#139934=CARTESIAN_POINT('Ctrl Pts',(20.2935357313021,17.1808649545431,8.74981199697633));
#139935=CARTESIAN_POINT('Ctrl Pts',(20.2268660954868,17.1296498004185,8.75399550841146));
#139936=CARTESIAN_POINT('Ctrl Pts',(20.1577482403935,17.0817815617839,8.75817901984659));
#139937=CARTESIAN_POINT('Ctrl Pts',(20.086560133894,17.0374818647638,8.76236253128172));
#139938=CARTESIAN_POINT('Ctrl Pts',(20.0221613278628,16.9974070863223,8.76614705589809));
#139939=CARTESIAN_POINT('Ctrl Pts',(19.9560688916324,16.9602521636411,8.76993158051446));
#139940=CARTESIAN_POINT('Ctrl Pts',(19.8885775886028,16.9261475776549,8.77371610513083));
#139941=CARTESIAN_POINT('Ctrl Pts',(19.8139509296381,16.8884373662162,8.77790073952388));
#139942=CARTESIAN_POINT('Ctrl Pts',(19.7373359438749,16.8543169479217,8.78208537391693));
#139943=CARTESIAN_POINT('Ctrl Pts',(19.6591123506695,16.8240003898955,8.78627000830997));
#139944=CARTESIAN_POINT('Ctrl Pts',(19.5810000990668,16.7937269837373,8.79044868639392));
#139945=CARTESIAN_POINT('Ctrl Pts',(19.5012842132702,16.7672468481168,8.79462736447787));
#139946=CARTESIAN_POINT('Ctrl Pts',(19.420368077509,16.7447277396491,8.79880604256181));
#139947=CARTESIAN_POINT('Ctrl Pts',(19.3380015781677,16.7218049923462,8.80305962044725));
#139948=CARTESIAN_POINT('Ctrl Pts',(19.2543918069889,16.7029868892007,8.80731319833268));
#139949=CARTESIAN_POINT('Ctrl Pts',(19.1699845756622,16.6883986740302,8.81156677621811));
#139950=CARTESIAN_POINT('Ctrl Pts',(19.0872137432219,16.6740932798773,8.81573789019606));
#139951=CARTESIAN_POINT('Ctrl Pts',(19.0036765695344,16.6638553099793,8.81990900417402));
#139952=CARTESIAN_POINT('Ctrl Pts',(18.9198060037776,16.6577518473599,8.82408011815197));
#139953=CARTESIAN_POINT('Ctrl Pts',(18.8359635815991,16.6516504328162,8.82824983247234));
#139954=CARTESIAN_POINT('Ctrl Pts',(18.7517884479705,16.6496808035662,8.83241954679272));
#139955=CARTESIAN_POINT('Ctrl Pts',(18.6677187513895,16.6518581914863,8.83658926111309));
#139956=CARTESIAN_POINT('Ctrl Pts',(18.5836520463691,16.6540355019256,8.84075882705714));
#139957=CARTESIAN_POINT('Ctrl Pts',(18.4996912307931,16.660359523368,8.84492839300118));
#139958=CARTESIAN_POINT('Ctrl Pts',(18.4162731576902,16.6707933836643,8.84909795894523));
#139959=CARTESIAN_POINT('Ctrl Pts',(18.3299222080443,16.681594085617,8.85341412168415));
#139960=CARTESIAN_POINT('Ctrl Pts',(18.2441533999762,16.6967989420232,8.85773028442307));
#139961=CARTESIAN_POINT('Ctrl Pts',(18.1594420717103,16.7163089996876,8.86204644716199));
#139962=CARTESIAN_POINT('Ctrl Pts',(18.0774902060527,16.7351835192758,8.86622201135367));
#139963=CARTESIAN_POINT('Ctrl Pts',(17.996528423794,16.758086889941,8.87039757554535));
#139964=CARTESIAN_POINT('Ctrl Pts',(17.9169718130409,16.7848786218092,8.87457313973703));
#139965=CARTESIAN_POINT('Ctrl Pts',(17.8333969870066,16.8130235403628,8.87895960174957));
#139966=CARTESIAN_POINT('Ctrl Pts',(17.7513735563979,16.8454597306831,8.88334606376211));
#139967=CARTESIAN_POINT('Ctrl Pts',(17.6713570660694,16.8819680133224,8.88773252577465));
#139968=CARTESIAN_POINT('Ctrl Pts',(17.5913405757408,16.9184762959617,8.89211898778719));
#139969=CARTESIAN_POINT('Ctrl Pts',(17.513331505326,16.959056335675,8.89650544979973));
#139970=CARTESIAN_POINT('Ctrl Pts',(17.4377516489576,17.003435683288,8.90089191181227));
#139971=CARTESIAN_POINT('Ctrl Pts',(17.365649333817,17.0457730713314,8.90507654620532));
#139972=CARTESIAN_POINT('Ctrl Pts',(17.2954892230291,17.091725414496,8.90926118059837));
#139973=CARTESIAN_POINT('Ctrl Pts',(17.2276568480541,17.1410892993693,8.91344581499142));
#139974=CARTESIAN_POINT('Ctrl Pts',(17.159921024069,17.1903829208624,8.91762449307535));
#139975=CARTESIAN_POINT('Ctrl Pts',(17.0945067235342,17.2430781703289,8.92180317115929));
#139976=CARTESIAN_POINT('Ctrl Pts',(17.0317733474474,17.2989266689429,8.92598184924323));
#139977=CARTESIAN_POINT('Ctrl Pts',(16.9679155206799,17.3557762117571,8.93023542712867));
#139978=CARTESIAN_POINT('Ctrl Pts',(16.9068360906096,17.4158929154663,8.9344890050141));
#139979=CARTESIAN_POINT('Ctrl Pts',(16.8488816768788,17.4789697150936,8.93874258289954));
#139980=CARTESIAN_POINT('Ctrl Pts',(16.792050822547,17.540823647876,8.94291369687749));
#139981=CARTESIAN_POINT('Ctrl Pts',(16.7382252223475,17.6055235719755,8.94708481085544));
#139982=CARTESIAN_POINT('Ctrl Pts',(16.6876956296653,17.6727417564176,8.9512559248334));
#139983=CARTESIAN_POINT('Ctrl Pts',(16.637182992676,17.7399373851488,8.95542563915377));
#139984=CARTESIAN_POINT('Ctrl Pts',(16.5899644428518,17.8096492285707,8.95959535347414));
#139985=CARTESIAN_POINT('Ctrl Pts',(16.5462899492621,17.8815171178611,8.96376506779451));
#139986=CARTESIAN_POINT('Ctrl Pts',(16.5026170097983,17.9533824497836,8.96793463373855));
#139987=CARTESIAN_POINT('Ctrl Pts',(16.4624881140049,18.0274032814579,8.9721041996826));
#139988=CARTESIAN_POINT('Ctrl Pts',(16.4261087184981,18.1031923304257,8.97627376562664));
#139989=CARTESIAN_POINT('Ctrl Pts',(16.3884502683242,18.1816460288594,8.98058992836556));
#139990=CARTESIAN_POINT('Ctrl Pts',(16.3548101172679,18.2619941236263,8.98490609110448));
#139991=CARTESIAN_POINT('Ctrl Pts',(16.3253623529172,18.3437833690158,8.9892222538434));
#139992=CARTESIAN_POINT('Ctrl Pts',(16.296873846393,18.4229083383394,8.99339781803508));
#139993=CARTESIAN_POINT('Ctrl Pts',(16.2723088794104,18.5033815448835,8.99757338222676));
#139994=CARTESIAN_POINT('Ctrl Pts',(16.2517740015379,18.5847779207351,9.00174894641844));
#139995=CARTESIAN_POINT('Ctrl Pts',(16.2302019558011,18.6702854340295,9.00613540843099));
#139996=CARTESIAN_POINT('Ctrl Pts',(16.213077931431,18.7568112533014,9.01052187044352));
#139997=CARTESIAN_POINT('Ctrl Pts',(16.2004642109876,18.8438536997419,9.01490833245606));
#139998=CARTESIAN_POINT('Ctrl Pts',(16.1878504905441,18.9308961461825,9.01929479446861));
#139999=CARTESIAN_POINT('Ctrl Pts',(16.179747051756,19.0184546350337,9.02368125648115));
#140000=CARTESIAN_POINT('Ctrl Pts',(16.1761531171477,19.10602703261,9.02806771849369));
#140001=CARTESIAN_POINT('Ctrl Pts',(16.1747268399112,19.1407807303868,9.0298085155863));
#140002=CARTESIAN_POINT('Ctrl Pts',(16.1740088273484,19.1755636940745,9.0315493126789));
#140003=CARTESIAN_POINT('Ctrl Pts',(16.1740000808904,19.2103564484228,9.0332901097715));
#140004=CARTESIAN_POINT('',(16.174000001606,19.2110906788005,8.96670989026365));
#140005=CARTESIAN_POINT('Ctrl Pts',(20.2935357313021,17.1808649545431,8.68337763228924));
#140006=CARTESIAN_POINT('Ctrl Pts',(20.2269370011896,17.1297042696901,8.68754916275219));
#140007=CARTESIAN_POINT('Ctrl Pts',(20.157763917459,17.0817825471759,8.69172069321514));
#140008=CARTESIAN_POINT('Ctrl Pts',(20.0863673947936,17.0373619368673,8.69589222367809));
#140009=CARTESIAN_POINT('Ctrl Pts',(20.0149989840445,16.9929588168851,8.70006211162806));
#140010=CARTESIAN_POINT('Ctrl Pts',(19.9414092630416,16.9520543143202,8.70423199957803));
#140011=CARTESIAN_POINT('Ctrl Pts',(19.8659780913813,16.9148672510865,8.70840188752799));
#140012=CARTESIAN_POINT('Ctrl Pts',(19.7905539926854,16.8776836747771,8.71257138447953));
#140013=CARTESIAN_POINT('Ctrl Pts',(19.7132891992873,16.8442170480217,8.71674088143107));
#140014=CARTESIAN_POINT('Ctrl Pts',(19.6345869032211,16.8146395868429,8.72091037838262));
#140015=CARTESIAN_POINT('Ctrl Pts',(19.5558683784269,16.7850560266733,8.7250807351011));
#140016=CARTESIAN_POINT('Ctrl Pts',(19.4757121933861,16.7593633850936,8.72925109181958));
#140017=CARTESIAN_POINT('Ctrl Pts',(19.3945388869154,16.7376847392876,8.73342144853806));
#140018=CARTESIAN_POINT('Ctrl Pts',(19.3132745110844,16.7159817719345,8.73759648403255));
#140019=CARTESIAN_POINT('Ctrl Pts',(19.2309911818684,16.6983019051782,8.74177151952703));
#140020=CARTESIAN_POINT('Ctrl Pts',(19.1481213253207,16.6847174489154,8.74594655502151));
#140021=CARTESIAN_POINT('Ctrl Pts',(19.0651969677462,16.6711240585619,8.75012433631201));
#140022=CARTESIAN_POINT('Ctrl Pts',(18.9816857717183,16.6616314907568,8.75430211760251));
#140023=CARTESIAN_POINT('Ctrl Pts',(18.8980246357382,16.6562601073943,8.75847989889301));
#140024=CARTESIAN_POINT('Ctrl Pts',(18.8142288636417,16.6508800798485,8.76266440349943));
#140025=CARTESIAN_POINT('Ctrl Pts',(18.7302831289701,16.6496344772916,8.76684890810586));
#140026=CARTESIAN_POINT('Ctrl Pts',(18.6466231447615,16.6524915897796,8.77103341271229));
#140027=CARTESIAN_POINT('Ctrl Pts',(18.6193179827511,16.6534241015426,8.77239916214785));
#140028=CARTESIAN_POINT('Ctrl Pts',(18.5920432050038,16.6547932470753,8.77376491158341));
#140029=CARTESIAN_POINT('Ctrl Pts',(18.5648137584889,16.6565967398072,8.77513066101897));
#140030=CARTESIAN_POINT('Ctrl Pts',(18.4813831705471,16.6621226126484,8.77931529541201));
#140031=CARTESIAN_POINT('Ctrl Pts',(18.3980683312295,16.6717505167586,8.78349992980505));
#140032=CARTESIAN_POINT('Ctrl Pts',(18.3153050503469,16.6854714337124,8.7876845641981));
#140033=CARTESIAN_POINT('Ctrl Pts',(18.2326595727503,16.6991728206391,8.79186324228205));
#140034=CARTESIAN_POINT('Ctrl Pts',(18.150564544139,16.7169555737483,8.796041920366));
#140035=CARTESIAN_POINT('Ctrl Pts',(18.0694525718374,16.738758766681,8.80022059844995));
#140036=CARTESIAN_POINT('Ctrl Pts',(17.9868867257265,16.7609527661774,8.80447417633538));
#140037=CARTESIAN_POINT('Ctrl Pts',(17.9053400062234,16.7873127240842,8.80872775422082));
#140038=CARTESIAN_POINT('Ctrl Pts',(17.8252599013638,16.8177195247672,8.81298133210625));
#140039=CARTESIAN_POINT('Ctrl Pts',(17.7467323056004,16.8475368302849,8.8171524460842));
#140040=CARTESIAN_POINT('Ctrl Pts',(17.6696154154523,16.8812452961237,8.82132356006215));
#140041=CARTESIAN_POINT('Ctrl Pts',(17.5943160431835,16.9186822910916,8.8254946740401));
#140042=CARTESIAN_POINT('Ctrl Pts',(17.5190419383462,16.9561067237143,8.82966438836047));
#140043=CARTESIAN_POINT('Ctrl Pts',(17.4455845517329,16.9972569960431,8.83383410268084));
#140044=CARTESIAN_POINT('Ctrl Pts',(17.3743287784396,17.0419231988562,8.83800381700122));
#140045=CARTESIAN_POINT('Ctrl Pts',(17.3030755407325,17.086587812254,8.84217338294526));
#140046=CARTESIAN_POINT('Ctrl Pts',(17.2340241499107,17.1347678623261,8.8463429488893));
#140047=CARTESIAN_POINT('Ctrl Pts',(17.1675318647116,17.1862092500394,8.85051251483334));
#140048=CARTESIAN_POINT('Ctrl Pts',(17.0987017927918,17.239459253485,8.85482867757226));
#140049=CARTESIAN_POINT('Ctrl Pts',(17.0326145482172,17.2962038761403,8.85914484031118));
#140050=CARTESIAN_POINT('Ctrl Pts',(16.9696289167233,17.3561159927108,8.86346100305011));
#140051=CARTESIAN_POINT('Ctrl Pts',(16.9086950355505,17.4140764783858,8.86763656724179));
#140052=CARTESIAN_POINT('Ctrl Pts',(16.8506640912072,17.4750008911688,8.87181213143347));
#140053=CARTESIAN_POINT('Ctrl Pts',(16.7958218659393,17.5385570202099,8.87598769562515));
#140054=CARTESIAN_POINT('Ctrl Pts',(16.7382096902482,17.6053232182385,8.88037415763769));
#140055=CARTESIAN_POINT('Ctrl Pts',(16.6841171816931,17.6749935141295,8.88476061965023));
#140056=CARTESIAN_POINT('Ctrl Pts',(16.6338248927155,17.7471473712348,8.88914708166278));
#140057=CARTESIAN_POINT('Ctrl Pts',(16.5835326037379,17.8193012283401,8.89353354367532));
#140058=CARTESIAN_POINT('Ctrl Pts',(16.5370407765469,17.8939381139568,8.89792000568786));
#140059=CARTESIAN_POINT('Ctrl Pts',(16.4945737975988,17.9706088181549,8.9023064677004));
#140060=CARTESIAN_POINT('Ctrl Pts',(16.4520961746313,18.0472987392713,8.90669402914567));
#140061=CARTESIAN_POINT('Ctrl Pts',(16.4134992022808,18.1262856298358,8.91108159059094));
#140062=CARTESIAN_POINT('Ctrl Pts',(16.3790251742671,18.2071605854698,8.91546915203621));
#140063=CARTESIAN_POINT('Ctrl Pts',(16.3446454932945,18.2878142059945,8.91984470579152));
#140064=CARTESIAN_POINT('Ctrl Pts',(16.3143664333072,18.3703452363826,8.92422025954683));
#140065=CARTESIAN_POINT('Ctrl Pts',(16.2883841141658,18.4543211123896,8.92859581330214));
#140066=CARTESIAN_POINT('Ctrl Pts',(16.2624439986578,18.5381605845957,8.93296425975245));
#140067=CARTESIAN_POINT('Ctrl Pts',(16.2407868563187,18.6234398583863,8.93733270620276));
#140068=CARTESIAN_POINT('Ctrl Pts',(16.2235607960525,18.7097066694205,8.94170115265307));
#140069=CARTESIAN_POINT('Ctrl Pts',(16.2063704951607,18.7957944002037,8.94606053069715));
#140070=CARTESIAN_POINT('Ctrl Pts',(16.193593030381,18.8828651985171,8.95041990874122));
#140071=CARTESIAN_POINT('Ctrl Pts',(16.1853263642748,18.9704533339262,8.9547792867853));
#140072=CARTESIAN_POINT('Ctrl Pts',(16.1777850503447,19.0503561166421,8.9587561545997));
#140073=CARTESIAN_POINT('Ctrl Pts',(16.1739971536887,19.1306890276032,8.96273302241411));
#140074=CARTESIAN_POINT('Ctrl Pts',(16.174000001606,19.21109067809,8.96670989022851));
#140075=CARTESIAN_POINT('Ctrl Pts',(16.174000001606,19.2110906788005,8.96670989026365));
#140076=CARTESIAN_POINT('Ctrl Pts',(16.1740031377284,19.2996281672636,8.97108917708311));
#140077=CARTESIAN_POINT('Ctrl Pts',(16.1786036643305,19.388071802769,8.97546846390256));
#140078=CARTESIAN_POINT('Ctrl Pts',(16.1877467776184,19.4759424985001,8.97984775072202));
#140079=CARTESIAN_POINT('Ctrl Pts',(16.1969159526896,19.5640636632955,8.98423952038188));
#140080=CARTESIAN_POINT('Ctrl Pts',(16.2106535575187,19.6516082364872,8.98863129004175));
#140081=CARTESIAN_POINT('Ctrl Pts',(16.2288531973791,19.7381048257399,8.99302305970162));
#140082=CARTESIAN_POINT('Ctrl Pts',(16.2470794228643,19.8247277672657,8.99742124475987));
#140083=CARTESIAN_POINT('Ctrl Pts',(16.2697805833341,19.9102992971043,9.00181942981813));
#140084=CARTESIAN_POINT('Ctrl Pts',(16.2968004138021,19.9943633748375,9.00621761487638));
#140085=CARTESIAN_POINT('Ctrl Pts',(16.3238953969119,20.0786612674176,9.01062803299533));
#140086=CARTESIAN_POINT('Ctrl Pts',(16.3553329301083,20.1614429605719,9.01503845111429));
#140087=CARTESIAN_POINT('Ctrl Pts',(16.3909082116845,20.2422714829415,9.01944886923325));
#140088=CARTESIAN_POINT('Ctrl Pts',(16.4178853374884,20.3035646370615,9.02279333761611));
#140089=CARTESIAN_POINT('Ctrl Pts',(16.4472408225494,20.363735085321,9.02613780599897));
#140090=CARTESIAN_POINT('Ctrl Pts',(16.478868382946,20.422602818486,9.02948227438183));
#140091=CARTESIAN_POINT('Ctrl Pts',(16.5184411227219,20.4962587519986,9.03366690877488));
#140092=CARTESIAN_POINT('Ctrl Pts',(16.5616998679758,20.5681109610611,9.03785154316793));
#140093=CARTESIAN_POINT('Ctrl Pts',(16.6084559713663,20.6377664778581,9.04203617756098));
#140094=CARTESIAN_POINT('Ctrl Pts',(16.6551455232309,20.7073228486487,9.04621485564492));
#140095=CARTESIAN_POINT('Ctrl Pts',(16.7053222910481,20.7746883591286,9.05039353372887));
#140096=CARTESIAN_POINT('Ctrl Pts',(16.7587517035101,20.8394944480144,9.05457221181282));
#140097=CARTESIAN_POINT('Ctrl Pts',(16.8131387997914,20.9054621394682,9.05882578969825));
#140098=CARTESIAN_POINT('Ctrl Pts',(16.8708960667842,20.9687773268414,9.06307936758369));
#140099=CARTESIAN_POINT('Ctrl Pts',(16.9317298045576,21.0290819955712,9.06733294546912));
#140100=CARTESIAN_POINT('Ctrl Pts',(16.9913841616171,21.0882175406228,9.07150405944708));
#140101=CARTESIAN_POINT('Ctrl Pts',(17.0539964254171,21.1444579161298,9.07567517342503));
#140102=CARTESIAN_POINT('Ctrl Pts',(17.1192501263854,21.1975001499274,9.07984628740298));
#140103=CARTESIAN_POINT('Ctrl Pts',(17.1844819308442,21.2505245848913,9.08401600172335));
#140104=CARTESIAN_POINT('Ctrl Pts',(17.2523530554692,21.3003527195435,9.08818571604373));
#140105=CARTESIAN_POINT('Ctrl Pts',(17.3225130695873,21.3467211066228,9.0923554303641));
#140106=CARTESIAN_POINT('Ctrl Pts',(17.3926705871109,21.3930878437158,9.09652499630815));
#140107=CARTESIAN_POINT('Ctrl Pts',(17.4651164479275,21.4359948250818,9.10069456225219));
#140108=CARTESIAN_POINT('Ctrl Pts',(17.5394714392698,21.475222055718,9.10486412819623));
#140109=CARTESIAN_POINT('Ctrl Pts',(17.6164406603808,21.5158284673913,9.10918029093515));
#140110=CARTESIAN_POINT('Ctrl Pts',(17.6954552934394,21.5524913076844,9.11349645367408));
#140111=CARTESIAN_POINT('Ctrl Pts',(17.7760690203244,21.5850194266639,9.117812616413));
#140112=CARTESIAN_POINT('Ctrl Pts',(17.8540567635352,21.6164879455891,9.12198818060468));
#140113=CARTESIAN_POINT('Ctrl Pts',(17.9335405590284,21.6440868736176,9.12616374479636));
#140114=CARTESIAN_POINT('Ctrl Pts',(18.0140996850996,21.6676936187906,9.13033930898804));
#140115=CARTESIAN_POINT('Ctrl Pts',(18.0987276611175,21.6924926845425,9.13472577100058));
#140116=CARTESIAN_POINT('Ctrl Pts',(18.1845418843915,21.7128855434687,9.13911223301312));
#140117=CARTESIAN_POINT('Ctrl Pts',(18.2710433987722,21.7287909336122,9.14349869502566));
#140118=CARTESIAN_POINT('Ctrl Pts',(18.3575449131529,21.7446963237556,9.14788515703819));
#140119=CARTESIAN_POINT('Ctrl Pts',(18.4447331334585,21.756114245197,9.15227161905073));
#140120=CARTESIAN_POINT('Ctrl Pts',(18.5321062576865,21.7630264334083,9.15665808106327));
#140121=CARTESIAN_POINT('Ctrl Pts',(18.6154592149507,21.7696205815937,9.16084271545632));
#140122=CARTESIAN_POINT('Ctrl Pts',(18.6992906902526,21.7721390606606,9.16502734984937));
#140123=CARTESIAN_POINT('Ctrl Pts',(18.78316814862,21.7705277871438,9.16921198424242));
#140124=CARTESIAN_POINT('Ctrl Pts',(18.8669262178074,21.7689188070754,9.17339066232636));
#140125=CARTESIAN_POINT('Ctrl Pts',(18.9507296840396,21.7631917591217,9.17756934041031));
#140126=CARTESIAN_POINT('Ctrl Pts',(19.0341416766033,21.7533443853982,9.18174801849425));
#140127=CARTESIAN_POINT('Ctrl Pts',(19.1190487691866,21.7433205045779,9.18600159637969));
#140128=CARTESIAN_POINT('Ctrl Pts',(19.2035497350918,21.7290270933803,9.19025517426511));
#140129=CARTESIAN_POINT('Ctrl Pts',(19.2871845665266,21.7105173204755,9.19450875215055));
#140130=CARTESIAN_POINT('Ctrl Pts',(19.369197973554,21.6923663956372,9.1986798661285));
#140131=CARTESIAN_POINT('Ctrl Pts',(19.4503780599824,21.6701612389659,9.20285098010646));
#140132=CARTESIAN_POINT('Ctrl Pts',(19.5302987751906,21.6440039582027,9.20702209408442));
#140133=CARTESIAN_POINT('Ctrl Pts',(19.610192672231,21.6178554547677,9.21119180840479));
#140134=CARTESIAN_POINT('Ctrl Pts',(19.6888276004821,21.5877576040183,9.21536152272516));
#140135=CARTESIAN_POINT('Ctrl Pts',(19.7657923610116,21.553862463688,9.21953123704553));
#140136=CARTESIAN_POINT('Ctrl Pts',(19.8427543828046,21.5199685294922,9.22370080298957));
#140137=CARTESIAN_POINT('Ctrl Pts',(19.9180459343718,21.4822777605697,9.22787036893362));
#140138=CARTESIAN_POINT('Ctrl Pts',(19.9912767740527,21.4409899357234,9.23203993487766));
#140139=CARTESIAN_POINT('Ctrl Pts',(20.0670823197166,21.3982504818896,9.23635609761658));
#140140=CARTESIAN_POINT('Ctrl Pts',(20.1406790886265,21.351656579909,9.2406722603555));
#140141=CARTESIAN_POINT('Ctrl Pts',(20.2116647704044,21.3014800468566,9.24498842309442));
#140142=CARTESIAN_POINT('Ctrl Pts',(20.2803381010648,21.2529380090908,9.2491639872861));
#140143=CARTESIAN_POINT('Ctrl Pts',(20.3465675028829,21.2010434919511,9.25333955147778));
#140144=CARTESIAN_POINT('Ctrl Pts',(20.4100221667426,21.1460838991081,9.25751511566946));
#140145=CARTESIAN_POINT('Ctrl Pts',(20.4766817748247,21.0883484278846,9.26190157768201));
#140146=CARTESIAN_POINT('Ctrl Pts',(20.5402785534045,21.0272305142621,9.26628803969455));
#140147=CARTESIAN_POINT('Ctrl Pts',(20.6004740985359,20.9631057158444,9.27067450170709));
#140148=CARTESIAN_POINT('Ctrl Pts',(20.6606696436673,20.8989809174267,9.27506096371963));
#140149=CARTESIAN_POINT('Ctrl Pts',(20.7174636386703,20.8318497263029,9.27944742573217));
#140150=CARTESIAN_POINT('Ctrl Pts',(20.7705691100607,20.7621241923026,9.28383388774471));
#140151=CARTESIAN_POINT('Ctrl Pts',(20.8212311199913,20.6956068334797,9.28801852213775));
#140152=CARTESIAN_POINT('Ctrl Pts',(20.8687251499198,20.6264810343217,9.2922031565308));
#140153=CARTESIAN_POINT('Ctrl Pts',(20.9127716012342,20.5550812139358,9.29638779092385));
#140154=CARTESIAN_POINT('Ctrl Pts',(20.9567553578771,20.4837830223568,9.30056646900779));
#140155=CARTESIAN_POINT('Ctrl Pts',(20.997301043686,20.4102176270062,9.30474514709174));
#140156=CARTESIAN_POINT('Ctrl Pts',(21.0341702903064,20.3347511448678,9.30892382517568));
#140157=CARTESIAN_POINT('Ctrl Pts',(21.071700391675,20.2579319802738,9.31317740306111));
#140158=CARTESIAN_POINT('Ctrl Pts',(21.1054206649962,20.1791432881301,9.31743098094655));
#140159=CARTESIAN_POINT('Ctrl Pts',(21.1351268232138,20.0988006413847,9.32168455883199));
#140160=CARTESIAN_POINT('Ctrl Pts',(21.1642570695876,20.0200155936223,9.32585567280994));
#140161=CARTESIAN_POINT('Ctrl Pts',(21.1895272879509,19.9397367578111,9.33002678678789));
#140162=CARTESIAN_POINT('Ctrl Pts',(21.2107927216344,19.8583776440833,9.33419790076584));
#140163=CARTESIAN_POINT('Ctrl Pts',(21.2320510194963,19.777045831192,9.33836761508621));
#140164=CARTESIAN_POINT('Ctrl Pts',(21.2493070853372,19.6946349050203,9.34253732940659));
#140165=CARTESIAN_POINT('Ctrl Pts',(21.2624662014641,19.6115729247638,9.34670704372696));
#140166=CARTESIAN_POINT('Ctrl Pts',(21.2756248493332,19.528513900209,9.350876609671));
#140167=CARTESIAN_POINT('Ctrl Pts',(21.284686766209,19.4448043221315,9.35504617561504));
#140168=CARTESIAN_POINT('Ctrl Pts',(21.2896087040397,19.3608804584879,9.35921574155908));
#140169=CARTESIAN_POINT('Ctrl Pts',(21.2947036911327,19.2740059353298,9.36353190429801));
#140170=CARTESIAN_POINT('Ctrl Pts',(21.2953621283496,19.1869023041989,9.36784806703693));
#140171=CARTESIAN_POINT('Ctrl Pts',(21.2915948078576,19.1000549738833,9.37216422977585));
#140172=CARTESIAN_POINT('Ctrl Pts',(21.2879502074343,19.016036686218,9.37633979396753));
#140173=CARTESIAN_POINT('Ctrl Pts',(21.2801638500694,18.9322587224487,9.38051535815921));
#140174=CARTESIAN_POINT('Ctrl Pts',(21.2682983360669,18.8491548068462,9.38469092235089));
#140175=CARTESIAN_POINT('Ctrl Pts',(21.2558335231598,18.7618535100274,9.38907738436343));
#140176=CARTESIAN_POINT('Ctrl Pts',(21.2388667599596,18.6752967161991,9.39346384637597));
#140177=CARTESIAN_POINT('Ctrl Pts',(21.2175306593405,18.5899722517346,9.39785030838851));
#140178=CARTESIAN_POINT('Ctrl Pts',(21.1961945587214,18.5046477872701,9.40223677040106));
#140179=CARTESIAN_POINT('Ctrl Pts',(21.1704893630394,18.4205561848056,9.4066232324136));
#140180=CARTESIAN_POINT('Ctrl Pts',(21.1406062076889,18.3381617783842,9.41100969442614));
#140181=CARTESIAN_POINT('Ctrl Pts',(21.1121004746698,18.259565227111,9.41519396859536));
#140182=CARTESIAN_POINT('Ctrl Pts',(21.0796873621586,18.182220330688,9.41937824276457));
#140183=CARTESIAN_POINT('Ctrl Pts',(21.0434966865738,18.1065430951347,9.42356251693379));
#140184=CARTESIAN_POINT('Ctrl Pts',(21.007355056005,18.0309684161425,9.42774112064258));
#140185=CARTESIAN_POINT('Ctrl Pts',(20.9674462242518,17.9570573217824,9.43191972435137));
#140186=CARTESIAN_POINT('Ctrl Pts',(20.9239489993286,17.8852083948299,9.43609832806016));
#140187=CARTESIAN_POINT('Ctrl Pts',(20.8805019784934,17.8134423952331,9.44027210886385));
#140188=CARTESIAN_POINT('Ctrl Pts',(20.8334750334886,17.7437342236849,9.44444588966753));
#140189=CARTESIAN_POINT('Ctrl Pts',(20.7830933894016,17.6764589345635,9.44861967047122));
#140190=CARTESIAN_POINT('Ctrl Pts',(20.7327462827087,17.6092297636906,9.45279059008379));
#140191=CARTESIAN_POINT('Ctrl Pts',(20.6790493196799,17.5444305296965,9.45696150969635));
#140192=CARTESIAN_POINT('Ctrl Pts',(20.6222709998958,17.4824073264784,9.46113242930892));
#140193=CARTESIAN_POINT('Ctrl Pts',(20.5655043373565,17.4203968573402,9.46530249258352));
#140194=CARTESIAN_POINT('Ctrl Pts',(20.5056578783566,17.3611616320062,9.46947255585812));
#140195=CARTESIAN_POINT('Ctrl Pts',(20.4430396423748,17.3050137721402,9.47364261913271));
#140196=CARTESIAN_POINT('Ctrl Pts',(20.3947976075597,17.2617566128161,9.47685529886603));
#140197=CARTESIAN_POINT('Ctrl Pts',(20.3449112621541,17.2203312827846,9.48006797859935));
#140198=CARTESIAN_POINT('Ctrl Pts',(20.2935357313021,17.1808649545431,9.48328065833267));
#140199=CARTESIAN_POINT('Origin',(18.734,19.211,-1.76670989022852));
#140200=CARTESIAN_POINT('',(20.2935357313021,17.1808649545432,10.3499274784722));
#140201=CARTESIAN_POINT('',(20.2935357313021,17.1808649545432,10.2832382208556));
#140202=CARTESIAN_POINT('',(20.2935357313021,17.1808649545432,-1.76670989022852));
#140203=CARTESIAN_POINT('',(16.1740007840082,19.2089964727374,9.83329010977151));
#140204=CARTESIAN_POINT('Ctrl Pts',(16.1740007840082,19.2089964727374,9.83329010977151));
#140205=CARTESIAN_POINT('Ctrl Pts',(16.1739350379054,19.2930033015151,9.83745593779553));
#140206=CARTESIAN_POINT('Ctrl Pts',(16.1780086491546,19.3770604200798,9.84162176581954));
#140207=CARTESIAN_POINT('Ctrl Pts',(16.186209790272,19.4607299485725,9.84578759384356));
#140208=CARTESIAN_POINT('Ctrl Pts',(16.1944094741073,19.544384609609,9.84995268163076));
#140209=CARTESIAN_POINT('Ctrl Pts',(16.2067351859308,19.6276513592373,9.85411776941796));
#140210=CARTESIAN_POINT('Ctrl Pts',(16.2231231591268,19.7100966739689,9.85828285720516));
#140211=CARTESIAN_POINT('Ctrl Pts',(16.2395131466373,19.7925521223991,9.86244845694073));
#140212=CARTESIAN_POINT('Ctrl Pts',(16.2599662961795,19.8741854840192,9.8666140566763));
#140213=CARTESIAN_POINT('Ctrl Pts',(16.2843678510517,19.9545740278134,9.87077965641186));
#140214=CARTESIAN_POINT('Ctrl Pts',(16.3087969918046,20.035053450603,9.87494996534479));
#140215=CARTESIAN_POINT('Ctrl Pts',(16.3371833165997,20.1142848040861,9.87912027427772));
#140216=CARTESIAN_POINT('Ctrl Pts',(16.3693624790257,20.191861557204,9.88329058321065));
#140217=CARTESIAN_POINT('Ctrl Pts',(16.4015603628986,20.2694834435371,9.88746331837879));
#140218=CARTESIAN_POINT('Ctrl Pts',(16.437555280145,20.3454483968708,9.89163605354694));
#140219=CARTESIAN_POINT('Ctrl Pts',(16.4771361744286,20.4193731513184,9.89580878871509));
#140220=CARTESIAN_POINT('Ctrl Pts',(16.5167895617082,20.4934333000524,9.8999891663097));
#140221=CARTESIAN_POINT('Ctrl Pts',(16.5600418069655,20.5654453913553,9.90416954390431));
#140222=CARTESIAN_POINT('Ctrl Pts',(16.6066377495773,20.6350540212634,9.90834992149893));
#140223=CARTESIAN_POINT('Ctrl Pts',(16.6436006876733,20.6902721225405,9.91166606942054));
#140224=CARTESIAN_POINT('Ctrl Pts',(16.6826668124624,20.7439783287842,9.91498221734214));
#140225=CARTESIAN_POINT('Ctrl Pts',(16.7236914224215,20.7960108589263,9.91829836526375));
#140226=CARTESIAN_POINT('Ctrl Pts',(16.7754602209958,20.8616705099242,9.9224829996568));
#140227=CARTESIAN_POINT('Ctrl Pts',(16.8305455538229,20.924913415419,9.92666763404985));
#140228=CARTESIAN_POINT('Ctrl Pts',(16.8886933634204,20.9853853631597,9.93085226844291));
#140229=CARTESIAN_POINT('Ctrl Pts',(16.9467584068082,21.0457712365676,9.93503094652685));
#140230=CARTESIAN_POINT('Ctrl Pts',(17.0078769523777,21.1033936577097,9.9392096246108));
#140231=CARTESIAN_POINT('Ctrl Pts',(17.07175395795,21.157930429083,9.94338830269474));
#140232=CARTESIAN_POINT('Ctrl Pts',(17.1367759129396,21.2134447328882,9.94764188058018));
#140233=CARTESIAN_POINT('Ctrl Pts',(17.2046558928942,21.2657612997092,9.95189545846561));
#140234=CARTESIAN_POINT('Ctrl Pts',(17.2750424589418,21.314578592159,9.95614903635105));
#140235=CARTESIAN_POINT('Ctrl Pts',(17.3440644440585,21.3624494661354,9.960320150329));
#140236=CARTESIAN_POINT('Ctrl Pts',(17.4154962970282,21.406955261226,9.96449126430695));
#140237=CARTESIAN_POINT('Ctrl Pts',(17.4889737195064,21.4478526015096,9.9686623782849));
#140238=CARTESIAN_POINT('Ctrl Pts',(17.5624264859258,21.4887362182957,9.97283209260527));
#140239=CARTESIAN_POINT('Ctrl Pts',(17.6379230570028,21.5260135615005,9.97700180692565));
#140240=CARTESIAN_POINT('Ctrl Pts',(17.7150725574697,21.5594860797668,9.98117152124603));
#140241=CARTESIAN_POINT('Ctrl Pts',(17.7922193126263,21.5929574069373,9.98534108719007));
#140242=CARTESIAN_POINT('Ctrl Pts',(17.8710184578639,21.6226239960436,9.98951065313412));
#140243=CARTESIAN_POINT('Ctrl Pts',(17.9510583236145,21.6483350880375,9.99368021907816));
#140244=CARTESIAN_POINT('Ctrl Pts',(18.033912292305,21.6749501503078,9.99799638181708));
#140245=CARTESIAN_POINT('Ctrl Pts',(18.1180953501449,21.6973262283484,10.002312544556));
#140246=CARTESIAN_POINT('Ctrl Pts',(18.2031347548813,21.7153526292288,10.0066287072949));
#140247=CARTESIAN_POINT('Ctrl Pts',(18.2854040099531,21.7327918219965,10.0108042714866));
#140248=CARTESIAN_POINT('Ctrl Pts',(18.3684742051326,21.7461603390116,10.0149798356783));
#140249=CARTESIAN_POINT('Ctrl Pts',(18.4519097174452,21.7554105550182,10.01915539987));
#140250=CARTESIAN_POINT('Ctrl Pts',(18.5395593591354,21.765127977445,10.0235418618825));
#140251=CARTESIAN_POINT('Ctrl Pts',(18.6276116092813,21.7703001003685,10.027928323895));
#140252=CARTESIAN_POINT('Ctrl Pts',(18.7155609817199,21.7709335933975,10.0323147859076));
#140253=CARTESIAN_POINT('Ctrl Pts',(18.8035103541584,21.7715670864265,10.0367012479201));
#140254=CARTESIAN_POINT('Ctrl Pts',(18.891356272623,21.767662051318,10.0410877099327));
#140255=CARTESIAN_POINT('Ctrl Pts',(18.9786013944248,21.7592876913421,10.0454741719452));
#140256=CARTESIAN_POINT('Ctrl Pts',(19.0618322388442,21.7512986480824,10.0496588063382));
#140257=CARTESIAN_POINT('Ctrl Pts',(19.1448261598418,21.7392127858656,10.0538434407313));
#140258=CARTESIAN_POINT('Ctrl Pts',(19.2271478044731,21.7230519984553,10.0580280751243));
#140259=CARTESIAN_POINT('Ctrl Pts',(19.3093522744327,21.7069142139256,10.0622067532083));
#140260=CARTESIAN_POINT('Ctrl Pts',(19.3908859211793,21.6867131129897,10.0663854312922));
#140261=CARTESIAN_POINT('Ctrl Pts',(19.4713181268662,21.6625223800313,10.0705641093762));
#140262=CARTESIAN_POINT('Ctrl Pts',(19.5531920220343,21.6378980455703,10.0748176872616));
#140263=CARTESIAN_POINT('Ctrl Pts',(19.6339241211584,21.6091396900263,10.079071265147));
#140264=CARTESIAN_POINT('Ctrl Pts',(19.7130706518194,21.5763796014057,10.0833248430325));
#140265=CARTESIAN_POINT('Ctrl Pts',(19.7906827725417,21.544254631029,10.0874959570104));
#140266=CARTESIAN_POINT('Ctrl Pts',(19.8667698102182,21.5082818897807,10.0916670709884));
#140267=CARTESIAN_POINT('Ctrl Pts',(19.9409299364302,21.4686359601469,10.0958381849663));
#140268=CARTESIAN_POINT('Ctrl Pts',(20.0150651774957,21.4290033340877,10.1000078992867));
#140269=CARTESIAN_POINT('Ctrl Pts',(20.0872743858818,21.3857001842594,10.1041776136071));
#140270=CARTESIAN_POINT('Ctrl Pts',(20.1571790379496,21.3389477028209,10.1083473279274));
#140271=CARTESIAN_POINT('Ctrl Pts',(20.22708120251,21.2921968850363,10.1125168938715));
#140272=CARTESIAN_POINT('Ctrl Pts',(20.2946785918821,21.2419972361384,10.1166864598155));
#140273=CARTESIAN_POINT('Ctrl Pts',(20.3596216126351,21.1886133020724,10.1208560257596));
#140274=CARTESIAN_POINT('Ctrl Pts',(20.4268479498819,21.1333524547408,10.1251721884985));
#140275=CARTESIAN_POINT('Ctrl Pts',(20.4912293829738,21.0746795720027,10.1294883512374));
#140276=CARTESIAN_POINT('Ctrl Pts',(20.5524169502583,21.0129322392957,10.1338045139763));
#140277=CARTESIAN_POINT('Ctrl Pts',(20.6116113389744,20.9531963194569,10.137980078168));
#140278=CARTESIAN_POINT('Ctrl Pts',(20.6678164672702,20.8905835561607,10.1421556423597));
#140279=CARTESIAN_POINT('Ctrl Pts',(20.7207564953884,20.8254344607422,10.1463312065514));
#140280=CARTESIAN_POINT('Ctrl Pts',(20.7763703984739,20.7569948393913,10.1507176685639));
#140281=CARTESIAN_POINT('Ctrl Pts',(20.8283803483074,20.6857564036306,10.1551041305764));
#140282=CARTESIAN_POINT('Ctrl Pts',(20.8765183429016,20.6121477974611,10.159490592589));
#140283=CARTESIAN_POINT('Ctrl Pts',(20.9246563374958,20.5385391912916,10.1638770546015));
#140284=CARTESIAN_POINT('Ctrl Pts',(20.9689221504901,20.4625609543414,10.1682635166141));
#140285=CARTESIAN_POINT('Ctrl Pts',(21.0091047687182,20.3846687315233,10.1726499786266));
#140286=CARTESIAN_POINT('Ctrl Pts',(21.0474385251168,20.3103604453409,10.1768346130197));
#140287=CARTESIAN_POINT('Ctrl Pts',(21.0821992629535,20.2340338438631,10.1810192474127));
#140288=CARTESIAN_POINT('Ctrl Pts',(21.113169743127,20.1560668406992,10.1852038818058));
#140289=CARTESIAN_POINT('Ctrl Pts',(21.1440961406553,20.0782108139138,10.1893825598897));
#140290=CARTESIAN_POINT('Ctrl Pts',(21.1712428282378,19.9987194471869,10.1935612379736));
#140291=CARTESIAN_POINT('Ctrl Pts',(21.1944386775071,19.9179947059399,10.1977399160576));
#140292=CARTESIAN_POINT('Ctrl Pts',(21.218050295704,19.835823031722,10.201993493943));
#140293=CARTESIAN_POINT('Ctrl Pts',(21.2375678238504,19.7523737600797,10.2062470718285));
#140294=CARTESIAN_POINT('Ctrl Pts',(21.252862289631,19.6680916383777,10.2105006497139));
#140295=CARTESIAN_POINT('Ctrl Pts',(21.2678602423477,19.585443490068,10.2146717636918));
#140296=CARTESIAN_POINT('Ctrl Pts',(21.2787973301571,19.5019949698559,10.2188428776698));
#140297=CARTESIAN_POINT('Ctrl Pts',(21.2856028472,19.4181784500398,10.2230139916477));
#140298=CARTESIAN_POINT('Ctrl Pts',(21.2924060805859,19.3343900556663,10.2271837059681));
#140299=CARTESIAN_POINT('Ctrl Pts',(21.2950804593957,19.2502343650758,10.2313534202885));
#140300=CARTESIAN_POINT('Ctrl Pts',(21.2936070835643,19.1661493838661,10.2355231346089));
#140301=CARTESIAN_POINT('Ctrl Pts',(21.2921337601619,19.0820673947608,10.2396927005529));
#140302=CARTESIAN_POINT('Ctrl Pts',(21.2865129844866,18.9980565699809,10.243862266497));
#140303=CARTESIAN_POINT('Ctrl Pts',(21.2767779695196,18.9145540559798,10.248031832441));
#140304=CARTESIAN_POINT('Ctrl Pts',(21.2667006834357,18.8281156965981,10.2523479951799));
#140305=CARTESIAN_POINT('Ctrl Pts',(21.2522145228802,18.7422225813438,10.2566641579188));
#140306=CARTESIAN_POINT('Ctrl Pts',(21.2334144574579,18.6573508603364,10.2609803206578));
#140307=CARTESIAN_POINT('Ctrl Pts',(21.2152268021894,18.575243826714,10.2651558848494));
#140308=CARTESIAN_POINT('Ctrl Pts',(21.1930021468739,18.4940931072444,10.2693314490411));
#140309=CARTESIAN_POINT('Ctrl Pts',(21.1668775008281,18.4143149518383,10.2735070132328));
#140310=CARTESIAN_POINT('Ctrl Pts',(21.139433361016,18.3305073914573,10.2778934752453));
#140311=CARTESIAN_POINT('Ctrl Pts',(21.1076851096663,18.2482152402669,10.2822799372579));
#140312=CARTESIAN_POINT('Ctrl Pts',(21.0718481041568,18.1678958623941,10.2866663992704));
#140313=CARTESIAN_POINT('Ctrl Pts',(21.0360110986473,18.0875764845214,10.2910528612829));
#140314=CARTESIAN_POINT('Ctrl Pts',(20.9960856701951,18.0092303623901,10.2954393232955));
#140315=CARTESIAN_POINT('Ctrl Pts',(20.9523407266399,17.9332815566288,10.299825785308));
#140316=CARTESIAN_POINT('Ctrl Pts',(20.9106208944253,17.8608486952342,10.3040091821604));
#140317=CARTESIAN_POINT('Ctrl Pts',(20.8652721209676,17.790326569507,10.3081925790129));
#140318=CARTESIAN_POINT('Ctrl Pts',(20.8164943998508,17.7221020603848,10.3123759758653));
#140319=CARTESIAN_POINT('Ctrl Pts',(20.7677772522461,17.6539622743297,10.3165541776607));
#140320=CARTESIAN_POINT('Ctrl Pts',(20.7156398718341,17.5881148134686,10.3207323794562));
#140321=CARTESIAN_POINT('Ctrl Pts',(20.6603275198124,17.5249210319758,10.3249105812517));
#140322=CARTESIAN_POINT('Ctrl Pts',(20.6050732438256,17.4617936017432,10.3290843960814));
#140323=CARTESIAN_POINT('Ctrl Pts',(20.546650919326,17.4013146604693,10.3332582109111));
#140324=CARTESIAN_POINT('Ctrl Pts',(20.4853475074074,17.3438144419212,10.3374320257408));
#140325=CARTESIAN_POINT('Ctrl Pts',(20.4241713478543,17.2864335811479,10.3415971766513));
#140326=CARTESIAN_POINT('Ctrl Pts',(20.3601263655428,17.2320194202034,10.3457623275617));
#140327=CARTESIAN_POINT('Ctrl Pts',(20.2935357313021,17.1808649545432,10.3499274784722));
#140328=CARTESIAN_POINT('Ctrl Pts',(20.2954164566376,17.1783794293288,9.5499633233039));
#140329=CARTESIAN_POINT('Ctrl Pts',(19.6881794277694,16.7191703127013,9.58795779950289));
#140330=CARTESIAN_POINT('Ctrl Pts',(17.9381456484885,16.3388456091724,9.66834421126236));
#140331=CARTESIAN_POINT('Ctrl Pts',(16.3483940920526,17.7909994706266,9.76278617059814));
#140332=CARTESIAN_POINT('Ctrl Pts',(16.1742904286681,18.9257985710608,9.81923365373494));
#140333=CARTESIAN_POINT('Ctrl Pts',(16.1763511750307,19.2089800092947,9.83328920131125));
#140334=CARTESIAN_POINT('',(16.1740010233873,19.2132890482674,9.76670989018929));
#140335=CARTESIAN_POINT('Ctrl Pts',(20.2935357313021,17.1808649545431,9.48328065833267));
#140336=CARTESIAN_POINT('Ctrl Pts',(20.226846789779,17.129634969907,9.48745093564785));
#140337=CARTESIAN_POINT('Ctrl Pts',(20.1576478303553,17.0817074848001,9.49162121296303));
#140338=CARTESIAN_POINT('Ctrl Pts',(20.0863050570472,17.0373231535749,9.49579149027821));
#140339=CARTESIAN_POINT('Ctrl Pts',(20.0148828973448,16.9928894338572,9.4999664080533));
#140340=CARTESIAN_POINT('Ctrl Pts',(19.9413125544491,16.9520069791659,9.50414132582839));
#140341=CARTESIAN_POINT('Ctrl Pts',(19.8659864662056,16.9148713798379,9.50831624360348));
#140342=CARTESIAN_POINT('Ctrl Pts',(19.7906119470755,16.8777119041871,9.51249384564074));
#140343=CARTESIAN_POINT('Ctrl Pts',(19.713479857659,16.8443042610608,9.516671447678));
#140344=CARTESIAN_POINT('Ctrl Pts',(19.6350021191175,16.8147956720376,9.52084904971526));
#140345=CARTESIAN_POINT('Ctrl Pts',(19.5563968495913,16.7852391298052,9.52503344060388));
#140346=CARTESIAN_POINT('Ctrl Pts',(19.4764420041446,16.7595944266193,9.52921783149249));
#140347=CARTESIAN_POINT('Ctrl Pts',(19.3955636525281,16.7379586469989,9.5334022223811));
#140348=CARTESIAN_POINT('Ctrl Pts',(19.3647456506557,16.7297145188295,9.53499664862326));
#140349=CARTESIAN_POINT('Ctrl Pts',(19.3337936524143,16.7220519237258,9.53659107486542));
#140350=CARTESIAN_POINT('Ctrl Pts',(19.3027314805897,16.7149742583486,9.53818550110757));
#140351=CARTESIAN_POINT('Ctrl Pts',(19.2212075887324,16.6963986471497,9.54237013550062));
#140352=CARTESIAN_POINT('Ctrl Pts',(19.1386209669252,16.6817867038644,9.54655476989367));
#140353=CARTESIAN_POINT('Ctrl Pts',(19.0553917867604,16.6712544774322,9.55073940428672));
#140354=CARTESIAN_POINT('Ctrl Pts',(18.9722810730318,16.6607372423208,9.55491808237066));
#140355=CARTESIAN_POINT('Ctrl Pts',(18.8885300701232,16.654288246849,9.5590967604546));
#140356=CARTESIAN_POINT('Ctrl Pts',(18.804570732492,16.6519728857014,9.56327543853855));
#140357=CARTESIAN_POINT('Ctrl Pts',(18.7191064840744,16.6496160233692,9.56752901642398));
#140358=CARTESIAN_POINT('Ctrl Pts',(18.6334268287623,16.6515425508617,9.57178259430942));
#140359=CARTESIAN_POINT('Ctrl Pts',(18.5479946282975,16.6577663636679,9.57603617219486));
#140360=CARTESIAN_POINT('Ctrl Pts',(18.4642186977459,16.663869515718,9.58020728617281));
#140361=CARTESIAN_POINT('Ctrl Pts',(18.3806811928207,16.6741047825049,9.58437840015076));
#140362=CARTESIAN_POINT('Ctrl Pts',(18.2978184502103,16.6884327252533,9.58854951412871));
#140363=CARTESIAN_POINT('Ctrl Pts',(18.2149835129935,16.7027558601221,9.59271922844909));
#140364=CARTESIAN_POINT('Ctrl Pts',(18.1328233413407,16.7211688651668,9.59688894276946));
#140365=CARTESIAN_POINT('Ctrl Pts',(18.0517667977985,16.7435807292205,9.60105865708984));
#140366=CARTESIAN_POINT('Ctrl Pts',(17.9707131385959,16.7659917957639,9.60522822303388));
#140367=CARTESIAN_POINT('Ctrl Pts',(17.8907634725904,16.7924013149753,9.60939778897792));
#140368=CARTESIAN_POINT('Ctrl Pts',(17.8123328245034,16.8226680260876,9.61356735492197));
#140369=CARTESIAN_POINT('Ctrl Pts',(17.7311446515844,16.8539988774246,9.61788351766089));
#140370=CARTESIAN_POINT('Ctrl Pts',(17.651584793418,16.8894630151456,9.6221996803998));
#140371=CARTESIAN_POINT('Ctrl Pts',(17.5740906315704,16.9288496418883,9.62651584313872));
#140372=CARTESIAN_POINT('Ctrl Pts',(17.499120833894,16.9669532534076,9.6306914073304));
#140373=CARTESIAN_POINT('Ctrl Pts',(17.4260846045835,17.0087274533692,9.63486697152208));
#140374=CARTESIAN_POINT('Ctrl Pts',(17.3553508285749,17.0539356842855,9.63904253571376));
#140375=CARTESIAN_POINT('Ctrl Pts',(17.2810444576937,17.101427275473,9.64342899772631));
#140376=CARTESIAN_POINT('Ctrl Pts',(17.2092797216846,17.152708580808,9.64781545973885));
#140377=CARTESIAN_POINT('Ctrl Pts',(17.1404457653641,17.2074569130478,9.65220192175139));
#140378=CARTESIAN_POINT('Ctrl Pts',(17.0716118090436,17.2622052452876,9.65658838376393));
#140379=CARTESIAN_POINT('Ctrl Pts',(17.0057090169082,17.3204201632973,9.66097484577647));
#140380=CARTESIAN_POINT('Ctrl Pts',(16.9430809195061,17.3817354354488,9.66536130778901));
#140381=CARTESIAN_POINT('Ctrl Pts',(16.8827886985013,17.4407637964061,9.66958416538902));
#140382=CARTESIAN_POINT('Ctrl Pts',(16.8252872091303,17.5029045422553,9.67380702298903));
#140383=CARTESIAN_POINT('Ctrl Pts',(16.7709203169311,17.5678572314245,9.67802988058904));
#140384=CARTESIAN_POINT('Ctrl Pts',(16.7179063153622,17.6311936081462,9.68214765466764));
#140385=CARTESIAN_POINT('Ctrl Pts',(16.6678730797622,17.6972032456021,9.68626542874624));
#140386=CARTESIAN_POINT('Ctrl Pts',(16.6211045875939,17.7655682388182,9.69038320282484));
#140387=CARTESIAN_POINT('Ctrl Pts',(16.57438033231,17.833868567681,9.69449708202705));
#140388=CARTESIAN_POINT('Ctrl Pts',(16.530914960773,17.9045194435154,9.69861096122926));
#140389=CARTESIAN_POINT('Ctrl Pts',(16.4909521572678,17.9771700379653,9.70272484043147));
#140390=CARTESIAN_POINT('Ctrl Pts',(16.451014356568,18.0497751784301,9.70683614577719));
#140391=CARTESIAN_POINT('Ctrl Pts',(16.4145750025456,18.1243771397533,9.7109474511229));
#140392=CARTESIAN_POINT('Ctrl Pts',(16.3818335581791,18.2005975900802,9.71505875646862));
#140393=CARTESIAN_POINT('Ctrl Pts',(16.3475554603697,18.2803952930204,9.71936301761201));
#140394=CARTESIAN_POINT('Ctrl Pts',(16.3173311789841,18.3619666588744,9.7236672787554));
#140395=CARTESIAN_POINT('Ctrl Pts',(16.2913340385439,18.4448518415191,9.72797153989879));
#140396=CARTESIAN_POINT('Ctrl Pts',(16.2665001036005,18.5240284432035,9.73208321292914));
#140397=CARTESIAN_POINT('Ctrl Pts',(16.2455232446819,18.6044033134949,9.73619488595948));
#140398=CARTESIAN_POINT('Ctrl Pts',(16.2285034541843,18.685560128173,9.74030655898983));
#140399=CARTESIAN_POINT('Ctrl Pts',(16.2114791195103,18.7667386112068,9.74441932981085));
#140400=CARTESIAN_POINT('Ctrl Pts',(16.1984140354435,18.84869898642,9.74853210063186));
#140401=CARTESIAN_POINT('Ctrl Pts',(16.1893567554131,18.9310165044539,9.75264487145288));
#140402=CARTESIAN_POINT('Ctrl Pts',(16.1802905487374,19.0134151527258,9.7567616957255));
#140403=CARTESIAN_POINT('Ctrl Pts',(16.1752400549859,19.0961711731434,9.76087851999813));
#140404=CARTESIAN_POINT('Ctrl Pts',(16.1742017924823,19.1788575547115,9.76499534427075));
#140405=CARTESIAN_POINT('Ctrl Pts',(16.1740576564023,19.1903364349233,9.76556685957693));
#140406=CARTESIAN_POINT('Ctrl Pts',(16.1739907628404,19.2018139780891,9.76613837488311));
#140407=CARTESIAN_POINT('Ctrl Pts',(16.1740010233873,19.2132890482674,9.76670989018929));
#140408=CARTESIAN_POINT('Ctrl Pts',(16.174001023388,19.2132890490549,9.76670989022851));
#140409=CARTESIAN_POINT('Ctrl Pts',(16.1741079389015,19.3328599270272,9.77266511192853));
#140410=CARTESIAN_POINT('Ctrl Pts',(16.1825955516607,19.4520702292312,9.77862033362856));
#140411=CARTESIAN_POINT('Ctrl Pts',(16.1992930219785,19.5699714968759,9.78457555532858));
#140412=CARTESIAN_POINT('Ctrl Pts',(16.2067339930653,19.6225123852222,9.78722940837587));
#140413=CARTESIAN_POINT('Ctrl Pts',(16.2158047738395,19.6747937484515,9.78988326142315));
#140414=CARTESIAN_POINT('Ctrl Pts',(16.2264874578014,19.7267333135613,9.79253711447044));
#140415=CARTESIAN_POINT('Ctrl Pts',(16.2433320704913,19.8086323813112,9.79672174886349));
#140416=CARTESIAN_POINT('Ctrl Pts',(16.2642246666771,19.8898577370365,9.80090638325653));
#140417=CARTESIAN_POINT('Ctrl Pts',(16.2890969179465,19.969978866218,9.80509101764958));
#140418=CARTESIAN_POINT('Ctrl Pts',(16.3139337666449,20.0499859528891,9.80926969573353));
#140419=CARTESIAN_POINT('Ctrl Pts',(16.3427388836329,20.1288914993742,9.81344837381748));
#140420=CARTESIAN_POINT('Ctrl Pts',(16.3753929533288,20.2062752380084,9.81762705190142));
#140421=CARTESIAN_POINT('Ctrl Pts',(16.4086323237558,20.2850460245429,9.82188062978686));
#140422=CARTESIAN_POINT('Ctrl Pts',(16.4458598919279,20.3622394375428,9.82613420767229));
#140423=CARTESIAN_POINT('Ctrl Pts',(16.4868966678982,20.4374283977701,9.83038778555773));
#140424=CARTESIAN_POINT('Ctrl Pts',(16.5271378658896,20.5111596732842,9.83455889953568));
#140425=CARTESIAN_POINT('Ctrl Pts',(16.5710416613174,20.5829631005169,9.83873001351363));
#140426=CARTESIAN_POINT('Ctrl Pts',(16.6183914981669,20.6524578269833,9.84290112749158));
#140427=CARTESIAN_POINT('Ctrl Pts',(16.6657254463213,20.7219292338231,9.84707084181195));
#140428=CARTESIAN_POINT('Ctrl Pts',(16.7165028805481,20.7890930986176,9.85124055613233));
#140429=CARTESIAN_POINT('Ctrl Pts',(16.7704633948897,20.8535967248207,9.8554102704527));
#140430=CARTESIAN_POINT('Ctrl Pts',(16.8244219890847,20.9180980557081,9.85957983639674));
#140431=CARTESIAN_POINT('Ctrl Pts',(16.8815631423605,20.9799389839165,9.86374940234079));
#140432=CARTESIAN_POINT('Ctrl Pts',(16.9415864376591,21.0388002137915,9.86791896828483));
#140433=CARTESIAN_POINT('Ctrl Pts',(17.0037200779736,21.0997309318957,9.87223513102375));
#140434=CARTESIAN_POINT('Ctrl Pts',(17.0689419268742,21.1574681514489,9.87655129376267));
#140435=CARTESIAN_POINT('Ctrl Pts',(17.1368790142891,21.2117010163945,9.88086745650159));
#140436=CARTESIAN_POINT('Ctrl Pts',(17.2026030582273,21.2641672514687,9.88504302069327));
#140437=CARTESIAN_POINT('Ctrl Pts',(17.270867749702,21.3133536974898,9.88921858488495));
#140438=CARTESIAN_POINT('Ctrl Pts',(17.3413050297812,21.3590225138316,9.89339414907663));
#140439=CARTESIAN_POINT('Ctrl Pts',(17.4152999294285,21.4069979535195,9.89778061108917));
#140440=CARTESIAN_POINT('Ctrl Pts',(17.4916921547949,21.4510907819032,9.9021670731017));
#140441=CARTESIAN_POINT('Ctrl Pts',(17.5700268579946,21.4910803768047,9.90655353511425));
#140442=CARTESIAN_POINT('Ctrl Pts',(17.6483615611942,21.5310699717063,9.91093999712678));
#140443=CARTESIAN_POINT('Ctrl Pts',(17.7286381814852,21.5669561657755,9.91532645913933));
#140444=CARTESIAN_POINT('Ctrl Pts',(17.8103811197832,21.5985778865007,9.91971292115187));
#140445=CARTESIAN_POINT('Ctrl Pts',(17.8883629443181,21.6287446449807,9.92389755554492));
#140446=CARTESIAN_POINT('Ctrl Pts',(17.9679693803479,21.6551430224068,9.92808218993796));
#140447=CARTESIAN_POINT('Ctrl Pts',(18.0488014484185,21.6775974428168,9.93226682433101));
#140448=CARTESIAN_POINT('Ctrl Pts',(18.1295184620453,21.7000199021387,9.93644550241496));
#140449=CARTESIAN_POINT('Ctrl Pts',(18.2114572030592,21.7185094330108,9.9406241804989));
#140450=CARTESIAN_POINT('Ctrl Pts',(18.2941997096014,21.7329388780391,9.94480285858285));
#140451=CARTESIAN_POINT('Ctrl Pts',(18.3784253161073,21.7476269604994,9.94905643646828));
#140452=CARTESIAN_POINT('Ctrl Pts',(18.4634833368926,21.758107797425,9.95331001435372));
#140453=CARTESIAN_POINT('Ctrl Pts',(18.5489177820416,21.7643007211442,9.95756359223915));
#140454=CARTESIAN_POINT('Ctrl Pts',(18.6326959137597,21.7703735829526,9.96173470621711));
#140455=CARTESIAN_POINT('Ctrl Pts',(18.7168355246874,21.7723232722254,9.96590582019506));
#140456=CARTESIAN_POINT('Ctrl Pts',(18.8008991604928,21.7701257300737,9.97007693417301));
#140457=CARTESIAN_POINT('Ctrl Pts',(18.8849345879332,21.7679289253285,9.97424664849338));
#140458=CARTESIAN_POINT('Ctrl Pts',(18.96889363139,21.7615876649968,9.97841636281375));
#140459=CARTESIAN_POINT('Ctrl Pts',(19.0523387760778,21.7511300013277,9.98258607713412));
#140460=CARTESIAN_POINT('Ctrl Pts',(19.1357809514292,21.7406727097872,9.98675564307817));
#140461=CARTESIAN_POINT('Ctrl Pts',(19.218708808014,21.7260993641991,9.99092520902222));
#140462=CARTESIAN_POINT('Ctrl Pts',(19.3006912586606,21.7074897390852,9.99509477496627));
#140463=CARTESIAN_POINT('Ctrl Pts',(19.3855561111356,21.6882258225098,9.99941093770519));
#140464=CARTESIAN_POINT('Ctrl Pts',(19.4694073254465,21.6646366310369,10.0037271004441));
#140465=CARTESIAN_POINT('Ctrl Pts',(19.5517816392177,21.6368675129855,10.008043263183));
#140466=CARTESIAN_POINT('Ctrl Pts',(19.631472618382,21.6100029710338,10.0122188273747));
#140467=CARTESIAN_POINT('Ctrl Pts',(19.7097810183149,21.5792268589616,10.0163943915664));
#140468=CARTESIAN_POINT('Ctrl Pts',(19.7863076293697,21.5447199174645,10.0205699557581));
#140469=CARTESIAN_POINT('Ctrl Pts',(19.8666994176241,21.5084701123847,10.0249564177706));
#140470=CARTESIAN_POINT('Ctrl Pts',(19.9451241711511,21.4681029519008,10.0293428797831));
#140471=CARTESIAN_POINT('Ctrl Pts',(20.0211501810795,21.423881472503,10.0337293417957));
#140472=CARTESIAN_POINT('Ctrl Pts',(20.0971761910079,21.3796599931052,10.0381158038082));
#140473=CARTESIAN_POINT('Ctrl Pts',(20.1708030131037,21.3315845757053,10.0425022658208));
#140474=CARTESIAN_POINT('Ctrl Pts',(20.2416377781111,21.2799679383722,10.0468887278333));
#140475=CARTESIAN_POINT('Ctrl Pts',(20.3092133305781,21.2307262590371,10.0510733622263));
#140476=CARTESIAN_POINT('Ctrl Pts',(20.3744996423272,21.1780787853436,10.0552579966194));
#140477=CARTESIAN_POINT('Ctrl Pts',(20.4371331217481,21.1222659599345,10.0594426310124));
#140478=CARTESIAN_POINT('Ctrl Pts',(20.4996774501636,21.0665325771742,10.0636213090964));
#140479=CARTESIAN_POINT('Ctrl Pts',(20.559576106015,21.0076430954477,10.0677999871803));
#140480=CARTESIAN_POINT('Ctrl Pts',(20.6164959352301,20.9458801266491,10.0719786652643));
#140481=CARTESIAN_POINT('Ctrl Pts',(20.6744360114764,20.8830101010231,10.0762322431497));
#140482=CARTESIAN_POINT('Ctrl Pts',(20.7292890301006,20.8171628445093,10.0804858210351));
#140483=CARTESIAN_POINT('Ctrl Pts',(20.7807403436638,20.7486781085842,10.0847393989206));
#140484=CARTESIAN_POINT('Ctrl Pts',(20.8311941731145,20.681521082902,10.0889105128985));
#140485=CARTESIAN_POINT('Ctrl Pts',(20.8783767288092,20.6118283153185,10.0930816268765));
#140486=CARTESIAN_POINT('Ctrl Pts',(20.9220309952966,20.539954613078,10.0972527408544));
#140487=CARTESIAN_POINT('Ctrl Pts',(20.9656706131734,20.4681050287524,10.1014224551748));
#140488=CARTESIAN_POINT('Ctrl Pts',(21.0057840545746,20.3940763560658,10.1055921694952));
#140489=CARTESIAN_POINT('Ctrl Pts',(21.0421580885472,20.3182516598651,10.1097618838155));
#140490=CARTESIAN_POINT('Ctrl Pts',(21.0785308281756,20.2424296618325,10.1139314497596));
#140491=CARTESIAN_POINT('Ctrl Pts',(21.111164226736,20.1648121825011,10.1181010157036));
#140492=CARTESIAN_POINT('Ctrl Pts',(21.1398920226671,20.0858048783968,10.1222705816477));
#140493=CARTESIAN_POINT('Ctrl Pts',(21.1696298524636,20.0040197749462,10.1265867443866));
#140494=CARTESIAN_POINT('Ctrl Pts',(21.1951821474478,19.9207457915132,10.1309029071255));
#140495=CARTESIAN_POINT('Ctrl Pts',(21.2164203674167,19.8364511327311,10.1352190698644));
#140496=CARTESIAN_POINT('Ctrl Pts',(21.236966754604,19.7549023635926,10.1393946340561));
#140497=CARTESIAN_POINT('Ctrl Pts',(21.253475766424,19.6723988660725,10.1435701982478));
#140498=CARTESIAN_POINT('Ctrl Pts',(21.2658832925888,19.5893741438177,10.1477457624395));
#140499=CARTESIAN_POINT('Ctrl Pts',(21.278917493404,19.5021560402143,10.152132224452));
#140500=CARTESIAN_POINT('Ctrl Pts',(21.2874249313198,19.4143632551381,10.1565186864645));
#140501=CARTESIAN_POINT('Ctrl Pts',(21.291393102574,19.3265011640939,10.1609051484771));
#140502=CARTESIAN_POINT('Ctrl Pts',(21.2953612738282,19.2386390730496,10.1652916104896));
#140503=CARTESIAN_POINT('Ctrl Pts',(21.294790258252,19.150708255748,10.1696780725022));
#140504=CARTESIAN_POINT('Ctrl Pts',(21.2897303495757,19.0632083214199,10.1740645345147));
#140505=CARTESIAN_POINT('Ctrl Pts',(21.2849027735544,18.9797260667271,10.1782495861007));
#140506=CARTESIAN_POINT('Ctrl Pts',(21.2759715218878,18.8963252255079,10.1824346376866));
#140507=CARTESIAN_POINT('Ctrl Pts',(21.2629419677493,18.8134417982782,10.1866196892726));
#140508=CARTESIAN_POINT('Ctrl Pts',(21.2499348195045,18.7307008991227,10.1907975441564));
#140509=CARTESIAN_POINT('Ctrl Pts',(21.2328434536036,18.6484760952755,10.1949753990401));
#140510=CARTESIAN_POINT('Ctrl Pts',(21.2117251381584,18.5672002331953,10.1991532539239));
#140511=CARTESIAN_POINT('Ctrl Pts',(21.1906274886263,18.486003905863,10.2033270204519));
#140512=CARTESIAN_POINT('Ctrl Pts',(21.1655108283412,18.4057551192369,10.20750078698));
#140513=CARTESIAN_POINT('Ctrl Pts',(21.1364836587692,18.3268776841708,10.211674553508));
#140514=CARTESIAN_POINT('Ctrl Pts',(21.1074761860984,18.248053772789,10.2158454878527));
#140515=CARTESIAN_POINT('Ctrl Pts',(21.0745636328033,18.1705997951948,10.2200164221973));
#140516=CARTESIAN_POINT('Ctrl Pts',(21.0379042545255,18.0949242024042,10.224187356542));
#140517=CARTESIAN_POINT('Ctrl Pts',(21.0012587547907,18.0192772589526,10.2283567118503));
#140518=CARTESIAN_POINT('Ctrl Pts',(20.9608694496223,17.9454077756907,10.2325260671586));
#140519=CARTESIAN_POINT('Ctrl Pts',(20.9169420720105,17.8737027592017,10.2366954224669));
#140520=CARTESIAN_POINT('Ctrl Pts',(20.8729998723135,17.8019735478277,10.2408661846094));
#140521=CARTESIAN_POINT('Ctrl Pts',(20.8255174487893,17.7324106591192,10.245036946752));
#140522=CARTESIAN_POINT('Ctrl Pts',(20.7747452964143,17.6653743547796,10.2492077088945));
#140523=CARTESIAN_POINT('Ctrl Pts',(20.7239654366808,17.5983278741366,10.2533791041707));
#140524=CARTESIAN_POINT('Ctrl Pts',(20.6698951413505,17.5338091011221,10.257550499447));
#140525=CARTESIAN_POINT('Ctrl Pts',(20.6128256045716,17.4721456795907,10.2617218947232));
#140526=CARTESIAN_POINT('Ctrl Pts',(20.5556935666741,17.4104147258338,10.2658978584064));
#140527=CARTESIAN_POINT('Ctrl Pts',(20.4955560493931,17.3515456983365,10.2700738220896));
#140528=CARTESIAN_POINT('Ctrl Pts',(20.4327411706385,17.2958293978922,10.2742497857728));
#140529=CARTESIAN_POINT('Ctrl Pts',(20.3876731334338,17.2558544054841,10.2772459308004));
#140530=CARTESIAN_POINT('Ctrl Pts',(20.3412276435305,17.2175015523797,10.280242075828));
#140531=CARTESIAN_POINT('Ctrl Pts',(20.2935357313021,17.1808649545432,10.2832382208556));
#140532=CARTESIAN_POINT('Origin',(18.734,19.211,-1.76670989022852));
#140533=CARTESIAN_POINT('',(20.2922817525491,17.1824654639373,11.1497835189211));
#140534=CARTESIAN_POINT('',(20.2948050193864,17.1791827951408,11.0834063379994));
#140535=CARTESIAN_POINT('',(20.2935357313021,17.1808649545432,-1.76670989022852));
#140536=CARTESIAN_POINT('',(16.1740004874608,19.2125798097913,10.6332901097715));
#140537=CARTESIAN_POINT('Ctrl Pts',(16.1772048569635,19.2125971087803,10.6332910657481));
#140538=CARTESIAN_POINT('Ctrl Pts',(16.1753928896008,19.5356421709025,10.6493117789495));
#140539=CARTESIAN_POINT('Ctrl Pts',(16.3822354944161,20.7112478477878,10.7077244277114));
#140540=CARTESIAN_POINT('Ctrl Pts',(18.1490152348825,22.181030878927,10.8085290120338));
#140541=CARTESIAN_POINT('Ctrl Pts',(20.9146847933563,21.3105009952899,10.9357048187152));
#140542=CARTESIAN_POINT('Ctrl Pts',(21.5989574420292,18.8090198185379,11.0494563210109));
#140543=CARTESIAN_POINT('Ctrl Pts',(20.7519189128693,17.541844350173,11.1208158877462));
#140544=CARTESIAN_POINT('Ctrl Pts',(20.2922817525494,17.1824654639375,11.1497835189211));
#140545=CARTESIAN_POINT('Ctrl Pts',(20.2935357313021,17.1808649545432,10.3499274784722));
#140546=CARTESIAN_POINT('Ctrl Pts',(20.2268718754302,17.1296542405312,10.3540972092932));
#140547=CARTESIAN_POINT('Ctrl Pts',(20.1576571101332,17.081710698567,10.3582669401141));
#140548=CARTESIAN_POINT('Ctrl Pts',(20.0862488639036,17.0372881952588,10.3624366709351));
#140549=CARTESIAN_POINT('Ctrl Pts',(20.0148436078252,16.9928675520998,10.3666062271526));
#140550=CARTESIAN_POINT('Ctrl Pts',(19.9412454444601,16.9519678967869,10.3707757833701));
#140551=CARTESIAN_POINT('Ctrl Pts',(19.8658394035043,16.9147988840968,10.3749453395876));
#140552=CARTESIAN_POINT('Ctrl Pts',(19.7873866918356,16.8761281118533,10.3792833606211));
#140553=CARTESIAN_POINT('Ctrl Pts',(19.706977385856,16.8414961001808,10.3836213816546));
#140554=CARTESIAN_POINT('Ctrl Pts',(19.6250697784902,16.8110844494313,10.3879594026881));
#140555=CARTESIAN_POINT('Ctrl Pts',(19.5462302936279,16.7818119684493,10.3921349286813));
#140556=CARTESIAN_POINT('Ctrl Pts',(19.4660032236778,16.7564493936647,10.3963104546746));
#140557=CARTESIAN_POINT('Ctrl Pts',(19.3848125373651,16.7351076272971,10.4004859806679));
#140558=CARTESIAN_POINT('Ctrl Pts',(19.3035638000568,16.7137506016573,10.4046644921445));
#140559=CARTESIAN_POINT('Ctrl Pts',(19.2213505247295,16.6964201991012,10.4088430036211));
#140560=CARTESIAN_POINT('Ctrl Pts',(19.1386057357174,16.6831759953223,10.4130215150977));
#140561=CARTESIAN_POINT('Ctrl Pts',(19.0557327160416,16.6699112668306,10.4172065020673));
#140562=CARTESIAN_POINT('Ctrl Pts',(18.9723269953436,16.6607454158577,10.4213914890369));
#140563=CARTESIAN_POINT('Ctrl Pts',(18.8888248773207,16.6556860745962,10.4255764760064));
#140564=CARTESIAN_POINT('Ctrl Pts',(18.8793465361394,16.6551117878144,10.4260515146675));
#140565=CARTESIAN_POINT('Ctrl Pts',(18.8698669499041,16.6545903564495,10.4265265533285));
#140566=CARTESIAN_POINT('Ctrl Pts',(18.8603867536229,16.6541217493771,10.4270015919895));
#140567=CARTESIAN_POINT('Ctrl Pts',(18.7768753288337,16.6499937711024,10.4311862263825));
#140568=CARTESIAN_POINT('Ctrl Pts',(18.693006041295,16.6499538232249,10.4353708607756));
#140569=CARTESIAN_POINT('Ctrl Pts',(18.6092128353627,16.6540431830901,10.4395554951686));
#140570=CARTESIAN_POINT('Ctrl Pts',(18.5255388986874,16.6581267222578,10.4437341732526));
#140571=CARTESIAN_POINT('Ctrl Pts',(18.4419412840711,16.6663278722549,10.4479128513365));
#140572=CARTESIAN_POINT('Ctrl Pts',(18.3588567381408,16.6786359793502,10.4520915294205));
#140573=CARTESIAN_POINT('Ctrl Pts',(18.2742829614365,16.6911647004195,10.4563451073059));
#140574=CARTESIAN_POINT('Ctrl Pts',(18.1902413093997,16.7079490849927,10.4605986851913));
#140575=CARTESIAN_POINT('Ctrl Pts',(18.1071900176366,16.7289223932339,10.4648522630768));
#140576=CARTESIAN_POINT('Ctrl Pts',(18.0257488372256,16.7494890929688,10.4690233770547));
#140577=CARTESIAN_POINT('Ctrl Pts',(17.9452604262029,16.7740836270437,10.4731944910327));
#140578=CARTESIAN_POINT('Ctrl Pts',(17.8661476315623,16.8025913414462,10.4773656050106));
#140579=CARTESIAN_POINT('Ctrl Pts',(17.7870613839839,16.8310894898098,10.481535319331));
#140580=CARTESIAN_POINT('Ctrl Pts',(17.7093502684716,16.8634980548293,10.4857050336514));
#140581=CARTESIAN_POINT('Ctrl Pts',(17.6334208106691,16.8996528932218,10.4898747479717));
#140582=CARTESIAN_POINT('Ctrl Pts',(17.5574940547626,16.9358064450701,10.4940443139158));
#140583=CARTESIAN_POINT('Ctrl Pts',(17.4833492454957,16.975705806696,10.4982138798598));
#140584=CARTESIAN_POINT('Ctrl Pts',(17.4113705501162,17.0191397539304,10.5023834458039));
#140585=CARTESIAN_POINT('Ctrl Pts',(17.3368611726026,17.0641007851681,10.5066996085428));
#140586=CARTESIAN_POINT('Ctrl Pts',(17.2646735157619,17.1128493061262,10.5110157712817));
#140587=CARTESIAN_POINT('Ctrl Pts',(17.1952016813755,17.1651017291668,10.5153319340206));
#140588=CARTESIAN_POINT('Ctrl Pts',(17.1279928846871,17.2156520350228,10.5195074982123));
#140589=CARTESIAN_POINT('Ctrl Pts',(17.063326023611,17.2694811317354,10.523683062404));
#140590=CARTESIAN_POINT('Ctrl Pts',(17.0015232692733,17.3262919649212,10.5278586265956));
#140591=CARTESIAN_POINT('Ctrl Pts',(16.936599004736,17.3859721782365,10.5322450886082));
#140592=CARTESIAN_POINT('Ctrl Pts',(16.8748361916359,17.4489428422736,10.5366315506207));
#140593=CARTESIAN_POINT('Ctrl Pts',(16.8165619874413,17.5148185627726,10.5410180126333));
#140594=CARTESIAN_POINT('Ctrl Pts',(16.7582877832466,17.5806942832716,10.5454044746458));
#140595=CARTESIAN_POINT('Ctrl Pts',(16.7035024899566,17.6494745589998,10.5497909366583));
#140596=CARTESIAN_POINT('Ctrl Pts',(16.6524807786037,17.7207390393097,10.5541773986709));
#140597=CARTESIAN_POINT('Ctrl Pts',(16.6033728384837,17.789330463214,10.5583993290636));
#140598=CARTESIAN_POINT('Ctrl Pts',(16.5575691753499,17.8604769154311,10.5626212594564));
#140599=CARTESIAN_POINT('Ctrl Pts',(16.5153433201941,17.9338302629828,10.5668431898491));
#140600=CARTESIAN_POINT('Ctrl Pts',(16.4731798646834,18.0070752119517,10.5710588812454));
#140601=CARTESIAN_POINT('Ctrl Pts',(16.4345839361663,18.082520192057,10.5752745726418));
#140602=CARTESIAN_POINT('Ctrl Pts',(16.3997870211447,18.1597865253224,10.5794902640381));
#140603=CARTESIAN_POINT('Ctrl Pts',(16.3650317212893,18.2369604523703,10.5837009137031));
#140604=CARTESIAN_POINT('Ctrl Pts',(16.3340665899183,18.3159509969196,10.587911563368));
#140605=CARTESIAN_POINT('Ctrl Pts',(16.3070776023613,18.3963542635971,10.592122213033));
#140606=CARTESIAN_POINT('Ctrl Pts',(16.2801155537106,18.4766772762055,10.5963286598617));
#140607=CARTESIAN_POINT('Ctrl Pts',(16.2571218975382,18.5584097818784,10.6005351066903));
#140608=CARTESIAN_POINT('Ctrl Pts',(16.238234292144,18.6411284956326,10.604741553519));
#140609=CARTESIAN_POINT('Ctrl Pts',(16.2193575415099,18.7237996707085,10.6089455828908));
#140610=CARTESIAN_POINT('Ctrl Pts',(16.2045822501751,18.807455489948,10.6131496122625));
#140611=CARTESIAN_POINT('Ctrl Pts',(16.19399578679,18.8916591211959,10.6173536416343));
#140612=CARTESIAN_POINT('Ctrl Pts',(16.1834116610726,18.975844158877,10.6215567426863));
#140613=CARTESIAN_POINT('Ctrl Pts',(16.1770145819501,19.0605763228053,10.6257598437382));
#140614=CARTESIAN_POINT('Ctrl Pts',(16.1748403468596,19.145411359684,10.6299629447902));
#140615=CARTESIAN_POINT('Ctrl Pts',(16.1742666403856,19.1677964320708,10.631071999784));
#140616=CARTESIAN_POINT('Ctrl Pts',(16.1739866695752,19.1901886456578,10.6321810547777));
#140617=CARTESIAN_POINT('Ctrl Pts',(16.1740004874608,19.2125798097913,10.6332901097715));
#140618=CARTESIAN_POINT('',(16.1739802642219,19.2096989559289,10.5667098967469));
#140619=CARTESIAN_POINT('Ctrl Pts',(20.2935357313021,17.1808649545432,10.2832382208556));
#140620=CARTESIAN_POINT('Ctrl Pts',(20.2269313029742,17.1296998923603,10.2874225053061));
#140621=CARTESIAN_POINT('Ctrl Pts',(20.1578950951659,17.0818841390033,10.2916067897566));
#140622=CARTESIAN_POINT('Ctrl Pts',(20.0868063265307,17.0376350874972,10.2957910742071));
#140623=CARTESIAN_POINT('Ctrl Pts',(20.055946276678,17.0184263156809,10.2976074965368));
#140624=CARTESIAN_POINT('Ctrl Pts',(20.0246997275378,16.9998890870178,10.2994239188665));
#140625=CARTESIAN_POINT('Ctrl Pts',(19.9930989518198,16.9820383965787,10.3012403411962));
#140626=CARTESIAN_POINT('Ctrl Pts',(19.9202977696528,16.9409143628506,10.3054249755892));
#140627=CARTESIAN_POINT('Ctrl Pts',(19.8453442312191,16.9032842410815,10.3096096099823));
#140628=CARTESIAN_POINT('Ctrl Pts',(19.7686077403709,16.8693794450073,10.3137942443753));
#140629=CARTESIAN_POINT('Ctrl Pts',(19.6919804744194,16.8355229082136,10.3179729224593));
#140630=CARTESIAN_POINT('Ctrl Pts',(19.6135757141379,16.8053813489309,10.3221516005432));
#140631=CARTESIAN_POINT('Ctrl Pts',(19.5337886464594,16.7791410153969,10.3263302786272));
#140632=CARTESIAN_POINT('Ctrl Pts',(19.4525714529348,16.752430342743,10.3305838565126));
#140633=CARTESIAN_POINT('Ctrl Pts',(19.3699223286582,16.7297623675601,10.334837434398));
#140634=CARTESIAN_POINT('Ctrl Pts',(19.2862808103369,16.7112828346924,10.3390910122835));
#140635=CARTESIAN_POINT('Ctrl Pts',(19.2042608460612,16.6931615636291,10.3432621262614));
#140636=CARTESIAN_POINT('Ctrl Pts',(19.1212870932384,16.6790678856914,10.3474332402394));
#140637=CARTESIAN_POINT('Ctrl Pts',(19.0377889319358,16.6690888519003,10.3516043542173));
#140638=CARTESIAN_POINT('Ctrl Pts',(18.9543187892476,16.6591131666705,10.3557740685377));
#140639=CARTESIAN_POINT('Ctrl Pts',(18.8703250439618,16.6532494380237,10.3599437828581));
#140640=CARTESIAN_POINT('Ctrl Pts',(18.7862446699247,16.6515331620698,10.3641134971784));
#140641=CARTESIAN_POINT('Ctrl Pts',(18.7021672878281,16.6498169471884,10.3682830631225));
#140642=CARTESIAN_POINT('Ctrl Pts',(18.6180037430637,16.652247900101,10.3724526290665));
#140643=CARTESIAN_POINT('Ctrl Pts',(18.5341921271336,16.6588094087744,10.3766221950106));
#140644=CARTESIAN_POINT('Ctrl Pts',(18.4474337981802,16.6656016119982,10.3809383577495));
#140645=CARTESIAN_POINT('Ctrl Pts',(18.361053131965,16.6768201947949,10.3852545204884));
#140646=CARTESIAN_POINT('Ctrl Pts',(18.2755295374794,16.6923883119869,10.3895706832273));
#140647=CARTESIAN_POINT('Ctrl Pts',(18.1927918650888,16.7074492993989,10.393746247419));
#140648=CARTESIAN_POINT('Ctrl Pts',(18.1108567316689,16.7265806476473,10.3979218116107));
#140649=CARTESIAN_POINT('Ctrl Pts',(18.030145283277,16.749661230601,10.4020973758024));
#140650=CARTESIAN_POINT('Ctrl Pts',(17.9453572914999,16.7739075589308,10.4064838378149));
#140651=CARTESIAN_POINT('Ctrl Pts',(17.8619204024433,16.8025123689437,10.4108702998274));
#140652=CARTESIAN_POINT('Ctrl Pts',(17.7802998178505,16.8352778018952,10.41525676184));
#140653=CARTESIAN_POINT('Ctrl Pts',(17.6986792332576,16.8680432348467,10.4196432238525));
#140654=CARTESIAN_POINT('Ctrl Pts',(17.6188754477656,16.9049689780518,10.4240296858651));
#140655=CARTESIAN_POINT('Ctrl Pts',(17.5413224142637,16.9458023979171,10.4284161478776));
#140656=CARTESIAN_POINT('Ctrl Pts',(17.4673377107945,16.9847570116046,10.4326007822707));
#140657=CARTESIAN_POINT('Ctrl Pts',(17.3951258047347,17.0274126045708,10.4367854166637));
#140658=CARTESIAN_POINT('Ctrl Pts',(17.3250812297131,17.0735838265015,10.4409700510568));
#140659=CARTESIAN_POINT('Ctrl Pts',(17.2551363544742,17.1196893294125,10.4451487291407));
#140660=CARTESIAN_POINT('Ctrl Pts',(17.1873530634461,17.1693002706272,10.4493274072246));
#140661=CARTESIAN_POINT('Ctrl Pts',(17.1221018691139,17.2221851731129,10.4535060853086));
#140662=CARTESIAN_POINT('Ctrl Pts',(17.0556810940185,17.276017999468,10.457759663194));
#140663=CARTESIAN_POINT('Ctrl Pts',(16.9918845107683,17.3332430884428,10.4620132410795));
#140664=CARTESIAN_POINT('Ctrl Pts',(16.9310725805955,17.3935697481445,10.4662668189649));
#140665=CARTESIAN_POINT('Ctrl Pts',(16.8714396083539,17.4527268578301,10.4704379329429));
#140666=CARTESIAN_POINT('Ctrl Pts',(16.8146769368999,17.5148660125131,10.4746090469208));
#140667=CARTESIAN_POINT('Ctrl Pts',(16.7610901776527,17.5796732905743,10.4787801608988));
#140668=CARTESIAN_POINT('Ctrl Pts',(16.7075213999602,17.6444588219275,10.4829498752191));
#140669=CARTESIAN_POINT('Ctrl Pts',(16.6571267108676,17.7119103443124,10.4871195895395));
#140670=CARTESIAN_POINT('Ctrl Pts',(16.610172482641,17.7816796452478,10.4912893038599));
#140671=CARTESIAN_POINT('Ctrl Pts',(16.5632199252474,17.8514464634922,10.4954588698039));
#140672=CARTESIAN_POINT('Ctrl Pts',(16.5197078414472,17.9235305141742,10.499628435748));
#140673=CARTESIAN_POINT('Ctrl Pts',(16.4798593937703,17.9975544398918,10.503798001692));
#140674=CARTESIAN_POINT('Ctrl Pts',(16.4386099238315,18.0741809555191,10.5081141644309));
#140675=CARTESIAN_POINT('Ctrl Pts',(16.4012867603008,18.1528858318599,10.5124303271698));
#140676=CARTESIAN_POINT('Ctrl Pts',(16.3680847835396,18.2332243669834,10.5167464899088));
#140677=CARTESIAN_POINT('Ctrl Pts',(16.3359643576791,18.3109458827753,10.5209220541004));
#140678=CARTESIAN_POINT('Ctrl Pts',(16.3077008602571,18.3901957994176,10.5250976182921));
#140679=CARTESIAN_POINT('Ctrl Pts',(16.2834204017388,18.4705544364466,10.5292731824838));
#140680=CARTESIAN_POINT('Ctrl Pts',(16.2579135949821,18.5549717971974,10.5336596444963));
#140681=CARTESIAN_POINT('Ctrl Pts',(16.236802907853,18.6406122578469,10.5380461065089));
#140682=CARTESIAN_POINT('Ctrl Pts',(16.2201737773398,18.726977560163,10.5424325685214));
#140683=CARTESIAN_POINT('Ctrl Pts',(16.2035446468265,18.8133428624791,10.546819030534));
#140684=CARTESIAN_POINT('Ctrl Pts',(16.1913970777482,18.9004324212999,10.5512054925465));
#140685=CARTESIAN_POINT('Ctrl Pts',(16.1837535357011,18.9877446051473,10.555591954559));
#140686=CARTESIAN_POINT('Ctrl Pts',(16.1772957565522,19.0615118189368,10.5592979331155));
#140687=CARTESIAN_POINT('Ctrl Pts',(16.174038011382,19.1355632322755,10.563003911672));
#140688=CARTESIAN_POINT('Ctrl Pts',(16.1740003306697,19.2096988355574,10.5667098902285));
#140689=CARTESIAN_POINT('Ctrl Pts',(16.1705863812103,19.2097193146384,10.566710999223));
#140690=CARTESIAN_POINT('Ctrl Pts',(16.1754041849044,19.9846332056276,10.6053965865622));
#140691=CARTESIAN_POINT('Ctrl Pts',(16.9631830908079,21.6171665575917,10.6864741094618));
#140692=CARTESIAN_POINT('Ctrl Pts',(19.742230707443,22.0652534613628,10.8099435679219));
#140693=CARTESIAN_POINT('Ctrl Pts',(21.6797116249341,19.9081907944462,10.9371193746034));
#140694=CARTESIAN_POINT('Ctrl Pts',(21.1313727624476,17.9036399101574,11.0282736312959));
#140695=CARTESIAN_POINT('Ctrl Pts',(20.3968579109702,17.2560798667746,11.0770359524279));
#140696=CARTESIAN_POINT('Ctrl Pts',(20.2948050193864,17.1791827951408,11.0834063379994));
#140697=CARTESIAN_POINT('Origin',(18.734,19.211,-1.76670989022852));
#140698=CARTESIAN_POINT('',(20.2935357313021,17.1808649545431,11.9498687317474));
#140699=CARTESIAN_POINT('',(20.2935357313021,17.1808649545431,11.8833305127049));
#140700=CARTESIAN_POINT('',(20.2935357313021,17.1808649545432,-1.76670989022852));
#140701=CARTESIAN_POINT('',(16.1739804710165,19.212301045312,11.4332901033202));
#140702=CARTESIAN_POINT('Ctrl Pts',(16.1740003306697,19.212301164443,11.4332901097715));
#140703=CARTESIAN_POINT('Ctrl Pts',(16.174038011382,19.2864367677247,11.436996088328));
#140704=CARTESIAN_POINT('Ctrl Pts',(16.1772957565522,19.3604881810636,11.4407020668845));
#140705=CARTESIAN_POINT('Ctrl Pts',(16.1837535357011,19.4342553948533,11.444408045441));
#140706=CARTESIAN_POINT('Ctrl Pts',(16.1910453870482,19.5175502156942,11.448592679834));
#140707=CARTESIAN_POINT('Ctrl Pts',(16.2024358975503,19.6006424250678,11.4527773142271));
#140708=CARTESIAN_POINT('Ctrl Pts',(16.217906819526,19.6830965019697,11.4569619486201));
#140709=CARTESIAN_POINT('Ctrl Pts',(16.2333557205591,19.765433215699,11.4611406267041));
#140710=CARTESIAN_POINT('Ctrl Pts',(16.2528734125179,19.8471331528557,11.465319304788));
#140711=CARTESIAN_POINT('Ctrl Pts',(16.2763898192683,19.927765093712,11.4694979828719));
#140712=CARTESIAN_POINT('Ctrl Pts',(16.3003277407088,20.0098423041589,11.4737515607574));
#140713=CARTESIAN_POINT('Ctrl Pts',(16.3284090988417,20.0908123737401,11.4780051386428));
#140714=CARTESIAN_POINT('Ctrl Pts',(16.3605053261111,20.1702304379142,11.4822587165282));
#140715=CARTESIAN_POINT('Ctrl Pts',(16.3919793053844,20.2481088279428,11.4864298305062));
#140716=CARTESIAN_POINT('Ctrl Pts',(16.4273136905277,20.3244944066986,11.4906009444841));
#140717=CARTESIAN_POINT('Ctrl Pts',(16.4663372697809,20.3989838980285,11.4947720584621));
#140718=CARTESIAN_POINT('Ctrl Pts',(16.5053477542952,20.4734483936902,11.4989417727825));
#140719=CARTESIAN_POINT('Ctrl Pts',(16.5480447610381,20.5460176583688,11.5031114871028));
#140720=CARTESIAN_POINT('Ctrl Pts',(16.5942102750742,20.6163113296,11.5072812014232));
#140721=CARTESIAN_POINT('Ctrl Pts',(16.6403741463432,20.6866024994807,11.5114507673673));
#140722=CARTESIAN_POINT('Ctrl Pts',(16.6900060262588,20.7546178528607,11.5156203333113));
#140723=CARTESIAN_POINT('Ctrl Pts',(16.7428443053794,20.8200055934583,11.5197898992554));
#140724=CARTESIAN_POINT('Ctrl Pts',(16.7975403132109,20.8876922863507,11.5241060619943));
#140725=CARTESIAN_POINT('Ctrl Pts',(16.8556720579015,20.9525627446115,11.5284222247332));
#140726=CARTESIAN_POINT('Ctrl Pts',(16.916904887788,21.0142651921377,11.5327383874721));
#140727=CARTESIAN_POINT('Ctrl Pts',(16.9761430646815,21.0739576889257,11.5369139516638));
#140728=CARTESIAN_POINT('Ctrl Pts',(17.0382830139766,21.1306851185866,11.5410895158555));
#140729=CARTESIAN_POINT('Ctrl Pts',(17.1029865459478,21.1841687998498,11.5452650800472));
#140730=CARTESIAN_POINT('Ctrl Pts',(17.1709580995008,21.2403538147083,11.5496515420597));
#140731=CARTESIAN_POINT('Ctrl Pts',(17.2417585461138,21.2929584378007,11.5540380040722));
#140732=CARTESIAN_POINT('Ctrl Pts',(17.3149615008576,21.3417110873959,11.5584244660848));
#140733=CARTESIAN_POINT('Ctrl Pts',(17.3881644556013,21.390463736991,11.5628109280973));
#140734=CARTESIAN_POINT('Ctrl Pts',(17.4637693807619,21.4353641822178,11.5671973901099));
#140735=CARTESIAN_POINT('Ctrl Pts',(17.5413224142637,21.4761976020829,11.5715838521224));
#140736=CARTESIAN_POINT('Ctrl Pts',(17.6153071177329,21.5151522157705,11.5757684865154));
#140737=CARTESIAN_POINT('Ctrl Pts',(17.6913399834856,21.5505508359911,11.5799531209085));
#140738=CARTESIAN_POINT('Ctrl Pts',(17.7690449301557,21.5821730668978,11.5841377553015));
#140739=CARTESIAN_POINT('Ctrl Pts',(17.8466392734521,21.6137502874729,11.5883164333855));
#140740=CARTESIAN_POINT('Ctrl Pts',(17.9259005477805,21.6415616236984,11.5924951114694));
#140741=CARTESIAN_POINT('Ctrl Pts',(18.0064282347094,21.6654325874532,11.5966737895534));
#140742=CARTESIAN_POINT('Ctrl Pts',(18.0883993225523,21.6897314210775,11.6009273674388));
#140743=CARTESIAN_POINT('Ctrl Pts',(18.1716822438311,21.7099470058045,11.6051809453242));
#140744=CARTESIAN_POINT('Ctrl Pts',(18.2558333466883,21.7259466498637,11.6094345232097));
#140745=CARTESIAN_POINT('Ctrl Pts',(18.3383530162092,21.7416361096021,11.6136056371876));
#140746=CARTESIAN_POINT('Ctrl Pts',(18.4217070321714,21.7532715484977,11.6177767511656));
#140747=CARTESIAN_POINT('Ctrl Pts',(18.5054636294713,21.7607786428131,11.6219478651435));
#140748=CARTESIAN_POINT('Ctrl Pts',(18.589192121436,21.7682832180504,11.6261175794639));
#140749=CARTESIAN_POINT('Ctrl Pts',(18.6733224686327,21.7716621589129,11.6302872937843));
#140750=CARTESIAN_POINT('Ctrl Pts',(18.7574168390729,21.7708928984721,11.6344570081046));
#140751=CARTESIAN_POINT('Ctrl Pts',(18.8415082170746,21.7701236654049,11.6386265740487));
#140752=CARTESIAN_POINT('Ctrl Pts',(18.9255631608594,21.7652065295826,11.6427961399927));
#140753=CARTESIAN_POINT('Ctrl Pts',(19.0091442611984,21.75617104249,11.6469657059368));
#140754=CARTESIAN_POINT('Ctrl Pts',(19.095663969917,21.7468178788177,11.6512818686757));
#140755=CARTESIAN_POINT('Ctrl Pts',(19.1816753701872,21.7330514297719,11.6555980314146));
#140756=CARTESIAN_POINT('Ctrl Pts',(19.2667015333779,21.7149626747092,11.6599141941535));
#140757=CARTESIAN_POINT('Ctrl Pts',(19.3489579782457,21.6974631589401,11.6640897583452));
#140758=CARTESIAN_POINT('Ctrl Pts',(19.4302919452563,21.6759187771978,11.6682653225369));
#140759=CARTESIAN_POINT('Ctrl Pts',(19.510286051879,21.6504630486355,11.6724408867286));
#140760=CARTESIAN_POINT('Ctrl Pts',(19.5943204706595,21.6237216117387,11.6768273487411));
#140761=CARTESIAN_POINT('Ctrl Pts',(19.6768755727334,21.5926635253051,11.6812138107537));
#140762=CARTESIAN_POINT('Ctrl Pts',(19.757492206768,21.557500309543,11.6856002727662));
#140763=CARTESIAN_POINT('Ctrl Pts',(19.8381088408025,21.5223370937809,11.6899867347787));
#140764=CARTESIAN_POINT('Ctrl Pts',(19.9167865216175,21.4830690758565,11.6943731967913));
#140765=CARTESIAN_POINT('Ctrl Pts',(19.9930989518204,21.4399616034209,11.6987596588038));
#140766=CARTESIAN_POINT('Ctrl Pts',(20.0659001339874,21.3988375696928,11.7029442931969));
#140767=CARTESIAN_POINT('Ctrl Pts',(20.1368199197944,21.3540665637942,11.7071289275899));
#140768=CARTESIAN_POINT('Ctrl Pts',(20.205469425502,21.3058455145458,11.711313561983));
#140769=CARTESIAN_POINT('Ctrl Pts',(20.2740212171354,21.2576931019925,11.7154922400669));
#140770=CARTESIAN_POINT('Ctrl Pts',(20.3403087741465,21.2061006624661,11.7196709181509));
#140771=CARTESIAN_POINT('Ctrl Pts',(20.4039685866086,21.1513105214735,11.7238495962348));
#140772=CARTESIAN_POINT('Ctrl Pts',(20.4687694554575,21.0955383065805,11.7281031741202));
#140773=CARTESIAN_POINT('Ctrl Pts',(20.5308470287299,21.036452862187,11.7323567520057));
#140774=CARTESIAN_POINT('Ctrl Pts',(20.5898495933098,20.9743554057569,11.7366103298911));
#140775=CARTESIAN_POINT('Ctrl Pts',(20.6477082780412,20.9134618296929,11.740781443869));
#140776=CARTESIAN_POINT('Ctrl Pts',(20.7026097887107,20.8496723357183,11.744952557847));
#140777=CARTESIAN_POINT('Ctrl Pts',(20.7542579245554,20.7833097399276,11.7491236718249));
#140778=CARTESIAN_POINT('Ctrl Pts',(20.8058887293692,20.7169694127468,11.7532933861453));
#140779=CARTESIAN_POINT('Ctrl Pts',(20.8542680451849,20.6480580612728,11.7574631004657));
#140780=CARTESIAN_POINT('Ctrl Pts',(20.8991399066357,20.5769316178687,11.761632814786));
#140781=CARTESIAN_POINT('Ctrl Pts',(20.9440101713531,20.5058077054488,11.7658023807301));
#140782=CARTESIAN_POINT('Ctrl Pts',(20.9853729851228,20.4324692473493,11.7699719466741));
#140783=CARTESIAN_POINT('Ctrl Pts',(21.0230164347473,20.3573000311684,11.7741415126182));
#140784=CARTESIAN_POINT('Ctrl Pts',(21.0619833816224,20.2794879580778,11.7784576753571));
#140785=CARTESIAN_POINT('Ctrl Pts',(21.0969643161937,20.1997144642828,11.782773838096));
#140786=CARTESIAN_POINT('Ctrl Pts',(21.1277775852798,20.1184298166866,11.7870900008349));
#140787=CARTESIAN_POINT('Ctrl Pts',(21.1575871153665,20.0397930079361,11.7912655650266));
#140788=CARTESIAN_POINT('Ctrl Pts',(21.1834962335157,19.9597424478441,11.7954411292183));
#140789=CARTESIAN_POINT('Ctrl Pts',(21.2053912869579,19.8787013604515,11.7996166934099));
#140790=CARTESIAN_POINT('Ctrl Pts',(21.2283922074989,19.7935670803916,11.8040031554225));
#140791=CARTESIAN_POINT('Ctrl Pts',(21.246962782828,19.7073401510526,11.808389617435));
#140792=CARTESIAN_POINT('Ctrl Pts',(21.2610323380592,19.6205211379197,11.8127760794476));
#140793=CARTESIAN_POINT('Ctrl Pts',(21.2751018932903,19.5337021247869,11.8171625414601));
#140794=CARTESIAN_POINT('Ctrl Pts',(21.2846704408994,19.4462916129091,11.8215490034726));
#140795=CARTESIAN_POINT('Ctrl Pts',(21.2897303495757,19.3587916785811,11.8259354654852));
#140796=CARTESIAN_POINT('Ctrl Pts',(21.2945575272397,19.2753163125985,11.830120171733));
#140797=CARTESIAN_POINT('Ctrl Pts',(21.2952996738552,19.1914488528641,11.8343048779808));
#140798=CARTESIAN_POINT('Ctrl Pts',(21.2919118781325,19.1076229052994,11.8384895842286));
#140799=CARTESIAN_POINT('Ctrl Pts',(21.2885289204165,19.0239166669875,11.8426683144263));
#140800=CARTESIAN_POINT('Ctrl Pts',(21.2810277540026,18.9402522788518,11.8468470446241));
#140801=CARTESIAN_POINT('Ctrl Pts',(21.2694153767469,18.8570665777929,11.8510257748218));
#140802=CARTESIAN_POINT('Ctrl Pts',(21.2578166868035,18.7739789263091,11.8551995796212));
#140803=CARTESIAN_POINT('Ctrl Pts',(21.2421164820731,18.6913692935119,11.8593733844205));
#140804=CARTESIAN_POINT('Ctrl Pts',(21.222373696678,18.6096711833937,11.8635471892198));
#140805=CARTESIAN_POINT('Ctrl Pts',(21.2026437041566,18.5280260117835,11.8677182894891));
#140806=CARTESIAN_POINT('Ctrl Pts',(21.1788764395505,18.4472916360316,11.8718893897583));
#140807=CARTESIAN_POINT('Ctrl Pts',(21.1511820426494,18.3678920752992,11.8760604900275));
#140808=CARTESIAN_POINT('Ctrl Pts',(21.1234972832826,18.2885201452817,11.8802301387713));
#140809=CARTESIAN_POINT('Ctrl Pts',(21.091888257503,18.2104825415903,11.884399787515));
#140810=CARTESIAN_POINT('Ctrl Pts',(21.056514760822,18.1341874881094,11.8885694362588));
#140811=CARTESIAN_POINT('Ctrl Pts',(21.0211429628484,18.0578960984727,11.8927388847675));
#140812=CARTESIAN_POINT('Ctrl Pts',(20.9820072479425,17.9833475094823,11.8969083332763));
#140813=CARTESIAN_POINT('Ctrl Pts',(20.9393147224051,17.9109280884722,11.901077781785));
#140814=CARTESIAN_POINT('Ctrl Pts',(20.8965841485715,17.8384441260572,11.9052509461763));
#140815=CARTESIAN_POINT('Ctrl Pts',(20.8502906654426,17.7680935196513,11.9094241105676));
#140816=CARTESIAN_POINT('Ctrl Pts',(20.8006860848068,17.7002357474225,11.9135972749589));
#140817=CARTESIAN_POINT('Ctrl Pts',(20.7510600241068,17.6323485910264,11.9177722464381));
#140818=CARTESIAN_POINT('Ctrl Pts',(20.6981202983251,17.5669567780695,11.9219472179173));
#140819=CARTESIAN_POINT('Ctrl Pts',(20.6421591183025,17.50438675171,11.9261221893965));
#140820=CARTESIAN_POINT('Ctrl Pts',(20.5861048294898,17.4417126206934,11.9303041072365));
#140821=CARTESIAN_POINT('Ctrl Pts',(20.5270193651102,17.3818699857993,11.9344860250764));
#140822=CARTESIAN_POINT('Ctrl Pts',(20.4652317777209,17.3251483271982,11.9386679429164));
#140823=CARTESIAN_POINT('Ctrl Pts',(20.4100681147629,17.2745075012702,11.9424015391934));
#140824=CARTESIAN_POINT('Ctrl Pts',(20.3527513018397,17.2263539471644,11.9461351354704));
#140825=CARTESIAN_POINT('Ctrl Pts',(20.2935357313021,17.1808649545431,11.9498687317474));
#140826=CARTESIAN_POINT('Ctrl Pts',(20.2922817525494,17.1824654639375,11.1497835189211));
#140827=CARTESIAN_POINT('Ctrl Pts',(20.0792747203257,17.0159205528436,11.1632078233067));
#140828=CARTESIAN_POINT('Ctrl Pts',(19.0902279311992,16.4618740896682,11.2190240632529));
#140829=CARTESIAN_POINT('Ctrl Pts',(16.9631832240595,16.8048336241861,11.3135258905591));
#140830=CARTESIAN_POINT('Ctrl Pts',(16.1754043777096,18.4373668536376,11.3946034134798));
#140831=CARTESIAN_POINT('Ctrl Pts',(16.1705865747788,19.2122806865248,11.4332890008399));
#140832=CARTESIAN_POINT('',(16.1740004874608,19.2094201902091,11.3667098902285));
#140833=CARTESIAN_POINT('Ctrl Pts',(20.2948050193864,17.1791827951408,11.0834063379994));
#140834=CARTESIAN_POINT('Ctrl Pts',(19.7177436634564,16.7443658317468,11.1194278879883));
#140835=CARTESIAN_POINT('Ctrl Pts',(18.0373628378674,16.3338524237142,11.1978413735377));
#140836=CARTESIAN_POINT('Ctrl Pts',(16.3822353164858,17.7107520392007,11.2922755723079));
#140837=CARTESIAN_POINT('Ctrl Pts',(16.1753926962513,18.8863578053553,11.3506882210889));
#140838=CARTESIAN_POINT('Ctrl Pts',(16.1772046638934,19.209402892261,11.3667089343096));
#140839=CARTESIAN_POINT('Ctrl Pts',(16.1740004874608,19.2094201902091,11.3667098902285));
#140840=CARTESIAN_POINT('Ctrl Pts',(16.1739481146197,19.2942876523606,11.3709134538372));
#140841=CARTESIAN_POINT('Ctrl Pts',(16.1781202862138,19.3791700299234,11.3751170174459));
#140842=CARTESIAN_POINT('Ctrl Pts',(16.1864949217896,19.463622003183,11.3793205810546));
#140843=CARTESIAN_POINT('Ctrl Pts',(16.1948707822013,19.5480863280015,11.3835247594573));
#140844=CARTESIAN_POINT('Ctrl Pts',(16.2074502833288,19.6321196761629,11.3877289378599));
#140845=CARTESIAN_POINT('Ctrl Pts',(16.2241595327125,19.7152824890538,11.3919331162626));
#140846=CARTESIAN_POINT('Ctrl Pts',(16.2408759290273,19.7984808725962,11.3961390928892));
#140847=CARTESIAN_POINT('Ctrl Pts',(16.2617254950327,19.8808075406061,11.4003450695159));
#140848=CARTESIAN_POINT('Ctrl Pts',(16.2865836343726,19.9618349574034,11.4045510461425));
#140849=CARTESIAN_POINT('Ctrl Pts',(16.3114761780105,20.0429745182097,11.408762843948));
#140850=CARTESIAN_POINT('Ctrl Pts',(16.3403882340966,20.1228108093805,11.4129746417534));
#140851=CARTESIAN_POINT('Ctrl Pts',(16.3731460171587,20.200933569338,11.4171864395589));
#140852=CARTESIAN_POINT('Ctrl Pts',(16.4059305542806,20.27912013401,11.4214016772397));
#140853=CARTESIAN_POINT('Ctrl Pts',(16.4425668768386,20.3555899771936,11.4256169149205));
#140854=CARTESIAN_POINT('Ctrl Pts',(16.4828349986459,20.4299569872143,11.4298321526013));
#140855=CARTESIAN_POINT('Ctrl Pts',(16.5231739006092,20.5044547137505,11.4340547994973));
#140856=CARTESIAN_POINT('Ctrl Pts',(16.5671571084148,20.5768418481604,11.4382774463933));
#140857=CARTESIAN_POINT('Ctrl Pts',(16.6145212917448,20.646761124022,11.4425000932893));
#140858=CARTESIAN_POINT('Ctrl Pts',(16.6269438222718,20.6650993339888,11.4436075959693));
#140859=CARTESIAN_POINT('Ctrl Pts',(16.6395987151329,20.6832679625289,11.4447150986492));
#140860=CARTESIAN_POINT('Ctrl Pts',(16.6524807786036,20.7012609606902,11.4458226013291));
#140861=CARTESIAN_POINT('Ctrl Pts',(16.7011549053849,20.7692464566217,11.4500072357222));
#140862=CARTESIAN_POINT('Ctrl Pts',(16.7532538754925,20.8349713096213,11.4541918701152));
#140863=CARTESIAN_POINT('Ctrl Pts',(16.8085402991528,20.8980699275411,11.4583765045082));
#140864=CARTESIAN_POINT('Ctrl Pts',(16.8637480294321,20.9610787323883,11.4625551825922));
#140865=CARTESIAN_POINT('Ctrl Pts',(16.9221339008884,21.0214683841931,11.4667338606761));
#140866=CARTESIAN_POINT('Ctrl Pts',(16.9834181011141,21.0789033741853,11.4709125387601));
#140867=CARTESIAN_POINT('Ctrl Pts',(17.0458007765846,21.1373678450953,11.4751661166455));
#140868=CARTESIAN_POINT('Ctrl Pts',(17.1111864272472,21.1927702956729,11.479419694531));
#140869=CARTESIAN_POINT('Ctrl Pts',(17.1792379481545,21.2447932446887,11.4836732724164));
#140870=CARTESIAN_POINT('Ctrl Pts',(17.2459701575374,21.2958076273233,11.4878443863943));
#140871=CARTESIAN_POINT('Ctrl Pts',(17.3152654110889,21.3435720832561,11.4920155003723));
#140872=CARTESIAN_POINT('Ctrl Pts',(17.3867710660548,21.3878266351598,11.4961866143502));
#140873=CARTESIAN_POINT('Ctrl Pts',(17.4582527266078,21.4320663370211,11.5003563286706));
#140874=CARTESIAN_POINT('Ctrl Pts',(17.5319429246535,21.4727982320514,11.504526042991));
#140875=CARTESIAN_POINT('Ctrl Pts',(17.607460394208,21.5098058892786,11.5086957573113));
#140876=CARTESIAN_POINT('Ctrl Pts',(17.682975176527,21.5468122296146,11.5128653232554));
#140877=CARTESIAN_POINT('Ctrl Pts',(17.7603166876027,21.5800943939658,11.5170348891994));
#140878=CARTESIAN_POINT('Ctrl Pts',(17.8390806772781,21.6094827299397,11.5212044551435));
#140879=CARTESIAN_POINT('Ctrl Pts',(17.9206139116645,21.639904323552,11.5255206178824));
#140880=CARTESIAN_POINT('Ctrl Pts',(18.0036710203269,21.6661529958307,11.5298367806213));
#140881=CARTESIAN_POINT('Ctrl Pts',(18.0877848913435,21.6880962906888,11.5341529433602));
#140882=CARTESIAN_POINT('Ctrl Pts',(18.169158761859,21.7093247850249,11.5383285075519));
#140883=CARTESIAN_POINT('Ctrl Pts',(18.2515211332004,21.7265240396988,11.5425040717436));
#140884=CARTESIAN_POINT('Ctrl Pts',(18.3344390537287,21.7396263168398,11.5466796359353));
#140885=CARTESIAN_POINT('Ctrl Pts',(18.4215449613043,21.7533903588514,11.5510660979478));
#140886=CARTESIAN_POINT('Ctrl Pts',(18.5092634338793,21.7626326086006,11.5554525599604));
#140887=CARTESIAN_POINT('Ctrl Pts',(18.5970892183626,21.7673363311332,11.5598390219729));
#140888=CARTESIAN_POINT('Ctrl Pts',(18.684915002846,21.7720400536657,11.5642254839854));
#140889=CARTESIAN_POINT('Ctrl Pts',(18.7728475188787,21.7722053239559,11.568611945998));
#140890=CARTESIAN_POINT('Ctrl Pts',(18.8603867536229,21.7678782506229,11.5729984080105));
#140891=CARTESIAN_POINT('Ctrl Pts',(18.9438981784122,21.7637502723483,11.5771830424036));
#140892=CARTESIAN_POINT('Ctrl Pts',(19.0273625629855,21.7555188996868,11.5813676767966));
#140893=CARTESIAN_POINT('Ctrl Pts',(19.1103440076205,21.7431858517747,11.5855523111897));
#140894=CARTESIAN_POINT('Ctrl Pts',(19.1932073384403,21.7308703584299,11.5897309892736));
#140895=CARTESIAN_POINT('Ctrl Pts',(19.2755886435823,21.7144648534412,11.5939096673576));
#140896=CARTESIAN_POINT('Ctrl Pts',(19.357054356117,21.6940230102284,11.5980883454415));
#140897=CARTESIAN_POINT('Ctrl Pts',(19.4399802830004,21.6732147616673,11.602341923327));
#140898=CARTESIAN_POINT('Ctrl Pts',(19.521956988875,21.6482240726706,11.6065955012124));
#140899=CARTESIAN_POINT('Ctrl Pts',(19.602535053755,21.6191625485832,11.6108490790978));
#140900=CARTESIAN_POINT('Ctrl Pts',(19.6815509556122,21.5906644388491,11.6150201930758));
#140901=CARTESIAN_POINT('Ctrl Pts',(19.7592215106217,21.5582520908958,11.6191913070537));
#140902=CARTESIAN_POINT('Ctrl Pts',(19.8351372401591,21.5220813006761,11.6233624210317));
#140903=CARTESIAN_POINT('Ctrl Pts',(19.9110274954402,21.4859226479144,11.627532135352));
#140904=CARTESIAN_POINT('Ctrl Pts',(19.9851636797555,21.446008255323,11.6317018496724));
#140905=CARTESIAN_POINT('Ctrl Pts',(20.0571574368626,21.4025415572777,11.6358715639928));
#140906=CARTESIAN_POINT('Ctrl Pts',(20.129148632123,21.359076405964,11.6400411299368));
#140907=CARTESIAN_POINT('Ctrl Pts',(20.1989971583731,21.3120594390258,11.6442106958809));
#140908=CARTESIAN_POINT('Ctrl Pts',(20.2663415518563,21.2617387372493,11.6483802618249));
#140909=CARTESIAN_POINT('Ctrl Pts',(20.3360536911359,21.2096488216756,11.6526964245639));
#140910=CARTESIAN_POINT('Ctrl Pts',(20.4030819081961,21.1540188458219,11.6570125873028));
#140911=CARTESIAN_POINT('Ctrl Pts',(20.4670619896057,21.0951698809248,11.6613287500417));
#140912=CARTESIAN_POINT('Ctrl Pts',(20.5289579265928,21.0382379148694,11.6655043142334));
#140913=CARTESIAN_POINT('Ctrl Pts',(20.5880009674137,20.9782938250444,11.6696798784251));
#140914=CARTESIAN_POINT('Ctrl Pts',(20.6438998067282,20.9156649900375,11.6738554426167));
#140915=CARTESIAN_POINT('Ctrl Pts',(20.7026219635295,20.8498729214604,11.6782419046293));
#140916=CARTESIAN_POINT('Ctrl Pts',(20.7578735784433,20.7811182222702,11.6826283666418));
#140917=CARTESIAN_POINT('Ctrl Pts',(20.809367096106,20.7098166720452,11.6870148286544));
#140918=CARTESIAN_POINT('Ctrl Pts',(20.8608606137687,20.6385151218202,11.6914012906669));
#140919=CARTESIAN_POINT('Ctrl Pts',(20.9085957830846,20.5646672491326,11.6957877526794));
#140920=CARTESIAN_POINT('Ctrl Pts',(20.9523407266398,20.4887184433713,11.700174214692));
#140921=CARTESIAN_POINT('Ctrl Pts',(20.9940729004966,20.4162641547461,11.704358849085));
#140922=CARTESIAN_POINT('Ctrl Pts',(21.0323293070735,20.3416283299438,11.7085434834781));
#140923=CARTESIAN_POINT('Ctrl Pts',(21.06687544764,20.265178422184,11.7127281178711));
#140924=CARTESIAN_POINT('Ctrl Pts',(21.1013724160514,20.1888373314054,11.7169067959551));
#140925=CARTESIAN_POINT('Ctrl Pts',(21.1321694205716,20.1106877022101,11.721085474039));
#140926=CARTESIAN_POINT('Ctrl Pts',(21.159076910497,20.0311231481762,11.7252641521229));
#140927=CARTESIAN_POINT('Ctrl Pts',(21.1864666978412,19.9501324566933,11.7295177300084));
#140928=CARTESIAN_POINT('Ctrl Pts',(21.209825919336,19.8676760341797,11.7337713078938));
#140929=CARTESIAN_POINT('Ctrl Pts',(21.2290051549001,19.7841921815777,11.7380248857793));
#140930=CARTESIAN_POINT('Ctrl Pts',(21.2478125635576,19.7023268263636,11.7421959997572));
#140931=CARTESIAN_POINT('Ctrl Pts',(21.2626005065823,19.6194739920341,11.7463671137352));
#140932=CARTESIAN_POINT('Ctrl Pts',(21.273278340702,19.5360623147051,11.7505382277131));
#140933=CARTESIAN_POINT('Ctrl Pts',(21.2839525917715,19.4526786269701,11.7547079420335));
#140934=CARTESIAN_POINT('Ctrl Pts',(21.2905194146576,19.3687369245929,11.7588776563539));
#140935=CARTESIAN_POINT('Ctrl Pts',(21.2929396556081,19.284673868884,11.7630473706742));
#140936=CARTESIAN_POINT('Ctrl Pts',(21.295359810436,19.2006138044994,11.7672169366183));
#140937=CARTESIAN_POINT('Ctrl Pts',(21.2936336643145,19.1164328552357,11.7713865025623));
#140938=CARTESIAN_POINT('Ctrl Pts',(21.2877741604491,19.0325692363337,11.7755560685064));
#140939=CARTESIAN_POINT('Ctrl Pts',(21.2817086436563,18.945757076048,11.7798722312453));
#140940=CARTESIAN_POINT('Ctrl Pts',(21.2712137402019,18.859285502122,11.7841883939842));
#140941=CARTESIAN_POINT('Ctrl Pts',(21.2563622783628,18.7736345501841,11.7885045567231));
#140942=CARTESIAN_POINT('Ctrl Pts',(21.241994601331,18.6907736689967,11.7926801209148));
#140943=CARTESIAN_POINT('Ctrl Pts',(21.2235499863026,18.6086812165374,11.7968556851065));
#140944=CARTESIAN_POINT('Ctrl Pts',(21.2011460288054,18.5277793383177,11.8010312492982));
#140945=CARTESIAN_POINT('Ctrl Pts',(21.1776105006754,18.442791298555,11.8054177113107));
#140946=CARTESIAN_POINT('Ctrl Pts',(21.1497053305466,18.3591178195345,11.8098041733232));
#140947=CARTESIAN_POINT('Ctrl Pts',(21.1176244749813,18.27722574341,11.8141906353358));
#140948=CARTESIAN_POINT('Ctrl Pts',(21.085543619416,18.1953336672856,11.8185770973483));
#140949=CARTESIAN_POINT('Ctrl Pts',(21.0492873869465,18.115223491295,11.8229635593609));
#140950=CARTESIAN_POINT('Ctrl Pts',(21.0091047687183,18.0373312684769,11.8273500213734));
#140951=CARTESIAN_POINT('Ctrl Pts',(20.970767809012,17.9630167728245,11.8315350054497));
#140952=CARTESIAN_POINT('Ctrl Pts',(20.9287145340175,17.8904443146227,11.835719989526));
#140953=CARTESIAN_POINT('Ctrl Pts',(20.8831270316874,17.8200100641376,11.8399049736022));
#140954=CARTESIAN_POINT('Ctrl Pts',(20.8376158265713,17.749693695458,11.8440829535083));
#140955=CARTESIAN_POINT('Ctrl Pts',(20.7885824023206,17.6815088023905,11.8482609334144));
#140956=CARTESIAN_POINT('Ctrl Pts',(20.7362550110473,17.6158276360418,11.8524389133204));
#140957=CARTESIAN_POINT('Ctrl Pts',(20.6839782703688,17.5502100461501,11.8566128491272));
#140958=CARTESIAN_POINT('Ctrl Pts',(20.6284141773837,17.4870917295154,11.8607867849339));
#140959=CARTESIAN_POINT('Ctrl Pts',(20.5698341380306,17.4268158677868,11.8649607207407));
#140960=CARTESIAN_POINT('Ctrl Pts',(20.5112960173992,17.366583138277,11.8691316697612));
#140961=CARTESIAN_POINT('Ctrl Pts',(20.4497465580658,17.3091891512985,11.8733026187818));
#140962=CARTESIAN_POINT('Ctrl Pts',(20.3854963550796,17.2549427950188,11.8774735678023));
#140963=CARTESIAN_POINT('Ctrl Pts',(20.3554224720524,17.2295514577532,11.8794258827698));
#140964=CARTESIAN_POINT('Ctrl Pts',(20.3247574130354,17.2048492349798,11.8813781977374));
#140965=CARTESIAN_POINT('Ctrl Pts',(20.2935357313021,17.1808649545431,11.8833305127049));
#140966=CARTESIAN_POINT('Origin',(18.734,19.211,-1.76670989022852));
#140967=CARTESIAN_POINT('',(20.2935357313021,17.1808649545432,12.7499597618547));
#140968=CARTESIAN_POINT('',(20.2929505239234,17.1816081970505,12.6831923935391));
#140969=CARTESIAN_POINT('',(20.2935357313021,17.1808649545432,-1.76670989022852));
#140970=CARTESIAN_POINT('',(16.1740010233873,19.2087109517327,12.2332901098107));
#140971=CARTESIAN_POINT('Ctrl Pts',(16.1740010233873,19.2087109517327,12.2332901098107));
#140972=CARTESIAN_POINT('Ctrl Pts',(16.1739252094451,19.293498859929,12.2375129674107));
#140973=CARTESIAN_POINT('Ctrl Pts',(16.1780663695147,19.3784221563148,12.2417358250107));
#140974=CARTESIAN_POINT('Ctrl Pts',(16.1864353355331,19.4630203967139,12.2459586826108));
#140975=CARTESIAN_POINT('Ctrl Pts',(16.1945865434513,19.5454174151127,12.2500716626647));
#140976=CARTESIAN_POINT('Ctrl Pts',(16.2067481850334,19.6275055813485,12.2541846427187));
#140977=CARTESIAN_POINT('Ctrl Pts',(16.2228775801224,19.7088596111236,12.2582976227727));
#140978=CARTESIAN_POINT('Ctrl Pts',(16.2389992540558,19.7901746966527,12.2624086339395));
#140979=CARTESIAN_POINT('Ctrl Pts',(16.25908482094,19.8707558783837,12.2665196451063));
#140980=CARTESIAN_POINT('Ctrl Pts',(16.2830401055299,19.9501857653521,12.2706306562731));
#140981=CARTESIAN_POINT('Ctrl Pts',(16.3069915898918,20.0296030516901,12.2747410152757));
#140982=CARTESIAN_POINT('Ctrl Pts',(16.3348114354692,20.1078689519365,12.2788513742782));
#140983=CARTESIAN_POINT('Ctrl Pts',(16.366355393672,20.1845805144548,12.2829617332808));
#140984=CARTESIAN_POINT('Ctrl Pts',(16.3994039228381,20.264951034063,12.2872681465249));
#140985=CARTESIAN_POINT('Ctrl Pts',(16.4365404963283,20.3436147061446,12.2915745597691));
#140986=CARTESIAN_POINT('Ctrl Pts',(16.4775431085385,20.4201328698599,12.2958809730133));
#140987=CARTESIAN_POINT('Ctrl Pts',(16.5167281737211,20.4932591677035,12.2999964933322));
#140988=CARTESIAN_POINT('Ctrl Pts',(16.5594435017451,20.5644257408165,12.304112013651));
#140989=CARTESIAN_POINT('Ctrl Pts',(16.6054498638678,20.6332778624347,12.3082275339699));
#140990=CARTESIAN_POINT('Ctrl Pts',(16.6514869443887,20.7021759565399,12.3123458022172));
#140991=CARTESIAN_POINT('Ctrl Pts',(16.7008191449123,20.768756147345,12.3164640704645));
#140992=CARTESIAN_POINT('Ctrl Pts',(16.7531665958489,20.8326963417974,12.3205823387118));
#140993=CARTESIAN_POINT('Ctrl Pts',(16.8055945346489,20.8967348487664,12.3247069390843));
#140994=CARTESIAN_POINT('Ctrl Pts',(16.8610466479906,20.9581249187389,12.3288315394568));
#140995=CARTESIAN_POINT('Ctrl Pts',(16.9192065009781,21.0165815007659,12.3329561398293));
#140996=CARTESIAN_POINT('Ctrl Pts',(16.9271149034352,21.0245302515482,12.3335169906232));
#140997=CARTESIAN_POINT('Ctrl Pts',(16.93507332294,21.0324248251516,12.3340778414171));
#140998=CARTESIAN_POINT('Ctrl Pts',(16.9430809195058,21.040264564551,12.334638692211));
#140999=CARTESIAN_POINT('Ctrl Pts',(17.0028274053093,21.0987586301397,12.338823326604));
#141000=CARTESIAN_POINT('Ctrl Pts',(17.0655538444182,21.1544313597729,12.3430079609971));
#141001=CARTESIAN_POINT('Ctrl Pts',(17.1309629349571,21.2069639696394,12.3471925953901));
#141002=CARTESIAN_POINT('Ctrl Pts',(17.1962789237517,21.259421805838,12.3513712734741));
#141003=CARTESIAN_POINT('Ctrl Pts',(17.2642696237805,21.3087481146435,12.355549951558));
#141004=CARTESIAN_POINT('Ctrl Pts',(17.3346011829193,21.3546611091199,12.3597286296419));
#141005=CARTESIAN_POINT('Ctrl Pts',(17.4061933847094,21.4013970610253,12.3639822075274));
#141006=CARTESIAN_POINT('Ctrl Pts',(17.4802108463241,21.4445957903897,12.3682357854128));
#141007=CARTESIAN_POINT('Ctrl Pts',(17.5562664269212,21.484003218397,12.3724893632982));
#141008=CARTESIAN_POINT('Ctrl Pts',(17.6308475216781,21.522646656515,12.3766604772762));
#141009=CARTESIAN_POINT('Ctrl Pts',(17.7073879875327,21.5576442636058,12.3808315912541));
#141010=CARTESIAN_POINT('Ctrl Pts',(17.7854953736982,21.5888012898231,12.3850027052321));
#141011=CARTESIAN_POINT('Ctrl Pts',(17.863576550176,21.6199478609992,12.3891724195525));
#141012=CARTESIAN_POINT('Ctrl Pts',(17.943223175791,21.6472562404631,12.3933421338728));
#141013=CARTESIAN_POINT('Ctrl Pts',(18.0240221782529,21.6705795357392,12.3975118481932));
#141014=CARTESIAN_POINT('Ctrl Pts',(18.1048183055395,21.6939020010724,12.4016814141373));
#141015=CARTESIAN_POINT('Ctrl Pts',(18.1867662859179,21.713239537401,12.4058509800813));
#141016=CARTESIAN_POINT('Ctrl Pts',(18.2694385404877,21.7284953128727,12.4100205460253));
#141017=CARTESIAN_POINT('Ctrl Pts',(18.3550174495409,21.7442874625899,12.4143367087643));
#141018=CARTESIAN_POINT('Ctrl Pts',(18.4413719926984,21.7557053858609,12.4186528715032));
#141019=CARTESIAN_POINT('Ctrl Pts',(18.5280191484745,21.762699803818,12.4229690342421));
#141020=CARTESIAN_POINT('Ctrl Pts',(18.6118437822648,21.7694663793459,12.4271445984338));
#141021=CARTESIAN_POINT('Ctrl Pts',(18.6959417854331,21.7720932477196,12.4313201626255));
#141022=CARTESIAN_POINT('Ctrl Pts',(18.7798750222012,21.7705889283903,12.4354957268171));
#141023=CARTESIAN_POINT('Ctrl Pts',(18.8680475272262,21.7690086294678,12.4398821888297));
#141024=CARTESIAN_POINT('Ctrl Pts',(18.9560376012523,21.7628688832022,12.4442686508422));
#141025=CARTESIAN_POINT('Ctrl Pts',(19.0433447687653,21.7522409988109,12.4486551128548));
#141026=CARTESIAN_POINT('Ctrl Pts',(19.1306519362784,21.7416131144196,12.4530415748673));
#141027=CARTESIAN_POINT('Ctrl Pts',(19.2172756387742,21.7264972665759,12.4574280368799));
#141028=CARTESIAN_POINT('Ctrl Pts',(19.3027314805894,21.7070257416514,12.4618144988924));
#141029=CARTESIAN_POINT('Ctrl Pts',(19.3842553724468,21.6884501304525,12.4659991332855));
#141030=CARTESIAN_POINT('Ctrl Pts',(19.4650199594565,21.6658417144697,12.4701837676785));
#141031=CARTESIAN_POINT('Ctrl Pts',(19.5445962710157,21.6392779259004,12.4743684020716));
#141032=CARTESIAN_POINT('Ctrl Pts',(19.6240593155452,21.6127519475962,12.4785470801555));
#141033=CARTESIAN_POINT('Ctrl Pts',(19.7023370115734,21.5822819240423,12.4827257582395));
#141034=CARTESIAN_POINT('Ctrl Pts',(19.7790117130577,21.5479960461182,12.4869044363234));
#141035=CARTESIAN_POINT('Ctrl Pts',(19.8570607534608,21.5130956184733,12.4911580142089));
#141036=CARTESIAN_POINT('Ctrl Pts',(19.9334482966289,21.4742412996488,12.4954115920943));
#141037=CARTESIAN_POINT('Ctrl Pts',(20.0077511504913,21.4316210857826,12.4996651699797));
#141038=CARTESIAN_POINT('Ctrl Pts',(20.0806134985415,21.3898271479286,12.5038362839577));
#141039=CARTESIAN_POINT('Ctrl Pts',(20.1514708500759,21.3444122698723,12.5080073979356));
#141040=CARTESIAN_POINT('Ctrl Pts',(20.219947025126,21.2956010262204,12.5121785119136));
#141041=CARTESIAN_POINT('Ctrl Pts',(20.2884002223341,21.2468061616529,12.516348226234));
#141042=CARTESIAN_POINT('Ctrl Pts',(20.354473455646,21.1946174617219,12.5205179405544));
#141043=CARTESIAN_POINT('Ctrl Pts',(20.4178196235401,21.1393027447425,12.5246876548747));
#141044=CARTESIAN_POINT('Ctrl Pts',(20.4811635373055,21.0839899960981,12.5288572208188));
#141045=CARTESIAN_POINT('Ctrl Pts',(20.5417802326388,21.0255517547982,12.5330267867628));
#141046=CARTESIAN_POINT('Ctrl Pts',(20.5993568489268,20.9642951337872,12.5371963527068));
#141047=CARTESIAN_POINT('Ctrl Pts',(20.6589577880152,20.9008848055495,12.5415125154458));
#141048=CARTESIAN_POINT('Ctrl Pts',(20.7153005309282,20.8344546059654,12.5458286781847));
#141049=CARTESIAN_POINT('Ctrl Pts',(20.7680821915678,20.765384005948,12.5501448409236));
#141050=CARTESIAN_POINT('Ctrl Pts',(20.8191444951636,20.6985633734613,12.5543204051153));
#141051=CARTESIAN_POINT('Ctrl Pts',(20.8668739298251,20.6292721356226,12.558495969307));
#141052=CARTESIAN_POINT('Ctrl Pts',(20.9110405044756,20.557883306702,12.5626715334986));
#141053=CARTESIAN_POINT('Ctrl Pts',(20.9574378278157,20.4828887977435,12.5670579955112));
#141054=CARTESIAN_POINT('Ctrl Pts',(20.9999026310488,20.4055797420146,12.5714444575237));
#141055=CARTESIAN_POINT('Ctrl Pts',(21.0382239760383,20.3264155585478,12.5758309195363));
#141056=CARTESIAN_POINT('Ctrl Pts',(21.0765453210277,20.2472513750809,12.5802173815488));
#141057=CARTESIAN_POINT('Ctrl Pts',(21.1107230523384,20.166232628037,12.5846038435613));
#141058=CARTESIAN_POINT('Ctrl Pts',(21.1406062076889,20.0838382216157,12.5889903055739));
#141059=CARTESIAN_POINT('Ctrl Pts',(21.1691143947643,20.0052349039716,12.5931749399669));
#141060=CARTESIAN_POINT('Ctrl Pts',(21.193820633909,19.9250871608006,12.59735957436));
#141061=CARTESIAN_POINT('Ctrl Pts',(21.2145578396958,19.8437976010731,12.601544208753));
#141062=CARTESIAN_POINT('Ctrl Pts',(21.2352655286368,19.7626237469725,12.605722886837));
#141063=CARTESIAN_POINT('Ctrl Pts',(21.2520152930198,19.6803117464873,12.6099015649209));
#141064=CARTESIAN_POINT('Ctrl Pts',(21.2646888572062,19.5972821611367,12.6140802430048));
#141065=CARTESIAN_POINT('Ctrl Pts',(21.2775895859223,19.5127643301408,12.6183338208903));
#141066=CARTESIAN_POINT('Ctrl Pts',(21.2862663809328,19.4275033890779,12.6225873987757));
#141067=CARTESIAN_POINT('Ctrl Pts',(21.290648251397,19.3419569342516,12.6268409766611));
#141068=CARTESIAN_POINT('Ctrl Pts',(21.2949451707517,19.2580689643825,12.6310120906391));
#141069=CARTESIAN_POINT('Ctrl Pts',(21.2951121858363,19.1739069330306,12.635183204617));
#141070=CARTESIAN_POINT('Ctrl Pts',(21.2911345092732,19.089908705993,12.639354318595));
#141071=CARTESIAN_POINT('Ctrl Pts',(21.2871581674578,19.0059386653716,12.6435240329154));
#141072=CARTESIAN_POINT('Ctrl Pts',(21.2790399178705,18.9221327790365,12.6476937472357));
#141073=CARTESIAN_POINT('Ctrl Pts',(21.2668170738605,18.8389278694117,12.6518634615561));
#141074=CARTESIAN_POINT('Ctrl Pts',(21.2545946647919,18.7557259205747,12.6560330275001));
#141075=CARTESIAN_POINT('Ctrl Pts',(21.2382680194082,18.6731253609526,12.6602025934442));
#141076=CARTESIAN_POINT('Ctrl Pts',(21.2179260255782,18.5915554912218,12.6643721593882));
#141077=CARTESIAN_POINT('Ctrl Pts',(21.1968688323396,18.5071177254984,12.6686883221271));
#141078=CARTESIAN_POINT('Ctrl Pts',(21.1715088054105,18.4237849880543,12.6730044848661));
#141079=CARTESIAN_POINT('Ctrl Pts',(21.1420010732761,18.3420173585733,12.677320647605));
#141080=CARTESIAN_POINT('Ctrl Pts',(21.1134545524124,18.2629133010223,12.6814962117967));
#141081=CARTESIAN_POINT('Ctrl Pts',(21.0810266246881,18.1852743669888,12.6856717759884));
#141082=CARTESIAN_POINT('Ctrl Pts',(21.044906446266,18.1094958481211,12.68984734018));
#141083=CARTESIAN_POINT('Ctrl Pts',(21.0069619234992,18.0298899364116,12.6942338021926));
#141084=CARTESIAN_POINT('Ctrl Pts',(20.9649426346359,17.9523378315094,12.6986202642051));
#141085=CARTESIAN_POINT('Ctrl Pts',(20.9191207015648,17.8772655738143,12.7030067262177));
#141086=CARTESIAN_POINT('Ctrl Pts',(20.8732987684937,17.8021933161192,12.7073931882302));
#141087=CARTESIAN_POINT('Ctrl Pts',(20.8236745814509,17.7296013416972,12.7117796502428));
#141088=CARTESIAN_POINT('Ctrl Pts',(20.7705691100603,17.6598758076968,12.7161661122553));
#141089=CARTESIAN_POINT('Ctrl Pts',(20.7199091712294,17.5933611681518,12.7203505755775));
#141090=CARTESIAN_POINT('Ctrl Pts',(20.6658929673671,17.5292072036879,12.7245350388997));
#141091=CARTESIAN_POINT('Ctrl Pts',(20.6087685574014,17.4677722879156,12.7287195022218));
#141092=CARTESIAN_POINT('Ctrl Pts',(20.5517322346267,17.4064321062362,12.7328975130026));
#141093=CARTESIAN_POINT('Ctrl Pts',(20.491597541221,17.3478029746891,12.7370755237833));
#141094=CARTESIAN_POINT('Ctrl Pts',(20.4286539389136,17.2922118336501,12.7412535345641));
#141095=CARTESIAN_POINT('Ctrl Pts',(20.3849328686936,17.2535978348975,12.7441556103276));
#141096=CARTESIAN_POINT('Ctrl Pts',(20.3398574537499,17.2164489820464,12.7470576860912));
#141097=CARTESIAN_POINT('Ctrl Pts',(20.2935357313021,17.1808649545432,12.7499597618547));
#141098=CARTESIAN_POINT('Ctrl Pts',(20.2935357313021,17.1808649545431,11.9498687317474));
#141099=CARTESIAN_POINT('Ctrl Pts',(20.2763932885852,17.1676962483536,11.9509495785538));
#141100=CARTESIAN_POINT('Ctrl Pts',(20.2590918286248,17.1547506666131,11.9520304253602));
#141101=CARTESIAN_POINT('Ctrl Pts',(20.2416377781113,17.1420320616279,11.9531112721667));
#141102=CARTESIAN_POINT('Ctrl Pts',(20.1740622256442,17.0927903822927,11.9572959065597));
#141103=CARTESIAN_POINT('Ctrl Pts',(20.1039459219086,17.0467712239067,11.9614805409528));
#141104=CARTESIAN_POINT('Ctrl Pts',(20.0316291334108,17.0042470387188,11.9656651753458));
#141105=CARTESIAN_POINT('Ctrl Pts',(19.9594152789104,16.961783381445,11.9698438534298));
#141106=CARTESIAN_POINT('Ctrl Pts',(19.8850075541816,16.9228050473158,11.9740225315137));
#141107=CARTESIAN_POINT('Ctrl Pts',(19.80877704316,16.887542596152,11.9782012095977));
#141108=CARTESIAN_POINT('Ctrl Pts',(19.7311801550142,16.8516480908937,11.9824547874831));
#141109=CARTESIAN_POINT('Ctrl Pts',(19.6516948805983,16.8196042772377,11.9867083653685));
#141110=CARTESIAN_POINT('Ctrl Pts',(19.5707410268099,16.7916065937816,11.990961943254));
#141111=CARTESIAN_POINT('Ctrl Pts',(19.4913566214456,16.7641517000523,11.9951330572319));
#141112=CARTESIAN_POINT('Ctrl Pts',(19.4105605259053,16.7405876095593,11.9993041712099));
#141113=CARTESIAN_POINT('Ctrl Pts',(19.3287692237664,16.721050287564,12.0034752851878));
#141114=CARTESIAN_POINT('Ctrl Pts',(19.2470053674889,16.7015195215057,12.0076449995082));
#141115=CARTESIAN_POINT('Ctrl Pts',(19.1642474149177,16.68601294719,12.0118147138286));
#141116=CARTESIAN_POINT('Ctrl Pts',(19.0809253355089,16.6746161939521,12.015984428149));
#141117=CARTESIAN_POINT('Ctrl Pts',(18.9976062210572,16.6632198462596,12.020153994093));
#141118=CARTESIAN_POINT('Ctrl Pts',(18.9137234755848,16.6559330903703,12.024323560037));
#141119=CARTESIAN_POINT('Ctrl Pts',(18.8297141852422,16.6527899236491,12.0284931259811));
#141120=CARTESIAN_POINT('Ctrl Pts',(18.742751231888,16.6495362470634,12.03280928872));
#141121=CARTESIAN_POINT('Ctrl Pts',(18.655653196516,16.6507229779044,12.0371254514589));
#141122=CARTESIAN_POINT('Ctrl Pts',(18.5689051504087,16.6563290445464,12.0414416141978));
#141123=CARTESIAN_POINT('Ctrl Pts',(18.484982912779,16.6617524941571,12.0456171783895));
#141124=CARTESIAN_POINT('Ctrl Pts',(18.4013886754037,16.6713116809417,12.0497927425812));
#141125=CARTESIAN_POINT('Ctrl Pts',(18.3185547392491,16.6849348315375,12.0539683067729));
#141126=CARTESIAN_POINT('Ctrl Pts',(18.2315370578984,16.6992460550839,12.0583547687854));
#141127=CARTESIAN_POINT('Ctrl Pts',(18.1453590723574,16.7180424488713,12.062741230798));
#141128=CARTESIAN_POINT('Ctrl Pts',(18.0605056905574,16.7411810966898,12.0671276928105));
#141129=CARTESIAN_POINT('Ctrl Pts',(17.9756523087575,16.7643197445083,12.071514154823));
#141130=CARTESIAN_POINT('Ctrl Pts',(17.8921240580815,16.7918003927741,12.0759006168356));
#141131=CARTESIAN_POINT('Ctrl Pts',(17.8103811197834,16.8234221134992,12.0802870788481));
#141132=CARTESIAN_POINT('Ctrl Pts',(17.7323992952485,16.8535888719792,12.0844717132412));
#141133=CARTESIAN_POINT('Ctrl Pts',(17.6557518403844,16.8876362896632,12.0886563476342));
#141134=CARTESIAN_POINT('Ctrl Pts',(17.5808520242221,16.9254257295027,12.0928409820273));
#141135=CARTESIAN_POINT('Ctrl Pts',(17.5060588186774,16.963161380752,12.0970196601112));
#141136=CARTESIAN_POINT('Ctrl Pts',(17.4330087179883,17.0046282689895,12.1011983381951));
#141137=CARTESIAN_POINT('Ctrl Pts',(17.3620964471734,17.0496391690091,12.1053770162791));
#141138=CARTESIAN_POINT('Ctrl Pts',(17.2899131248678,17.0954568570628,12.1096305941645));
#141139=CARTESIAN_POINT('Ctrl Pts',(17.2199454771428,17.1449466854561,12.11388417205));
#141140=CARTESIAN_POINT('Ctrl Pts',(17.1525850704413,17.1978614502303,12.1181377499354));
#141141=CARTESIAN_POINT('Ctrl Pts',(17.0865305766667,17.2497503590347,12.1223088639134));
#141142=CARTESIAN_POINT('Ctrl Pts',(17.0229835115634,17.3049322938693,12.1264799778913));
#141143=CARTESIAN_POINT('Ctrl Pts',(16.9622836350606,17.3631306533724,12.1306510918693));
#141144=CARTESIAN_POINT('Ctrl Pts',(16.9016041269875,17.421309483854,12.1348208061896));
#141145=CARTESIAN_POINT('Ctrl Pts',(16.8437702418585,17.4825024106647,12.13899052051));
#141146=CARTESIAN_POINT('Ctrl Pts',(16.789086714705,17.5463942470714,12.1431602348304));
#141147=CARTESIAN_POINT('Ctrl Pts',(16.734405133426,17.6102838099324,12.1473298007744));
#141148=CARTESIAN_POINT('Ctrl Pts',(16.6828739857151,17.6768717413838,12.1514993667185));
#141149=CARTESIAN_POINT('Ctrl Pts',(16.6347584444193,17.7458089232721,12.1556689326625));
#141150=CARTESIAN_POINT('Ctrl Pts',(16.5849512200484,17.8171698514323,12.1599850954014));
#141151=CARTESIAN_POINT('Ctrl Pts',(16.5388045582795,17.8910478705134,12.1643012581403));
#141152=CARTESIAN_POINT('Ctrl Pts',(16.496563301095,17.9670237066595,12.1686174208793));
#141153=CARTESIAN_POINT('Ctrl Pts',(16.4556980484203,18.0405246379344,12.1727929850709));
#141154=CARTESIAN_POINT('Ctrl Pts',(16.4184878365309,18.1159883689942,12.1769685492626));
#141155=CARTESIAN_POINT('Ctrl Pts',(16.3851063117011,18.1930125535796,12.1811441134543));
#141156=CARTESIAN_POINT('Ctrl Pts',(16.3500387654091,18.2739270466208,12.1855305754669));
#141157=CARTESIAN_POINT('Ctrl Pts',(16.3191970489119,18.3565632259542,12.1899170374794));
#141158=CARTESIAN_POINT('Ctrl Pts',(16.2927234637602,18.4404360029142,12.1943034994919));
#141159=CARTESIAN_POINT('Ctrl Pts',(16.2662498786085,18.5243087798742,12.1986899615045));
#141160=CARTESIAN_POINT('Ctrl Pts',(16.2441444970407,18.6094175737551,12.203076423517));
#141161=CARTESIAN_POINT('Ctrl Pts',(16.2264874578015,18.6952666864385,12.2074628855296));
#141162=CARTESIAN_POINT('Ctrl Pts',(16.2025156137663,18.811818590295,12.2134181072293));
#141163=CARTESIAN_POINT('Ctrl Pts',(16.1866633864877,18.9300931627176,12.219373328929));
#141164=CARTESIAN_POINT('Ctrl Pts',(16.1791211348988,19.0491544419537,12.2253285506288));
#141165=CARTESIAN_POINT('Ctrl Pts',(16.1757600463661,19.10221227165,12.2279824036764));
#141166=CARTESIAN_POINT('Ctrl Pts',(16.1740486686438,19.1554260264049,12.2306362567239));
#141167=CARTESIAN_POINT('Ctrl Pts',(16.174001023388,19.2087109509454,12.2332901097715));
#141168=CARTESIAN_POINT('',(16.1740007840082,19.2130035272629,12.1667098902285));
#141169=CARTESIAN_POINT('Ctrl Pts',(20.2935357313021,17.1808649545431,11.8833305127049));
#141170=CARTESIAN_POINT('Ctrl Pts',(20.2268566426188,17.1296425387906,11.8875000056864));
#141171=CARTESIAN_POINT('Ctrl Pts',(20.1576368380672,17.0816975104457,11.8916694986678));
#141172=CARTESIAN_POINT('Ctrl Pts',(20.0862361972163,17.0372803154643,11.8958389916493));
#141173=CARTESIAN_POINT('Ctrl Pts',(20.0148284810753,16.9928587190582,11.9000088977976));
#141174=CARTESIAN_POINT('Ctrl Pts',(19.9412398908411,16.9519658920357,11.9041788039458));
#141175=CARTESIAN_POINT('Ctrl Pts',(19.8658573577931,16.9148077341804,11.9083487100941));
#141176=CARTESIAN_POINT('Ctrl Pts',(19.7903948874427,16.8776101729941,11.9125230381029));
#141177=CARTESIAN_POINT('Ctrl Pts',(19.7131350895596,16.8441553918421,11.9166973661117));
#141178=CARTESIAN_POINT('Ctrl Pts',(19.6344869976528,16.814602043262,11.9208716941205));
#141179=CARTESIAN_POINT('Ctrl Pts',(19.5557947353724,16.785032096918,11.9250483665171));
#141180=CARTESIAN_POINT('Ctrl Pts',(19.4757130648504,16.7593680861741,11.9292250389137));
#141181=CARTESIAN_POINT('Ctrl Pts',(19.3946660667926,16.7377187082362,11.9334017113104));
#141182=CARTESIAN_POINT('Ctrl Pts',(19.3134800357285,16.7160321916235,11.9375855486277));
#141183=CARTESIAN_POINT('Ctrl Pts',(19.2313258199933,16.6983741580632,11.9417693859451));
#141184=CARTESIAN_POINT('Ctrl Pts',(19.1486372983812,16.6848020840023,11.9459532232625));
#141185=CARTESIAN_POINT('Ctrl Pts',(19.0921615511293,16.6755324416214,11.9488107581933));
#141186=CARTESIAN_POINT('Ctrl Pts',(19.0354367169183,16.6681677363091,11.9516682931241));
#141187=CARTESIAN_POINT('Ctrl Pts',(18.9786013944249,16.662712308658,11.9545258280548));
#141188=CARTESIAN_POINT('Ctrl Pts',(18.8953705500055,16.6547232653983,11.9587104624479));
#141189=CARTESIAN_POINT('Ctrl Pts',(18.8115930039275,16.6508013065455,11.9628950968409));
#141190=CARTESIAN_POINT('Ctrl Pts',(18.7277003248361,16.6510077511655,11.967079731234));
#141191=CARTESIAN_POINT('Ctrl Pts',(18.6439270565892,16.6512139019371,11.9712584093179));
#141192=CARTESIAN_POINT('Ctrl Pts',(18.5600394369382,16.655536782935,11.9754370874019));
#141193=CARTESIAN_POINT('Ctrl Pts',(18.476474237527,16.6639859675175,11.9796157654858));
#141194=CARTESIAN_POINT('Ctrl Pts',(18.3914111919738,16.6725865976613,11.9838693433713));
#141195=CARTESIAN_POINT('Ctrl Pts',(18.306682719051,16.6854629604529,11.9881229212567));
#141196=CARTESIAN_POINT('Ctrl Pts',(18.2227496524044,16.7025695979192,11.9923764991421));
#141197=CARTESIAN_POINT('Ctrl Pts',(18.1404437920366,16.7193445898373,11.9965476131201));
#141198=CARTESIAN_POINT('Ctrl Pts',(18.0589032436843,16.7401871997927,12.0007187270981));
#141199=CARTESIAN_POINT('Ctrl Pts',(17.9785557081123,16.7650024689599,12.004889841076));
#141200=CARTESIAN_POINT('Ctrl Pts',(17.8982351339319,16.7898094111239,12.0090595553964));
#141201=CARTESIAN_POINT('Ctrl Pts',(17.819107216657,16.8185862293725,12.0132292697168));
#141202=CARTESIAN_POINT('Ctrl Pts',(17.7415856439031,16.8511877731877,12.0173989840371));
#141203=CARTESIAN_POINT('Ctrl Pts',(17.6640668296994,16.8837881569001,12.0215685499812));
#141204=CARTESIAN_POINT('Ctrl Pts',(17.5881546700955,16.9202128164544,12.0257381159252));
#141205=CARTESIAN_POINT('Ctrl Pts',(17.5142426975059,16.9602685360061,12.0299076818693));
#141206=CARTESIAN_POINT('Ctrl Pts',(17.4377320711404,17.0017325652431,12.0342238446082));
#141207=CARTESIAN_POINT('Ctrl Pts',(17.3633653656321,17.047087490087,12.0385400073471));
#141208=CARTESIAN_POINT('Ctrl Pts',(17.2915493867659,17.0960682686242,12.042856170086));
#141209=CARTESIAN_POINT('Ctrl Pts',(17.2220728058575,17.1434535034523,12.0470317342777));
#141210=CARTESIAN_POINT('Ctrl Pts',(17.1549836708366,17.1942316733332,12.0512072984694));
#141211=CARTESIAN_POINT('Ctrl Pts',(17.0906175572634,17.2481209545911,12.0553828626611));
#141212=CARTESIAN_POINT('Ctrl Pts',(17.0230004643096,17.3047320553358,12.0597693246736));
#141213=CARTESIAN_POINT('Ctrl Pts',(16.9583891293618,17.3647764140015,12.0641557866861));
#141214=CARTESIAN_POINT('Ctrl Pts',(16.897128197962,17.4278841925221,12.0685422486987));
#141215=CARTESIAN_POINT('Ctrl Pts',(16.8358672665622,17.4909919710426,12.0729287107112));
#141216=CARTESIAN_POINT('Ctrl Pts',(16.7779570635865,17.5571626827013,12.0773151727237));
#141217=CARTESIAN_POINT('Ctrl Pts',(16.7236914224212,17.6259891410741,12.0817016347363));
#141218=CARTESIAN_POINT('Ctrl Pts',(16.6719732357611,17.6915845997261,12.0858821780095));
#141219=CARTESIAN_POINT('Ctrl Pts',(16.62336875941,17.759841108002,12.0900627212828));
#141220=CARTESIAN_POINT('Ctrl Pts',(16.5781640651477,17.8304307616062,12.094243264556));
#141221=CARTESIAN_POINT('Ctrl Pts',(16.5330221281563,17.9009224162283,12.0984180040186));
#141222=CARTESIAN_POINT('Ctrl Pts',(16.4912708487475,17.9737404018919,12.1025927434812));
#141223=CARTESIAN_POINT('Ctrl Pts',(16.4531558825329,18.0485241457064,12.1067674829438));
#141224=CARTESIAN_POINT('Ctrl Pts',(16.4150823671077,18.1232265607011,12.1109376822935));
#141225=CARTESIAN_POINT('Ctrl Pts',(16.3806375190246,18.1998900805266,12.1151078816433));
#141226=CARTESIAN_POINT('Ctrl Pts',(16.350022764859,18.2781267276155,12.1192780809931));
#141227=CARTESIAN_POINT('Ctrl Pts',(16.3194306012405,18.3563056440868,12.1234452031636));
#141228=CARTESIAN_POINT('Ctrl Pts',(16.2926630858421,18.4360549550053,12.1276123253342));
#141229=CARTESIAN_POINT('Ctrl Pts',(16.2698743296475,18.5169649283287,12.1317794475047));
#141230=CARTESIAN_POINT('Ctrl Pts',(16.2470959536793,18.597838047344,12.1359446715606));
#141231=CARTESIAN_POINT('Ctrl Pts',(16.2282928589741,18.6798703351889,12.1401098956165));
#141232=CARTESIAN_POINT('Ctrl Pts',(16.2135694673997,18.7626363860258,12.1442751196725));
#141233=CARTESIAN_POINT('Ctrl Pts',(16.1988435352844,18.8454167182549,12.1484410624433));
#141234=CARTESIAN_POINT('Ctrl Pts',(16.1881988016352,18.9289306143268,12.1526070052142));
#141235=CARTESIAN_POINT('Ctrl Pts',(16.181688476361,19.0127428783137,12.1567729479851));
#141236=CARTESIAN_POINT('Ctrl Pts',(16.1765121589546,19.0793814658902,12.1600852620662));
#141237=CARTESIAN_POINT('Ctrl Pts',(16.1739485082683,19.146208402676,12.1633975761474));
#141238=CARTESIAN_POINT('Ctrl Pts',(16.1740007840082,19.2130035272629,12.1667098902285));
#141239=CARTESIAN_POINT('Ctrl Pts',(16.1763509819005,19.2130199893541,12.1667107986141));
#141240=CARTESIAN_POINT('Ctrl Pts',(16.174290235218,19.4962014494758,12.1807663462153));
#141241=CARTESIAN_POINT('Ctrl Pts',(16.3483939114844,20.6310006362221,12.237213829377));
#141242=CARTESIAN_POINT('Ctrl Pts',(18.0121684955946,22.150770613565,12.3360532480991));
#141243=CARTESIAN_POINT('Ctrl Pts',(20.8151681545049,21.409188138856,12.4632290547806));
#141244=CARTESIAN_POINT('Ctrl Pts',(21.6282770636252,18.8995173227485,12.5789421032606));
#141245=CARTESIAN_POINT('Ctrl Pts',(20.782749801677,17.5654744033761,12.6522632161801));
#141246=CARTESIAN_POINT('Ctrl Pts',(20.2929505239237,17.1816081970507,12.6831923935391));
#141247=CARTESIAN_POINT('Origin',(18.734,19.211,-1.76670989022852));
#141248=CARTESIAN_POINT('',(20.2935357313021,17.1808649545431,13.5498657053664));
#141249=CARTESIAN_POINT('',(20.2935357313021,17.1808649545432,13.4833228577974));
#141250=CARTESIAN_POINT('',(20.2935357313021,17.1808649545432,-1.76670989022852));
#141251=CARTESIAN_POINT('',(16.174000001606,19.2109093211998,13.0332901097364));
#141252=CARTESIAN_POINT('Ctrl Pts',(16.174000001606,19.2109093219104,13.0332901097715));
#141253=CARTESIAN_POINT('Ctrl Pts',(16.1739968821085,19.2989781543512,13.0376462156856));
#141254=CARTESIAN_POINT('Ctrl Pts',(16.1785426714359,19.3869643923453,13.0420023215996));
#141255=CARTESIAN_POINT('Ctrl Pts',(16.1875860737585,19.4743934627951,13.0463584275137));
#141256=CARTESIAN_POINT('Ctrl Pts',(16.1966529338893,19.5620493167382,13.0507258327921));
#141257=CARTESIAN_POINT('Ctrl Pts',(16.2102406836426,19.6491447181138,13.0550932380704));
#141258=CARTESIAN_POINT('Ctrl Pts',(16.2282463851319,19.7352125728895,13.0594606433488));
#141259=CARTESIAN_POINT('Ctrl Pts',(16.2462755658189,19.8213926590147,13.0638337436661));
#141260=CARTESIAN_POINT('Ctrl Pts',(16.2687340840994,19.9065421429603,13.0682068439834));
#141261=CARTESIAN_POINT('Ctrl Pts',(16.2954690366782,19.9902090482795,13.0725799443008));
#141262=CARTESIAN_POINT('Ctrl Pts',(16.3222767415773,20.0741036316347,13.0769649448896));
#141263=CARTESIAN_POINT('Ctrl Pts',(16.3533840099471,20.1565071961889,13.0813499454785));
#141264=CARTESIAN_POINT('Ctrl Pts',(16.3885892814888,20.2369866283206,13.0857349460673));
#141265=CARTESIAN_POINT('Ctrl Pts',(16.4205927188907,20.310146651112,13.0897211414781));
#141266=CARTESIAN_POINT('Ctrl Pts',(16.4559819492917,20.3817167133684,13.0937073368888));
#141267=CARTESIAN_POINT('Ctrl Pts',(16.4945737975983,20.4513911818441,13.0976935322996));
#141268=CARTESIAN_POINT('Ctrl Pts',(16.5350868078939,20.524534153289,13.1018781666926));
#141269=CARTESIAN_POINT('Ctrl Pts',(16.5792624158945,20.5958263313022,13.1060628010857));
#141270=CARTESIAN_POINT('Ctrl Pts',(16.6269069559,20.6648771968449,13.1102474354787));
#141271=CARTESIAN_POINT('Ctrl Pts',(16.6744836798,20.7338297770272,13.1144261135626));
#141272=CARTESIAN_POINT('Ctrl Pts',(16.7255192690591,20.8005470061347,13.1186047916466));
#141273=CARTESIAN_POINT('Ctrl Pts',(16.7797744504213,20.8646633579341,13.1227834697305));
#141274=CARTESIAN_POINT('Ctrl Pts',(16.8350021169169,20.9299289492599,13.127037047616));
#141275=CARTESIAN_POINT('Ctrl Pts',(16.8935656995718,20.9924990829437,13.1312906255014));
#141276=CARTESIAN_POINT('Ctrl Pts',(16.9551669364597,21.0520195360332,13.1355442033868));
#141277=CARTESIAN_POINT('Ctrl Pts',(17.0155739131657,21.110386068995,13.1397153173648));
#141278=CARTESIAN_POINT('Ctrl Pts',(17.0789014673909,21.1658197797781,13.1438864313427));
#141279=CARTESIAN_POINT('Ctrl Pts',(17.1448292745178,21.2180217749866,13.1480575453207));
#141280=CARTESIAN_POINT('Ctrl Pts',(17.2107349589323,21.2702062533115,13.1522272596411));
#141281=CARTESIAN_POINT('Ctrl Pts',(17.279238803008,21.3191608844269,13.1563969739614));
#141282=CARTESIAN_POINT('Ctrl Pts',(17.3499870301186,21.364626731632,13.1605666882818));
#141283=CARTESIAN_POINT('Ctrl Pts',(17.4207327397037,21.4100909609672,13.1647362542259));
#141284=CARTESIAN_POINT('Ctrl Pts',(17.493722286064,21.4520664052353,13.1689058201699));
#141285=CARTESIAN_POINT('Ctrl Pts',(17.5685736694553,21.490337945122,13.1730753861139));
#141286=CARTESIAN_POINT('Ctrl Pts',(17.6460567351475,21.5299550651381,13.1773915488529));
#141287=CARTESIAN_POINT('Ctrl Pts',(17.7255345286225,21.5656027360313,13.1817077115918));
#141288=CARTESIAN_POINT('Ctrl Pts',(17.8065583197873,21.5970955407955,13.1860238743307));
#141289=CARTESIAN_POINT('Ctrl Pts',(17.8849427694771,21.627562470757,13.1901994385224));
#141290=CARTESIAN_POINT('Ctrl Pts',(17.9647735800336,21.654140963194,13.1943750027141));
#141291=CARTESIAN_POINT('Ctrl Pts',(18.0456284938942,21.6767138255648,13.1985505669057));
#141292=CARTESIAN_POINT('Ctrl Pts',(18.1305671972396,21.7004267895521,13.2029370289183));
#141293=CARTESIAN_POINT('Ctrl Pts',(18.2166356079045,21.7197187126534,13.2073234909308));
#141294=CARTESIAN_POINT('Ctrl Pts',(18.3033337697291,21.7345147311051,13.2117099529434));
#141295=CARTESIAN_POINT('Ctrl Pts',(18.3900319315536,21.7493107495567,13.2160964149559));
#141296=CARTESIAN_POINT('Ctrl Pts',(18.4773592594052,21.7596108709354,13.2204828769685));
#141297=CARTESIAN_POINT('Ctrl Pts',(18.5648137584886,21.7654032601927,13.224869338981));
#141298=CARTESIAN_POINT('Ctrl Pts',(18.6482443464305,21.7709291330339,13.2290539733741));
#141299=CARTESIAN_POINT('Ctrl Pts',(18.7321012046618,21.7723735414423,13.2332386077671));
#141300=CARTESIAN_POINT('Ctrl Pts',(18.8159511409016,21.7696879470746,13.2374232421601));
#141301=CARTESIAN_POINT('Ctrl Pts',(18.8996817271358,21.7670061753181,13.2416019202441));
#141302=CARTESIAN_POINT('Ctrl Pts',(18.9834049550843,21.7602060920318,13.2457805983281));
#141303=CARTESIAN_POINT('Ctrl Pts',(19.0666839609554,21.749291035741,13.249959276412));
#141304=CARTESIAN_POINT('Ctrl Pts',(19.1514556831552,21.7381803349106,13.2542128542974));
#141305=CARTESIAN_POINT('Ctrl Pts',(19.2357666201898,21.7228056564124,13.2584664321829));
#141306=CARTESIAN_POINT('Ctrl Pts',(19.3191574830897,21.7032260571594,13.2627200100683));
#141307=CARTESIAN_POINT('Ctrl Pts',(19.4009316513884,21.6840260466443,13.2668911240463));
#141308=CARTESIAN_POINT('Ctrl Pts',(19.4818206335821,21.660782811607,13.2710622380242));
#141309=CARTESIAN_POINT('Ctrl Pts',(19.5613997219857,21.6336039090322,13.2752333520022));
#141310=CARTESIAN_POINT('Ctrl Pts',(19.6409521068576,21.6064341266006,13.2794030663225));
#141311=CARTESIAN_POINT('Ctrl Pts',(19.7191950359073,21.5753314480261,13.2835727806429));
#141312=CARTESIAN_POINT('Ctrl Pts',(19.7957192917692,21.5404531859398,13.2877424949633));
#141313=CARTESIAN_POINT('Ctrl Pts',(19.8722408245697,21.5055761649718,13.2919120609073));
#141314=CARTESIAN_POINT('Ctrl Pts',(19.9470433875298,21.466924019184,13.2960816268514));
#141315=CARTESIAN_POINT('Ctrl Pts',(20.019739330133,21.4247015099035,13.3002511927954));
#141316=CARTESIAN_POINT('Ctrl Pts',(20.0949911723979,21.380994509284,13.3045673555344));
#141317=CARTESIAN_POINT('Ctrl Pts',(20.1679850444452,21.333461670748,13.3088835182733));
#141318=CARTESIAN_POINT('Ctrl Pts',(20.2383221508272,21.2823799425819,13.3131996810122));
#141319=CARTESIAN_POINT('Ctrl Pts',(20.3063680333671,21.232962196338,13.3173752452039));
#141320=CARTESIAN_POINT('Ctrl Pts',(20.3719272430122,21.1802235520147,13.3215508093956));
#141321=CARTESIAN_POINT('Ctrl Pts',(20.4346726793712,21.1244556272986,13.3257263735873));
#141322=CARTESIAN_POINT('Ctrl Pts',(20.5005872385574,21.0658709972807,13.3301128355998));
#141323=CARTESIAN_POINT('Ctrl Pts',(20.5633958911488,21.0039434366074,13.3344992976123));
#141324=CARTESIAN_POINT('Ctrl Pts',(20.6227650717808,20.9390528069538,13.3388857596249));
#141325=CARTESIAN_POINT('Ctrl Pts',(20.6821342524128,20.8741621773001,13.3432722216374));
#141326=CARTESIAN_POINT('Ctrl Pts',(20.738063650735,20.8063089747713,13.3476586836499));
#141327=CARTESIAN_POINT('Ctrl Pts',(20.7902715950829,20.7359088914605,13.3520451456625));
#141328=CARTESIAN_POINT('Ctrl Pts',(20.8400773745207,20.6687480203406,13.3562297800555));
#141329=CARTESIAN_POINT('Ctrl Pts',(20.8866820202991,20.5990195040797,13.3604144144486));
#141330=CARTESIAN_POINT('Ctrl Pts',(20.9298102405871,20.5270613159472,13.3645990488416));
#141331=CARTESIAN_POINT('Ctrl Pts',(20.9728770731919,20.4552055513888,13.3687777269256));
#141332=CARTESIAN_POINT('Ctrl Pts',(21.0124770746366,20.3811268100631,13.3729564050095));
#141333=CARTESIAN_POINT('Ctrl Pts',(21.0483765860078,20.305194232364,13.3771350830935));
#141334=CARTESIAN_POINT('Ctrl Pts',(21.0849195703199,20.2279006177816,13.3813886609789));
#141335=CARTESIAN_POINT('Ctrl Pts',(21.1176278099319,20.1486864403633,13.3856422388643));
#141336=CARTESIAN_POINT('Ctrl Pts',(21.1463023579538,20.0679698558354,13.3898958167498));
#141337=CARTESIAN_POINT('Ctrl Pts',(21.1744209939084,19.9888181198042,13.3940669307277));
#141338=CARTESIAN_POINT('Ctrl Pts',(21.1986607834443,19.9082221644555,13.3982380447057));
#141339=CARTESIAN_POINT('Ctrl Pts',(21.2188822787495,19.8265973202968,13.4024091586836));
#141340=CARTESIAN_POINT('Ctrl Pts',(21.2390969885367,19.7449998661428,13.406578873004));
#141341=CARTESIAN_POINT('Ctrl Pts',(21.2552959714612,19.6623746550205,13.4107485873244));
#141342=CARTESIAN_POINT('Ctrl Pts',(21.2673900009521,19.5791509243179,13.4149183016447));
#141343=CARTESIAN_POINT('Ctrl Pts',(21.2794836000854,19.4959301550728,13.4190878675888));
#141344=CARTESIAN_POINT('Ctrl Pts',(21.2874724709,19.4121113639667,13.4232574335328));
#141345=CARTESIAN_POINT('Ctrl Pts',(21.2913189573957,19.3281313371595,13.4274269994769));
#141346=CARTESIAN_POINT('Ctrl Pts',(21.2953006816113,19.2411986762104,13.4317431622158));
#141347=CARTESIAN_POINT('Ctrl Pts',(21.2948432851383,19.1540937573814,13.4360593249547));
#141348=CARTESIAN_POINT('Ctrl Pts',(21.2899637772452,19.0673018113878,13.4403754876936));
#141349=CARTESIAN_POINT('Ctrl Pts',(21.2852432188086,18.9833371039062,13.4445510518853));
#141350=CARTESIAN_POINT('Ctrl Pts',(21.2763843217563,18.89966575566,13.448726616077));
#141351=CARTESIAN_POINT('Ctrl Pts',(21.2634552371753,18.8167206534363,13.4529021802687));
#141352=CARTESIAN_POINT('Ctrl Pts',(21.249873135268,18.7295861912825,13.4572886422812));
#141353=CARTESIAN_POINT('Ctrl Pts',(21.2317989893781,18.6432538400943,13.4616751042937));
#141354=CARTESIAN_POINT('Ctrl Pts',(21.2093716504547,18.5582096874759,13.4660615663063));
#141355=CARTESIAN_POINT('Ctrl Pts',(21.1869443115313,18.4731655348574,13.4704480283188));
#141356=CARTESIAN_POINT('Ctrl Pts',(21.1601640287335,18.3894101102965,13.4748344903314));
#141357=CARTESIAN_POINT('Ctrl Pts',(21.1292278697973,18.3074052613331,13.4792209523439));
#141358=CARTESIAN_POINT('Ctrl Pts',(21.099717216383,18.2291791091776,13.4834052908209));
#141359=CARTESIAN_POINT('Ctrl Pts',(21.066315417783,18.1522546019502,13.4875896292979));
#141360=CARTESIAN_POINT('Ctrl Pts',(21.0291576153336,18.0770460676129,13.4917739677749));
#141361=CARTESIAN_POINT('Ctrl Pts',(20.992050293613,18.0019397078225,13.4959526216193));
#141362=CARTESIAN_POINT('Ctrl Pts',(20.951197302462,17.9285451006079,13.5001312754636));
#141363=CARTESIAN_POINT('Ctrl Pts',(20.906782548638,17.8572585193863,13.504309929308));
#141364=CARTESIAN_POINT('Ctrl Pts',(20.8624197060777,17.7860552567964,13.5084836992077));
#141365=CARTESIAN_POINT('Ctrl Pts',(20.8145036177023,17.7169555110608,13.5126574691073));
#141366=CARTESIAN_POINT('Ctrl Pts',(20.7632642938687,17.6503314171069,13.516831239007));
#141367=CARTESIAN_POINT('Ctrl Pts',(20.7120601643926,17.5837530847285,13.5210021421017));
#141368=CARTESIAN_POINT('Ctrl Pts',(20.6575376129952,17.5196473901183,13.5251730451963));
#141369=CARTESIAN_POINT('Ctrl Pts',(20.5999695483242,17.4583569545607,13.529343948291));
#141370=CARTESIAN_POINT('Ctrl Pts',(20.5424157972193,17.3970817580893,13.5335138143437));
#141371=CARTESIAN_POINT('Ctrl Pts',(20.481818346985,17.338620769584,13.5376836803964));
#141372=CARTESIAN_POINT('Ctrl Pts',(20.4184891456858,17.2832820958276,13.5418535464492));
#141373=CARTESIAN_POINT('Ctrl Pts',(20.3779280006757,17.2478387312367,13.5445242660882));
#141374=CARTESIAN_POINT('Ctrl Pts',(20.3362470303383,17.2136754796983,13.5471949857273));
#141375=CARTESIAN_POINT('Ctrl Pts',(20.2935357313021,17.1808649545431,13.5498657053664));
#141376=CARTESIAN_POINT('Ctrl Pts',(20.2935357313021,17.1808649545432,12.7499597618547));
#141377=CARTESIAN_POINT('Ctrl Pts',(20.2269466206031,17.1297116592572,12.7541315981782));
#141378=CARTESIAN_POINT('Ctrl Pts',(20.1577807292293,17.0817939555633,12.7583034345017));
#141379=CARTESIAN_POINT('Ctrl Pts',(20.0863882141111,17.0373748901125,12.7624752708252));
#141380=CARTESIAN_POINT('Ctrl Pts',(20.0150265963101,16.992975048385,12.7666453016577));
#141381=CARTESIAN_POINT('Ctrl Pts',(19.9414406583524,16.9520710809438,12.7708153324901));
#141382=CARTESIAN_POINT('Ctrl Pts',(19.8660096487203,16.9148828089133,12.7749853633225));
#141383=CARTESIAN_POINT('Ctrl Pts',(19.7905886566178,16.8776994756289,12.7791548403587));
#141384=CARTESIAN_POINT('Ctrl Pts',(19.7133234924244,16.8442310603422,12.7833243173949));
#141385=CARTESIAN_POINT('Ctrl Pts',(19.6346168965686,16.8146508589909,12.7874937944311));
#141386=CARTESIAN_POINT('Ctrl Pts',(19.555897143493,16.7850657127781,12.7916639684702));
#141387=CARTESIAN_POINT('Ctrl Pts',(19.4757359113357,16.7593702317383,12.7958341425094));
#141388=CARTESIAN_POINT('Ctrl Pts',(19.3945534566075,16.7376886304058,12.8000043165485));
#141389=CARTESIAN_POINT('Ctrl Pts',(19.3132817042356,16.7159831801282,12.804179077622));
#141390=CARTESIAN_POINT('Ctrl Pts',(19.2309869325325,16.6983005401868,12.8083538386956));
#141391=CARTESIAN_POINT('Ctrl Pts',(19.1481014831742,16.6847141963679,12.8125285997691));
#141392=CARTESIAN_POINT('Ctrl Pts',(19.0651644239002,16.6711193928005,12.8167059603227));
#141393=CARTESIAN_POINT('Ctrl Pts',(18.9816364116983,16.6616260140211,12.8208833208762));
#141394=CARTESIAN_POINT('Ctrl Pts',(18.8979544455511,16.6562556018685,12.8250606814298));
#141395=CARTESIAN_POINT('Ctrl Pts',(18.8141346488939,16.6508763442422,12.8292449224112));
#141396=CARTESIAN_POINT('Ctrl Pts',(18.7301608515015,16.6496336145246,12.8334291633927));
#141397=CARTESIAN_POINT('Ctrl Pts',(18.6464691460235,16.6524968537049,12.8376134043741));
#141398=CARTESIAN_POINT('Ctrl Pts',(18.6082759065393,16.6538035110264,12.8395229092283));
#141399=CARTESIAN_POINT('Ctrl Pts',(18.5701413311388,16.6559645682452,12.8414324140825));
#141400=CARTESIAN_POINT('Ctrl Pts',(18.5321062576876,16.6589735665916,12.8433419189367));
#141401=CARTESIAN_POINT('Ctrl Pts',(18.4487533004234,16.665567714777,12.8475265533297));
#141402=CARTESIAN_POINT('Ctrl Pts',(18.3655686284662,16.6762620749485,12.8517111877228));
#141403=CARTESIAN_POINT('Ctrl Pts',(18.2829879003452,16.6910420467863,12.8558958221158));
#141404=CARTESIAN_POINT('Ctrl Pts',(18.2005247156691,16.7058009811636,12.8600745001998));
#141405=CARTESIAN_POINT('Ctrl Pts',(18.1186642162791,16.7246338957134,12.8642531782837));
#141406=CARTESIAN_POINT('Ctrl Pts',(18.0378381935504,16.7474743274646,12.8684318563677));
#141407=CARTESIAN_POINT('Ctrl Pts',(17.9555634224531,16.7707241575398,12.8726854342531));
#141408=CARTESIAN_POINT('Ctrl Pts',(17.8743610594189,16.7981265494107,12.8769390121385));
#141409=CARTESIAN_POINT('Ctrl Pts',(17.794677029921,16.8295566649861,12.881192590024));
#141410=CARTESIAN_POINT('Ctrl Pts',(17.7165378308257,16.8603774464402,12.8853637040019));
#141411=CARTESIAN_POINT('Ctrl Pts',(17.6398590665653,16.8950709981006,12.8895348179799));
#141412=CARTESIAN_POINT('Ctrl Pts',(17.5650454327531,16.933469490937,12.8937059319578));
#141413=CARTESIAN_POINT('Ctrl Pts',(17.4902569033782,16.9718550987884,12.8978756462782));
#141414=CARTESIAN_POINT('Ctrl Pts',(17.4173326704111,17.0139429688571,12.9020453605985));
#141415=CARTESIAN_POINT('Ctrl Pts',(17.3466549084732,17.0595182787166,12.9062150749189));
#141416=CARTESIAN_POINT('Ctrl Pts',(17.2759796615534,17.1050919668111,12.9103846408629));
#141417=CARTESIAN_POINT('Ctrl Pts',(17.2075511128835,17.1541525979349,12.914554206807));
#141418=CARTESIAN_POINT('Ctrl Pts',(17.1417232369316,17.2064415174926,12.918723772751));
#141419=CARTESIAN_POINT('Ctrl Pts',(17.0735809340684,17.2605688509567,12.9230399354899));
#141420=CARTESIAN_POINT('Ctrl Pts',(17.0082259988606,17.3181553818451,12.9273560982289));
#141421=CARTESIAN_POINT('Ctrl Pts',(16.946012997198,17.3788694157317,12.9316722609678));
#141422=CARTESIAN_POINT('Ctrl Pts',(16.8858265775211,17.4376056963503,12.9358478251595));
#141423=CARTESIAN_POINT('Ctrl Pts',(16.8285808237901,17.4992684748645,12.9400233893511));
#141424=CARTESIAN_POINT('Ctrl Pts',(16.77455723925,17.5635219068696,12.9441989535428));
#141425=CARTESIAN_POINT('Ctrl Pts',(16.7178050518835,17.6310206269775,12.9485854155554));
#141426=CARTESIAN_POINT('Ctrl Pts',(16.6646094437671,17.7013781204553,12.9529718775679));
#141427=CARTESIAN_POINT('Ctrl Pts',(16.6152455573351,17.7741702913401,12.9573583395805));
#141428=CARTESIAN_POINT('Ctrl Pts',(16.565881670903,17.846962462225,12.961744801593));
#141429=CARTESIAN_POINT('Ctrl Pts',(16.5203497415207,17.922188774755,12.9661312636056));
#141430=CARTESIAN_POINT('Ctrl Pts',(16.4788683829465,17.9993971815129,12.9705177256181));
#141431=CARTESIAN_POINT('Ctrl Pts',(16.4371381237559,18.0770688619124,12.9749305077209));
#141432=CARTESIAN_POINT('Ctrl Pts',(16.3993648293881,18.1570094498413,12.9793432898236));
#141433=CARTESIAN_POINT('Ctrl Pts',(16.3657873879884,18.2388019624021,12.9837560719264));
#141434=CARTESIAN_POINT('Ctrl Pts',(16.3323070847556,18.3203578525641,12.9881560880307));
#141435=CARTESIAN_POINT('Ctrl Pts',(16.3029985969533,18.4037546379833,12.992556104135));
#141436=CARTESIAN_POINT('Ctrl Pts',(16.2780542372553,18.4885524860197,12.9969561202393));
#141437=CARTESIAN_POINT('Ctrl Pts',(16.2531532512187,18.5732028861683,13.0013484855236));
#141438=CARTESIAN_POINT('Ctrl Pts',(16.2326014031163,18.6592491335653,13.0057408508078));
#141439=CARTESIAN_POINT('Ctrl Pts',(16.2165427462274,18.7462323425329,13.010133216092));
#141440=CARTESIAN_POINT('Ctrl Pts',(16.2005210016679,18.833015612434,13.0145154851125));
#141441=CARTESIAN_POINT('Ctrl Pts',(16.1889719431304,18.9207311752712,13.018897754133));
#141442=CARTESIAN_POINT('Ctrl Pts',(16.1819893075699,19.0089073833058,13.0232800231536));
#141443=CARTESIAN_POINT('Ctrl Pts',(16.176672671659,19.0760454703589,13.0266167186812));
#141444=CARTESIAN_POINT('Ctrl Pts',(16.1740023911013,19.1434502453368,13.0299534142088));
#141445=CARTESIAN_POINT('Ctrl Pts',(16.174000001606,19.2109093211998,13.0332901097364));
#141446=CARTESIAN_POINT('',(16.1736697067219,19.2116425106688,12.9667098340815));
#141447=CARTESIAN_POINT('Ctrl Pts',(20.2929505239237,17.1816081970507,12.6831923935391));
#141448=CARTESIAN_POINT('Ctrl Pts',(20.1114244968023,17.0393423535811,12.6946551517406));
#141449=CARTESIAN_POINT('Ctrl Pts',(19.1726622027867,16.486376634711,12.7485098455025));
#141450=CARTESIAN_POINT('Ctrl Pts',(17.0319370398065,16.7305239353302,12.8430154491721));
#141451=CARTESIAN_POINT('Ctrl Pts',(16.1727139355615,18.3978728515243,12.9260582946402));
#141452=CARTESIAN_POINT('Ctrl Pts',(16.1699654719056,19.2116308397489,12.9667092045479));
#141453=CARTESIAN_POINT('Ctrl Pts',(16.1740000808904,19.2116435515775,12.9667098902285));
#141454=CARTESIAN_POINT('Ctrl Pts',(16.1740088273484,19.2464363059256,12.9684506873211));
#141455=CARTESIAN_POINT('Ctrl Pts',(16.1747268399112,19.281219269613,12.9701914844137));
#141456=CARTESIAN_POINT('Ctrl Pts',(16.1761531171477,19.3159729673894,12.9719322815063));
#141457=CARTESIAN_POINT('Ctrl Pts',(16.1795816894971,19.3995160291397,12.9761169158993));
#141458=CARTESIAN_POINT('Ctrl Pts',(16.1871139062631,19.4830464110296,12.9803015502924));
#141459=CARTESIAN_POINT('Ctrl Pts',(16.1987516982625,19.5661282142232,12.9844861846854));
#141460=CARTESIAN_POINT('Ctrl Pts',(16.2103729253056,19.6490917607534,12.9886648627694));
#141461=CARTESIAN_POINT('Ctrl Pts',(16.2260880567289,19.7316075451534,12.9928435408533));
#141462=CARTESIAN_POINT('Ctrl Pts',(16.2458470513545,19.8132415662726,12.9970222189372));
#141463=CARTESIAN_POINT('Ctrl Pts',(16.2659602117582,19.896338818551,13.0012757968227));
#141464=CARTESIAN_POINT('Ctrl Pts',(16.2902636140325,19.9785219036749,13.0055293747081));
#141465=CARTESIAN_POINT('Ctrl Pts',(16.3186494198466,20.0593404829151,13.0097829525936));
#141466=CARTESIAN_POINT('Ctrl Pts',(16.3464849114246,20.1385922362921,13.0139540665715));
#141467=CARTESIAN_POINT('Ctrl Pts',(16.3782457689157,20.2165314648406,13.0181251805495));
#141468=CARTESIAN_POINT('Ctrl Pts',(16.4137796304916,20.2927473997743,13.0222962945274));
#141469=CARTESIAN_POINT('Ctrl Pts',(16.4493015683371,20.3689377597149,13.0264660088478));
#141470=CARTESIAN_POINT('Ctrl Pts',(16.4885938016079,20.4434055578922,13.0306357231682));
#141471=CARTESIAN_POINT('Ctrl Pts',(16.5314561548597,20.5157607482732,13.0348054374885));
#141472=CARTESIAN_POINT('Ctrl Pts',(16.574316982885,20.5881133639461,13.0389750034326));
#141473=CARTESIAN_POINT('Ctrl Pts',(16.6207474431038,20.6583531259277,13.0431445693766));
#141474=CARTESIAN_POINT('Ctrl Pts',(16.6705024900496,20.7261165058927,13.0473141353206));
#141475=CARTESIAN_POINT('Ctrl Pts',(16.7220068630667,20.7962623627024,13.0516302980596));
#141476=CARTESIAN_POINT('Ctrl Pts',(16.7770736453881,20.8637540331555,13.0559464607985));
#141477=CARTESIAN_POINT('Ctrl Pts',(16.8353848266791,20.9282246281822,13.0602626235374));
#141478=CARTESIAN_POINT('Ctrl Pts',(16.8917965273727,20.9905951003569,13.0644381877291));
#141479=CARTESIAN_POINT('Ctrl Pts',(16.951244134227,21.0501379976127,13.0686137519208));
#141480=CARTESIAN_POINT('Ctrl Pts',(17.0134027193005,21.1065592836019,13.0727893161124));
#141481=CARTESIAN_POINT('Ctrl Pts',(17.0787007867382,21.1658302746177,13.077175778125));
#141482=CARTESIAN_POINT('Ctrl Pts',(17.1469904406111,21.2216556522274,13.0815622401375));
#141483=CARTESIAN_POINT('Ctrl Pts',(17.2178583236868,21.273744389726,13.0859487021501));
#141484=CARTESIAN_POINT('Ctrl Pts',(17.2887262067624,21.3258331272246,13.0903351641627));
#141485=CARTESIAN_POINT('Ctrl Pts',(17.3621717925896,21.3741849690991,13.0947216261752));
#141486=CARTESIAN_POINT('Ctrl Pts',(17.4377516489582,21.4185643167123,13.0991080881878));
#141487=CARTESIAN_POINT('Ctrl Pts',(17.5098539640988,21.4609017047557,13.1032927225808));
#141488=CARTESIAN_POINT('Ctrl Pts',(17.5841668423744,21.4997817138926,13.1074773569739));
#141489=CARTESIAN_POINT('Ctrl Pts',(17.660324806961,21.5349667768392,13.1116619913669));
#141490=CARTESIAN_POINT('Ctrl Pts',(17.7363743701113,21.5701017582038,13.1158406694508));
#141491=CARTESIAN_POINT('Ctrl Pts',(17.8142633889641,21.6015520487103,13.1200193475348));
#141492=CARTESIAN_POINT('Ctrl Pts',(17.8935998508933,21.629124808479,13.1241980256187));
#141493=CARTESIAN_POINT('Ctrl Pts',(17.9743583618844,21.6571917901503,13.1284516035042));
#141494=CARTESIAN_POINT('Ctrl Pts',(18.0566163014189,21.6812406201864,13.1327051813896));
#141495=CARTESIAN_POINT('Ctrl Pts',(18.1399366350501,21.701118213745,13.136958759275));
#141496=CARTESIAN_POINT('Ctrl Pts',(18.2216416414276,21.7206104413645,13.141129873253));
#141497=CARTESIAN_POINT('Ctrl Pts',(18.3043677482543,21.7360916126581,13.1453009872309));
#141498=CARTESIAN_POINT('Ctrl Pts',(18.3876870934184,21.7474674984582,13.1494721012089));
#141499=CARTESIAN_POINT('Ctrl Pts',(18.4709784799716,21.75883956697,13.1536418155293));
#141500=CARTESIAN_POINT('Ctrl Pts',(18.5548622540875,21.76610902368,13.1578115298496));
#141501=CARTESIAN_POINT('Ctrl Pts',(18.6389020976073,21.7692330599381,13.16198124417));
#141502=CARTESIAN_POINT('Ctrl Pts',(18.7229389506288,21.7723569850297,13.1661508101141));
#141503=CARTESIAN_POINT('Ctrl Pts',(18.8071314022652,21.7713357667235,13.1703203760581));
#141504=CARTESIAN_POINT('Ctrl Pts',(18.8910411442612,21.7661786784898,13.1744899420021));
#141505=CARTESIAN_POINT('Ctrl Pts',(18.9779010492718,21.7608402733959,13.1788061047411));
#141506=CARTESIAN_POINT('Ctrl Pts',(19.0644574681807,21.7510697851064,13.18312226748));
#141507=CARTESIAN_POINT('Ctrl Pts',(19.1502297723789,21.7369360198915,13.1874384302189));
#141508=CARTESIAN_POINT('Ctrl Pts',(19.2332080527895,21.7232626605919,13.1916139944106));
#141509=CARTESIAN_POINT('Ctrl Pts',(19.3154520685912,21.7055060719794,13.1957895586023));
#141510=CARTESIAN_POINT('Ctrl Pts',(19.3965387044155,21.6837803107335,13.1999651227939));
#141511=CARTESIAN_POINT('Ctrl Pts',(19.48172083345,21.6609572329353,13.2043515848065));
#141512=CARTESIAN_POINT('Ctrl Pts',(19.5656250358875,21.6337536591884,13.208738046819));
#141513=CARTESIAN_POINT('Ctrl Pts',(19.6477828618952,21.6023596302745,13.2131245088315));
#141514=CARTESIAN_POINT('Ctrl Pts',(19.7299406879028,21.5709656013606,13.2175109708441));
#141515=CARTESIAN_POINT('Ctrl Pts',(19.8103516376766,21.5353814216376,13.2218974328566));
#141516=CARTESIAN_POINT('Ctrl Pts',(19.8885775886019,21.4958524223455,13.2262838948691));
#141517=CARTESIAN_POINT('Ctrl Pts',(19.9632042475665,21.4581422109069,13.2304685292622));
#141518=CARTESIAN_POINT('Ctrl Pts',(20.0361203339113,21.4167018520732,13.2346531636552));
#141519=CARTESIAN_POINT('Ctrl Pts',(20.1069282654731,21.3717100633507,13.2388377980483));
#141520=CARTESIAN_POINT('Ctrl Pts',(20.1776354107087,21.3267823148705,13.2430164761322));
#141521=CARTESIAN_POINT('Ctrl Pts',(20.2462399765313,21.278313421969,13.2471951542162));
#141522=CARTESIAN_POINT('Ctrl Pts',(20.3123676261203,21.2265286246579,13.2513738323001));
#141523=CARTESIAN_POINT('Ctrl Pts',(20.379680566303,21.1738156220721,13.2556274101856));
#141524=CARTESIAN_POINT('Ctrl Pts',(20.4444264890784,21.1176668881011,13.259880988071));
#141525=CARTESIAN_POINT('Ctrl Pts',(20.5062401158633,21.0583670376308,13.2641345659564));
#141526=CARTESIAN_POINT('Ctrl Pts',(20.5668553648736,21.000216830476,13.2683056799344));
#141527=CARTESIAN_POINT('Ctrl Pts',(20.6246506525837,20.9390369307226,13.2724767939123));
#141528=CARTESIAN_POINT('Ctrl Pts',(20.6793151535296,20.8751360982348,13.2766479078903));
#141529=CARTESIAN_POINT('Ctrl Pts',(20.7339613112743,20.8112567082884,13.2808176222106));
#141530=CARTESIAN_POINT('Ctrl Pts',(20.7854784698982,20.744658548193,13.284987336531));
#141531=CARTESIAN_POINT('Ctrl Pts',(20.8335944633575,20.6756853209609,13.2891570508514));
#141532=CARTESIAN_POINT('Ctrl Pts',(20.8817087446433,20.6067145480924,13.2933266167954));
#141533=CARTESIAN_POINT('Ctrl Pts',(20.9264218388937,20.5353692539103,13.2974961827395));
#141534=CARTESIAN_POINT('Ctrl Pts',(20.9675042956844,20.4620230058473,13.3016657486835));
#141535=CARTESIAN_POINT('Ctrl Pts',(21.0100311609753,20.3860979941847,13.3059819114224));
#141536=CARTESIAN_POINT('Ctrl Pts',(21.0486670744203,20.3080291637333,13.3102980741614));
#141537=CARTESIAN_POINT('Ctrl Pts',(21.0832097360536,20.2282578906212,13.3146142369003));
#141538=CARTESIAN_POINT('Ctrl Pts',(21.1166271741174,20.1510851583403,13.318789801092));
#141539=CARTESIAN_POINT('Ctrl Pts',(21.1462138190076,20.0723196518132,13.3229653652836));
#141540=CARTESIAN_POINT('Ctrl Pts',(21.1718365500182,19.9923788808226,13.3271409294753));
#141541=CARTESIAN_POINT('Ctrl Pts',(21.1987534242598,19.9084004915303,13.3315273914879));
#141542=CARTESIAN_POINT('Ctrl Pts',(21.221295277208,19.8231255568953,13.3359138535004));
#141543=CARTESIAN_POINT('Ctrl Pts',(21.2393683400758,19.7370508345643,13.340300315513));
#141544=CARTESIAN_POINT('Ctrl Pts',(21.2574414029436,19.6509761122332,13.3446867775255));
#141545=CARTESIAN_POINT('Ctrl Pts',(21.2710456611134,19.5641021872051,13.349073239538));
#141546=CARTESIAN_POINT('Ctrl Pts',(21.2801502518719,19.4769302444118,13.3534597015506));
#141547=CARTESIAN_POINT('Ctrl Pts',(21.2888359269133,19.3937692119263,13.3576443359436));
#141548=CARTESIAN_POINT('Ctrl Pts',(21.2934592377886,19.3100274422731,13.3618289703367));
#141549=CARTESIAN_POINT('Ctrl Pts',(21.2939552539536,19.2261359755289,13.3660136047297));
#141550=CARTESIAN_POINT('Ctrl Pts',(21.294450564101,19.1423639179039,13.3701922828137));
#141551=CARTESIAN_POINT('Ctrl Pts',(21.2908302458307,19.0584430425126,13.3743709608976));
#141552=CARTESIAN_POINT('Ctrl Pts',(21.2830810689264,18.9748100255276,13.3785496389816));
#141553=CARTESIAN_POINT('Ctrl Pts',(21.2751929935952,18.8896779468192,13.382803216867));
#141554=CARTESIAN_POINT('Ctrl Pts',(21.2630265340501,18.804844627276,13.3870567947524));
#141555=CARTESIAN_POINT('Ctrl Pts',(21.2466232879999,18.7207712650195,13.3913103726379));
#141556=CARTESIAN_POINT('Ctrl Pts',(21.2305380508827,18.6383278289459,13.3954814866158));
#141557=CARTESIAN_POINT('Ctrl Pts',(21.2103789301822,18.5566156189164,13.3996526005938));
#141558=CARTESIAN_POINT('Ctrl Pts',(21.1862373001536,18.4760631158151,13.4038237145717));
#141559=CARTESIAN_POINT('Ctrl Pts',(21.1621037710821,18.3955376428842,13.4079934288921));
#141560=CARTESIAN_POINT('Ctrl Pts',(21.1339905186921,18.3161715443229,13.4121631432125));
#141561=CARTESIAN_POINT('Ctrl Pts',(21.1020392245073,18.2383797086247,13.4163328575329));
#141562=CARTESIAN_POINT('Ctrl Pts',(21.0700890672866,18.1605906410939,13.4205024234769));
#141563=CARTESIAN_POINT('Ctrl Pts',(21.0343013153839,18.0843761502596,13.4246719894209));
#141564=CARTESIAN_POINT('Ctrl Pts',(20.9948658827287,18.0101313725834,13.428841555365));
#141565=CARTESIAN_POINT('Ctrl Pts',(20.9540439489102,17.933276240115,13.4331577181039));
#141566=CARTESIAN_POINT('Ctrl Pts',(20.9093133043206,17.8585323739429,13.4374738808428));
#141567=CARTESIAN_POINT('Ctrl Pts',(20.8609355752997,17.7863087848504,13.4417900435817));
#141568=CARTESIAN_POINT('Ctrl Pts',(20.8141337457132,17.7164378715759,13.4459656077734));
#141569=CARTESIAN_POINT('Ctrl Pts',(20.7639191093595,17.6489259106341,13.4501411719651));
#141570=CARTESIAN_POINT('Ctrl Pts',(20.7105706701801,17.5841108255988,13.4543167361568));
#141571=CARTESIAN_POINT('Ctrl Pts',(20.6545277281616,17.5160220847016,13.4587031981693));
#141572=CARTESIAN_POINT('Ctrl Pts',(20.5950264806455,17.450910248947,13.4630896601819));
#141573=CARTESIAN_POINT('Ctrl Pts',(20.5324338669329,17.3891230485379,13.4674761221944));
#141574=CARTESIAN_POINT('Ctrl Pts',(20.4698412532203,17.3273358481288,13.4718625842069));
#141575=CARTESIAN_POINT('Ctrl Pts',(20.4041577572906,17.2688736120053,13.4762490462195));
#141576=CARTESIAN_POINT('Ctrl Pts',(20.3357880909559,17.2140335727229,13.480635508232));
#141577=CARTESIAN_POINT('Ctrl Pts',(20.3218259507328,17.20283439099,13.4815312914205));
#141578=CARTESIAN_POINT('Ctrl Pts',(20.3077408086975,17.1917771969645,13.4824270746089));
#141579=CARTESIAN_POINT('Ctrl Pts',(20.2935357313021,17.1808649545432,13.4833228577973));
#141580=CARTESIAN_POINT('Origin',(18.734,19.211,-1.76670989022852));
#141581=CARTESIAN_POINT('',(20.2947698000194,17.1792870601113,14.3497865242445));
#141582=CARTESIAN_POINT('',(20.2923704939389,17.1824127799558,14.2834124336844));
#141583=CARTESIAN_POINT('',(20.2935357313021,17.1808649545432,-1.76670989022852));
#141584=CARTESIAN_POINT('',(16.1740010575059,19.2133268925441,13.8332901097715));
#141585=CARTESIAN_POINT('Ctrl Pts',(16.1735504167883,19.2133273021507,13.8332901097715));
#141586=CARTESIAN_POINT('Ctrl Pts',(16.1718448984259,19.397218647613,13.8424428639771));
#141587=CARTESIAN_POINT('Ctrl Pts',(16.2739023704358,20.430943821993,13.8939875537431));
#141588=CARTESIAN_POINT('Ctrl Pts',(17.6781137250704,22.0479692933859,13.9879241790696));
#141589=CARTESIAN_POINT('Ctrl Pts',(20.547911001461,21.6344309307215,14.1150999857511));
#141590=CARTESIAN_POINT('Ctrl Pts',(21.6914148573177,19.1334581591447,14.235720767476));
#141591=CARTESIAN_POINT('Ctrl Pts',(20.8607340381188,17.6225946302628,14.3139496136405));
#141592=CARTESIAN_POINT('Ctrl Pts',(20.2947698000194,17.1792870601114,14.3497865242445));
#141593=CARTESIAN_POINT('Ctrl Pts',(20.2935357313021,17.1808649545431,13.5498657053664));
#141594=CARTESIAN_POINT('Ctrl Pts',(20.2268456363114,17.1296340838212,13.554035809073));
#141595=CARTESIAN_POINT('Ctrl Pts',(20.1576422952453,17.0817034154883,13.5582059127796));
#141596=CARTESIAN_POINT('Ctrl Pts',(20.0862913115335,17.0373146021673,13.5623760164862));
#141597=CARTESIAN_POINT('Ctrl Pts',(20.014862512693,16.9928773785647,13.566550668093));
#141598=CARTESIAN_POINT('Ctrl Pts',(19.9412817874356,16.9519899633664,13.5707253196998));
#141599=CARTESIAN_POINT('Ctrl Pts',(19.8659411499047,16.914849039555,13.5748999713067));
#141600=CARTESIAN_POINT('Ctrl Pts',(19.7905547067899,16.8776855348131,13.5790771610172));
#141601=CARTESIAN_POINT('Ctrl Pts',(19.7134066434974,16.8442732382304,13.5832543507278));
#141602=CARTESIAN_POINT('Ctrl Pts',(19.6349086321998,16.8147605218952,13.5874315404384));
#141603=CARTESIAN_POINT('Ctrl Pts',(19.5562800602382,16.7851987189682,13.5916156777984));
#141604=CARTESIAN_POINT('Ctrl Pts',(19.47629749576,16.7595495841754,13.5957998151583));
#141605=CARTESIAN_POINT('Ctrl Pts',(19.3953870345571,16.7379114066577,13.5999839525183));
#141606=CARTESIAN_POINT('Ctrl Pts',(19.3540513033222,16.7268568424273,13.6021215546873));
#141607=CARTESIAN_POINT('Ctrl Pts',(19.3124735468993,16.7168483144191,13.6042591568563));
#141608=CARTESIAN_POINT('Ctrl Pts',(19.2707112385803,16.7078937205181,13.6063967590253));
#141609=CARTESIAN_POINT('Ctrl Pts',(19.1889560858867,16.6903639377749,13.6105813934184));
#141610=CARTESIAN_POINT('Ctrl Pts',(19.1061890642126,16.676811111084,13.6147660278114));
#141611=CARTESIAN_POINT('Ctrl Pts',(19.0228317972389,16.6673458975514,13.6189506622045));
#141612=CARTESIAN_POINT('Ctrl Pts',(18.9395931790174,16.6578941565786,13.6231293402884));
#141613=CARTESIAN_POINT('Ctrl Pts',(18.8557664374668,16.6525185234246,13.6273080183724));
#141614=CARTESIAN_POINT('Ctrl Pts',(18.771784329296,16.6512788541602,13.6314866964563));
#141615=CARTESIAN_POINT('Ctrl Pts',(18.6862969021931,16.6500169647151,13.6357402743417));
#141616=CARTESIAN_POINT('Ctrl Pts',(18.6006489552155,16.6530408729659,13.6399938522272));
#141617=CARTESIAN_POINT('Ctrl Pts',(18.5153034901262,16.6603585440974,13.6442474301126));
#141618=CARTESIAN_POINT('Ctrl Pts',(18.4316126134156,16.6675343478947,13.6484185440906));
#141619=CARTESIAN_POINT('Ctrl Pts',(18.3482130743119,16.6788388732104,13.6525896580685));
#141620=CARTESIAN_POINT('Ctrl Pts',(18.2655406685,16.6942270951215,13.6567607720465));
#141621=CARTESIAN_POINT('Ctrl Pts',(18.1828960042123,16.7096101533661,13.6609304863668));
#141622=CARTESIAN_POINT('Ctrl Pts',(18.1009784405238,16.7290741026091,13.6651002006872));
#141623=CARTESIAN_POINT('Ctrl Pts',(18.0202156389589,16.7525224455096,13.6692699150076));
#141624=CARTESIAN_POINT('Ctrl Pts',(17.9394557112813,16.7759699540174,13.6734394809516));
#141625=CARTESIAN_POINT('Ctrl Pts',(17.8598509055788,16.8034014451983,13.6776090468957));
#141626=CARTESIAN_POINT('Ctrl Pts',(17.7818144029991,16.8346703534939,13.6817786128397));
#141627=CARTESIAN_POINT('Ctrl Pts',(17.7010342332569,16.8670386380308,13.6860947755786));
#141628=CARTESIAN_POINT('Ctrl Pts',(17.6219351912177,16.9035190114424,13.6904109383175));
#141629=CARTESIAN_POINT('Ctrl Pts',(17.54495192229,16.9438950908936,13.6947271010565));
#141630=CARTESIAN_POINT('Ctrl Pts',(17.4704763752505,16.9829559238035,13.6989026652482));
#141631=CARTESIAN_POINT('Ctrl Pts',(17.3979812574156,17.0256622753739,13.7030782294398));
#141632=CARTESIAN_POINT('Ctrl Pts',(17.3278323932019,17.0717728821858,13.7072537936315));
#141633=CARTESIAN_POINT('Ctrl Pts',(17.25414047662,17.1202124261302,13.7116402556441));
#141634=CARTESIAN_POINT('Ctrl Pts',(17.1830385318337,17.1724088154588,13.7160267176566));
#141635=CARTESIAN_POINT('Ctrl Pts',(17.1149115381733,17.2280344045396,13.7204131796692));
#141636=CARTESIAN_POINT('Ctrl Pts',(17.046784544513,17.2836599936204,13.7247996416817));
#141637=CARTESIAN_POINT('Ctrl Pts',(16.9816328807926,17.3427143364292,13.7291861036942));
#141638=CARTESIAN_POINT('Ctrl Pts',(16.919795358022,17.4048268308312,13.7335725657068));
#141639=CARTESIAN_POINT('Ctrl Pts',(16.8612222805614,17.4636603639818,13.7377274633762));
#141640=CARTESIAN_POINT('Ctrl Pts',(16.8053896617353,17.5254713783546,13.7418823610455));
#141641=CARTESIAN_POINT('Ctrl Pts',(16.7526212754374,17.5899699725635,13.7460372587149));
#141642=CARTESIAN_POINT('Ctrl Pts',(16.70029462084,17.6539286398257,13.7501573751423));
#141643=CARTESIAN_POINT('Ctrl Pts',(16.650981430094,17.7205297194408,13.7542774915697));
#141644=CARTESIAN_POINT('Ctrl Pts',(16.6049624110077,17.7894519196813,13.7583976079971));
#141645=CARTESIAN_POINT('Ctrl Pts',(16.5589874739682,17.8583080987046,13.7625137777266));
#141646=CARTESIAN_POINT('Ctrl Pts',(16.5163007099123,17.9294805955777,13.7666299474561));
#141647=CARTESIAN_POINT('Ctrl Pts',(16.4771421768206,18.0026156381539,13.7707461171856));
#141648=CARTESIAN_POINT('Ctrl Pts',(16.4380086398887,18.0757039962642,13.7748596594307));
#141649=CARTESIAN_POINT('Ctrl Pts',(16.4023990866292,18.1507519968567,13.7789732016757));
#141650=CARTESIAN_POINT('Ctrl Pts',(16.3705090605921,18.2273788435904,13.7830867439208));
#141651=CARTESIAN_POINT('Ctrl Pts',(16.3380758082444,18.3053109799212,13.7872703577417));
#141652=CARTESIAN_POINT('Ctrl Pts',(16.3094902338593,18.384875816755,13.7914539715626));
#141653=CARTESIAN_POINT('Ctrl Pts',(16.2849076425234,18.4656499986249,13.7956375853835));
#141654=CARTESIAN_POINT('Ctrl Pts',(16.260736137924,18.5450734199358,13.7997512379815));
#141655=CARTESIAN_POINT('Ctrl Pts',(16.2404348481342,18.625665568199,13.8038648905794));
#141656=CARTESIAN_POINT('Ctrl Pts',(16.2241009663663,18.7070090864265,13.8079785431774));
#141657=CARTESIAN_POINT('Ctrl Pts',(16.2073503971231,18.7904277283583,13.8121971376098));
#141658=CARTESIAN_POINT('Ctrl Pts',(16.1947725425285,18.8746360871018,13.8164157320421));
#141659=CARTESIAN_POINT('Ctrl Pts',(16.1864159534739,18.9591756050623,13.8206343264745));
#141660=CARTESIAN_POINT('Ctrl Pts',(16.1780593644194,19.0437151230227,13.8248529209068));
#141661=CARTESIAN_POINT('Ctrl Pts',(16.1739240322153,19.1285852645551,13.8290715153392));
#141662=CARTESIAN_POINT('Ctrl Pts',(16.1740010575059,19.2133268925441,13.8332901097715));
#141663=CARTESIAN_POINT('',(16.1740010826188,19.2086456408846,13.7667098774927));
#141664=CARTESIAN_POINT('Ctrl Pts',(20.2935357313021,17.1808649545432,13.4833228577973));
#141665=CARTESIAN_POINT('Ctrl Pts',(20.2271990472176,17.1299055716403,13.4875061005018));
#141666=CARTESIAN_POINT('Ctrl Pts',(20.1582439195132,17.0821103150656,13.4916893432062));
#141667=CARTESIAN_POINT('Ctrl Pts',(20.0870050548683,17.037758798131,13.4958725859106));
#141668=CARTESIAN_POINT('Ctrl Pts',(20.0158625393595,16.9934672657339,13.5000501708631));
#141669=CARTESIAN_POINT('Ctrl Pts',(19.9424428099246,16.952610462243,13.5042277558156));
#141670=CARTESIAN_POINT('Ctrl Pts',(19.8671122176929,16.9154267160217,13.5084053407681));
#141671=CARTESIAN_POINT('Ctrl Pts',(19.7918615726562,16.8782824323364,13.5125784921142));
#141672=CARTESIAN_POINT('Ctrl Pts',(19.7147045060799,16.8448036608316,13.5167516434603));
#141673=CARTESIAN_POINT('Ctrl Pts',(19.6360336298753,16.8151837861443,13.5209247948064));
#141674=CARTESIAN_POINT('Ctrl Pts',(19.5574081539594,16.7855810048329,13.5250955378626));
#141675=CARTESIAN_POINT('Ctrl Pts',(19.4772710323891,16.7598328607242,13.5292662809187));
#141676=CARTESIAN_POINT('Ctrl Pts',(19.3960355713781,16.7380849383309,13.5334370239749));
#141677=CARTESIAN_POINT('Ctrl Pts',(19.3148226216747,16.7163430425441,13.5376066112689));
#141678=CARTESIAN_POINT('Ctrl Pts',(19.2325123812022,16.6985992855769,13.5417761985628));
#141679=CARTESIAN_POINT('Ctrl Pts',(19.1495327464081,16.6849492212819,13.5459457858567));
#141680=CARTESIAN_POINT('Ctrl Pts',(19.0665512144905,16.671298844912,13.5501154684779));
#141681=CARTESIAN_POINT('Ctrl Pts',(18.9829007120166,16.6617424204531,13.5542851510991));
#141682=CARTESIAN_POINT('Ctrl Pts',(18.8990173854919,16.6563240396314,13.5584548337203));
#141683=CARTESIAN_POINT('Ctrl Pts',(18.81504898099,16.6509001632612,13.562628745408));
#141684=CARTESIAN_POINT('Ctrl Pts',(18.7308477408885,16.6496227436427,13.5668026570956));
#141685=CARTESIAN_POINT('Ctrl Pts',(18.6468524989643,16.6524837672856,13.5709765687833));
#141686=CARTESIAN_POINT('Ctrl Pts',(18.5628158254364,16.6553462021608,13.5751525393001));
#141687=CARTESIAN_POINT('Ctrl Pts',(18.4789858114393,16.6623511081852,13.5793285098169));
#141688=CARTESIAN_POINT('Ctrl Pts',(18.395796391128,16.6734385093271,13.5835044803338));
#141689=CARTESIAN_POINT('Ctrl Pts',(18.3124575762843,16.68454582162,13.5876879502076));
#141690=CARTESIAN_POINT('Ctrl Pts',(18.2297621072741,16.6997501950311,13.5918714200815));
#141691=CARTESIAN_POINT('Ctrl Pts',(18.1481338641761,16.7189404359256,13.5960548899553));
#141692=CARTESIAN_POINT('Ctrl Pts',(18.0716697213006,16.7369166322258,13.5999736982747));
#141693=CARTESIAN_POINT('Ctrl Pts',(17.9961422105312,16.7583897434859,13.6038925065941));
#141694=CARTESIAN_POINT('Ctrl Pts',(17.921884774769,16.783229652346,13.6078113149135));
#141695=CARTESIAN_POINT('Ctrl Pts',(17.842590205016,16.809754536562,13.6119959493065));
#141696=CARTESIAN_POINT('Ctrl Pts',(17.7644489508447,16.8402176845382,13.6161805836996));
#141697=CARTESIAN_POINT('Ctrl Pts',(17.6878802554244,16.8744997367838,13.6203652180926));
#141698=CARTESIAN_POINT('Ctrl Pts',(17.6114205460648,16.9087329927714,13.6245438961766));
#141699=CARTESIAN_POINT('Ctrl Pts',(17.5365293656819,16.9467741695629,13.6287225742605));
#141700=CARTESIAN_POINT('Ctrl Pts',(17.4636096823066,16.9884545132415,13.6329012523445));
#141701=CARTESIAN_POINT('Ctrl Pts',(17.3893829660133,17.0308819471252,13.6371548302299));
#141702=CARTESIAN_POINT('Ctrl Pts',(17.3171995773181,17.0770801423178,13.6414084081153));
#141703=CARTESIAN_POINT('Ctrl Pts',(17.2474621052951,17.126820284235,13.6456619860008));
#141704=CARTESIAN_POINT('Ctrl Pts',(17.1790766302487,17.1755961164412,13.6498330999787));
#141705=CARTESIAN_POINT('Ctrl Pts',(17.1130434722311,17.2277775063953,13.6540042139567));
#141706=CARTESIAN_POINT('Ctrl Pts',(17.0497148300456,17.2831038756531,13.6581753279346));
#141707=CARTESIAN_POINT('Ctrl Pts',(16.9864074383976,17.3384116796135,13.662345042255));
#141708=CARTESIAN_POINT('Ctrl Pts',(16.9258031063752,17.3968620645643,13.6665147565754));
#141709=CARTESIAN_POINT('Ctrl Pts',(16.8682208314236,17.4581542868505,13.6706844708957));
#141710=CARTESIAN_POINT('Ctrl Pts',(16.8106406054966,17.5194443280964,13.6748540368398));
#141711=CARTESIAN_POINT('Ctrl Pts',(16.7560825371937,17.5835756697509,13.6790236027838));
#141712=CARTESIAN_POINT('Ctrl Pts',(16.7048276747609,17.650211841894,13.6831931687278));
#141713=CARTESIAN_POINT('Ctrl Pts',(16.6517707545947,17.7191908596451,13.6875093314668));
#141714=CARTESIAN_POINT('Ctrl Pts',(16.6022539651132,17.7908537067502,13.6918254942057));
#141715=CARTESIAN_POINT('Ctrl Pts',(16.5565412927829,17.8647928917271,13.6961416569446));
#141716=CARTESIAN_POINT('Ctrl Pts',(16.5123177059456,17.9363235155305,13.7003172211363));
#141717=CARTESIAN_POINT('Ctrl Pts',(16.4716543903427,18.0099840160617,13.704492785328));
#141718=CARTESIAN_POINT('Ctrl Pts',(16.4347434295141,18.0853805158593,13.7086683495197));
#141719=CARTESIAN_POINT('Ctrl Pts',(16.3959681838015,18.1645851136235,13.7130548115322));
#141720=CARTESIAN_POINT('Ctrl Pts',(16.3613345469612,18.2457051531361,13.7174412735447));
#141721=CARTESIAN_POINT('Ctrl Pts',(16.3310071212994,18.3282626523624,13.7218277355573));
#141722=CARTESIAN_POINT('Ctrl Pts',(16.3006796956376,18.4108201515888,13.7262141975698));
#141723=CARTESIAN_POINT('Ctrl Pts',(16.2746585801944,18.494814533789,13.7306006595824));
#141724=CARTESIAN_POINT('Ctrl Pts',(16.253046772176,18.5797543415202,13.7349871215949));
#141725=CARTESIAN_POINT('Ctrl Pts',(16.2263033450825,18.6848626949471,13.7404151277539));
#141726=CARTESIAN_POINT('Ctrl Pts',(16.2062281520531,18.7917315462651,13.7458431339129));
#141727=CARTESIAN_POINT('Ctrl Pts',(16.1930065418683,18.8996284442475,13.7512711400719));
#141728=CARTESIAN_POINT('Ctrl Pts',(16.180471247327,19.0019245622985,13.7564173858788));
#141729=CARTESIAN_POINT('Ctrl Pts',(16.1740962693074,19.1051449394228,13.7615636316857));
#141730=CARTESIAN_POINT('Ctrl Pts',(16.1740010826188,19.2086456408846,13.7667098774927));
#141731=CARTESIAN_POINT('Ctrl Pts',(16.1744182524956,19.2086462806443,13.7667098902285));
#141732=CARTESIAN_POINT('Ctrl Pts',(16.1802301046829,19.8484613837252,13.7985275695778));
#141733=CARTESIAN_POINT('Ctrl Pts',(16.7471749375075,21.3499116609599,13.8727371844876));
#141734=CARTESIAN_POINT('Ctrl Pts',(19.2691669576991,22.1904107317588,13.9893387349578));
#141735=CARTESIAN_POINT('Ctrl Pts',(21.528888647397,20.3737078006893,14.1165145416392));
#141736=CARTESIAN_POINT('Ctrl Pts',(21.294251524494,18.1512291001575,14.2145391078814));
#141737=CARTESIAN_POINT('Ctrl Pts',(20.5052428603892,17.3430212386448,14.2701717385632));
#141738=CARTESIAN_POINT('Ctrl Pts',(20.2923704939387,17.1824127799556,14.2834124336845));
#141739=CARTESIAN_POINT('Origin',(18.734,19.211,-1.76670989022852));
#141740=CARTESIAN_POINT('',(20.2935357313021,17.1808649545431,15.149955387129));
#141741=CARTESIAN_POINT('',(20.2935357313021,17.1808649545432,15.0832685864905));
#141742=CARTESIAN_POINT('',(20.2935357313021,17.1808649545432,-1.76670989022852));
#141743=CARTESIAN_POINT('',(16.1738766799073,19.2098698167329,14.6332901097715));
#141744=CARTESIAN_POINT('Ctrl Pts',(16.1740002494514,19.2098698712835,14.6332901097715));
#141745=CARTESIAN_POINT('Ctrl Pts',(16.1739637014967,19.2926593390013,14.6374299052976));
#141746=CARTESIAN_POINT('Ctrl Pts',(16.1779474618949,19.3756125071059,14.6415697008237));
#141747=CARTESIAN_POINT('Ctrl Pts',(16.1859729132155,19.4583013647604,14.6457094963498));
#141748=CARTESIAN_POINT('Ctrl Pts',(16.1939875490477,19.5408787868903,14.6498437128862));
#141749=CARTESIAN_POINT('Ctrl Pts',(16.2060330170348,19.6231921412973,14.6539779294227));
#141750=CARTESIAN_POINT('Ctrl Pts',(16.2220786798975,19.7048130026784,14.6581121459591));
#141751=CARTESIAN_POINT('Ctrl Pts',(16.2381078732804,19.7863500873324,14.6622421190812));
#141752=CARTESIAN_POINT('Ctrl Pts',(16.2581290152452,19.8671956313601,14.6663720922033));
#141753=CARTESIAN_POINT('Ctrl Pts',(16.2820597821147,19.9469274202778,14.6705020653254));
#141754=CARTESIAN_POINT('Ctrl Pts',(16.3059775967094,20.0266160552067,14.6746298031431));
#141755=CARTESIAN_POINT('Ctrl Pts',(16.3338007023326,20.1051916814476,14.6787575409609));
#141756=CARTESIAN_POINT('Ctrl Pts',(16.3653962152437,20.1822446194642,14.6828852787787));
#141757=CARTESIAN_POINT('Ctrl Pts',(16.3969845852851,20.2592801379472,14.6870120834293));
#141758=CARTESIAN_POINT('Ctrl Pts',(16.4323434905921,20.3347932165774,14.69113888808));
#141759=CARTESIAN_POINT('Ctrl Pts',(16.4712914723381,20.4083930511099,14.6952656927307));
#141760=CARTESIAN_POINT('Ctrl Pts',(16.5102429241535,20.4819994430175,14.6993928650588));
#141761=CARTESIAN_POINT('Ctrl Pts',(16.5527838651363,20.5536918375771,14.703520037387));
#141762=CARTESIAN_POINT('Ctrl Pts',(16.5986870593961,20.6231043324377,14.7076472097152));
#141763=CARTESIAN_POINT('Ctrl Pts',(16.6446377721104,20.6925886823084,14.7117786544444));
#141764=CARTESIAN_POINT('Ctrl Pts',(16.6939574240325,20.7597880294055,14.7159100991735));
#141765=CARTESIAN_POINT('Ctrl Pts',(16.7463760416131,20.8243663564257,14.7200415439027));
#141766=CARTESIAN_POINT('Ctrl Pts',(16.7988250781885,20.8889821588294,14.7241753861463));
#141767=CARTESIAN_POINT('Ctrl Pts',(16.8543763437708,20.9509735655353,14.7283092283899));
#141768=CARTESIAN_POINT('Ctrl Pts',(16.9127219511763,21.0100403744422,14.7324430706336));
#141769=CARTESIAN_POINT('Ctrl Pts',(16.9711635405887,21.0692043517755,14.7365837132945));
#141770=CARTESIAN_POINT('Ctrl Pts',(17.0324082986529,21.1254338132414,14.7407243559553));
#141771=CARTESIAN_POINT('Ctrl Pts',(17.0961145829399,21.1784682616454,14.7448649986162));
#141772=CARTESIAN_POINT('Ctrl Pts',(17.1274705472745,21.2045715933853,14.7469030054636));
#141773=CARTESIAN_POINT('Ctrl Pts',(17.1594223751536,21.2299015689542,14.7489410123109));
#141774=CARTESIAN_POINT('Ctrl Pts',(17.1919269101815,21.2544310817,14.7509790191583));
#141775=CARTESIAN_POINT('Ctrl Pts',(17.2586683911457,21.3047974692387,14.7551636535514));
#141776=CARTESIAN_POINT('Ctrl Pts',(17.3280042311,21.3519843348469,14.7593482879444));
#141777=CARTESIAN_POINT('Ctrl Pts',(17.3995987737075,21.395713566413,14.7635329223375));
#141778=CARTESIAN_POINT('Ctrl Pts',(17.4710914103449,21.4393805548304,14.7677116004214));
#141779=CARTESIAN_POINT('Ctrl Pts',(17.5448359744303,21.4795994471399,14.7718902785053));
#141780=CARTESIAN_POINT('Ctrl Pts',(17.6204652949927,21.5161335017183,14.7760689565893));
#141781=CARTESIAN_POINT('Ctrl Pts',(17.6974502167725,21.5533224029686,14.7803225344747));
#141782=CARTESIAN_POINT('Ctrl Pts',(17.7763877432988,21.5866927752842,14.7845761123601));
#141783=CARTESIAN_POINT('Ctrl Pts',(17.8568613993343,21.616042177431,14.7888296902455));
#141784=CARTESIAN_POINT('Ctrl Pts',(17.9357749165162,21.6448225841466,14.7930008042235));
#141785=CARTESIAN_POINT('Ctrl Pts',(18.0161650808992,21.6697363732161,14.7971719182015));
#141786=CARTESIAN_POINT('Ctrl Pts',(18.0976177441658,21.6906406240541,14.8013430321794));
#141787=CARTESIAN_POINT('Ctrl Pts',(18.1790430752045,21.7115378602688,14.8055127464998));
#141788=CARTESIAN_POINT('Ctrl Pts',(18.2615297518276,21.7284281160528,14.8096824608201));
#141789=CARTESIAN_POINT('Ctrl Pts',(18.34464929881,21.7412185738554,14.8138521751405));
#141790=CARTESIAN_POINT('Ctrl Pts',(18.4277658880425,21.7540085765186,14.8180217410846));
#141791=CARTESIAN_POINT('Ctrl Pts',(18.5115148480474,21.7626990021399,14.8221913070286));
#141792=CARTESIAN_POINT('Ctrl Pts',(18.5954597232798,21.7672485387235,14.8263608729727));
#141793=CARTESIAN_POINT('Ctrl Pts',(18.682355996768,21.7719580314011,14.8306770357116));
#141794=CARTESIAN_POINT('Ctrl Pts',(18.7694616919209,21.7722300013651,14.8349931984505));
#141795=CARTESIAN_POINT('Ctrl Pts',(18.8562914526108,21.7680773943349,14.8393093611894));
#141796=CARTESIAN_POINT('Ctrl Pts',(18.9402927429791,21.7640600580418,14.8434849253811));
#141797=CARTESIAN_POINT('Ctrl Pts',(19.0240353356991,21.7559020718403,14.8476604895728));
#141798=CARTESIAN_POINT('Ctrl Pts',(19.1070857885135,21.7436679597628,14.8518360537644));
#141799=CARTESIAN_POINT('Ctrl Pts',(19.1943309222658,21.7308159317682,14.856222515777));
#141800=CARTESIAN_POINT('Ctrl Pts',(19.2808115861344,21.7134653009972,14.8606089777895));
#141801=CARTESIAN_POINT('Ctrl Pts',(19.3660405469232,21.6917508434031,14.864995439802));
#141802=CARTESIAN_POINT('Ctrl Pts',(19.4512695077121,21.6700363858089,14.8693819018146));
#141803=CARTESIAN_POINT('Ctrl Pts',(19.5352462338657,21.6439583461085,14.8737683638271));
#141804=CARTESIAN_POINT('Ctrl Pts',(19.6175072439392,21.6137099179691,14.8781548258397));
#141805=CARTESIAN_POINT('Ctrl Pts',(19.6959833029991,21.5848532648472,14.8823394602327));
#141806=CARTESIAN_POINT('Ctrl Pts',(19.7731901646012,21.5520941514644,14.8865240946257));
#141807=CARTESIAN_POINT('Ctrl Pts',(19.8487122960628,21.5155642748698,14.8907087290188));
#141808=CARTESIAN_POINT('Ctrl Pts',(19.924126931118,21.4790863940332,14.8948874071027));
#141809=CARTESIAN_POINT('Ctrl Pts',(19.997861188636,21.4388486095631,14.8990660851867));
#141810=CARTESIAN_POINT('Ctrl Pts',(20.069517263694,21.3950315103897,14.9032447632706));
#141811=CARTESIAN_POINT('Ctrl Pts',(20.1424577223992,21.3504290212044,14.907498341156));
#141812=CARTESIAN_POINT('Ctrl Pts',(20.2132443104809,21.3021178031455,14.9117519190415));
#141813=CARTESIAN_POINT('Ctrl Pts',(20.2814813767513,21.2503384683784,14.9160054969269));
#141814=CARTESIAN_POINT('Ctrl Pts',(20.3483955343384,21.1995629770548,14.9201766109049));
#141815=CARTESIAN_POINT('Ctrl Pts',(20.4128577595137,21.145452932324,14.9243477248828));
#141816=CARTESIAN_POINT('Ctrl Pts',(20.4745237080533,21.0882792071784,14.9285188388608));
#141817=CARTESIAN_POINT('Ctrl Pts',(20.5361689639883,21.0311246672285,14.9326885531811));
#141818=CARTESIAN_POINT('Ctrl Pts',(20.5950194697343,20.9709088010949,14.9368582675015));
#141819=CARTESIAN_POINT('Ctrl Pts',(20.6507652549071,20.9079416482546,14.9410279818219));
#141820=CARTESIAN_POINT('Ctrl Pts',(20.7065090564057,20.8449767360557,14.9451975477659));
#141821=CARTESIAN_POINT('Ctrl Pts',(20.7591480526894,20.7792610768138,14.9493671137099));
#141822=CARTESIAN_POINT('Ctrl Pts',(20.8084112617993,20.711139299172,14.953536679654));
#141823=CARTESIAN_POINT('Ctrl Pts',(20.8594065045688,20.6406224438655,14.9578528423929));
#141824=CARTESIAN_POINT('Ctrl Pts',(20.9067838489647,20.5675275512001,14.9621690051318));
#141825=CARTESIAN_POINT('Ctrl Pts',(20.9502914662215,20.4922697361422,14.9664851678708));
#141826=CARTESIAN_POINT('Ctrl Pts',(20.9923818274223,20.4194634364942,14.9706607320624));
#141827=CARTESIAN_POINT('Ctrl Pts',(21.0308505291915,20.3446334053669,14.9748362962541));
#141828=CARTESIAN_POINT('Ctrl Pts',(21.0655172119567,20.2681790247398,14.9790118604458));
#141829=CARTESIAN_POINT('Ctrl Pts',(21.1019348264562,20.1878631151,14.9833983224583));
#141830=CARTESIAN_POINT('Ctrl Pts',(21.1341560348913,20.1057549952925,14.9877847844709));
#141831=CARTESIAN_POINT('Ctrl Pts',(21.162030432422,20.0223373029958,14.9921712464835));
#141832=CARTESIAN_POINT('Ctrl Pts',(21.1899048299528,19.938919610699,14.996557708496));
#141833=CARTESIAN_POINT('Ctrl Pts',(21.2134323346265,19.8541929253279,15.0009441705086));
#141834=CARTESIAN_POINT('Ctrl Pts',(21.2325245180281,19.7686515334979,15.0053306325211));
#141835=CARTESIAN_POINT('Ctrl Pts',(21.2507382417699,19.6870460279089,15.0095152669142));
#141836=CARTESIAN_POINT('Ctrl Pts',(21.2649836214983,19.6043953888038,15.0136999013072));
#141837=CARTESIAN_POINT('Ctrl Pts',(21.2751464736302,19.5211202985242,15.0178845357003));
#141838=CARTESIAN_POINT('Ctrl Pts',(21.2852948602001,19.4379637400282,15.0220632137842));
#141839=CARTESIAN_POINT('Ctrl Pts',(21.2913722063418,19.3541849485909,15.0262418918681));
#141840=CARTESIAN_POINT('Ctrl Pts',(21.2933150345072,19.2702161645612,15.0304205699521));
#141841=CARTESIAN_POINT('Ctrl Pts',(21.2952926864712,19.1847423004251,15.0346741478375));
#141842=CARTESIAN_POINT('Ctrl Pts',(21.2929860350544,19.0990720360282,15.038927725723));
#141843=CARTESIAN_POINT('Ctrl Pts',(21.2863832385264,19.0136682902081,15.0431813036084));
#141844=CARTESIAN_POINT('Ctrl Pts',(21.2799084500935,18.9299202626523,15.0473524175864));
#141845=CARTESIAN_POINT('Ctrl Pts',(21.2693026454397,18.8464289917135,15.0515235315643));
#141846=CARTESIAN_POINT('Ctrl Pts',(21.2546071988876,18.7636306348037,15.0556946455423));
#141847=CARTESIAN_POINT('Ctrl Pts',(21.2399166835345,18.6808600616823,15.0598643598626));
#141848=CARTESIAN_POINT('Ctrl Pts',(21.2211393320557,18.5987823933904,15.064034074183));
#141849=CARTESIAN_POINT('Ctrl Pts',(21.1983680574965,18.5178260844557,15.0682037885034));
#141850=CARTESIAN_POINT('Ctrl Pts',(21.1755975932369,18.436872656294,15.0723733544475));
#141851=CARTESIAN_POINT('Ctrl Pts',(21.1488336138538,18.3570409507695,15.0765429203915));
#141852=CARTESIAN_POINT('Ctrl Pts',(21.1182192201025,18.2787453617742,15.0807124863355));
#141853=CARTESIAN_POINT('Ctrl Pts',(21.0865284620339,18.1976969964578,15.0850286490745));
#141854=CARTESIAN_POINT('Ctrl Pts',(21.0507116827589,18.1182952684028,15.0893448118134));
#141855=CARTESIAN_POINT('Ctrl Pts',(21.0109816181366,18.0409766196062,15.0936609745523));
#141856=CARTESIAN_POINT('Ctrl Pts',(20.9725457561904,17.9661766176617,15.097836538744));
#141857=CARTESIAN_POINT('Ctrl Pts',(20.9304479207725,17.8933264506923,15.1020121029357));
#141858=CARTESIAN_POINT('Ctrl Pts',(20.8849263037083,17.8227939504469,15.1061876671273));
#141859=CARTESIAN_POINT('Ctrl Pts',(20.8371054979835,17.7486990212892,15.1105741291399));
#141860=CARTESIAN_POINT('Ctrl Pts',(20.7855062921195,17.6771625161641,15.1149605911524));
#141861=CARTESIAN_POINT('Ctrl Pts',(20.7304530967377,17.6085721443614,15.119347053165));
#141862=CARTESIAN_POINT('Ctrl Pts',(20.6753999013559,17.5399817725587,15.1237335151775));
#141863=CARTESIAN_POINT('Ctrl Pts',(20.616893159293,17.474337916614,15.12811997719));
#141864=CARTESIAN_POINT('Ctrl Pts',(20.5553006227462,17.4119824788001,15.1325064392026));
#141865=CARTESIAN_POINT('Ctrl Pts',(20.4965457256996,17.3524998282314,15.1366908118295));
#141866=CARTESIAN_POINT('Ctrl Pts',(20.434764426497,17.2957878690111,15.1408751844563));
#141867=CARTESIAN_POINT('Ctrl Pts',(20.3702485909646,17.2421702591219,15.1450595570832));
#141868=CARTESIAN_POINT('Ctrl Pts',(20.3450868288406,17.2212589040327,15.1466915004318));
#141869=CARTESIAN_POINT('Ctrl Pts',(20.3195095624847,17.2008178724038,15.1483234437804));
#141870=CARTESIAN_POINT('Ctrl Pts',(20.2935357313021,17.1808649545431,15.149955387129));
#141871=CARTESIAN_POINT('Ctrl Pts',(20.2947698000194,17.1792870601114,14.3497865242445));
#141872=CARTESIAN_POINT('Ctrl Pts',(20.1912477708408,17.0982004894008,14.356341549201));
#141873=CARTESIAN_POINT('Ctrl Pts',(19.3719149925772,16.5548827574419,14.405288509718));
#141874=CARTESIAN_POINT('Ctrl Pts',(17.2895133755746,16.5507840333809,14.4966274057954));
#141875=CARTESIAN_POINT('Ctrl Pts',(16.200898327955,18.2345794040693,14.5845735760146));
#141876=CARTESIAN_POINT('Ctrl Pts',(16.1700292343928,19.1465375881033,14.6301278106733));
#141877=CARTESIAN_POINT('Ctrl Pts',(16.1703790132248,19.209868272665,14.6332901097715));
#141878=CARTESIAN_POINT('',(16.17436451349,19.211560173865,14.5667099150528));
#141879=CARTESIAN_POINT('Ctrl Pts',(20.2923704939387,17.1824127799556,14.2834124336845));
#141880=CARTESIAN_POINT('Ctrl Pts',(19.8237022344235,16.8288108162419,14.3125636741237));
#141881=CARTESIAN_POINT('Ctrl Pts',(18.3750627724065,16.3386617668037,14.3841068501234));
#141882=CARTESIAN_POINT('Ctrl Pts',(16.5197423492181,17.430869440195,14.478539335638));
#141883=CARTESIAN_POINT('Ctrl Pts',(16.1790023518676,18.7496082788979,14.5438205807135));
#141884=CARTESIAN_POINT('Ctrl Pts',(16.1781028428963,19.2115588546613,14.5667098902285));
#141885=CARTESIAN_POINT('Ctrl Pts',(16.1740000613162,19.211560302475,14.5667099174729));
#141886=CARTESIAN_POINT('Ctrl Pts',(16.1740197372987,19.30145909156,14.5711571992719));
#141887=CARTESIAN_POINT('Ctrl Pts',(16.1787790795977,19.3912344818004,14.5756044810709));
#141888=CARTESIAN_POINT('Ctrl Pts',(16.1882138900509,19.4803939167657,14.5800517628699));
#141889=CARTESIAN_POINT('Ctrl Pts',(16.1976832329532,19.5698796851174,14.5845153222118));
#141890=CARTESIAN_POINT('Ctrl Pts',(16.2118622325346,19.6587446305158,14.5889788815537));
#141891=CARTESIAN_POINT('Ctrl Pts',(16.2306352202496,19.7465042292131,14.5934424408955));
#141892=CARTESIAN_POINT('Ctrl Pts',(16.2494446598929,19.8344342326776,14.59791466723));
#141893=CARTESIAN_POINT('Ctrl Pts',(16.2728657964751,19.9212542602436,14.6023868935645));
#141894=CARTESIAN_POINT('Ctrl Pts',(16.3007333122769,20.0064955854165,14.606859119899));
#141895=CARTESIAN_POINT('Ctrl Pts',(16.3286838403156,20.0919908289195,14.6113446681784));
#141896=CARTESIAN_POINT('Ctrl Pts',(16.3611071025133,20.175897631469,14.6158302164578));
#141897=CARTESIAN_POINT('Ctrl Pts',(16.3977895032108,20.2577666954446,14.6203157647373));
#141898=CARTESIAN_POINT('Ctrl Pts',(16.4111522146037,20.2875900617759,14.6219497659465));
#141899=CARTESIAN_POINT('Ctrl Pts',(16.4250796827617,20.3171432681483,14.6235837671557));
#141900=CARTESIAN_POINT('Ctrl Pts',(16.4395601204677,20.3464054955,14.625217768365));
#141901=CARTESIAN_POINT('Ctrl Pts',(16.4766441429939,20.4213452949944,14.629402402758));
#141902=CARTESIAN_POINT('Ctrl Pts',(16.5174725051856,20.4946058152549,14.633587037151));
#141903=CARTESIAN_POINT('Ctrl Pts',(16.5618698248528,20.5657879916116,14.6377716715441));
#141904=CARTESIAN_POINT('Ctrl Pts',(16.6062039504308,20.636868848951,14.641950349628));
#141905=CARTESIAN_POINT('Ctrl Pts',(16.6540967016935,20.7058768514384,14.646129027712));
#141906=CARTESIAN_POINT('Ctrl Pts',(16.7053259809371,20.7724357893872,14.6503077057959));
#141907=CARTESIAN_POINT('Ctrl Pts',(16.7574735081934,20.8401877484638,14.6545612836814));
#141908=CARTESIAN_POINT('Ctrl Pts',(16.8130781406444,20.9054015483267,14.6588148615668));
#141909=CARTESIAN_POINT('Ctrl Pts',(16.8718583319471,20.9677095400496,14.6630684394523));
#141910=CARTESIAN_POINT('Ctrl Pts',(16.9294989545412,21.0288095697688,14.6672395534302));
#141911=CARTESIAN_POINT('Ctrl Pts',(16.9901927757377,21.0871151053885,14.6714106674082));
#141912=CARTESIAN_POINT('Ctrl Pts',(17.0536336491124,21.1423127470207,14.6755817813861));
#141913=CARTESIAN_POINT('Ctrl Pts',(17.1170532342894,21.1974918665512,14.6797514957065));
#141914=CARTESIAN_POINT('Ctrl Pts',(17.1832176941668,21.249564861567,14.6839212100268));
#141915=CARTESIAN_POINT('Ctrl Pts',(17.2517856166925,21.2982566976576,14.6880909243472));
#141916=CARTESIAN_POINT('Ctrl Pts',(17.3203510992774,21.3469468010837,14.6922604902913));
#141917=CARTESIAN_POINT('Ctrl Pts',(17.3913194988898,21.3922557191442,14.6964300562353));
#141918=CARTESIAN_POINT('Ctrl Pts',(17.4643191824367,21.4339508814888,14.7005996221793));
#141919=CARTESIAN_POINT('Ctrl Pts',(17.5398854448023,21.4771119943049,14.7049157849183));
#141920=CARTESIAN_POINT('Ctrl Pts',(17.6176280306767,21.5164002423865,14.7092319476572));
#141921=CARTESIAN_POINT('Ctrl Pts',(17.6971072733111,21.5516096371116,14.7135481103961));
#141922=CARTESIAN_POINT('Ctrl Pts',(17.7739974879763,21.5856720895068,14.7177236745878));
#141923=CARTESIAN_POINT('Ctrl Pts',(17.8525124972024,21.6159172197027,14.7218992387795));
#141924=CARTESIAN_POINT('Ctrl Pts',(17.9322359204944,21.6422084157502,14.7260748029711));
#141925=CARTESIAN_POINT('Ctrl Pts',(18.0159859843726,21.6698275176087,14.7304612649837));
#141926=CARTESIAN_POINT('Ctrl Pts',(18.1010691812453,21.6930826078308,14.7348477269962));
#141927=CARTESIAN_POINT('Ctrl Pts',(18.1869895560291,21.7118757614457,14.7392341890088));
#141928=CARTESIAN_POINT('Ctrl Pts',(18.2729099308129,21.7306689150606,14.7436206510213));
#141929=CARTESIAN_POINT('Ctrl Pts',(18.3596668986516,21.7450001125529,14.7480071130339));
#141930=CARTESIAN_POINT('Ctrl Pts',(18.4467595506039,21.7548342957494,14.7523935750464));
#141931=CARTESIAN_POINT('Ctrl Pts',(18.5298449405376,21.7642159935992,14.7565782094394));
#141932=CARTESIAN_POINT('Ctrl Pts',(18.6135450624313,21.7695403323457,14.7607628438325));
#141933=CARTESIAN_POINT('Ctrl Pts',(18.6974294349979,21.7707387745189,14.7649474782255));
#141934=CARTESIAN_POINT('Ctrl Pts',(18.781194408543,21.7719355108579,14.7691261563095));
#141935=CARTESIAN_POINT('Ctrl Pts',(18.8651426557824,21.7690180091444,14.7733048343934));
#141936=CARTESIAN_POINT('Ctrl Pts',(18.9488376266316,21.7619693832313,14.7774835124774));
#141937=CARTESIAN_POINT('Ctrl Pts',(19.0340327696827,21.7547944157644,14.7817370903628));
#141938=CARTESIAN_POINT('Ctrl Pts',(19.1189649879803,21.7433387124852,14.7859906682483));
#141939=CARTESIAN_POINT('Ctrl Pts',(19.2031727512633,21.7276400079217,14.7902442461337));
#141940=CARTESIAN_POINT('Ctrl Pts',(19.2857479827372,21.7122456533796,14.7944153601116));
#141941=CARTESIAN_POINT('Ctrl Pts',(19.3676261254066,21.6927714353378,14.7985864740896));
#141942=CARTESIAN_POINT('Ctrl Pts',(19.4483779483096,21.6693051370749,14.8027575880675));
#141943=CARTESIAN_POINT('Ctrl Pts',(19.5291026741586,21.6458467131551,14.8069273023879));
#141944=CARTESIAN_POINT('Ctrl Pts',(19.6087013894602,21.6183989977105,14.8110970167083));
#141945=CARTESIAN_POINT('Ctrl Pts',(19.686758033932,21.5871001933374,14.8152667310287));
#141946=CARTESIAN_POINT('Ctrl Pts',(19.7648119008134,21.55580250271,14.8194362969727));
#141947=CARTESIAN_POINT('Ctrl Pts',(19.8413233792987,21.5206541676233,14.8236058629168));
#141948=CARTESIAN_POINT('Ctrl Pts',(19.9158957565834,21.4818417867765,14.8277754288608));
#141949=CARTESIAN_POINT('Ctrl Pts',(19.9930900066584,21.4416648104994,14.8320915915997));
#141950=CARTESIAN_POINT('Ctrl Pts',(20.068205793024,21.397561582336,14.8364077543386));
#141951=CARTESIAN_POINT('Ctrl Pts',(20.1408319285751,21.349790294709,14.8407239170776));
#141952=CARTESIAN_POINT('Ctrl Pts',(20.2110922753996,21.3035751517518,14.8448994812692));
#141953=CARTESIAN_POINT('Ctrl Pts',(20.2790223288379,21.253927569593,14.8490750454609));
#141954=CARTESIAN_POINT('Ctrl Pts',(20.3442818409956,21.2011237128781,14.8532506096526));
#141955=CARTESIAN_POINT('Ctrl Pts',(20.4128374559725,21.1456528588899,14.8576370716651));
#141956=CARTESIAN_POINT('Ctrl Pts',(20.4784452273881,21.0866988942974,14.8620235336777));
#141957=CARTESIAN_POINT('Ctrl Pts',(20.5407543647588,21.0246258339098,14.8664099956902));
#141958=CARTESIAN_POINT('Ctrl Pts',(20.6030635021294,20.9625527735222,14.8707964577027));
#141959=CARTESIAN_POINT('Ctrl Pts',(20.6620736724742,20.8973610985477,14.8751829197153));
#141960=CARTESIAN_POINT('Ctrl Pts',(20.7174842649081,20.8294530178111,14.8795693817278));
#141961=CARTESIAN_POINT('Ctrl Pts',(20.770345333846,20.764669488533,14.8837540161209));
#141962=CARTESIAN_POINT('Ctrl Pts',(20.8201275486196,20.6971728954314,14.8879386505139));
#141963=CARTESIAN_POINT('Ctrl Pts',(20.866540268707,20.6272881071107,14.892123284907));
#141964=CARTESIAN_POINT('Ctrl Pts',(20.912886926032,20.5575027911363,14.8963019629909));
#141965=CARTESIAN_POINT('Ctrl Pts',(20.9558733628218,20.4853364119634,14.9004806410749));
#141966=CARTESIAN_POINT('Ctrl Pts',(20.995249084218,20.4111468989766,14.9046593191588));
#141967=CARTESIAN_POINT('Ctrl Pts',(21.0353305871215,20.3356275922885,14.9089128970442));
#141968=CARTESIAN_POINT('Ctrl Pts',(21.0716703524657,20.2580122826047,14.9131664749297));
#141969=CARTESIAN_POINT('Ctrl Pts',(21.1040502914401,20.1787094688203,14.9174200528151));
#141970=CARTESIAN_POINT('Ctrl Pts',(21.1358024821133,20.1009440948279,14.9215911667931));
#141971=CARTESIAN_POINT('Ctrl Pts',(21.1637468322871,20.0215565094717,14.925762280771));
#141972=CARTESIAN_POINT('Ctrl Pts',(21.1877248192282,19.9409551434873,14.929933394749));
#141973=CARTESIAN_POINT('Ctrl Pts',(21.2116947601242,19.8603808240695,14.9341031090693));
#141974=CARTESIAN_POINT('Ctrl Pts',(21.2317008500142,19.7785939734877,14.9382728233897));
#141975=CARTESIAN_POINT('Ctrl Pts',(21.2476340898708,19.6960192390404,14.9424425377101));
#141976=CARTESIAN_POINT('Ctrl Pts',(21.2635667627544,19.6134474429565,14.9466121036541));
#141977=CARTESIAN_POINT('Ctrl Pts',(21.2754267874401,19.5300882706128,14.9507816695982));
#141978=CARTESIAN_POINT('Ctrl Pts',(21.2831563307877,19.4463762970336,14.9549512355422));
#141979=CARTESIAN_POINT('Ctrl Pts',(21.2911576353439,19.3597211137331,14.9592673982812));
#141980=CARTESIAN_POINT('Ctrl Pts',(21.2947325504218,19.2726883838095,14.9635835610201));
#141981=CARTESIAN_POINT('Ctrl Pts',(21.2938756072079,19.1857636052077,14.967899723759));
#141982=CARTESIAN_POINT('Ctrl Pts',(21.293046578829,19.1016703921261,14.9720752879507));
#141983=CARTESIAN_POINT('Ctrl Pts',(21.2880700686645,19.0176786727669,14.9762508521424));
#141984=CARTESIAN_POINT('Ctrl Pts',(21.2789941177452,18.9342240244486,14.980426416334));
#141985=CARTESIAN_POINT('Ctrl Pts',(21.269459762121,18.8465542802383,14.9848128783466));
#141986=CARTESIAN_POINT('Ctrl Pts',(21.2554010498833,18.7594778642489,14.9891993403591));
#141987=CARTESIAN_POINT('Ctrl Pts',(21.2369341836445,18.6734867700757,14.9935858023717));
#141988=CARTESIAN_POINT('Ctrl Pts',(21.2184673174058,18.5874956759025,14.9979722643842));
#141989=CARTESIAN_POINT('Ctrl Pts',(21.1955925215496,18.5025904439985,15.0023587263968));
#141990=CARTESIAN_POINT('Ctrl Pts',(21.1684852750763,18.4192415485537,15.0067451884093));
#141991=CARTESIAN_POINT('Ctrl Pts',(21.1426284959746,18.3397375686859,15.0109293012962));
#141992=CARTESIAN_POINT('Ctrl Pts',(21.1128249191573,18.2613536084881,15.015113414183));
#141993=CARTESIAN_POINT('Ctrl Pts',(21.079190343033,18.1845097394789,15.0192975270699));
#141994=CARTESIAN_POINT('Ctrl Pts',(21.0456010518531,18.1077693315725,15.0234760065479));
#141995=CARTESIAN_POINT('Ctrl Pts',(21.0081911857072,18.0325653152852,15.0276544860259));
#141996=CARTESIAN_POINT('Ctrl Pts',(20.9671260875766,17.9593020024844,15.0318329655039));
#141997=CARTESIAN_POINT('Ctrl Pts',(20.9250013379249,17.8841481893707,15.0361192672527));
#141998=CARTESIAN_POINT('Ctrl Pts',(20.8790302462392,17.8110370933069,15.0404055690016));
#141999=CARTESIAN_POINT('Ctrl Pts',(20.829443678116,17.740382513417,15.0446918707505));
#142000=CARTESIAN_POINT('Ctrl Pts',(20.7811918107953,17.6716297131431,15.0488627999177));
#142001=CARTESIAN_POINT('Ctrl Pts',(20.7295169255159,17.6052032571564,15.0530337290848));
#142002=CARTESIAN_POINT('Ctrl Pts',(20.6746769356327,17.5414572387916,15.0572046582519));
#142003=CARTESIAN_POINT('Ctrl Pts',(20.6175615422498,17.4750662908128,15.0615486462917));
#142004=CARTESIAN_POINT('Ctrl Pts',(20.5570129607975,17.4115834945697,15.0658926343315));
#142005=CARTESIAN_POINT('Ctrl Pts',(20.4933694385991,17.3513712256143,15.0702366223712));
#142006=CARTESIAN_POINT('Ctrl Pts',(20.4297259164008,17.2911589566588,15.074580610411));
#142007=CARTESIAN_POINT('Ctrl Pts',(20.3629878634338,17.2342176031351,15.0789245984507));
#142008=CARTESIAN_POINT('Ctrl Pts',(20.2935357313021,17.1808649545432,15.0832685864905));
#142009=CARTESIAN_POINT('Origin',(18.734,19.211,-1.76670989022852));
#142010=CARTESIAN_POINT('',(20.2935357313021,17.1808649545432,15.9499155261591));
#142011=CARTESIAN_POINT('',(20.2954006413529,17.1784744524704,15.8832287081017));
#142012=CARTESIAN_POINT('',(20.2935357313021,17.1808649545432,-1.76670989022852));
#142013=CARTESIAN_POINT('',(16.174000571626,19.2092892327452,15.4332901097416));
#142014=CARTESIAN_POINT('Ctrl Pts',(16.1740005716256,19.2092892333484,15.4332901097715));
#142015=CARTESIAN_POINT('Ctrl Pts',(16.1739440307447,19.2938972788889,15.437482057942));
#142016=CARTESIAN_POINT('Ctrl Pts',(16.1780862675835,19.3785303101354,15.4416740061124));
#142017=CARTESIAN_POINT('Ctrl Pts',(16.1864081330308,19.4627452667924,15.4458659542829));
#142018=CARTESIAN_POINT('Ctrl Pts',(16.1947304086796,19.5469643745742,15.4500581090829));
#142019=CARTESIAN_POINT('Ctrl Pts',(16.2072326772703,19.6307649161166,15.4542502638829));
#142020=CARTESIAN_POINT('Ctrl Pts',(16.2238439368849,19.713709199047,15.458442418683));
#142021=CARTESIAN_POINT('Ctrl Pts',(16.2404607969944,19.7966814466863,15.4626359868702));
#142022=CARTESIAN_POINT('Ctrl Pts',(16.261189311038,19.8787964183332,15.4668295550574));
#142023=CARTESIAN_POINT('Ctrl Pts',(16.2859076895266,19.9596281048698,15.4710231232447));
#142024=CARTESIAN_POINT('Ctrl Pts',(16.3106584247115,20.0405656011923,15.4752221808702));
#142025=CARTESIAN_POINT('Ctrl Pts',(16.3394093150967,20.1202160261802,15.4794212384956));
#142026=CARTESIAN_POINT('Ctrl Pts',(16.3719892689075,20.1981703531832,15.4836202961211));
#142027=CARTESIAN_POINT('Ctrl Pts',(16.4045936038559,20.2761830171373,15.4878224961023));
#142028=CARTESIAN_POINT('Ctrl Pts',(16.4410325111314,20.3524966484666,15.4920246960834));
#142029=CARTESIAN_POINT('Ctrl Pts',(16.4810885578785,20.426726134439,15.4962268960645));
#142030=CARTESIAN_POINT('Ctrl Pts',(16.5212156880345,20.5010873479616,15.5004365532643));
#142031=CARTESIAN_POINT('Ctrl Pts',(16.5649725361191,20.5733566470847,15.5046462104641));
#142032=CARTESIAN_POINT('Ctrl Pts',(16.6120981192869,20.6431775059769,15.5088558676639));
#142033=CARTESIAN_POINT('Ctrl Pts',(16.6314200308982,20.6718046841136,15.5105818648583));
#142034=CARTESIAN_POINT('Ctrl Pts',(16.6513077816385,20.700020648932,15.5123078620526));
#142035=CARTESIAN_POINT('Ctrl Pts',(16.6717415022698,20.7278025212728,15.5140338592469));
#142036=CARTESIAN_POINT('Ctrl Pts',(16.7212825156696,20.7951589334866,15.5182184936399));
#142037=CARTESIAN_POINT('Ctrl Pts',(16.7742191330187,20.8602110167103,15.522403128033));
#142038=CARTESIAN_POINT('Ctrl Pts',(16.8303093008605,20.9225962497066,15.526587762426));
#142039=CARTESIAN_POINT('Ctrl Pts',(16.8863196312909,20.9848926850454,15.53076644051));
#142040=CARTESIAN_POINT('Ctrl Pts',(16.9454742913218,21.044529470903,15.5349451185939));
#142041=CARTESIAN_POINT('Ctrl Pts',(17.0074891937054,21.1011747103768,15.5391237966779));
#142042=CARTESIAN_POINT('Ctrl Pts',(17.0706156686449,21.1588352750579,15.5433773745633));
#142043=CARTESIAN_POINT('Ctrl Pts',(17.1367056485331,21.2133956031449,15.5476309524487));
#142044=CARTESIAN_POINT('Ctrl Pts',(17.2054179892121,21.2645425577026,15.5518845303342));
#142045=CARTESIAN_POINT('Ctrl Pts',(17.2727982070859,21.314697928741,15.5560556443121));
#142046=CARTESIAN_POINT('Ctrl Pts',(17.3426996279385,21.3615708076596,15.5602267582901));
#142047=CARTESIAN_POINT('Ctrl Pts',(17.4147663076934,21.4049057557432,15.564397872268));
#142048=CARTESIAN_POINT('Ctrl Pts',(17.4868088047781,21.4482261623665,15.5685675865884));
#142049=CARTESIAN_POINT('Ctrl Pts',(17.561014723861,21.4880107590573,15.5727373009088));
#142050=CARTESIAN_POINT('Ctrl Pts',(17.6370000578042,21.5240480165406,15.5769070152292));
#142051=CARTESIAN_POINT('Ctrl Pts',(17.7129826878631,21.5600839916636,15.5810765811732));
#142052=CARTESIAN_POINT('Ctrl Pts',(17.7907441908666,21.5923726963449,15.5852461471172));
#142053=CARTESIAN_POINT('Ctrl Pts',(17.8698781766135,21.6207496704735,15.5894157130613));
#142054=CARTESIAN_POINT('Ctrl Pts',(17.951794415677,21.6501243440057,15.5937318758002));
#142055=CARTESIAN_POINT('Ctrl Pts',(18.0351809497172,21.6753069180702,15.5980480385391));
#142056=CARTESIAN_POINT('Ctrl Pts',(18.119569008403,21.6961709310559,15.602364201278));
#142057=CARTESIAN_POINT('Ctrl Pts',(18.2012081349532,21.7163553010131,15.6065397654697));
#142058=CARTESIAN_POINT('Ctrl Pts',(18.2837840674898,21.7324980994093,15.6107153296614));
#142059=CARTESIAN_POINT('Ctrl Pts',(18.3668630221883,21.7445371399534,15.6148908938531));
#142060=CARTESIAN_POINT('Ctrl Pts',(18.4541380973871,21.7571842438152,15.6192773558656));
#142061=CARTESIAN_POINT('Ctrl Pts',(18.5419677640929,21.7653020795901,15.6236638178781));
#142062=CARTESIAN_POINT('Ctrl Pts',(18.6298465962985,21.7688803858854,15.6280502798907));
#142063=CARTESIAN_POINT('Ctrl Pts',(18.7177254285041,21.7724586921808,15.6324367419032));
#142064=CARTESIAN_POINT('Ctrl Pts',(18.8056528468587,21.771497551399,15.6368232039158));
#142065=CARTESIAN_POINT('Ctrl Pts',(18.8931294701918,21.7660494734381,15.6412096659283));
#142066=CARTESIAN_POINT('Ctrl Pts',(18.9765811644138,21.7608520696202,15.6453943003213));
#142067=CARTESIAN_POINT('Ctrl Pts',(19.0599332586381,21.7515522106696,15.6495789347144));
#142068=CARTESIAN_POINT('Ctrl Pts',(19.1427499109294,21.7381571993675,15.6537635691074));
#142069=CARTESIAN_POINT('Ctrl Pts',(19.225448683967,21.7247812542061,15.6579422471914));
#142070=CARTESIAN_POINT('Ctrl Pts',(19.3076130786653,21.7073218076316,15.6621209252753));
#142071=CARTESIAN_POINT('Ctrl Pts',(19.388810251214,21.6858380825632,15.6662996033593));
#142072=CARTESIAN_POINT('Ctrl Pts',(19.4714628247252,21.6639692771631,15.6705531812447));
#142073=CARTESIAN_POINT('Ctrl Pts',(19.5531126789051,21.6379305338182,15.6748067591302));
#142074=CARTESIAN_POINT('Ctrl Pts',(19.6333118602839,21.6078392056942,15.6790603370156));
#142075=CARTESIAN_POINT('Ctrl Pts',(19.7119562240359,21.5783312566842,15.6832314509935));
#142076=CARTESIAN_POINT('Ctrl Pts',(19.7892052107347,21.5449266242311,15.6874025649715));
#142077=CARTESIAN_POINT('Ctrl Pts',(19.8646513710675,21.5077863368418,15.6915736789494));
#142078=CARTESIAN_POINT('Ctrl Pts',(19.9400722147125,21.4706585122347,15.6957433932698));
#142079=CARTESIAN_POINT('Ctrl Pts',(20.0136910210535,21.4297977252414,15.6999131075902));
#142080=CARTESIAN_POINT('Ctrl Pts',(20.0851220716649,21.3854123683101,15.7040828219106));
#142081=CARTESIAN_POINT('Ctrl Pts',(20.156550580453,21.3410285908003,15.7082523878546));
#142082=CARTESIAN_POINT('Ctrl Pts',(20.2257910980039,21.2931207362392,15.7124219537986));
#142083=CARTESIAN_POINT('Ctrl Pts',(20.2924853680827,21.2419414953347,15.7165915197427));
#142084=CARTESIAN_POINT('Ctrl Pts',(20.3615245264211,21.1889628554564,15.7209076824816));
#142085=CARTESIAN_POINT('Ctrl Pts',(20.4278346353059,21.1324788262494,15.7252238452205));
#142086=CARTESIAN_POINT('Ctrl Pts',(20.4910556240458,21.0728151181063,15.7295400079595));
#142087=CARTESIAN_POINT('Ctrl Pts',(20.5522171957272,21.0150949489804,15.7337155721511));
#142088=CARTESIAN_POINT('Ctrl Pts',(20.6104875206308,20.9543994482413,15.7378911363428));
#142089=CARTESIAN_POINT('Ctrl Pts',(20.6655795109702,20.8910596991774,15.7420667005345));
#142090=CARTESIAN_POINT('Ctrl Pts',(20.7234540667728,20.8245208099644,15.746453162547));
#142091=CARTESIAN_POINT('Ctrl Pts',(20.7778204147506,20.7550639901489,15.7508396245596));
#142092=CARTESIAN_POINT('Ctrl Pts',(20.8283963491848,20.6831086687203,15.7552260865721));
#142093=CARTESIAN_POINT('Ctrl Pts',(20.8789722836189,20.6111533472918,15.7596125485847));
#142094=CARTESIAN_POINT('Ctrl Pts',(20.9257575602053,20.5367000559954,15.7639990105972));
#142095=CARTESIAN_POINT('Ctrl Pts',(20.968526025902,20.4601971179788,15.7683854726097));
#142096=CARTESIAN_POINT('Ctrl Pts',(21.009326651094,20.3872141935449,15.7725701070028));
#142097=CARTESIAN_POINT('Ctrl Pts',(21.0466238491572,20.3120944357929,15.7767547413958));
#142098=CARTESIAN_POINT('Ctrl Pts',(21.0801878476019,20.2352082716739,15.7809393757889));
#142099=CARTESIAN_POINT('Ctrl Pts',(21.1137040718492,20.158431545493,15.7851180538728));
#142100=CARTESIAN_POINT('Ctrl Pts',(21.1434974687764,20.079893825063,15.7892967319568));
#142101=CARTESIAN_POINT('Ctrl Pts',(21.1693835453415,19.9999911197724,15.7934754100407));
#142102=CARTESIAN_POINT('Ctrl Pts',(21.1957336112251,19.9186562159145,15.7977289879261));
#142103=CARTESIAN_POINT('Ctrl Pts',(21.2180346662481,19.8359073320101,15.8019825658116));
#142104=CARTESIAN_POINT('Ctrl Pts',(21.2361429171343,19.7521846470798,15.806236143697));
#142105=CARTESIAN_POINT('Ctrl Pts',(21.2539001042417,19.6700850897683,15.8104072576749));
#142106=CARTESIAN_POINT('Ctrl Pts',(21.2676255061034,19.587049622894,15.8145783716529));
#142107=CARTESIAN_POINT('Ctrl Pts',(21.2772339776254,19.5035080085254,15.8187494856308));
#142108=CARTESIAN_POINT('Ctrl Pts',(21.2868392249321,19.4199944273523,15.8229191999512));
#142109=CARTESIAN_POINT('Ctrl Pts',(21.2923302330118,19.3359754926349,15.8270889142716));
#142110=CARTESIAN_POINT('Ctrl Pts',(21.2936734448665,19.2518883314075,15.8312586285919));
#142111=CARTESIAN_POINT('Ctrl Pts',(21.295016608924,19.1678041623623,15.835428194536));
#142112=CARTESIAN_POINT('Ctrl Pts',(21.2922122637205,19.0836522316219,15.83959776048));
#142113=CARTESIAN_POINT('Ctrl Pts',(21.2852789648471,18.9998705526724,15.8437673264241));
#142114=CARTESIAN_POINT('Ctrl Pts',(21.2781018997384,18.9131432132468,15.848083489163));
#142115=CARTESIAN_POINT('Ctrl Pts',(21.2665001742354,18.8268131717716,15.8523996519019));
#142116=CARTESIAN_POINT('Ctrl Pts',(21.2505527597976,18.7413594915737,15.8567158146408));
#142117=CARTESIAN_POINT('Ctrl Pts',(21.2351248307078,18.6586894560201,15.8608913788325));
#142118=CARTESIAN_POINT('Ctrl Pts',(21.2156301415437,18.5768400108863,15.8650669430242));
#142119=CARTESIAN_POINT('Ctrl Pts',(21.1921916857822,18.4962317606726,15.8692425072158));
#142120=CARTESIAN_POINT('Ctrl Pts',(21.1675694093398,18.4115521793684,15.8736289692284));
#142121=CARTESIAN_POINT('Ctrl Pts',(21.1385946886761,18.3282430251669,15.8780154312409));
#142122=CARTESIAN_POINT('Ctrl Pts',(21.105467444592,18.2467686173742,15.8824018932534));
#142123=CARTESIAN_POINT('Ctrl Pts',(21.0723402005079,18.1652942095816,15.886788355266));
#142124=CARTESIAN_POINT('Ctrl Pts',(21.0350607478797,18.0856550414427,15.8911748172785));
#142125=CARTESIAN_POINT('Ctrl Pts',(20.9938836431738,18.0082839406927,15.8955612792911));
#142126=CARTESIAN_POINT('Ctrl Pts',(20.9545971350278,17.9344652397039,15.8997463422482));
#142127=CARTESIAN_POINT('Ctrl Pts',(20.9116167922617,17.8624361059936,15.9039314052054));
#142128=CARTESIAN_POINT('Ctrl Pts',(20.8651297737837,17.7925903668923,15.9081164681625));
#142129=CARTESIAN_POINT('Ctrl Pts',(20.8187208419221,17.722861951242,15.9122945012559));
#142130=CARTESIAN_POINT('Ctrl Pts',(20.7688171985839,17.6553100179064,15.9164725343493));
#142131=CARTESIAN_POINT('Ctrl Pts',(20.7156518556546,17.5903038770391,15.9206505674427));
#142132=CARTESIAN_POINT('Ctrl Pts',(20.6625380463695,17.5253607472076,15.9248245507312));
#142133=CARTESIAN_POINT('Ctrl Pts',(20.6061691036096,17.4629588649992,15.9289985340196));
#142134=CARTESIAN_POINT('Ctrl Pts',(20.5468208180928,17.4034379176666,15.933172517308));
#142135=CARTESIAN_POINT('Ctrl Pts',(20.4875162743701,17.343960839386,15.9373434242225));
#142136=CARTESIAN_POINT('Ctrl Pts',(20.4252370755919,17.2873608011117,15.941514331137));
#142137=CARTESIAN_POINT('Ctrl Pts',(20.3602977400031,17.2339426763847,15.9456852380515));
#142138=CARTESIAN_POINT('Ctrl Pts',(20.3383431144115,17.2158831302321,15.9470953340874));
#142139=CARTESIAN_POINT('Ctrl Pts',(20.3160847536487,17.1981869578917,15.9485054301233));
#142140=CARTESIAN_POINT('Ctrl Pts',(20.2935357313021,17.1808649545432,15.9499155261591));
#142141=CARTESIAN_POINT('Ctrl Pts',(20.2935357313021,17.1808649545431,15.149955387129));
#142142=CARTESIAN_POINT('Ctrl Pts',(20.2270593312522,17.1297982427999,15.1541321186299));
#142143=CARTESIAN_POINT('Ctrl Pts',(20.157982890463,17.0819316190979,15.1583088501308));
#142144=CARTESIAN_POINT('Ctrl Pts',(20.0866487390076,17.0375370054079,15.1624855816317));
#142145=CARTESIAN_POINT('Ctrl Pts',(20.0153845446641,16.9931859293349,15.166658217029));
#142146=CARTESIAN_POINT('Ctrl Pts',(19.9418674289854,16.9523003382024,15.1708308524263));
#142147=CARTESIAN_POINT('Ctrl Pts',(19.866470098234,16.915109872706,15.1750034878237));
#142148=CARTESIAN_POINT('Ctrl Pts',(19.7911122885109,16.8779389013406,15.1791739360502));
#142149=CARTESIAN_POINT('Ctrl Pts',(19.713876632298,16.8444594130657,15.1833443842767));
#142150=CARTESIAN_POINT('Ctrl Pts',(19.6351609058952,16.8148553838121,15.1875148325032));
#142151=CARTESIAN_POINT('Ctrl Pts',(19.5564628268888,16.7852579915301,15.1916843457507));
#142152=CARTESIAN_POINT('Ctrl Pts',(19.476285767298,16.7595344941138,15.1958538589982));
#142153=CARTESIAN_POINT('Ctrl Pts',(19.39504670236,16.7378204154775,15.2000233722457));
#142154=CARTESIAN_POINT('Ctrl Pts',(19.3138014809693,16.7161046913065,15.2041932014669));
#142155=CARTESIAN_POINT('Ctrl Pts',(19.2314945392017,16.6983991067548,15.2083630306881));
#142156=CARTESIAN_POINT('Ctrl Pts',(19.1485558711826,16.6847887203031,15.2125328599093));
#142157=CARTESIAN_POINT('Ctrl Pts',(19.0655304067008,16.6711640903938,15.2167070529145));
#142158=CARTESIAN_POINT('Ctrl Pts',(18.9818723507359,16.6616432910686,15.2208812459196));
#142159=CARTESIAN_POINT('Ctrl Pts',(18.8980192099718,16.6562597590439,15.2250554389248));
#142160=CARTESIAN_POINT('Ctrl Pts',(18.8141207284214,16.6508733160541,15.2292318889854));
#142161=CARTESIAN_POINT('Ctrl Pts',(18.7300274122327,16.6496286018667,15.2334083390461));
#142162=CARTESIAN_POINT('Ctrl Pts',(18.6461767343805,16.6525068743466,15.2375847891067));
#142163=CARTESIAN_POINT('Ctrl Pts',(18.5621801887309,16.6553901539089,15.2417685045776));
#142164=CARTESIAN_POINT('Ctrl Pts',(18.4784275833816,16.6624107077525,15.2459522200485));
#142165=CARTESIAN_POINT('Ctrl Pts',(18.3953510240905,16.6734979071702,15.2501359355193));
#142166=CARTESIAN_POINT('Ctrl Pts',(18.3321635993764,16.6819307501343,15.2533180389742));
#142167=CARTESIAN_POINT('Ctrl Pts',(18.2693671588674,16.6927150749222,15.2565001424291));
#142168=CARTESIAN_POINT('Ctrl Pts',(18.2071464487601,16.7058003401833,15.259682245884));
#142169=CARTESIAN_POINT('Ctrl Pts',(18.125322923169,16.7230081562804,15.2638668802771));
#142170=CARTESIAN_POINT('Ctrl Pts',(18.0441910630359,16.74426092691,15.2680515146701));
#142171=CARTESIAN_POINT('Ctrl Pts',(17.9641810754836,16.7694884142285,15.2722361490632));
#142172=CARTESIAN_POINT('Ctrl Pts',(17.8842849722453,16.7946799933414,15.2764148271471));
#142173=CARTESIAN_POINT('Ctrl Pts',(17.8055080047355,16.8238349143801,15.2805935052311));
#142174=CARTESIAN_POINT('Ctrl Pts',(17.7282699071042,16.8568319982967,15.284772183315));
#142175=CARTESIAN_POINT('Ctrl Pts',(17.6496473720828,16.8904205312279,15.2890257612004));
#142176=CARTESIAN_POINT('Ctrl Pts',(17.5726198898781,16.92799022417,15.2932793390859));
#142177=CARTESIAN_POINT('Ctrl Pts',(17.4976137413829,16.969360194076,15.2975329169713));
#142178=CARTESIAN_POINT('Ctrl Pts',(17.4240617334388,17.0099281263886,15.3017040309493));
#142179=CARTESIAN_POINT('Ctrl Pts',(17.3524538049873,17.0541500666244,15.3058751449272));
#142180=CARTESIAN_POINT('Ctrl Pts',(17.2831698439506,17.1018077711367,15.3100462589052));
#142181=CARTESIAN_POINT('Ctrl Pts',(17.213909131816,17.1494494836459,15.3142159732255));
#142182=CARTESIAN_POINT('Ctrl Pts',(17.1469712170492,17.2005244102484,15.3183856875459));
#142183=CARTESIAN_POINT('Ctrl Pts',(17.0827076373572,17.2547705827083,15.3225554018663));
#142184=CARTESIAN_POINT('Ctrl Pts',(17.0184463444392,17.3090148248565,15.3267249678103));
#142185=CARTESIAN_POINT('Ctrl Pts',(16.9568595483703,17.3664297911051,15.3308945337544));
#142186=CARTESIAN_POINT('Ctrl Pts',(16.8982652087742,17.4267136507043,15.3350640996984));
#142187=CARTESIAN_POINT('Ctrl Pts',(16.8376107644817,17.4891170164388,15.3393802624373));
#142188=CARTESIAN_POINT('Ctrl Pts',(16.7801634890497,17.5545943914717,15.3436964251763));
#142189=CARTESIAN_POINT('Ctrl Pts',(16.7262325806843,17.6227714301982,15.3480125879152));
#142190=CARTESIAN_POINT('Ctrl Pts',(16.6740584659865,17.6887276090592,15.3521881521069));
#142191=CARTESIAN_POINT('Ctrl Pts',(16.6251753803871,17.7572098587054,15.3563637162985));
#142192=CARTESIAN_POINT('Ctrl Pts',(16.5798195291699,17.8278490685777,15.3605392804902));
#142193=CARTESIAN_POINT('Ctrl Pts',(16.5321728617311,17.9020560970119,15.3649257425027));
#142194=CARTESIAN_POINT('Ctrl Pts',(16.4884194038191,17.9786432012271,15.3693122045153));
#142195=CARTESIAN_POINT('Ctrl Pts',(16.4487777573747,18.0571545589593,15.3736986665278));
#142196=CARTESIAN_POINT('Ctrl Pts',(16.4091361109302,18.1356659166915,15.3780851285404));
#142197=CARTESIAN_POINT('Ctrl Pts',(16.3736064408138,18.2161009664617,15.3824715905529));
#142198=CARTESIAN_POINT('Ctrl Pts',(16.3423477078172,18.2979833992217,15.3868580525655));
#142199=CARTESIAN_POINT('Ctrl Pts',(16.3083133302776,18.3871366489943,15.3916340140293));
#142200=CARTESIAN_POINT('Ctrl Pts',(16.2792349760219,18.4782809296076,15.396409975493));
#142201=CARTESIAN_POINT('Ctrl Pts',(16.2553188691388,18.5708907503302,15.4011859369568));
#142202=CARTESIAN_POINT('Ctrl Pts',(16.2315006236311,18.6631216245767,15.4059423558521));
#142203=CARTESIAN_POINT('Ctrl Pts',(16.2128025911618,18.756805887815,15.4106987747473));
#142204=CARTESIAN_POINT('Ctrl Pts',(16.1993817363335,18.8514026453261,15.4154551936426));
#142205=CARTESIAN_POINT('Ctrl Pts',(16.1860549755608,18.9453361818529,15.4201782651283));
#142206=CARTESIAN_POINT('Ctrl Pts',(16.1779317634136,19.0401692636772,15.4249013366139));
#142207=CARTESIAN_POINT('Ctrl Pts',(16.1751178968034,19.1353535728534,15.4296244080995));
#142208=CARTESIAN_POINT('Ctrl Pts',(16.1743899245164,19.1599785991389,15.4308463086469));
#142209=CARTESIAN_POINT('Ctrl Pts',(16.1740170525925,19.1846270439603,15.4320682091943));
#142210=CARTESIAN_POINT('Ctrl Pts',(16.174000571626,19.2092892327452,15.4332901097416));
#142211=CARTESIAN_POINT('',(16.1740008768645,19.213118854712,15.3667098902285));
#142212=CARTESIAN_POINT('Ctrl Pts',(20.2935357313021,17.1808649545432,15.0832685864905));
#142213=CARTESIAN_POINT('Ctrl Pts',(20.2260494003338,17.1290224208383,15.0874896205405));
#142214=CARTESIAN_POINT('Ctrl Pts',(20.15600103177,17.0805683880659,15.0917106545905));
#142215=CARTESIAN_POINT('Ctrl Pts',(20.0837719748573,17.0357492981521,15.0959316886405));
#142216=CARTESIAN_POINT('Ctrl Pts',(20.0123180844573,16.9914112093633,15.1001074223034));
#142217=CARTESIAN_POINT('Ctrl Pts',(19.9387305254191,16.9506305872145,15.1042831559662));
#142218=CARTESIAN_POINT('Ctrl Pts',(19.8634030708264,16.9135995769984,15.108458889629));
#142219=CARTESIAN_POINT('Ctrl Pts',(19.7868498330056,16.8759659712017,15.1127025738726));
#142220=CARTESIAN_POINT('Ctrl Pts',(19.7085000246848,16.8422052935393,15.1169462581162));
#142221=CARTESIAN_POINT('Ctrl Pts',(19.6287860049645,16.8124675309015,15.1211899423598));
#142222=CARTESIAN_POINT('Ctrl Pts',(19.5490719852442,16.7827297682637,15.1254336266034));
#142223=CARTESIAN_POINT('Ctrl Pts',(19.467994242552,16.7570150062661,15.1296773108471));
#142224=CARTESIAN_POINT('Ctrl Pts',(19.3859971465604,16.7354193164275,15.1339209950907));
#142225=CARTESIAN_POINT('Ctrl Pts',(19.3051410205342,16.7141241254443,15.1381056294837));
#142226=CARTESIAN_POINT('Ctrl Pts',(19.2230900288855,16.6967547916185,15.1422902638768));
#142227=CARTESIAN_POINT('Ctrl Pts',(19.140260221412,16.6834413691275,15.1464748982698));
#142228=CARTESIAN_POINT('Ctrl Pts',(19.0575483119171,16.6701468966454,15.1506535763538));
#142229=CARTESIAN_POINT('Ctrl Pts',(18.9740602388407,16.66089694071,15.1548322544377));
#142230=CARTESIAN_POINT('Ctrl Pts',(18.8902255245013,16.6557713242267,15.1590109325216));
#142231=CARTESIAN_POINT('Ctrl Pts',(18.8048881331583,16.6505538347516,15.1632645104071));
#142232=CARTESIAN_POINT('Ctrl Pts',(18.7191920174707,16.6496101194126,15.1675180882925));
#142233=CARTESIAN_POINT('Ctrl Pts',(18.6335993142648,16.652969565798,15.171771666178));
#142234=CARTESIAN_POINT('Ctrl Pts',(18.549665992631,16.6562638827597,15.1759427801559));
#142235=CARTESIAN_POINT('Ctrl Pts',(18.4658325904041,16.6636959811426,15.1801138941339));
#142236=CARTESIAN_POINT('Ctrl Pts',(18.3825365202428,16.6752410559367,15.1842850081118));
#142237=CARTESIAN_POINT('Ctrl Pts',(18.2992684008824,16.6867822566694,15.1884547224322));
#142238=CARTESIAN_POINT('Ctrl Pts',(18.2165377107927,16.70243362971,15.1926244367525));
#142239=CARTESIAN_POINT('Ctrl Pts',(18.1347761196918,16.7221185762941,15.1967941510729));
#142240=CARTESIAN_POINT('Ctrl Pts',(18.0530174380192,16.7418028224032,15.200963717017));
#142241=CARTESIAN_POINT('Ctrl Pts',(17.9722282338244,16.7655202481684,15.205133282961));
#142242=CARTESIAN_POINT('Ctrl Pts',(17.8928280294743,16.7931435700187,15.209302848905));
#142243=CARTESIAN_POINT('Ctrl Pts',(17.8106362118899,16.8217380937883,15.213619011644));
#142244=CARTESIAN_POINT('Ctrl Pts',(17.7299333840843,16.8545181133117,15.2179351743829));
#142245=CARTESIAN_POINT('Ctrl Pts',(17.6511637413086,16.891287596088,15.2222513371218));
#142246=CARTESIAN_POINT('Ctrl Pts',(17.5749600113613,16.9268593168303,15.2264269013135));
#142247=CARTESIAN_POINT('Ctrl Pts',(17.5005658480124,16.966164316944,15.2306024655052));
#142248=CARTESIAN_POINT('Ctrl Pts',(17.4283578509306,17.0089785244977,15.2347780296969));
#142249=CARTESIAN_POINT('Ctrl Pts',(17.3525027995743,17.0539551758939,15.2391644917094));
#142250=CARTESIAN_POINT('Ctrl Pts',(17.2790610511154,17.1028045279329,15.243550953722));
#142251=CARTESIAN_POINT('Ctrl Pts',(17.2084323379752,17.1552171056787,15.2479374157345));
#142252=CARTESIAN_POINT('Ctrl Pts',(17.137803624835,17.2076296834245,15.252323877747));
#142253=CARTESIAN_POINT('Ctrl Pts',(17.0699883460668,17.2636050588652,15.2567103397596));
#142254=CARTESIAN_POINT('Ctrl Pts',(17.0053421035811,17.3227887096121,15.2610968017721));
#142255=CARTESIAN_POINT('Ctrl Pts',(16.9445899812052,17.3784072924496,15.2652190348167));
#142256=CARTESIAN_POINT('Ctrl Pts',(16.8863955977243,17.4370795204071,15.2693412678613));
#142257=CARTESIAN_POINT('Ctrl Pts',(16.8310887538612,17.4985372152019,15.2734635009059));
#142258=CARTESIAN_POINT('Ctrl Pts',(16.7758743514516,17.5598921878336,15.2775788439313));
#142259=CARTESIAN_POINT('Ctrl Pts',(16.7235382140142,17.6240230272318,15.2816941869568));
#142260=CARTESIAN_POINT('Ctrl Pts',(16.6743754759291,17.6906228034315,15.2858095299822));
#142261=CARTESIAN_POINT('Ctrl Pts',(16.6252589923635,17.7571599195604,15.2899210011074));
#142262=CARTESIAN_POINT('Ctrl Pts',(16.5793102664133,17.8261609852053,15.2940324722327));
#142263=CARTESIAN_POINT('Ctrl Pts',(16.5367853878605,17.8972846776411,15.2981439433579));
#142264=CARTESIAN_POINT('Ctrl Pts',(16.4942868717928,17.9683642783041,15.3022528656553));
#142265=CARTESIAN_POINT('Ctrl Pts',(16.4552082342176,18.0415634879277,15.3063617879526));
#142266=CARTESIAN_POINT('Ctrl Pts',(16.4197623875935,18.1165118669794,15.31047071025));
#142267=CARTESIAN_POINT('Ctrl Pts',(16.3843271437776,18.1914378269504,15.3145784034579));
#142268=CARTESIAN_POINT('Ctrl Pts',(16.3525227351488,18.2681114878987,15.3186860966658));
#142269=CARTESIAN_POINT('Ctrl Pts',(16.3245154961046,18.3461390715913,15.3227937898737));
#142270=CARTESIAN_POINT('Ctrl Pts',(16.2964946934756,18.4242044431483,15.3269034723904));
#142271=CARTESIAN_POINT('Ctrl Pts',(16.2722748983311,18.5036246009546,15.331013154907));
#142272=CARTESIAN_POINT('Ctrl Pts',(16.2519734104525,18.5839880313907,15.3351228374237));
#142273=CARTESIAN_POINT('Ctrl Pts',(16.2316667383952,18.664371983396,15.339233569387));
#142274=CARTESIAN_POINT('Ctrl Pts',(16.2152804642371,18.7456992225571,15.3433443013503));
#142275=CARTESIAN_POINT('Ctrl Pts',(16.2028808242116,18.8275476327413,15.3474550333136));
#142276=CARTESIAN_POINT('Ctrl Pts',(16.1904661338127,18.9094953884816,15.3515707547807));
#142277=CARTESIAN_POINT('Ctrl Pts',(16.1820477886727,18.9919651056506,15.3556864762478));
#142278=CARTESIAN_POINT('Ctrl Pts',(16.1776401048969,19.0745299054429,15.3598021977149));
#142279=CARTESIAN_POINT('Ctrl Pts',(16.175174200724,19.1207212600628,15.3621047618861));
#142280=CARTESIAN_POINT('Ctrl Pts',(16.173962657598,19.1669423575626,15.3644073260573));
#142281=CARTESIAN_POINT('Ctrl Pts',(16.1740008768645,19.213118854712,15.3667098902285));
#142282=CARTESIAN_POINT('Ctrl Pts',(16.1723624648697,19.2131202107894,15.3667098902285));
#142283=CARTESIAN_POINT('Ctrl Pts',(16.1710770500739,19.3573559412274,15.3738974629702));
#142284=CARTESIAN_POINT('Ctrl Pts',(16.2478506686825,20.350918062683,15.4234769712723));
#142285=CARTESIAN_POINT('Ctrl Pts',(17.5479306856132,21.9960550376254,15.515448415135));
#142286=CARTESIAN_POINT('Ctrl Pts',(20.4337937178339,21.715794062981,15.6426242218164));
#142287=CARTESIAN_POINT('Ctrl Pts',(21.7124086289,19.2304391852282,15.7652176528054));
#142288=CARTESIAN_POINT('Ctrl Pts',(20.8926534908113,17.6447068409585,15.8454191482338));
#142289=CARTESIAN_POINT('Ctrl Pts',(20.2954006413529,17.1784744524704,15.8832287081017));
#142290=CARTESIAN_POINT('Origin',(18.734,19.211,-1.76670989022852));
#142291=CARTESIAN_POINT('',(20.2935357313021,17.1808649545432,16.7498176665395));
#142292=CARTESIAN_POINT('',(20.2935357313021,17.1808649545431,16.6833822583817));
#142293=CARTESIAN_POINT('',(20.2935357313021,17.1808649545432,-1.76670989022852));
#142294=CARTESIAN_POINT('',(16.1740007055014,19.2129005700936,16.2332901098004));
#142295=CARTESIAN_POINT('Ctrl Pts',(16.1740007055014,19.2129005700936,16.2332901098004));
#142296=CARTESIAN_POINT('Ctrl Pts',(16.1740727513108,19.3099436741144,16.2381006886061));
#142297=CARTESIAN_POINT('Ctrl Pts',(16.1796667621362,19.4067618611662,16.2429112674118));
#142298=CARTESIAN_POINT('Ctrl Pts',(16.1906824963736,19.5027808693996,16.2477218462175));
#142299=CARTESIAN_POINT('Ctrl Pts',(16.201890345519,19.6004744535201,16.2526163217372));
#142300=CARTESIAN_POINT('Ctrl Pts',(16.218710639996,19.6973405506009,16.2575107972568));
#142301=CARTESIAN_POINT('Ctrl Pts',(16.2409867483461,19.7927945746377,16.2624052727765));
#142302=CARTESIAN_POINT('Ctrl Pts',(16.2632628566961,19.8882485986746,16.2672997482961));
#142303=CARTESIAN_POINT('Ctrl Pts',(16.2909946214077,19.9822904288897,16.2721942238158));
#142304=CARTESIAN_POINT('Ctrl Pts',(16.3239764935689,20.074357804418,16.2770886993355));
#142305=CARTESIAN_POINT('Ctrl Pts',(16.3521750361989,20.1530727360925,16.2812733337285));
#142306=CARTESIAN_POINT('Ctrl Pts',(16.3842865295797,20.2305511910394,16.2854579681216));
#142307=CARTESIAN_POINT('Ctrl Pts',(16.4201827606335,20.3063765484118,16.2896426025146));
#142308=CARTESIAN_POINT('Ctrl Pts',(16.4560278978456,20.3820939777733,16.2938212805986));
#142309=CARTESIAN_POINT('Ctrl Pts',(16.4956468770878,20.4561625710813,16.2979999586825));
#142310=CARTESIAN_POINT('Ctrl Pts',(16.5388624466769,20.5281830252439,16.3021786367664));
#142311=CARTESIAN_POINT('Ctrl Pts',(16.5828526242924,20.6014943942872,16.3064322146519));
#142312=CARTESIAN_POINT('Ctrl Pts',(16.6305694356436,20.6726830222909,16.3106857925373));
#142313=CARTESIAN_POINT('Ctrl Pts',(16.6817755898824,20.7413512572339,16.3149393704228));
#142314=CARTESIAN_POINT('Ctrl Pts',(16.7319890129006,20.8086882244474,16.3191104844007));
#142315=CARTESIAN_POINT('Ctrl Pts',(16.7855574030483,20.8736012662212,16.3232815983787));
#142316=CARTESIAN_POINT('Ctrl Pts',(16.8422127801055,20.9357437823178,16.3274527123566));
#142317=CARTESIAN_POINT('Ctrl Pts',(16.8988491459038,20.997865445893,16.331622426677));
#142318=CARTESIAN_POINT('Ctrl Pts',(16.9585701316818,21.0572180904717,16.3357921409973));
#142319=CARTESIAN_POINT('Ctrl Pts',(17.0210683042879,21.1134891605013,16.3399618553177));
#142320=CARTESIAN_POINT('Ctrl Pts',(17.0835642529408,21.1697582281647,16.3441314212618));
#142321=CARTESIAN_POINT('Ctrl Pts',(17.1488368494857,21.2229456321214,16.3483009872058));
#142322=CARTESIAN_POINT('Ctrl Pts',(17.2165437463578,21.2727775142537,16.3524705531499));
#142323=CARTESIAN_POINT('Ctrl Pts',(17.2866311341984,21.3243614238875,16.3567867158888));
#142324=CARTESIAN_POINT('Ctrl Pts',(17.3593267625536,21.3723491485032,16.3611028786277));
#142325=CARTESIAN_POINT('Ctrl Pts',(17.4342176396321,21.4164853923063,16.3654190413666));
#142326=CARTESIAN_POINT('Ctrl Pts',(17.5066689542669,21.4591839026099,16.3695946055583));
#142327=CARTESIAN_POINT('Ctrl Pts',(17.5811742544608,21.4982778256331,16.37377016975));
#142328=CARTESIAN_POINT('Ctrl Pts',(17.6573356824291,21.533583464005,16.3779457339417));
#142329=CARTESIAN_POINT('Ctrl Pts',(17.7373438430675,21.5706723062399,16.3823321959542));
#142330=CARTESIAN_POINT('Ctrl Pts',(17.8191792885613,21.6035798961265,16.3867186579667));
#142331=CARTESIAN_POINT('Ctrl Pts',(17.9023606575271,21.6321517928563,16.3911051199793));
#142332=CARTESIAN_POINT('Ctrl Pts',(17.985542026493,21.6607236895861,16.3954915819918));
#142333=CARTESIAN_POINT('Ctrl Pts',(18.0700687402226,21.6849598063577,16.3998780440044));
#142334=CARTESIAN_POINT('Ctrl Pts',(18.1554472698608,21.7047675790756,16.4042645060169));
#142335=CARTESIAN_POINT('Ctrl Pts',(18.2368974067891,21.7236639668085,16.4084491404099));
#142336=CARTESIAN_POINT('Ctrl Pts',(18.3194258684925,21.7386009007969,16.412633774803));
#142337=CARTESIAN_POINT('Ctrl Pts',(18.4026129434633,21.7494606789864,16.416818409196));
#142338=CARTESIAN_POINT('Ctrl Pts',(18.4856816119294,21.7603049996258,16.42099708728));
#142339=CARTESIAN_POINT('Ctrl Pts',(18.5694065793227,21.7670836326581,16.4251757653639));
#142340=CARTESIAN_POINT('Ctrl Pts',(18.65335615196,21.769729483508,16.4293544434479));
#142341=CARTESIAN_POINT('Ctrl Pts',(18.7388104603533,21.772422759333,16.4336080213333));
#142342=CARTESIAN_POINT('Ctrl Pts',(18.8244970356233,21.770833526475,16.4378615992187));
#142343=CARTESIAN_POINT('Ctrl Pts',(18.9099530743145,21.7649460674884,16.4421151771042));
#142344=CARTESIAN_POINT('Ctrl Pts',(18.9937523809418,21.7591727483826,16.4462862910821));
#142345=CARTESIAN_POINT('Ctrl Pts',(19.077329529944,21.7492664079889,16.4504574050601));
#142346=CARTESIAN_POINT('Ctrl Pts',(19.1602480327617,21.7352647671286,16.454628519038));
#142347=CARTESIAN_POINT('Ctrl Pts',(19.243138711475,21.7212678246541,16.4587982333584));
#142348=CARTESIAN_POINT('Ctrl Pts',(19.3253707297096,21.7031783874643,16.4629679476788));
#142349=CARTESIAN_POINT('Ctrl Pts',(19.4065148699746,21.6810857777946,16.4671376619991));
#142350=CARTESIAN_POINT('Ctrl Pts',(19.4876561227829,21.6589939542747,16.4713072279432));
#142351=CARTESIAN_POINT('Ctrl Pts',(19.5677091309384,21.6328993631757,16.4754767938872));
#142352=CARTESIAN_POINT('Ctrl Pts',(19.6462583168593,21.6029416304168,16.4796463598313));
#142353=CARTESIAN_POINT('Ctrl Pts',(19.7275691952563,21.571930620731,16.4839625225702));
#142354=CARTESIAN_POINT('Ctrl Pts',(19.8072680422831,21.5367799467921,16.4882786853091));
#142355=CARTESIAN_POINT('Ctrl Pts',(19.8849166499543,21.4976986825679,16.492594848048));
#142356=CARTESIAN_POINT('Ctrl Pts',(19.9600358623978,21.4598904864152,16.4967704122397));
#142357=CARTESIAN_POINT('Ctrl Pts',(20.0332359708031,21.4184041187291,16.5009459764314));
#142358=CARTESIAN_POINT('Ctrl Pts',(20.104147161879,21.3734746830414,16.5051215406231));
#142359=CARTESIAN_POINT('Ctrl Pts',(20.1786399086407,21.3262759683667,16.5095080026356));
#142360=CARTESIAN_POINT('Ctrl Pts',(20.2506059585102,21.2752775637102,16.5138944646481));
#142361=CARTESIAN_POINT('Ctrl Pts',(20.3196548994211,21.2208006219379,16.5182809266607));
#142362=CARTESIAN_POINT('Ctrl Pts',(20.388703840332,21.1663236801656,16.5226673886732));
#142363=CARTESIAN_POINT('Ctrl Pts',(20.4548352860543,21.1083686408955,16.5270538506858));
#142364=CARTESIAN_POINT('Ctrl Pts',(20.5177042670233,21.0473003806031,16.5314403126983));
#142365=CARTESIAN_POINT('Ctrl Pts',(20.5776805529837,20.9890419614915,16.5356249470914));
#142366=CARTESIAN_POINT('Ctrl Pts',(20.6349112416909,20.9277336646777,16.5398095814844));
#142367=CARTESIAN_POINT('Ctrl Pts',(20.6890701824651,20.8636646912292,16.5439942158775));
#142368=CARTESIAN_POINT('Ctrl Pts',(20.7431520346907,20.7996869120343,16.5481728939614));
#142369=CARTESIAN_POINT('Ctrl Pts',(20.7941705292094,20.7329566097132,16.5523515720454));
#142370=CARTESIAN_POINT('Ctrl Pts',(20.8418355824983,20.6638004533156,16.5565302501293));
#142371=CARTESIAN_POINT('Ctrl Pts',(20.890354997611,20.5934047225164,16.5607838280148));
#142372=CARTESIAN_POINT('Ctrl Pts',(20.9353992222983,20.520495651305,16.5650374059002));
#142373=CARTESIAN_POINT('Ctrl Pts',(20.9767045339426,20.4454538765921,16.5692909837856));
#142374=CARTESIAN_POINT('Ctrl Pts',(21.0172090615201,20.3718669331139,16.5734620977636));
#142375=CARTESIAN_POINT('Ctrl Pts',(21.0541181225502,20.2962296630071,16.5776332117415));
#142376=CARTESIAN_POINT('Ctrl Pts',(21.0872271712958,20.2189295016394,16.5818043257195));
#142377=CARTESIAN_POINT('Ctrl Pts',(21.1203251099804,20.1416552790873,16.5859740400399));
#142378=CARTESIAN_POINT('Ctrl Pts',(21.1496253878361,20.0627196959935,16.5901437543602));
#142379=CARTESIAN_POINT('Ctrl Pts',(21.1749707834402,19.9825320047744,16.5943134686806));
#142380=CARTESIAN_POINT('Ctrl Pts',(21.2003152771465,19.9023471669775,16.5984830346247));
#142381=CARTESIAN_POINT('Ctrl Pts',(21.2217050305799,19.820910748543,16.6026526005687));
#142382=CARTESIAN_POINT('Ctrl Pts',(21.2390325027795,19.7386477613126,16.6068221665128));
#142383=CARTESIAN_POINT('Ctrl Pts',(21.2569691875259,19.6534925089337,16.6111383292517));
#142384=CARTESIAN_POINT('Ctrl Pts',(21.2705525077455,19.5674519980823,16.6154544919906));
#142385=CARTESIAN_POINT('Ctrl Pts',(21.2797210678871,19.4810078600997,16.6197706547295));
#142386=CARTESIAN_POINT('Ctrl Pts',(21.2885909631466,19.3973796308195,16.6239462189212));
#142387=CARTESIAN_POINT('Ctrl Pts',(21.2933293236125,19.3133741398416,16.6281217831129));
#142388=CARTESIAN_POINT('Ctrl Pts',(21.2939336612287,19.2294295987024,16.6322973473046));
#142389=CARTESIAN_POINT('Ctrl Pts',(21.2945685225012,19.1412452183496,16.6366838093171));
#142390=CARTESIAN_POINT('Ctrl Pts',(21.2906407927078,19.0531286901045,16.6410702713296));
#142391=CARTESIAN_POINT('Ctrl Pts',(21.2822091879386,18.965582122686,16.6454567333422));
#142392=CARTESIAN_POINT('Ctrl Pts',(21.2737775831694,18.8780355552674,16.6498431953547));
#142393=CARTESIAN_POINT('Ctrl Pts',(21.2608422640145,18.7910595113906,16.6542296573673));
#142394=CARTESIAN_POINT('Ctrl Pts',(21.2435233083642,18.7051415565825,16.6586161193798));
#142395=CARTESIAN_POINT('Ctrl Pts',(21.2270051786283,18.6231964351316,16.6627997520461));
#142396=CARTESIAN_POINT('Ctrl Pts',(21.2064383857994,18.5419087704169,16.6669833847124));
#142397=CARTESIAN_POINT('Ctrl Pts',(21.1818895089893,18.4617090339659,16.6711670173787));
#142398=CARTESIAN_POINT('Ctrl Pts',(21.1573729381811,18.381614839323,16.6753451444389));
#142399=CARTESIAN_POINT('Ctrl Pts',(21.1288848202261,18.3026061663239,16.6795232714992));
#142400=CARTESIAN_POINT('Ctrl Pts',(21.0965427533354,18.2251035862412,16.6837013985594));
#142401=CARTESIAN_POINT('Ctrl Pts',(21.0642335424463,18.1476797403009,16.6878752810997));
#142402=CARTESIAN_POINT('Ctrl Pts',(21.0280783340578,18.0717593708865,16.6920491636399));
#142403=CARTESIAN_POINT('Ctrl Pts',(20.9882441729213,17.9977468488191,16.6962230461801));
#142404=CARTESIAN_POINT('Ctrl Pts',(20.9484385271439,17.9237873087547,16.7003939408387));
#142405=CARTESIAN_POINT('Ctrl Pts',(20.9049593786091,17.8517333063674,16.7045648354973));
#142406=CARTESIAN_POINT('Ctrl Pts',(20.8580208517661,17.7819669628512,16.7087357301559));
#142407=CARTESIAN_POINT('Ctrl Pts',(20.8110938747848,17.7122177862909,16.7129055985092));
#142408=CARTESIAN_POINT('Ctrl Pts',(20.7607094614797,17.6447555353991,16.7170754668625));
#142409=CARTESIAN_POINT('Ctrl Pts',(20.7071258294302,17.5799345625527,16.7212453352158));
#142410=CARTESIAN_POINT('Ctrl Pts',(20.6535492745797,17.5151221511065,16.7254146528228));
#142411=CARTESIAN_POINT('Ctrl Pts',(20.596774638735,17.4529506748439,16.7295839704299));
#142412=CARTESIAN_POINT('Ctrl Pts',(20.537100285066,17.3937412506759,16.7337532880369));
#142413=CARTESIAN_POINT('Ctrl Pts',(20.4773989743761,17.3345050795122,16.7379244890724));
#142414=CARTESIAN_POINT('Ctrl Pts',(20.4147956627377,17.2782339503688,16.742095690108));
#142415=CARTESIAN_POINT('Ctrl Pts',(20.3496246776528,17.2252112647718,16.7462668911436));
#142416=CARTESIAN_POINT('Ctrl Pts',(20.3311321996355,17.2101659060658,16.7474504829422));
#142417=CARTESIAN_POINT('Ctrl Pts',(20.3124331846543,17.1953818477909,16.7486340747409));
#142418=CARTESIAN_POINT('Ctrl Pts',(20.2935357313021,17.1808649545432,16.7498176665395));
#142419=CARTESIAN_POINT('Ctrl Pts',(20.2935357313021,17.1808649545432,15.9499155261591));
#142420=CARTESIAN_POINT('Ctrl Pts',(20.226860236598,17.1296452996606,15.9540850572956));
#142421=CARTESIAN_POINT('Ctrl Pts',(20.1576411597185,17.0817002678535,15.9582545884321));
#142422=CARTESIAN_POINT('Ctrl Pts',(20.0862377111805,17.0372812572779,15.9624241195686));
#142423=CARTESIAN_POINT('Ctrl Pts',(20.0148299716009,16.9928595773099,15.966593901276));
#142424=CARTESIAN_POINT('Ctrl Pts',(19.9412379910235,16.9519645812164,15.9707636829835));
#142425=CARTESIAN_POINT('Ctrl Pts',(19.8658481843313,16.9148032123474,15.974933464691));
#142426=CARTESIAN_POINT('Ctrl Pts',(19.7903801947207,16.8776033053207,15.9791075706661));
#142427=CARTESIAN_POINT('Ctrl Pts',(19.71311106918,16.8441449617549,15.9832816766412));
#142428=CARTESIAN_POINT('Ctrl Pts',(19.6344495075874,16.8145879560715,15.9874557826163));
#142429=CARTESIAN_POINT('Ctrl Pts',(19.5557465188748,16.7850153841878,15.9916320868848));
#142430=CARTESIAN_POINT('Ctrl Pts',(19.4756500721021,16.7593483824272,15.9958083911533));
#142431=CARTESIAN_POINT('Ctrl Pts',(19.3945840932351,16.7376968128099,15.9999846954218));
#142432=CARTESIAN_POINT('Ctrl Pts',(19.3133757562407,16.7160072213621,16.0041683336036));
#142433=CARTESIAN_POINT('Ctrl Pts',(19.2311949364436,16.6983472448517,16.0083519717853));
#142434=CARTESIAN_POINT('Ctrl Pts',(19.1484756398584,16.684775555505,16.012535609967));
#142435=CARTESIAN_POINT('Ctrl Pts',(19.0812407848784,16.6737443862044,16.0159361019689));
#142436=CARTESIAN_POINT('Ctrl Pts',(19.0136504336294,16.6654131890496,16.0193365939707));
#142437=CARTESIAN_POINT('Ctrl Pts',(18.9459382820314,16.6597880988421,16.0227370859726));
#142438=CARTESIAN_POINT('Ctrl Pts',(18.862611928595,16.6528658811356,16.0269217203656));
#142439=CARTESIAN_POINT('Ctrl Pts',(18.7787910168741,16.6500174172728,16.0311063547587));
#142440=CARTESIAN_POINT('Ctrl Pts',(18.6949078655888,16.6512984929826,16.0352909891517));
#142441=CARTESIAN_POINT('Ctrl Pts',(18.6111441115869,16.6525777452396,16.0394696672357));
#142442=CARTESIAN_POINT('Ctrl Pts',(18.5273187500338,16.6579748547684,16.0436483453196));
#142443=CARTESIAN_POINT('Ctrl Pts',(18.4438686393698,16.6674937991861,16.0478270234035));
#142444=CARTESIAN_POINT('Ctrl Pts',(18.3589227454464,16.6771833638414,16.052080601289));
#142445=CARTESIAN_POINT('Ctrl Pts',(18.2743661679611,16.691144024519,16.0563341791744));
#142446=CARTESIAN_POINT('Ctrl Pts',(18.1906591204417,16.709324423791,16.0605877570599));
#142447=CARTESIAN_POINT('Ctrl Pts',(18.1085748973793,16.7271523605469,16.0647588710378));
#142448=CARTESIAN_POINT('Ctrl Pts',(18.0273080288931,16.7490377781068,16.0689299850158));
#142449=CARTESIAN_POINT('Ctrl Pts',(17.9472849642524,16.7748802466774,16.0731010989937));
#142450=CARTESIAN_POINT('Ctrl Pts',(17.8672887521237,16.8007140435581,16.0772708133141));
#142451=CARTESIAN_POINT('Ctrl Pts',(17.7885359523436,16.8305021131094,16.0814405276345));
#142452=CARTESIAN_POINT('Ctrl Pts',(17.7114383592366,16.8640940174691,16.0856102419549));
#142453=CARTESIAN_POINT('Ctrl Pts',(17.6343435095929,16.8976847264847,16.0897798078989));
#142454=CARTESIAN_POINT('Ctrl Pts',(17.5589041709148,16.9350788166487,16.093949373843));
#142455=CARTESIAN_POINT('Ctrl Pts',(17.4855113682725,16.9760780469002,16.098118939787));
#142456=CARTESIAN_POINT('Ctrl Pts',(17.4095381652293,17.0185187595094,16.1024351025259));
#142457=CARTESIAN_POINT('Ctrl Pts',(17.3357585487127,17.0648225852953,16.1067512652648));
#142458=CARTESIAN_POINT('Ctrl Pts',(17.2645758959968,17.1147192929919,16.1110674280038));
#142459=CARTESIAN_POINT('Ctrl Pts',(17.1957120107061,17.1629906206834,16.1152429921954));
#142460=CARTESIAN_POINT('Ctrl Pts',(17.1292788382186,17.214624022349,16.1194185563871));
#142461=CARTESIAN_POINT('Ctrl Pts',(17.0656083164574,17.2693333987819,16.1235941205788));
#142462=CARTESIAN_POINT('Ctrl Pts',(16.9987219480044,17.3268060157592,16.1279805825913));
#142463=CARTESIAN_POINT('Ctrl Pts',(16.934885070269,17.3876731058187,16.1323670446039));
#142464=CARTESIAN_POINT('Ctrl Pts',(16.8744375629657,17.4515604464003,16.1367535066164));
#142465=CARTESIAN_POINT('Ctrl Pts',(16.8139900556624,17.5154477869819,16.141139968629));
#142466=CARTESIAN_POINT('Ctrl Pts',(16.7569322374058,17.5823548872471,16.1455264306415));
#142467=CARTESIAN_POINT('Ctrl Pts',(16.703552701499,17.6518708302357,16.149912892654));
#142468=CARTESIAN_POINT('Ctrl Pts',(16.652554439824,17.7182856499019,16.1541036735168));
#142469=CARTESIAN_POINT('Ctrl Pts',(16.6047208600205,17.7873320135743,16.1582944543796));
#142470=CARTESIAN_POINT('Ctrl Pts',(16.5603345705064,17.8586765917043,16.1624852352424));
#142471=CARTESIAN_POINT('Ctrl Pts',(16.5160108372518,17.9299206196422,16.1666701097864));
#142472=CARTESIAN_POINT('Ctrl Pts',(16.4751249866853,18.0034560458725,16.1708549843304));
#142473=CARTESIAN_POINT('Ctrl Pts',(16.4379187528239,18.0789174471946,16.1750398588744));
#142474=CARTESIAN_POINT('Ctrl Pts',(16.4007539244062,18.15429487031,16.1792200762261));
#142475=CARTESIAN_POINT('Ctrl Pts',(16.367260780246,18.2315936031771,16.1834002935778));
#142476=CARTESIAN_POINT('Ctrl Pts',(16.3376364602561,18.3104214163183,16.1875805109295));
#142477=CARTESIAN_POINT('Ctrl Pts',(16.3080359860438,18.3891857778597,16.1917573634602));
#142478=CARTESIAN_POINT('Ctrl Pts',(16.2822983085872,18.4694763469326,16.1959342159909));
#142479=CARTESIAN_POINT('Ctrl Pts',(16.2605729619713,18.5508797931071,16.2001110685216));
#142480=CARTESIAN_POINT('Ctrl Pts',(16.238858101653,18.632243947813,16.2042859049869));
#142481=CARTESIAN_POINT('Ctrl Pts',(16.2211518401951,18.7147194701818,16.2084607414522));
#142482=CARTESIAN_POINT('Ctrl Pts',(16.2075538451844,18.7978779516685,16.2126355779176));
#142483=CARTESIAN_POINT('Ctrl Pts',(16.1939550163504,18.8810415323988,16.2168106703821));
#142484=CARTESIAN_POINT('Ctrl Pts',(16.1844650395064,18.964887705472,16.2209857628467));
#142485=CARTESIAN_POINT('Ctrl Pts',(16.1791322578277,19.048978951962,16.2251608553112));
#142486=CARTESIAN_POINT('Ctrl Pts',(16.1756711337435,19.1035565169223,16.227870606798));
#142487=CARTESIAN_POINT('Ctrl Pts',(16.1739601228212,19.158237148325,16.2305803582847));
#142488=CARTESIAN_POINT('Ctrl Pts',(16.174000705501,19.2129005695108,16.2332901097715));
#142489=CARTESIAN_POINT('',(16.1740005630998,19.2093020392336,16.1667098902285));
#142490=CARTESIAN_POINT('Ctrl Pts',(20.2954006413529,17.1784744524704,15.8832287081017));
#142491=CARTESIAN_POINT('Ctrl Pts',(20.2230158542988,17.1219688498783,15.8878110837942));
#142492=CARTESIAN_POINT('Ctrl Pts',(19.4492534959823,16.5850864470858,15.9347853950472));
#142493=CARTESIAN_POINT('Ctrl Pts',(17.4141947910433,16.4867742032747,16.0241516418607));
#142494=CARTESIAN_POINT('Ctrl Pts',(16.2227678179363,18.1548349051303,16.1140629935438));
#142495=CARTESIAN_POINT('Ctrl Pts',(16.1704458861955,19.106523168223,16.1615824096664));
#142496=CARTESIAN_POINT('Ctrl Pts',(16.1712324881214,19.2093002032634,16.1667098902285));
#142497=CARTESIAN_POINT('Ctrl Pts',(16.1740005630998,19.2093020392336,16.1667098902285));
#142498=CARTESIAN_POINT('Ctrl Pts',(16.1739457994085,19.2918687402816,16.1708335669039));
#142499=CARTESIAN_POINT('Ctrl Pts',(16.1778897355288,19.3745927743499,16.1749572435793));
#142500=CARTESIAN_POINT('Ctrl Pts',(16.185851592152,19.4570481489095,16.1790809202548));
#142501=CARTESIAN_POINT('Ctrl Pts',(16.193849980064,19.5398818524496,16.1832235175451));
#142502=CARTESIAN_POINT('Ctrl Pts',(16.2059033176551,19.6224439445466,16.1873661148355));
#142503=CARTESIAN_POINT('Ctrl Pts',(16.2219780566694,19.7043008779901,16.1915087121259));
#142504=CARTESIAN_POINT('Ctrl Pts',(16.23794569149,19.7856124078128,16.1956237077524));
#142505=CARTESIAN_POINT('Ctrl Pts',(16.2578812222445,19.8662276743518,16.1997387033789));
#142506=CARTESIAN_POINT('Ctrl Pts',(16.2816998746989,19.9457272251988,16.2038536990054));
#142507=CARTESIAN_POINT('Ctrl Pts',(16.3055083094403,20.0251926723702,16.2079669293832));
#142508=CARTESIAN_POINT('Ctrl Pts',(16.33319642467,20.1035429002386,16.2120801597611));
#142509=CARTESIAN_POINT('Ctrl Pts',(16.3646289972004,20.1803714721883,16.2161933901389));
#142510=CARTESIAN_POINT('Ctrl Pts',(16.3960581246075,20.2571916234494,16.2203061696919));
#142511=CARTESIAN_POINT('Ctrl Pts',(16.4312307139715,20.3324900117992,16.2244189492448));
#142512=CARTESIAN_POINT('Ctrl Pts',(16.469963164482,20.405879578626,16.2285317287978));
#142513=CARTESIAN_POINT('Ctrl Pts',(16.5091807554344,20.48018838104,16.2326960226666));
#142514=CARTESIAN_POINT('Ctrl Pts',(16.5520477937182,20.552539761255,16.2368603165354));
#142515=CARTESIAN_POINT('Ctrl Pts',(16.5983263505016,20.6225587351713,16.2410246104042));
#142516=CARTESIAN_POINT('Ctrl Pts',(16.6440925485817,20.6918025157112,16.2451428005837));
#142517=CARTESIAN_POINT('Ctrl Pts',(16.6931947649456,20.7587649302322,16.2492609907631));
#142518=CARTESIAN_POINT('Ctrl Pts',(16.7453611252724,20.8231152024351,16.2533791809425));
#142519=CARTESIAN_POINT('Ctrl Pts',(16.7984034996618,20.8885460894828,16.257566526656));
#142520=CARTESIAN_POINT('Ctrl Pts',(16.8546135316783,20.9512759179513,16.2617538723695));
#142521=CARTESIAN_POINT('Ctrl Pts',(16.9136665630956,21.010996160687,16.265941218083));
#142522=CARTESIAN_POINT('Ctrl Pts',(16.972719594513,21.0707164034227,16.2701285637965));
#142523=CARTESIAN_POINT('Ctrl Pts',(17.0346152026565,21.1274267716985,16.2743159095101));
#142524=CARTESIAN_POINT('Ctrl Pts',(17.0989955289249,21.1808630357374,16.2785032552236));
#142525=CARTESIAN_POINT('Ctrl Pts',(17.1633341687151,21.2342646996152,16.2826878896166));
#142526=CARTESIAN_POINT('Ctrl Pts',(17.2304115572045,21.2846103343966,16.2868725240096));
#142527=CARTESIAN_POINT('Ctrl Pts',(17.29990527078,21.3316065895454,16.2910571584027));
#142528=CARTESIAN_POINT('Ctrl Pts',(17.3693000686558,21.378535951342,16.2952358364866));
#142529=CARTESIAN_POINT('Ctrl Pts',(17.4411039821925,21.4221251476138,16.2994145145706));
#142530=CARTESIAN_POINT('Ctrl Pts',(17.5149611920068,21.4621206952553,16.3035931926545));
#142531=CARTESIAN_POINT('Ctrl Pts',(17.5901422392269,21.5028331343439,16.30784677054));
#142532=CARTESIAN_POINT('Ctrl Pts',(17.6674505464319,21.5398215173808,16.3121003484254));
#142533=CARTESIAN_POINT('Ctrl Pts',(17.7464794551571,21.5728643427414,16.3163539263108));
#142534=CARTESIAN_POINT('Ctrl Pts',(17.8239762342744,21.6052665684546,16.3205250402888));
#142535=CARTESIAN_POINT('Ctrl Pts',(17.9031270518499,21.6338746703221,16.3246961542667));
#142536=CARTESIAN_POINT('Ctrl Pts',(17.983524818815,21.6585267112792,16.3288672682447));
#142537=CARTESIAN_POINT('Ctrl Pts',(18.0638956075329,21.6831704800059,16.3330369825651));
#142538=CARTESIAN_POINT('Ctrl Pts',(18.1455120751846,21.7038606894987,16.3372066968854));
#142539=CARTESIAN_POINT('Ctrl Pts',(18.2279505020329,21.7204847888774,16.3413764112058));
#142540=CARTESIAN_POINT('Ctrl Pts',(18.3103859953682,21.7371082966994,16.3455459771499));
#142541=CARTESIAN_POINT('Ctrl Pts',(18.3936429386223,21.7496658919856,16.3497155430939));
#142542=CARTESIAN_POINT('Ctrl Pts',(18.4772872562561,21.758096104822,16.353885109038));
#142543=CARTESIAN_POINT('Ctrl Pts',(18.5638724049115,21.7668227135419,16.3582012717769));
#142544=CARTESIAN_POINT('Ctrl Pts',(18.6508721501767,21.7711262492444,16.3625174345158));
#142545=CARTESIAN_POINT('Ctrl Pts',(18.7378010569183,21.7709971781169,16.3668335972547));
#142546=CARTESIAN_POINT('Ctrl Pts',(18.821898263666,21.7708723114677,16.3710091614464));
#142547=CARTESIAN_POINT('Ctrl Pts',(18.9059287081101,21.7665992585964,16.3751847256381));
#142548=CARTESIAN_POINT('Ctrl Pts',(18.9894564259429,21.7582224116564,16.3793602898298));
#142549=CARTESIAN_POINT('Ctrl Pts',(19.0772029302352,21.7494224700914,16.3837467518423));
#142550=CARTESIAN_POINT('Ctrl Pts',(19.1643940106307,21.7360933624401,16.3881332138548));
#142551=CARTESIAN_POINT('Ctrl Pts',(19.2505367177894,21.7183471676605,16.3925196758674));
#142552=CARTESIAN_POINT('Ctrl Pts',(19.3366794249481,21.700600972881,16.3969061378799));
#142553=CARTESIAN_POINT('Ctrl Pts',(19.4217732165569,21.6784379108237,16.4012925998925));
#142554=CARTESIAN_POINT('Ctrl Pts',(19.5053461655911,21.652029514944,16.405679061905));
#142555=CARTESIAN_POINT('Ctrl Pts',(19.5850737993555,21.6268362085053,16.4098636962981));
#142556=CARTESIAN_POINT('Ctrl Pts',(19.6637142290032,21.5976858772393,16.4140483306911));
#142557=CARTESIAN_POINT('Ctrl Pts',(19.7408462713707,21.5646908432984,16.4182329650842));
#142558=CARTESIAN_POINT('Ctrl Pts',(19.817868525823,21.5317427737044,16.4224116431681));
#142559=CARTESIAN_POINT('Ctrl Pts',(19.8933862382763,21.4949610508431,16.4265903212521));
#142560=CARTESIAN_POINT('Ctrl Pts',(19.96699367127,21.4545076569087,16.430768999336));
#142561=CARTESIAN_POINT('Ctrl Pts',(20.0419204645992,21.4133291649615,16.4350225772215));
#142562=CARTESIAN_POINT('Ctrl Pts',(20.1148673616167,21.3683462231047,16.4392761551069));
#142563=CARTESIAN_POINT('Ctrl Pts',(20.1854279979956,21.3197808721237,16.4435297329923));
#142564=CARTESIAN_POINT('Ctrl Pts',(20.2546206787505,21.2721570552389,16.4477008469703));
#142565=CARTESIAN_POINT('Ctrl Pts',(20.3215184014305,21.2210887664917,16.4518719609482));
#142566=CARTESIAN_POINT('Ctrl Pts',(20.3857646529993,21.1668306499036,16.4560430749262));
#142567=CARTESIAN_POINT('Ctrl Pts',(20.4499893461179,21.1125907401505,16.4602127892466));
#142568=CARTESIAN_POINT('Ctrl Pts',(20.5115639839658,21.055163424919,16.4643825035669));
#142569=CARTESIAN_POINT('Ctrl Pts',(20.5701645776071,20.9948440637962,16.4685522178873));
#142570=CARTESIAN_POINT('Ctrl Pts',(20.6287630859878,20.9345268490952,16.4727217838314));
#142571=CARTESIAN_POINT('Ctrl Pts',(20.6843874406314,20.8713181236703,16.4768913497754));
#142572=CARTESIAN_POINT('Ctrl Pts',(20.7367509982118,20.8055496038573,16.4810609157195));
#142573=CARTESIAN_POINT('Ctrl Pts',(20.7909555938794,20.7374687440219,16.4853770784584));
#142574=CARTESIAN_POINT('Ctrl Pts',(20.8416654983873,20.6666451485148,16.4896932411973));
#142575=CARTESIAN_POINT('Ctrl Pts',(20.888609938477,20.5934818309896,16.4940094039362));
#142576=CARTESIAN_POINT('Ctrl Pts',(20.9340251683684,20.5227018008373,16.4981849681279));
#142577=CARTESIAN_POINT('Ctrl Pts',(20.9759162929432,20.4497325726915,16.5023605323196));
#142578=CARTESIAN_POINT('Ctrl Pts',(21.0140846597658,20.3749647521729,16.5065360965113));
#142579=CARTESIAN_POINT('Ctrl Pts',(21.0541808200599,20.2964205867835,16.5109225585238));
#142580=CARTESIAN_POINT('Ctrl Pts',(21.0901680280105,20.2158918932934,16.5153090205363));
#142581=CARTESIAN_POINT('Ctrl Pts',(21.1218737001564,20.133853830301,16.5196954825489));
#142582=CARTESIAN_POINT('Ctrl Pts',(21.1535793723023,20.0518157673086,16.5240819445614));
#142583=CARTESIAN_POINT('Ctrl Pts',(21.1810033999592,19.9682689098143,16.5284684065739));
#142584=CARTESIAN_POINT('Ctrl Pts',(21.2040345704695,19.8837029215676,16.5328548685865));
#142585=CARTESIAN_POINT('Ctrl Pts',(21.2260060426842,19.8030279397969,16.5370395029795));
#142586=CARTESIAN_POINT('Ctrl Pts',(21.244061800264,19.7211252621464,16.5412241373726));
#142587=CARTESIAN_POINT('Ctrl Pts',(21.2580683099057,19.6384098348539,16.5454087717656));
#142588=CARTESIAN_POINT('Ctrl Pts',(21.2720548830145,19.5558121427341,16.5495874498496));
#142589=CARTESIAN_POINT('Ctrl Pts',(21.2820035803663,19.4724044485339,16.5537661279335));
#142590=CARTESIAN_POINT('Ctrl Pts',(21.28783098536,19.3886155911379,16.5579448060175));
#142591=CARTESIAN_POINT('Ctrl Pts',(21.2937628424001,19.3033248786909,16.5621983839029));
#142592=CARTESIAN_POINT('Ctrl Pts',(21.2954240788116,19.2176396691378,16.5664519617883));
#142593=CARTESIAN_POINT('Ctrl Pts',(21.2927814384536,19.1320218370346,16.5707055396738));
#142594=CARTESIAN_POINT('Ctrl Pts',(21.2901900308356,19.0480638736762,16.5748766536517));
#142595=CARTESIAN_POINT('Ctrl Pts',(21.2834601502021,18.9641711795844,16.5790477676297));
#142596=CARTESIAN_POINT('Ctrl Pts',(21.2726129381323,18.8807813597822,16.5832188816076));
#142597=CARTESIAN_POINT('Ctrl Pts',(21.2617693659493,18.7974195222394,16.587388595928));
#142598=CARTESIAN_POINT('Ctrl Pts',(21.246811265521,18.7145606796674,16.5915583102484));
#142599=CARTESIAN_POINT('Ctrl Pts',(21.2278116184524,18.6326371280314,16.5957280245688));
#142600=CARTESIAN_POINT('Ctrl Pts',(21.2088126474729,18.5507164915871,16.5998975905128));
#142601=CARTESIAN_POINT('Ctrl Pts',(21.1857725205575,18.4697315278525,16.6040671564568));
#142602=CARTESIAN_POINT('Ctrl Pts',(21.1588150040536,18.3901028102639,16.6082367224009));
#142603=CARTESIAN_POINT('Ctrl Pts',(21.130909694525,18.3076744451973,16.6125528851398));
#142604=CARTESIAN_POINT('Ctrl Pts',(21.0988065683012,18.2266999715503,16.6168690478787));
#142605=CARTESIAN_POINT('Ctrl Pts',(21.0626979316574,18.1476252104292,16.6211852106176));
#142606=CARTESIAN_POINT('Ctrl Pts',(21.0277655300543,18.0711263013345,16.6253607748093));
#142607=CARTESIAN_POINT('Ctrl Pts',(20.9890848280187,17.9964056357569,16.629536339001));
#142608=CARTESIAN_POINT('Ctrl Pts',(20.9468767362674,17.9238416763713,16.6337119031927));
#142609=CARTESIAN_POINT('Ctrl Pts',(20.9025368141419,17.8476126839014,16.6380983652052));
#142610=CARTESIAN_POINT('Ctrl Pts',(20.854304119971,17.7737644826753,16.6424848272177));
#142611=CARTESIAN_POINT('Ctrl Pts',(20.8024847707863,17.7026993824091,16.6468712892303));
#142612=CARTESIAN_POINT('Ctrl Pts',(20.7506654216016,17.6316342821429,16.6512577512428));
#142613=CARTESIAN_POINT('Ctrl Pts',(20.6952598420585,17.5633526854597,16.6556442132554));
#142614=CARTESIAN_POINT('Ctrl Pts',(20.6366195645773,17.4982131503051,16.6600306752679));
#142615=CARTESIAN_POINT('Ctrl Pts',(20.5806916320437,17.4360865764914,16.6642142460496));
#142616=CARTESIAN_POINT('Ctrl Pts',(20.5216135032554,17.3765866334633,16.6683978168312));
#142617=CARTESIAN_POINT('Ctrl Pts',(20.459661587099,17.320049951265,16.6725813876129));
#142618=CARTESIAN_POINT('Ctrl Pts',(20.40634711204,17.2713957090722,16.6761816778691));
#142619=CARTESIAN_POINT('Ctrl Pts',(20.3509051344092,17.2249357340853,16.6797819681254));
#142620=CARTESIAN_POINT('Ctrl Pts',(20.2935357313021,17.1808649545431,16.6833822583817));
#142621=CARTESIAN_POINT('Origin',(18.734,19.211,-1.76670989022852));
#142622=CARTESIAN_POINT('',(20.2961055602205,17.1775141780511,17.5498940766593));
#142623=CARTESIAN_POINT('',(20.2910030380574,17.1841723135106,17.4833253062578));
#142624=CARTESIAN_POINT('',(20.2935357313021,17.1808649545432,-1.76670989022852));
#142625=CARTESIAN_POINT('',(16.1737370555978,19.211835565301,17.0332901097715));
#142626=CARTESIAN_POINT('Ctrl Pts',(16.1700998775752,19.2118367523274,17.0332901097715));
#142627=CARTESIAN_POINT('Ctrl Pts',(16.1699051698649,19.2575742435185,17.0355745863224));
#142628=CARTESIAN_POINT('Ctrl Pts',(16.1917620114795,20.1518505208751,17.0802509984337));
#142629=CARTESIAN_POINT('Ctrl Pts',(17.2348044634258,21.8407724883182,17.1673193461055));
#142630=CARTESIAN_POINT('Ctrl Pts',(20.1337363827015,21.8950321637681,17.2944951527869));
#142631=CARTESIAN_POINT('Ctrl Pts',(21.7484970482859,19.4868589187841,17.4216709594684));
#142632=CARTESIAN_POINT('Ctrl Pts',(20.978102385576,17.7053825246215,17.5068039340925));
#142633=CARTESIAN_POINT('Ctrl Pts',(20.301649822008,17.1817662346287,17.5495449731561));
#142634=CARTESIAN_POINT('Ctrl Pts',(20.2961055602205,17.1775141780511,17.5498940766593));
#142635=CARTESIAN_POINT('Ctrl Pts',(20.2935357313021,17.1808649545432,16.7498176665395));
#142636=CARTESIAN_POINT('Ctrl Pts',(20.226858468591,17.1296439414898,16.7539938197931));
#142637=CARTESIAN_POINT('Ctrl Pts',(20.1577087704231,17.0817524478804,16.7581699730466));
#142638=CARTESIAN_POINT('Ctrl Pts',(20.0864599566968,17.0374195286276,16.7623461263002));
#142639=CARTESIAN_POINT('Ctrl Pts',(20.0150847693762,16.9930079763412,16.7665296867718));
#142640=CARTESIAN_POINT('Ctrl Pts',(19.9416034309245,16.952167832392,16.7707132472434));
#142641=CARTESIAN_POINT('Ctrl Pts',(19.8664139286561,16.9150821673706,16.7748968077149));
#142642=CARTESIAN_POINT('Ctrl Pts',(19.8011426897056,16.8828884803502,16.7785285138304));
#142643=CARTESIAN_POINT('Ctrl Pts',(19.7345847399538,16.8535234039901,16.7821602199458));
#142644=CARTESIAN_POINT('Ctrl Pts',(19.6670104728629,16.8270764572814,16.7857919260613));
#142645=CARTESIAN_POINT('Ctrl Pts',(19.5891480046,16.7966029554973,16.7899765604543));
#142646=CARTESIAN_POINT('Ctrl Pts',(19.5096461031212,16.7698914102528,16.7941611948473));
#142647=CARTESIAN_POINT('Ctrl Pts',(19.4289030536308,16.7471189667408,16.7983458292404));
#142648=CARTESIAN_POINT('Ctrl Pts',(19.3482749318773,16.7243789369834,16.8025245073243));
#142649=CARTESIAN_POINT('Ctrl Pts',(19.2664096101499,16.7055669958483,16.8067031854083));
#142650=CARTESIAN_POINT('Ctrl Pts',(19.1837245465113,16.6908119450594,16.8108818634922));
#142651=CARTESIAN_POINT('Ctrl Pts',(19.0995574125318,16.6757924205894,16.8151354413777));
#142652=CARTESIAN_POINT('Ctrl Pts',(19.0145413088147,16.66497683224,16.8193890192631));
#142653=CARTESIAN_POINT('Ctrl Pts',(18.929131904193,16.6584476420716,16.8236425971485));
#142654=CARTESIAN_POINT('Ctrl Pts',(18.8453783275426,16.6520450329952,16.8278137111265));
#142655=CARTESIAN_POINT('Ctrl Pts',(18.7612470435307,16.6497641415373,16.8319848251044));
#142656=CARTESIAN_POINT('Ctrl Pts',(18.6771754083917,16.6516307484483,16.8361559390824));
#142657=CARTESIAN_POINT('Ctrl Pts',(18.5931319843017,16.6534967290012,16.8403256534028));
#142658=CARTESIAN_POINT('Ctrl Pts',(18.5091486288698,16.6595074337161,16.8444953677231));
#142659=CARTESIAN_POINT('Ctrl Pts',(18.4256629639196,16.6696365328468,16.8486650820435));
#142660=CARTESIAN_POINT('Ctrl Pts',(18.3421802697477,16.6797652715406,16.8528346479875));
#142661=CARTESIAN_POINT('Ctrl Pts',(18.2591956874269,16.6940120570168,16.8570042139316));
#142662=CARTESIAN_POINT('Ctrl Pts',(18.1771406148226,16.7122988123547,16.8611737798756));
#142663=CARTESIAN_POINT('Ctrl Pts',(18.0922005870915,16.7312285074512,16.8654899426145));
#142664=CARTESIAN_POINT('Ctrl Pts',(18.008257163138,16.7544874341396,16.8698061053535));
#142665=CARTESIAN_POINT('Ctrl Pts',(17.9257741739148,16.781932068869,16.8741222680924));
#142666=CARTESIAN_POINT('Ctrl Pts',(17.8459780593899,16.8084826975088,16.878297832284));
#142667=CARTESIAN_POINT('Ctrl Pts',(17.7675491154086,16.838950308513,16.8824733964757));
#142668=CARTESIAN_POINT('Ctrl Pts',(17.6908872600139,16.8731557340835,16.8866489606674));
#142669=CARTESIAN_POINT('Ctrl Pts',(17.6103533965496,16.9090887943838,16.8910354226799));
#142670=CARTESIAN_POINT('Ctrl Pts',(17.5317703445184,16.9491469214588,16.8954218846925));
#142671=CARTESIAN_POINT('Ctrl Pts',(17.4555708448952,16.9930687802869,16.899808346705));
#142672=CARTESIAN_POINT('Ctrl Pts',(17.3793713452719,17.0369906391151,16.9041948087175));
#142673=CARTESIAN_POINT('Ctrl Pts',(17.3055558437866,17.0847758505362,16.9085812707301));
#142674=CARTESIAN_POINT('Ctrl Pts',(17.2345184376722,17.1361132454423,16.9129677327426));
#142675=CARTESIAN_POINT('Ctrl Pts',(17.167299168743,17.1846913445463,16.9171184300414));
#142676=CARTESIAN_POINT('Ctrl Pts',(17.1023079512147,17.2366370916662,16.9212691273401));
#142677=CARTESIAN_POINT('Ctrl Pts',(17.0399060592653,17.2917173944502,16.9254198246388));
#142678=CARTESIAN_POINT('Ctrl Pts',(16.9775932241692,17.3467190893861,16.9295645982704));
#142679=CARTESIAN_POINT('Ctrl Pts',(16.9178627255451,17.4048461509352,16.9337093719019));
#142680=CARTESIAN_POINT('Ctrl Pts',(16.8610458812396,17.4658229691466,16.9378541455334));
#142681=CARTESIAN_POINT('Ctrl Pts',(16.8042942087153,17.5267298438772,16.9419941649009));
#142682=CARTESIAN_POINT('Ctrl Pts',(16.7504498675423,17.5904796396564,16.9461341842684));
#142683=CARTESIAN_POINT('Ctrl Pts',(16.6998090154256,17.6567583719781,16.9502742036359));
#142684=CARTESIAN_POINT('Ctrl Pts',(16.6491995836851,17.7229959813207,16.9544116543072));
#142685=CARTESIAN_POINT('Ctrl Pts',(16.6017899801563,17.7917590422704,16.9585491049784));
#142686=CARTESIAN_POINT('Ctrl Pts',(16.5578367768805,17.8626997269368,16.9626865556497));
#142687=CARTESIAN_POINT('Ctrl Pts',(16.5138971231854,17.9336185425139,16.9668227308571));
#142688=CARTESIAN_POINT('Ctrl Pts',(16.473412000563,18.0067132510728,16.9709589060645));
#142689=CARTESIAN_POINT('Ctrl Pts',(16.436594403761,18.0816074524907,16.9750950812719));
#142690=CARTESIAN_POINT('Ctrl Pts',(16.3997766632185,18.1565019463048,16.9792312726275));
#142691=CARTESIAN_POINT('Ctrl Pts',(16.3666266817619,18.2331955257885,16.983367463983));
#142692=CARTESIAN_POINT('Ctrl Pts',(16.3373106052885,18.3112889656799,16.9875036553386));
#142693=CARTESIAN_POINT('Ctrl Pts',(16.3079666664254,18.3894566266172,16.9916437777855));
#142694=CARTESIAN_POINT('Ctrl Pts',(16.2824640727846,18.4690263650884,16.9957839002324));
#142695=CARTESIAN_POINT('Ctrl Pts',(16.2609198329123,18.5495814584111,16.9999240226793));
#142696=CARTESIAN_POINT('Ctrl Pts',(16.2393648184701,18.6301768384414,17.0040662156583));
#142697=CARTESIAN_POINT('Ctrl Pts',(16.2217721969232,18.711758096276,17.0082084086373));
#142698=CARTESIAN_POINT('Ctrl Pts',(16.2082078057625,18.7938983438913,17.0123506016163));
#142699=CARTESIAN_POINT('Ctrl Pts',(16.194621013815,18.8761742412484,17.016499635181));
#142700=CARTESIAN_POINT('Ctrl Pts',(16.1850757885661,18.9590105062903,17.0206486687458));
#142701=CARTESIAN_POINT('Ctrl Pts',(16.1795860271471,19.0419755778186,17.0247977023105));
#142702=CARTESIAN_POINT('Ctrl Pts',(16.1758404729028,19.0985809841505,17.0276285047975));
#142703=CARTESIAN_POINT('Ctrl Pts',(16.1739816679355,19.1552463005709,17.0304593072845));
#142704=CARTESIAN_POINT('Ctrl Pts',(16.1740001363332,19.2118354794422,17.0332901097715));
#142705=CARTESIAN_POINT('',(16.1741505176752,19.209803254934,16.9667098397549));
#142706=CARTESIAN_POINT('Ctrl Pts',(20.2935357313021,17.1808649545431,16.6833822583817));
#142707=CARTESIAN_POINT('Ctrl Pts',(20.2246022413362,17.1279107232836,16.687708267697));
#142708=CARTESIAN_POINT('Ctrl Pts',(20.1528852221898,17.0784073718384,16.6920342770124));
#142709=CARTESIAN_POINT('Ctrl Pts',(20.0787694878185,17.0326531440948,16.6963602863277));
#142710=CARTESIAN_POINT('Ctrl Pts',(20.0073031354739,16.988534472278,16.7005316557217));
#142711=CARTESIAN_POINT('Ctrl Pts',(19.9336070721956,16.9479017083688,16.7047030251158));
#142712=CARTESIAN_POINT('Ctrl Pts',(19.8580574417036,16.9109793766684,16.7088743945098));
#142713=CARTESIAN_POINT('Ctrl Pts',(19.7825359166057,16.8740707805306,16.7130442121031));
#142714=CARTESIAN_POINT('Ctrl Pts',(19.7051626065606,16.8408700772147,16.7172140296963));
#142715=CARTESIAN_POINT('Ctrl Pts',(19.6263379519364,16.8115556935961,16.7213838472895));
#142716=CARTESIAN_POINT('Ctrl Pts',(19.5475189755514,16.7822434216783,16.7255533645043));
#142717=CARTESIAN_POINT('Ctrl Pts',(19.4672492937651,16.7568170727964,16.7297228817192));
#142718=CARTESIAN_POINT('Ctrl Pts',(19.3859477207409,16.7354062996079,16.733892398934));
#142719=CARTESIAN_POINT('Ctrl Pts',(19.3046276162901,16.7139906461674,16.7380628665253));
#142720=CARTESIAN_POINT('Ctrl Pts',(19.2222755986575,16.6965925017586,16.7422333341166));
#142721=CARTESIAN_POINT('Ctrl Pts',(19.1393226393413,16.6832908478155,16.7464038017079));
#142722=CARTESIAN_POINT('Ctrl Pts',(19.0562756193694,16.6699741110796,16.7505789982072));
#142723=CARTESIAN_POINT('Ctrl Pts',(18.9726267529364,16.6607632053402,16.7547541947066));
#142724=CARTESIAN_POINT('Ctrl Pts',(18.8888135568868,16.6556853887233,16.7589293912059));
#142725=CARTESIAN_POINT('Ctrl Pts',(18.8049436062157,16.6506041336317,16.7631074149653));
#142726=CARTESIAN_POINT('Ctrl Pts',(18.7209095638014,16.6496615421292,16.7672854387246));
#142727=CARTESIAN_POINT('Ctrl Pts',(18.6371480049381,16.6528327476389,16.771463462484));
#142728=CARTESIAN_POINT('Ctrl Pts',(18.5532533714703,16.6560089913419,16.7756481240001));
#142729=CARTESIAN_POINT('Ctrl Pts',(18.4696325420907,16.6633120309538,16.7798327855163));
#142730=CARTESIAN_POINT('Ctrl Pts',(18.3867154598213,16.6746653517028,16.7840174470325));
#142731=CARTESIAN_POINT('Ctrl Pts',(18.3656523886079,16.677549387138,16.7850804586714));
#142732=CARTESIAN_POINT('Ctrl Pts',(18.3446346664914,16.68069452864,16.7861434703104));
#142733=CARTESIAN_POINT('Ctrl Pts',(18.3236691980735,16.6840990060965,16.7872064819493));
#142734=CARTESIAN_POINT('Ctrl Pts',(18.2411368748191,16.6975010168866,16.7913911163424));
#142735=CARTESIAN_POINT('Ctrl Pts',(18.1591082470636,16.7149756618514,16.7955757507354));
#142736=CARTESIAN_POINT('Ctrl Pts',(18.078016311923,16.7364726914061,16.7997603851285));
#142737=CARTESIAN_POINT('Ctrl Pts',(17.9970398011148,16.7579391226001,16.8039390632124));
#142738=CARTESIAN_POINT('Ctrl Pts',(17.9169977755058,16.7834164491321,16.8081177412964));
#142739=CARTESIAN_POINT('Ctrl Pts',(17.8383151283773,16.8128030500507,16.8122964193803));
#142740=CARTESIAN_POINT('Ctrl Pts',(17.7582221513472,16.8427163846709,16.8165499972657));
#142741=CARTESIAN_POINT('Ctrl Pts',(17.679538241764,16.8766804423687,16.8208035751512));
#142742=CARTESIAN_POINT('Ctrl Pts',(17.6026975961517,16.9145342652138,16.8250571530366));
#142743=CARTESIAN_POINT('Ctrl Pts',(17.5273466563967,16.9516542178374,16.8292282670146));
#142744=CARTESIAN_POINT('Ctrl Pts',(17.4537685795461,16.9925142474789,16.8333993809925));
#142745=CARTESIAN_POINT('Ctrl Pts',(17.3823529481856,17.0369139282629,16.8375704949705));
#142746=CARTESIAN_POINT('Ctrl Pts',(17.31096128103,17.081298710305,16.8417402092909));
#142747=CARTESIAN_POINT('Ctrl Pts',(17.2417310086119,17.1292205418818,16.8459099236112));
#142748=CARTESIAN_POINT('Ctrl Pts',(17.1750254175662,17.1804340071484,16.8500796379316));
#142749=CARTESIAN_POINT('Ctrl Pts',(17.1083222001916,17.2316456500202,16.8542492038756));
#142750=CARTESIAN_POINT('Ctrl Pts',(17.0441438499409,17.2861484128722,16.8584187698197));
#142751=CARTESIAN_POINT('Ctrl Pts',(16.9828219564696,17.3436555058434,16.8625883357637));
#142752=CARTESIAN_POINT('Ctrl Pts',(16.9193440608726,17.4031844772607,16.8669044985027));
#142753=CARTESIAN_POINT('Ctrl Pts',(16.8589276101184,17.465932613281,16.8712206612416));
#142754=CARTESIAN_POINT('Ctrl Pts',(16.8018987983272,17.5315402813719,16.8755368239805));
#142755=CARTESIAN_POINT('Ctrl Pts',(16.7467276940818,17.5950107865753,16.8797123881722));
#142756=CARTESIAN_POINT('Ctrl Pts',(16.6947271674386,17.6611569867925,16.8838879523639));
#142757=CARTESIAN_POINT('Ctrl Pts',(16.6461502555165,17.7296211003055,16.8880635165556));
#142758=CARTESIAN_POINT('Ctrl Pts',(16.5951198392538,17.8015431734341,16.8924499785681));
#142759=CARTESIAN_POINT('Ctrl Pts',(16.5478682932595,17.8760229761491,16.8968364405806));
#142760=CARTESIAN_POINT('Ctrl Pts',(16.5046350837973,17.9526152931617,16.9012229025932));
#142761=CARTESIAN_POINT('Ctrl Pts',(16.461401874335,18.0292076101744,16.9056093646057));
#142762=CARTESIAN_POINT('Ctrl Pts',(16.4221871920777,18.1079118882384,16.9099958266183));
#142763=CARTESIAN_POINT('Ctrl Pts',(16.3871718743353,18.1882596866316,16.9143822886308));
#142764=CARTESIAN_POINT('Ctrl Pts',(16.3503471043862,18.272759539339,16.9189954255354));
#142765=CARTESIAN_POINT('Ctrl Pts',(16.3180481684135,18.3593459986726,16.9236085624399));
#142766=CARTESIAN_POINT('Ctrl Pts',(16.2904920397068,18.4475415217682,16.9282216993445));
#142767=CARTESIAN_POINT('Ctrl Pts',(16.2630147812854,18.5354846144106,16.9328216326736));
#142768=CARTESIAN_POINT('Ctrl Pts',(16.240253377301,18.6250273148911,16.9374215660027));
#142769=CARTESIAN_POINT('Ctrl Pts',(16.2223767943066,18.7156729639699,16.9420214993319));
#142770=CARTESIAN_POINT('Ctrl Pts',(16.2045882581335,18.8058721596483,16.9465987767929));
#142771=CARTESIAN_POINT('Ctrl Pts',(16.1916366671697,18.8971631896627,16.9511760542538));
#142772=CARTESIAN_POINT('Ctrl Pts',(16.1836406660146,18.9890376888893,16.9557533317148));
#142773=CARTESIAN_POINT('Ctrl Pts',(16.1772607284144,19.0623435277384,16.9594055003442));
#142774=CARTESIAN_POINT('Ctrl Pts',(16.174034774907,19.1360203999197,16.9630576689737));
#142775=CARTESIAN_POINT('Ctrl Pts',(16.1740002797795,19.2098031412859,16.9667098376031));
#142776=CARTESIAN_POINT('Ctrl Pts',(16.1776746320478,19.209805920766,16.9667098902285));
#142777=CARTESIAN_POINT('Ctrl Pts',(16.1797896414426,19.7131225343252,16.9916592919231));
#142778=CARTESIAN_POINT('Ctrl Pts',(16.5671403882425,21.07463612297,17.0590006291781));
#142779=CARTESIAN_POINT('Ctrl Pts',(18.7821183121777,22.2377105261597,17.1687339019936));
#142780=CARTESIAN_POINT('Ctrl Pts',(21.3050300949207,20.8088411160513,17.2959097086751));
#142781=CARTESIAN_POINT('Ctrl Pts',(21.4403822833153,18.4219199310893,17.4007735100965));
#142782=CARTESIAN_POINT('Ctrl Pts',(20.61274935573,17.4306044799469,17.4632453759574));
#142783=CARTESIAN_POINT('Ctrl Pts',(20.2910030380574,17.1841723135106,17.4833253062578));
#142784=CARTESIAN_POINT('Origin',(18.734,19.211,-1.76670989022852));
#142785=CARTESIAN_POINT('',(20.2935357313021,17.1808649545432,18.3499540490682));
#142786=CARTESIAN_POINT('',(20.2935357313021,17.1808649545431,18.283231856284));
#142787=CARTESIAN_POINT('',(20.2935357313021,17.1808649545432,-1.76670989022852));
#142788=CARTESIAN_POINT('',(16.1740010840393,19.2086440968075,17.8332901097715));
#142789=CARTESIAN_POINT('Ctrl Pts',(16.1740010840393,19.2086440968075,17.8332901097715));
#142790=CARTESIAN_POINT('Ctrl Pts',(16.1739248258781,19.2915086264566,17.837412174938));
#142791=CARTESIAN_POINT('Ctrl Pts',(16.177876160498,19.3744847533445,17.8415342401044));
#142792=CARTESIAN_POINT('Ctrl Pts',(16.1858608731257,19.4571442465142,17.8456563052709));
#142793=CARTESIAN_POINT('Ctrl Pts',(16.1938402258665,19.5397482529614,17.8497756034244));
#142794=CARTESIAN_POINT('Ctrl Pts',(16.205847540348,19.6220355783689,17.853894901578));
#142795=CARTESIAN_POINT('Ctrl Pts',(16.2218365582967,19.7035797825425,17.8580141997315));
#142796=CARTESIAN_POINT('Ctrl Pts',(16.2378199266111,19.7850951735058,17.862132042353));
#142797=CARTESIAN_POINT('Ctrl Pts',(16.2577821151893,19.8658675009388,17.8662498849745));
#142798=CARTESIAN_POINT('Ctrl Pts',(16.2816254461127,19.9454787590162,17.8703677275959));
#142799=CARTESIAN_POINT('Ctrl Pts',(16.3054679320359,20.0250871956956,17.8744854242824));
#142800=CARTESIAN_POINT('Ctrl Pts',(16.3331911499574,20.1035341923719,17.8786031209688));
#142801=CARTESIAN_POINT('Ctrl Pts',(16.364647494651,20.1804166830608,17.8827208176552));
#142802=CARTESIAN_POINT('Ctrl Pts',(16.396133878009,20.257372591286,17.8868424464612));
#142803=CARTESIAN_POINT('Ctrl Pts',(16.4313603282317,20.3327605713697,17.8909640752672));
#142804=CARTESIAN_POINT('Ctrl Pts',(16.4701312380089,20.4061979871474,17.8950857040732));
#142805=CARTESIAN_POINT('Ctrl Pts',(16.5089205032735,20.479670170733,17.8992092842006));
#142806=CARTESIAN_POINT('Ctrl Pts',(16.5512573267502,20.5511895451374,17.903332864328));
#142807=CARTESIAN_POINT('Ctrl Pts',(16.5969016205558,20.6204007650689,17.9074564444553));
#142808=CARTESIAN_POINT('Ctrl Pts',(16.6426258760309,20.6897332322415,17.9115872484507));
#142809=CARTESIAN_POINT('Ctrl Pts',(16.6916688941171,20.7567490876318,17.915718052446));
#142810=CARTESIAN_POINT('Ctrl Pts',(16.743749207993,20.8211247730892,17.9198488564413));
#142811=CARTESIAN_POINT('Ctrl Pts',(16.7879829276106,20.8758014024869,17.9233572996922));
#142812=CARTESIAN_POINT('Ctrl Pts',(16.8344068718463,20.9285739549632,17.9268657429432));
#142813=CARTESIAN_POINT('Ctrl Pts',(16.8828286089276,20.979265953095,17.9303741861941));
#142814=CARTESIAN_POINT('Ctrl Pts',(16.9405827898753,21.039727948248,17.9345588205871));
#142815=CARTESIAN_POINT('Ctrl Pts',(17.0014097311532,21.0974699797563,17.9387434549801));
#142816=CARTESIAN_POINT('Ctrl Pts',(17.0650229727701,21.152163486824,17.9429280893731));
#142817=CARTESIAN_POINT('Ctrl Pts',(17.1285456688113,21.2067791444541,17.947106767457));
#142818=CARTESIAN_POINT('Ctrl Pts',(17.1948464417153,21.2583545993042,17.9512854455409));
#142819=CARTESIAN_POINT('Ctrl Pts',(17.2636010628233,21.3065970427421,17.9554641236248));
#142820=CARTESIAN_POINT('Ctrl Pts',(17.3335880611026,21.3557041973082,17.9597177015102));
#142821=CARTESIAN_POINT('Ctrl Pts',(17.4061174102899,21.4013573280785,17.9639712793957));
#142822=CARTESIAN_POINT('Ctrl Pts',(17.4808106950311,21.4432895345164,17.9682248572811));
#142823=CARTESIAN_POINT('Ctrl Pts',(17.5540559046944,21.4844088033079,17.972395971259));
#142824=CARTESIAN_POINT('Ctrl Pts',(17.6293814748144,21.5219498994727,17.9765670852369));
#142825=CARTESIAN_POINT('Ctrl Pts',(17.706401696316,21.5557050403549,17.9807381992148));
#142826=CARTESIAN_POINT('Ctrl Pts',(17.7833960729387,21.5894488543737,17.9849079135351));
#142827=CARTESIAN_POINT('Ctrl Pts',(17.8620835505882,21.6194090516659,17.9890776278554));
#142828=CARTESIAN_POINT('Ctrl Pts',(17.9420562076477,21.6454249895519,17.9932473421757));
#142829=CARTESIAN_POINT('Ctrl Pts',(18.0220260189367,21.6714400016791,17.9974169081197));
#142830=CARTESIAN_POINT('Ctrl Pts',(18.1032804809775,21.6935108919569,18.0015864740637));
#142831=CARTESIAN_POINT('Ctrl Pts',(18.1853954972942,21.7115265644682,18.0057560400077));
#142832=CARTESIAN_POINT('Ctrl Pts',(18.2703975762872,21.7301756458007,18.0100722027467));
#142833=CARTESIAN_POINT('Ctrl Pts',(18.3563213344853,21.7444789277004,18.0143883654857));
#142834=CARTESIAN_POINT('Ctrl Pts',(18.4426856715114,21.7543709839536,18.0187045282247));
#142835=CARTESIAN_POINT('Ctrl Pts',(18.5262366993405,21.7639408075146,18.0228800924163));
#142836=CARTESIAN_POINT('Ctrl Pts',(18.6101995699748,21.7693824000208,18.0270556566079));
#142837=CARTESIAN_POINT('Ctrl Pts',(18.6941361080731,21.7706896042529,18.0312312207995));
#142838=CARTESIAN_POINT('Ctrl Pts',(18.7823120811743,21.7720628322632,18.0356176828122));
#142839=CARTESIAN_POINT('Ctrl Pts',(18.870458408217,21.7688730610124,18.0400041448249));
#142840=CARTESIAN_POINT('Ctrl Pts',(18.9580725064404,21.7611748002554,18.0443906068375));
#142841=CARTESIAN_POINT('Ctrl Pts',(19.0456866046639,21.7534765394983,18.0487770688502));
#142842=CARTESIAN_POINT('Ctrl Pts',(19.132767910028,21.7412699451077,18.0531635308629));
#142843=CARTESIAN_POINT('Ctrl Pts',(19.2188278686568,21.7246710082614,18.0575499928755));
#142844=CARTESIAN_POINT('Ctrl Pts',(19.3009280810131,21.7088358131057,18.0617346272685));
#142845=CARTESIAN_POINT('Ctrl Pts',(19.3824044612751,21.6889446480546,18.0659192616614));
#142846=CARTESIAN_POINT('Ctrl Pts',(19.4628256864492,21.6650605369004,18.0701038960543));
#142847=CARTESIAN_POINT('Ctrl Pts',(19.5431324419635,21.6412104218221,18.0742825741382));
#142848=CARTESIAN_POINT('Ctrl Pts',(19.6223865883777,21.6133787796397,18.078461252222));
#142849=CARTESIAN_POINT('Ctrl Pts',(19.7001664211467,21.5816797435859,18.0826399303058));
#142850=CARTESIAN_POINT('Ctrl Pts',(19.7793404015215,21.5494125250915,18.0868935081913));
#142851=CARTESIAN_POINT('Ctrl Pts',(19.8569862208222,21.5131379942492,18.0911470860767));
#142852=CARTESIAN_POINT('Ctrl Pts',(19.9326746288814,21.4730298702882,18.0954006639622));
#142853=CARTESIAN_POINT('Ctrl Pts',(20.0068956694542,21.433699320576,18.09957177794));
#142854=CARTESIAN_POINT('Ctrl Pts',(20.0792340927642,21.3906827199666,18.1037428919179));
#142855=CARTESIAN_POINT('Ctrl Pts',(20.1493064094734,21.3441919199415,18.1079140058957));
#142856=CARTESIAN_POINT('Ctrl Pts',(20.2193552127399,21.2977167203534,18.112083720216));
#142857=CARTESIAN_POINT('Ctrl Pts',(20.2871390365835,21.2477698907686,18.1162534345363));
#142858=CARTESIAN_POINT('Ctrl Pts',(20.3523020056983,21.1946074758765,18.1204231488565));
#142859=CARTESIAN_POINT('Ctrl Pts',(20.4174626560349,21.1414469527312,18.1245927148004));
#142860=CARTESIAN_POINT('Ctrl Pts',(20.4800022811539,21.0850713632533,18.1287622807444));
#142861=CARTESIAN_POINT('Ctrl Pts',(20.5395979115911,21.0257771713513,18.1329318466883));
#142862=CARTESIAN_POINT('Ctrl Pts',(20.6012888508791,20.9643982688056,18.1372480094273));
#142863=CARTESIAN_POINT('Ctrl Pts',(20.6598245480544,20.8998920810988,18.1415641721664));
#142864=CARTESIAN_POINT('Ctrl Pts',(20.7148895795158,20.8326277235438,18.1458803349055));
#142865=CARTESIAN_POINT('Ctrl Pts',(20.768160873366,20.767554495365,18.150055899097));
#142866=CARTESIAN_POINT('Ctrl Pts',(20.8181839009053,20.6999004393907,18.1542314632886));
#142867=CARTESIAN_POINT('Ctrl Pts',(20.864716308885,20.6300306589541,18.1584070274802));
#142868=CARTESIAN_POINT('Ctrl Pts',(20.9135989581756,20.5566319220009,18.162793489493));
#142869=CARTESIAN_POINT('Ctrl Pts',(20.9586288003486,20.4807882477351,18.1671799515058));
#142870=CARTESIAN_POINT('Ctrl Pts',(20.9995796309652,20.4029517338197,18.1715664135186));
#142871=CARTESIAN_POINT('Ctrl Pts',(21.0405304615817,20.3251152199043,18.1759528755314));
#142872=CARTESIAN_POINT('Ctrl Pts',(21.0774021064019,20.2452864249786,18.1803393375442));
#142873=CARTESIAN_POINT('Ctrl Pts',(21.1100276507034,20.1639389293617,18.184725799557));
#142874=CARTESIAN_POINT('Ctrl Pts',(21.1411520453503,20.0863343526005,18.1889104339505));
#142875=CARTESIAN_POINT('Ctrl Pts',(21.1685283427045,20.00705890033,18.193095068344));
#142876=CARTESIAN_POINT('Ctrl Pts',(21.1919760688457,19.926509360513,18.1972797027374));
#142877=CARTESIAN_POINT('Ctrl Pts',(21.2153904200511,19.8460744729959,18.2014583808218));
#142878=CARTESIAN_POINT('Ctrl Pts',(21.2348871797096,19.7643695380469,18.2056370589062));
#142879=CARTESIAN_POINT('Ctrl Pts',(21.2503340551361,19.6818109206067,18.2098157369906));
#142880=CARTESIAN_POINT('Ctrl Pts',(21.266057804701,19.5977724992938,18.2140693148759));
#142881=CARTESIAN_POINT('Ctrl Pts',(21.2775848741471,19.5128499374387,18.2183228927613));
#142882=CARTESIAN_POINT('Ctrl Pts',(21.2848289888802,19.4274981974254,18.2225764706466));
#142883=CARTESIAN_POINT('Ctrl Pts',(21.2919326623144,19.3438011674314,18.226747584625));
#142884=CARTESIAN_POINT('Ctrl Pts',(21.2949179252555,19.2596919311857,18.2309186986034));
#142885=CARTESIAN_POINT('Ctrl Pts',(21.2937553357682,19.1756076137221,18.2350898125818));
#142886=CARTESIAN_POINT('Ctrl Pts',(21.2925931363989,19.0915515115633,18.2392595269026));
#142887=CARTESIAN_POINT('Ctrl Pts',(21.287285855196,19.0075207711861,18.2434292412234));
#142888=CARTESIAN_POINT('Ctrl Pts',(21.2778561566697,18.9239532195383,18.2475989555442));
#142889=CARTESIAN_POINT('Ctrl Pts',(21.2684267936926,18.8403886415826,18.2517685214887));
#142890=CARTESIAN_POINT('Ctrl Pts',(21.2548753574853,18.7572876766216,18.2559380874331));
#142891=CARTESIAN_POINT('Ctrl Pts',(21.2372763100334,18.6750823611546,18.2601076533776));
#142892=CARTESIAN_POINT('Ctrl Pts',(21.2190585017879,18.5899868082262,18.264423816116));
#142893=CARTESIAN_POINT('Ctrl Pts',(21.1965032689153,18.5058515744424,18.2687399788544));
#142894=CARTESIAN_POINT('Ctrl Pts',(21.1697502461669,18.4231416762528,18.2730561415928));
#142895=CARTESIAN_POINT('Ctrl Pts',(21.1438687003149,18.3431260442794,18.2772317057849));
#142896=CARTESIAN_POINT('Ctrl Pts',(21.114058861765,18.2644447370881,18.281407269977));
#142897=CARTESIAN_POINT('Ctrl Pts',(21.0804965434245,18.1874991589174,18.2855828341691));
#142898=CARTESIAN_POINT('Ctrl Pts',(21.045239072183,18.1066672425405,18.2899692961807));
#142899=CARTESIAN_POINT('Ctrl Pts',(21.0058403441653,18.0277515290332,18.2943557581922));
#142900=CARTESIAN_POINT('Ctrl Pts',(20.9625580617871,17.9511869324206,18.2987422202038));
#142901=CARTESIAN_POINT('Ctrl Pts',(20.9192757794088,17.8746223358079,18.3031286822153));
#142902=CARTESIAN_POINT('Ctrl Pts',(20.8721103180847,17.8004093049791,18.3075151442269));
#142903=CARTESIAN_POINT('Ctrl Pts',(20.8213695361433,17.7289445288449,18.3119016062384));
#142904=CARTESIAN_POINT('Ctrl Pts',(20.7729692668539,17.6607761980217,18.3160857345562));
#142905=CARTESIAN_POINT('Ctrl Pts',(20.7211361130899,17.5948544666328,18.320269862874));
#142906=CARTESIAN_POINT('Ctrl Pts',(20.6661059353023,17.5315457270977,18.3244539911917));
#142907=CARTESIAN_POINT('Ctrl Pts',(20.6102092780632,17.4672401577484,18.3287040008378));
#142908=CARTESIAN_POINT('Ctrl Pts',(20.551014254789,17.4056310123225,18.3329540104839));
#142909=CARTESIAN_POINT('Ctrl Pts',(20.4888142269941,17.3470721503397,18.33720402013));
#142910=CARTESIAN_POINT('Ctrl Pts',(20.4266141991991,17.2885132883569,18.3414540297761));
#142911=CARTESIAN_POINT('Ctrl Pts',(20.3614094818074,17.2330051012627,18.3457040394221));
#142912=CARTESIAN_POINT('Ctrl Pts',(20.2935357313021,17.1808649545432,18.3499540490682));
#142913=CARTESIAN_POINT('Ctrl Pts',(20.2961055602205,17.1775141780511,17.5498940766593));
#142914=CARTESIAN_POINT('Ctrl Pts',(19.6284053936389,16.6654353848825,17.5919369087166));
#142915=CARTESIAN_POINT('Ctrl Pts',(17.7316712639343,16.3587002035979,17.6763716763344));
#142916=CARTESIAN_POINT('Ctrl Pts',(16.286227466659,17.9552740380232,17.7708370079901));
#142917=CARTESIAN_POINT('Ctrl Pts',(16.1722336618266,19.0070072559387,17.8232595075886));
#142918=CARTESIAN_POINT('Ctrl Pts',(16.1740883584118,19.2086434103328,17.8332900716265));
#142919=CARTESIAN_POINT('',(16.1740009581142,19.2132148462219,17.7667099127475));
#142920=CARTESIAN_POINT('Ctrl Pts',(20.2910030380574,17.1841723135106,17.4833253062578));
#142921=CARTESIAN_POINT('Ctrl Pts',(19.9334915614287,16.9103468713152,17.5056373115179));
#142922=CARTESIAN_POINT('Ctrl Pts',(18.6971962548141,16.3747766224752,17.5703412523384));
#142923=CARTESIAN_POINT('Ctrl Pts',(16.6895185666654,17.1540155201862,17.6648027803286));
#142924=CARTESIAN_POINT('Ctrl Pts',(16.1805385807744,18.6141143559075,17.7369523030588));
#142925=CARTESIAN_POINT('Ctrl Pts',(16.1756125809373,19.2132129985223,17.7667098902285));
#142926=CARTESIAN_POINT('Ctrl Pts',(16.1740009581142,19.2132148462218,17.7667099127475));
#142927=CARTESIAN_POINT('Ctrl Pts',(16.1740887027227,19.3146332252549,17.7717442924629));
#142928=CARTESIAN_POINT('Ctrl Pts',(16.1802070184511,19.4157876786429,17.7767786721782));
#142929=CARTESIAN_POINT('Ctrl Pts',(16.1922394471755,19.5160463769745,17.7818130518935));
#142930=CARTESIAN_POINT('Ctrl Pts',(16.2044426849033,19.6177283198346,17.7869188982596));
#142931=CARTESIAN_POINT('Ctrl Pts',(16.2227290670649,19.71848890314,17.7920247446257));
#142932=CARTESIAN_POINT('Ctrl Pts',(16.2469282568518,19.8176911441861,17.7971305909918));
#142933=CARTESIAN_POINT('Ctrl Pts',(16.2587491290717,19.8661496680319,17.7996247057948));
#142934=CARTESIAN_POINT('Ctrl Pts',(16.2719801580739,19.9142366801005,17.8021188205978));
#142935=CARTESIAN_POINT('Ctrl Pts',(16.2865973915759,19.9618797988219,17.8046129354008));
#142936=CARTESIAN_POINT('Ctrl Pts',(16.3111222362101,20.0418155872439,17.8087975697939));
#142937=CARTESIAN_POINT('Ctrl Pts',(16.3396130703746,20.1206973427815,17.8129822041869));
#142938=CARTESIAN_POINT('Ctrl Pts',(16.3719611025222,20.1981029565358,17.8171668385799));
#142939=CARTESIAN_POINT('Ctrl Pts',(16.4042630912499,20.2753983929799,17.8213455166639));
#142940=CARTESIAN_POINT('Ctrl Pts',(16.440411196743,20.351221440268,17.8255241947478));
#142941=CARTESIAN_POINT('Ctrl Pts',(16.480246839823,20.4251650188471,17.8297028728317));
#142942=CARTESIAN_POINT('Ctrl Pts',(16.5207965081758,20.5004339829301,17.8339564507172));
#142943=CARTESIAN_POINT('Ctrl Pts',(16.5651670712162,20.5737549756816,17.8382100286026));
#142944=CARTESIAN_POINT('Ctrl Pts',(16.6131398985284,20.6447197878197,17.8424636064881));
#142945=CARTESIAN_POINT('Ctrl Pts',(16.6601826789718,20.7143088085979,17.846634720466));
#142946=CARTESIAN_POINT('Ctrl Pts',(16.7106890267626,20.7816317931436,17.8508058344439));
#142947=CARTESIAN_POINT('Ctrl Pts',(16.7644072919754,20.8463301087231,17.8549769484219));
#142948=CARTESIAN_POINT('Ctrl Pts',(16.8181075315056,20.9110067141581,17.8591466627423));
#142949=CARTESIAN_POINT('Ctrl Pts',(16.875017254325,20.9730600461346,17.8633163770626));
#142950=CARTESIAN_POINT('Ctrl Pts',(16.934843824038,21.032163653958,17.867486091383));
#142951=CARTESIAN_POINT('Ctrl Pts',(16.9946682648649,21.0912651586214,17.871655657327));
#142952=CARTESIAN_POINT('Ctrl Pts',(17.0574090183537,21.147416825124,17.8758252232711));
#142953=CARTESIAN_POINT('Ctrl Pts',(17.1227367799309,21.2003292426476,17.8799947892151));
#142954=CARTESIAN_POINT('Ctrl Pts',(17.1903613850149,21.2551019954968,17.884310951954));
#142955=CARTESIAN_POINT('Ctrl Pts',(17.2607578915088,21.3064031452814,17.888627114693));
#142956=CARTESIAN_POINT('Ctrl Pts',(17.333525567137,21.3539585537049,17.8929432774319));
#142957=CARTESIAN_POINT('Ctrl Pts',(17.4039228433852,21.3999648497009,17.8971188416236));
#142958=CARTESIAN_POINT('Ctrl Pts',(17.4765387490622,21.4424654946024,17.9012944058152));
#142959=CARTESIAN_POINT('Ctrl Pts',(17.5509843556048,21.4812585723032,17.9054699700069));
#142960=CARTESIAN_POINT('Ctrl Pts',(17.6291900327565,21.5220109961371,17.9098564320195));
#142961=CARTESIAN_POINT('Ctrl Pts',(17.7094145736836,21.558671228602,17.914242894032));
#142962=CARTESIAN_POINT('Ctrl Pts',(17.7911842815277,21.5910627136699,17.9186293560446));
#142963=CARTESIAN_POINT('Ctrl Pts',(17.8729539893717,21.6234541987377,17.9230158180571));
#142964=CARTESIAN_POINT('Ctrl Pts',(17.9562682900627,21.6515768229132,17.9274022800697));
#142965=CARTESIAN_POINT('Ctrl Pts',(18.0406384682269,21.6753152773656,17.9317887420822));
#142966=CARTESIAN_POINT('Ctrl Pts',(18.1211266494267,21.6979614903396,17.9359733764753));
#142967=CARTESIAN_POINT('Ctrl Pts',(18.2028752706869,21.716702405741,17.9401580108683));
#142968=CARTESIAN_POINT('Ctrl Pts',(18.2854705184225,21.7314010205037,17.9443426452613));
#142969=CARTESIAN_POINT('Ctrl Pts',(18.3679482020463,21.7460787136075,17.9485213233452));
#142970=CARTESIAN_POINT('Ctrl Pts',(18.4512696694583,21.7567254548487,17.9527000014292));
#142971=CARTESIAN_POINT('Ctrl Pts',(18.5350067952745,21.7632542397796,17.9568786795131));
#142972=CARTESIAN_POINT('Ctrl Pts',(18.6202448488907,21.7699000484884,17.9611322573985));
#142973=CARTESIAN_POINT('Ctrl Pts',(18.7059131447156,21.7722786894991,17.965385835284));
#142974=CARTESIAN_POINT('Ctrl Pts',(18.7915501028463,21.7703530404503,17.9696394131694));
#142975=CARTESIAN_POINT('Ctrl Pts',(18.8755268214362,21.768464723866,17.9738105271473));
#142976=CARTESIAN_POINT('Ctrl Pts',(18.9594729254761,21.76243753283,17.9779816411253));
#142977=CARTESIAN_POINT('Ctrl Pts',(19.04295064826,21.7522889440085,17.9821527551032));
#142978=CARTESIAN_POINT('Ctrl Pts',(19.1264003592878,21.742143760644,17.9863224694236));
#142979=CARTESIAN_POINT('Ctrl Pts',(19.209381544911,21.7278799815763,17.9904921837439));
#142980=CARTESIAN_POINT('Ctrl Pts',(19.2914613132264,21.709566966134,17.9946618980643));
#142981=CARTESIAN_POINT('Ctrl Pts',(19.3735381607915,21.6912546023473,17.9988314640083));
#142982=CARTESIAN_POINT('Ctrl Pts',(19.454713206017,21.6688933896802,18.0030010299523));
#142983=CARTESIAN_POINT('Ctrl Pts',(19.5345648538852,21.6426035685785,18.0071705958964));
#142984=CARTESIAN_POINT('Ctrl Pts',(19.6172239871857,21.6153894297986,18.0114867586353));
#142985=CARTESIAN_POINT('Ctrl Pts',(19.6984644293619,21.5839654477009,18.0158029213742));
#142986=CARTESIAN_POINT('Ctrl Pts',(19.7778387647094,21.5485201888519,18.0201190841132));
#142987=CARTESIAN_POINT('Ctrl Pts',(19.8546274894308,21.514229555582,18.0242946483049));
#142988=CARTESIAN_POINT('Ctrl Pts',(19.9296694183931,21.4761758636208,18.0284702124965));
#142989=CARTESIAN_POINT('Ctrl Pts',(20.0025842524506,21.434576846982,18.0326457766882));
#142990=CARTESIAN_POINT('Ctrl Pts',(20.079181841439,21.3908767629043,18.0370322387008));
#142991=CARTESIAN_POINT('Ctrl Pts',(20.1534313177603,21.34326410831,18.0414187007134));
#142992=CARTESIAN_POINT('Ctrl Pts',(20.2249278226102,21.2920416208636,18.045805162726));
#142993=CARTESIAN_POINT('Ctrl Pts',(20.2964243274601,21.2408191334172,18.0501916247385));
#142994=CARTESIAN_POINT('Ctrl Pts',(20.365167454674,21.1859872343881,18.0545780867511));
#142995=CARTESIAN_POINT('Ctrl Pts',(20.4307957154104,21.1278944415812,18.0589645487637));
#142996=CARTESIAN_POINT('Ctrl Pts',(20.4934043225861,21.0724745842854,18.0631491831568));
#142997=CARTESIAN_POINT('Ctrl Pts',(20.5534114448285,21.0138810328615,18.0673338175499));
#142998=CARTESIAN_POINT('Ctrl Pts',(20.6104778947951,20.9523875818856,18.071518451943));
#142999=CARTESIAN_POINT('Ctrl Pts',(20.6674631177336,20.8909816592258,18.0756971300271));
#143000=CARTESIAN_POINT('Ctrl Pts',(20.7215156722283,20.8266843701415,18.0798758081111));
#143001=CARTESIAN_POINT('Ctrl Pts',(20.7723306651574,20.7598086064711,18.0840544861951));
#143002=CARTESIAN_POINT('Ctrl Pts',(20.8240564803137,20.6917341428009,18.0883080640805));
#143003=CARTESIAN_POINT('Ctrl Pts',(20.8724271646773,20.6209881765789,18.0925616419659));
#143004=CARTESIAN_POINT('Ctrl Pts',(20.91716165977,20.5479387298266,18.0968152198513));
#143005=CARTESIAN_POINT('Ctrl Pts',(20.9610288893839,20.4763054891425,18.1009863338293));
#143006=CARTESIAN_POINT('Ctrl Pts',(21.0013994094997,20.4024576962095,18.1051574478073));
#143007=CARTESIAN_POINT('Ctrl Pts',(21.0380509604128,20.326772903337,18.1093285617853));
#143008=CARTESIAN_POINT('Ctrl Pts',(21.0746902125439,20.2511135072276,18.1134982761058));
#143009=CARTESIAN_POINT('Ctrl Pts',(21.1076127735552,20.173618749099,18.1176679904262));
#143010=CARTESIAN_POINT('Ctrl Pts',(21.136642647489,20.094690165424,18.1218377047466));
#143011=CARTESIAN_POINT('Ctrl Pts',(21.1656714884152,20.0157643903668,18.1260072706907));
#143012=CARTESIAN_POINT('Ctrl Pts',(21.1908077596747,19.9354053232572,18.1301768366348));
#143013=CARTESIAN_POINT('Ctrl Pts',(21.211924363067,19.8540325426592,18.1343464025789));
#143014=CARTESIAN_POINT('Ctrl Pts',(21.2337834001838,19.7697987954823,18.1386625653178));
#143015=CARTESIAN_POINT('Ctrl Pts',(21.2513347146947,19.6844792346863,18.1429787280566));
#143016=CARTESIAN_POINT('Ctrl Pts',(21.2644946836059,19.5985521335795,18.1472948907955));
#143017=CARTESIAN_POINT('Ctrl Pts',(21.2772259679145,19.5154240987508,18.1514704549872));
#143018=CARTESIAN_POINT('Ctrl Pts',(21.2858476079666,19.4317279704214,18.1556460191789));
#143019=CARTESIAN_POINT('Ctrl Pts',(21.290336834896,19.3479013752813,18.1598215833707));
#143020=CARTESIAN_POINT('Ctrl Pts',(21.2950528020053,19.2598408981036,18.1642080453831));
#143021=CARTESIAN_POINT('Ctrl Pts',(21.295207927637,19.1716370118692,18.1685945073955));
#143022=CARTESIAN_POINT('Ctrl Pts',(21.2908376238657,19.083794004918,18.1729809694079));
#143023=CARTESIAN_POINT('Ctrl Pts',(21.2864673200944,18.9959509979668,18.1773674314203));
#143024=CARTESIAN_POINT('Ctrl Pts',(21.2775717212916,18.9084694398441,18.1817538934327));
#143025=CARTESIAN_POINT('Ctrl Pts',(21.2642482087237,18.8218419315364,18.1861403554451));
#143026=CARTESIAN_POINT('Ctrl Pts',(21.2515412573717,18.7392232130713,18.1903238287683));
#143027=CARTESIAN_POINT('Ctrl Pts',(21.2347598613936,18.6570738106191,18.1945073020914));
#143028=CARTESIAN_POINT('Ctrl Pts',(21.2139505970127,18.5758267666406,18.1986907754146));
#143029=CARTESIAN_POINT('Ctrl Pts',(21.1931684634965,18.4946856515652,18.2028687943764));
#143030=CARTESIAN_POINT('Ctrl Pts',(21.1683689994549,18.4144450007966,18.2070468133382));
#143031=CARTESIAN_POINT('Ctrl Pts',(21.1396501998692,18.3355303455463,18.2112248323));
#143032=CARTESIAN_POINT('Ctrl Pts',(21.11096022557,18.2566948975601,18.2153986577511));
#143033=CARTESIAN_POINT('Ctrl Pts',(21.078358883834,18.1791832320113,18.2195724832022));
#143034=CARTESIAN_POINT('Ctrl Pts',(21.0419943136825,18.103407002546,18.2237463086533));
#143035=CARTESIAN_POINT('Ctrl Pts',(21.0056553325363,18.0276840952658,18.2279171970687));
#143036=CARTESIAN_POINT('Ctrl Pts',(20.9655585822467,17.9536946114992,18.2320880854841));
#143037=CARTESIAN_POINT('Ctrl Pts',(20.9219002659552,17.8818301740435,18.2362589738995));
#143038=CARTESIAN_POINT('Ctrl Pts',(20.8782487043954,17.8099768553171,18.2404292170029));
#143039=CARTESIAN_POINT('Ctrl Pts',(20.8310368995156,17.7402483290549,18.2445994601063));
#143040=CARTESIAN_POINT('Ctrl Pts',(20.7805064538479,17.6730106195559,18.2487697032098));
#143041=CARTESIAN_POINT('Ctrl Pts',(20.7299824361656,17.6057814633758,18.252939415816));
#143042=CARTESIAN_POINT('Ctrl Pts',(20.6761408980458,17.5410428584497,18.2571091284222));
#143043=CARTESIAN_POINT('Ctrl Pts',(20.6192651021105,17.4791294809472,18.2612788410284));
#143044=CARTESIAN_POINT('Ctrl Pts',(20.5623509460967,17.4171743457517,18.2654513659117));
#143045=CARTESIAN_POINT('Ctrl Pts',(20.502398759404,17.3580485804598,18.2696238907951));
#143046=CARTESIAN_POINT('Ctrl Pts',(20.4397297081047,17.3020510318793,18.2737964156785));
#143047=CARTESIAN_POINT('Ctrl Pts',(20.3924913150559,17.2598414538696,18.276941562547));
#143048=CARTESIAN_POINT('Ctrl Pts',(20.343710066172,17.2194085323209,18.2800867094155));
#143049=CARTESIAN_POINT('Ctrl Pts',(20.2935357313021,17.1808649545431,18.2832318562841));
#143050=CARTESIAN_POINT('Origin',(18.734,19.211,-1.76670989022852));
#143051=CARTESIAN_POINT('',(20.2912840337091,17.1837659559064,19.1498287221711));
#143052=CARTESIAN_POINT('',(20.2935357313021,17.1808649545431,19.0833436983648));
#143053=CARTESIAN_POINT('',(20.2935357313021,17.1808649545432,-1.76670989022852));
#143054=CARTESIAN_POINT('',(16.1743944470979,19.2113823947302,18.633290134885));
#143055=CARTESIAN_POINT('Ctrl Pts',(16.1781629602604,19.2113866753936,18.633290374834));
#143056=CARTESIAN_POINT('Ctrl Pts',(16.1776269335845,19.615981772308,18.6533365919835));
#143057=CARTESIAN_POINT('Ctrl Pts',(16.4590846999913,20.8754715672834,18.7157747446936));
#143058=CARTESIAN_POINT('Ctrl Pts',(18.4329096444066,22.2230815390193,18.8206048329641));
#143059=CARTESIAN_POINT('Ctrl Pts',(21.103709402057,21.094551947962,18.9477806396456));
#143060=CARTESIAN_POINT('Ctrl Pts',(21.532350072377,18.6295872811128,19.0575219360479));
#143061=CARTESIAN_POINT('Ctrl Pts',(20.6891187884342,17.492345631807,19.1248712968897));
#143062=CARTESIAN_POINT('Ctrl Pts',(20.2912840337091,17.1837659559064,19.1498287221711));
#143063=CARTESIAN_POINT('Ctrl Pts',(20.2935357313021,17.1808649545432,18.3499540490682));
#143064=CARTESIAN_POINT('Ctrl Pts',(20.2269224839007,17.129693117609,18.3541251305527));
#143065=CARTESIAN_POINT('Ctrl Pts',(20.157738873817,17.0817655823163,18.3582962120371));
#143066=CARTESIAN_POINT('Ctrl Pts',(20.0863370241469,17.0373430415262,18.3624672935216));
#143067=CARTESIAN_POINT('Ctrl Pts',(20.0149587887766,16.9929351923331,18.3666369955296));
#143068=CARTESIAN_POINT('Ctrl Pts',(19.9413641611146,16.9520302782791,18.3708066975376));
#143069=CARTESIAN_POINT('Ctrl Pts',(19.8659339714226,16.9148455007688,18.3749763995456));
#143070=CARTESIAN_POINT('Ctrl Pts',(19.7905061011064,16.8776618666399,18.379145973341));
#143071=CARTESIAN_POINT('Ctrl Pts',(19.7132431940035,16.844198344213,18.3833155471363));
#143072=CARTESIAN_POINT('Ctrl Pts',(19.6345491545281,16.8146254006774,18.3874851209316));
#143073=CARTESIAN_POINT('Ctrl Pts',(19.5534056519861,16.7841319575277,18.3917844785973));
#143074=CARTESIAN_POINT('Ctrl Pts',(19.4707409318527,16.7577754970438,18.396083836263));
#143075=CARTESIAN_POINT('Ctrl Pts',(19.3870163605659,16.7356879726319,18.4003831939287));
#143076=CARTESIAN_POINT('Ctrl Pts',(19.3057019355853,16.7142362730985,18.4045587876761));
#143077=CARTESIAN_POINT('Ctrl Pts',(19.2233883259854,16.6968110951066,18.4087343814235));
#143078=CARTESIAN_POINT('Ctrl Pts',(19.1405083013071,16.6834812560599,18.4129099751709));
#143079=CARTESIAN_POINT('Ctrl Pts',(19.0539434509894,16.6695587756273,18.4172712147957));
#143080=CARTESIAN_POINT('Ctrl Pts',(18.9667612123123,16.6601043263589,18.4216324544206));
#143081=CARTESIAN_POINT('Ctrl Pts',(18.8794581009856,16.6551357741739,18.4259936940454));
#143082=CARTESIAN_POINT('Ctrl Pts',(18.7921549896588,16.6501672219889,18.4303549336702));
#143083=CARTESIAN_POINT('Ctrl Pts',(18.7047315697535,16.6496844957764,18.434716173295));
#143084=CARTESIAN_POINT('Ctrl Pts',(18.6176794289206,16.6536440363642,18.4390774129198));
#143085=CARTESIAN_POINT('Ctrl Pts',(18.5341524013311,16.6574432382304,18.4432620473123));
#143086=CARTESIAN_POINT('Ctrl Pts',(18.4506562604971,16.6653459878634,18.4474466817047));
#143087=CARTESIAN_POINT('Ctrl Pts',(18.3676269095308,16.6773522820684,18.4516313160972));
#143088=CARTESIAN_POINT('Ctrl Pts',(18.2847157405689,16.6893414867996,18.4558099941805));
#143089=CARTESIAN_POINT('Ctrl Pts',(18.2022704931355,16.7054225689873,18.4599886722639));
#143090=CARTESIAN_POINT('Ctrl Pts',(18.1207249420869,16.725543562373,18.4641673503472));
#143091=CARTESIAN_POINT('Ctrl Pts',(18.0377177456267,16.746025210108,18.4684209282328));
#143092=CARTESIAN_POINT('Ctrl Pts',(17.9556432985583,16.7706930025008,18.4726745061184));
#143093=CARTESIAN_POINT('Ctrl Pts',(17.8749514567222,16.7994371042222,18.476928084004));
#143094=CARTESIAN_POINT('Ctrl Pts',(17.7958239837114,16.8276239454371,18.4810991979813));
#143095=CARTESIAN_POINT('Ctrl Pts',(17.7180264386454,16.8597302905275,18.4852703119587));
#143096=CARTESIAN_POINT('Ctrl Pts',(17.6419689102696,16.8956019566687,18.489441425936));
#143097=CARTESIAN_POINT('Ctrl Pts',(17.5659369037321,16.9314615857259,18.4936111402558));
#143098=CARTESIAN_POINT('Ctrl Pts',(17.4916441700226,16.971083830448,18.4977808545755));
#143099=CARTESIAN_POINT('Ctrl Pts',(17.4194798631979,17.0142667868078,18.5019505688953));
#143100=CARTESIAN_POINT('Ctrl Pts',(17.3473181242892,17.0574482065325,18.5061201348387));
#143101=CARTESIAN_POINT('Ctrl Pts',(17.2772850559937,17.1041898490211,18.5102897007821));
#143102=CARTESIAN_POINT('Ctrl Pts',(17.2097430958426,17.1542450583192,18.5144592667256));
#143103=CARTESIAN_POINT('Ctrl Pts',(17.1398264436724,17.2060601470428,18.5187754294652));
#143104=CARTESIAN_POINT('Ctrl Pts',(17.0725797574077,17.2614258339335,18.5230915922048));
#143105=CARTESIAN_POINT('Ctrl Pts',(17.0083685115614,17.3200224839758,18.5274077549445));
#143106=CARTESIAN_POINT('Ctrl Pts',(16.9462489403142,17.3767103542884,18.5315833191355));
#143107=CARTESIAN_POINT('Ctrl Pts',(16.8869703858411,17.4364215555155,18.5357588833266));
#143108=CARTESIAN_POINT('Ctrl Pts',(16.8308254399579,17.4988298583352,18.5399344475177));
#143109=CARTESIAN_POINT('Ctrl Pts',(16.7718447463028,17.5643902561989,18.5443209095316));
#143110=CARTESIAN_POINT('Ctrl Pts',(16.7163229051916,17.6329269235817,18.5487073715455));
#143111=CARTESIAN_POINT('Ctrl Pts',(16.6645491064847,17.7040252160939,18.5530938335595));
#143112=CARTESIAN_POINT('Ctrl Pts',(16.6127753077779,17.775123508606,18.5574802955734));
#143113=CARTESIAN_POINT('Ctrl Pts',(16.5647498046499,17.8487828986679,18.5618667575873));
#143114=CARTESIAN_POINT('Ctrl Pts',(16.5207062260027,17.924558913131,18.5662532196012));
#143115=CARTESIAN_POINT('Ctrl Pts',(16.4770273612299,17.9997074453442,18.5706033584188));
#143116=CARTESIAN_POINT('Ctrl Pts',(16.4371122169921,18.0771985084612,18.5749534972363));
#143117=CARTESIAN_POINT('Ctrl Pts',(16.4012086273385,18.1566355413635,18.5793036360539));
#143118=CARTESIAN_POINT('Ctrl Pts',(16.3640774712899,18.2387885765663,18.5838025088637));
#143119=CARTESIAN_POINT('Ctrl Pts',(16.3312374248385,18.3230227236652,18.5883013816735));
#143120=CARTESIAN_POINT('Ctrl Pts',(16.3029130373493,18.4088677290933,18.5928002544833));
#143121=CARTESIAN_POINT('Ctrl Pts',(16.2756354411695,18.4915401396801,18.5971328613513));
#143122=CARTESIAN_POINT('Ctrl Pts',(16.2525458055772,18.5757060184788,18.6014654682194));
#143123=CARTESIAN_POINT('Ctrl Pts',(16.2337970621827,18.660922487526,18.6057980750875));
#143124=CARTESIAN_POINT('Ctrl Pts',(16.2150725182344,18.7460289656627,18.6101250897576));
#143125=CARTESIAN_POINT('Ctrl Pts',(16.2006778102744,18.8321829392905,18.6144521044276));
#143126=CARTESIAN_POINT('Ctrl Pts',(16.1907160845812,18.9189265065566,18.6187791190976));
#143127=CARTESIAN_POINT('Ctrl Pts',(16.1807681682272,19.005549826451,18.6231001354883));
#143128=CARTESIAN_POINT('Ctrl Pts',(16.1752410444519,19.0927607071638,18.6274211518791));
#143129=CARTESIAN_POINT('Ctrl Pts',(16.1741865858058,19.1800923227742,18.6317421682699));
#143130=CARTESIAN_POINT('Ctrl Pts',(16.1740606709629,19.190520751334,18.6322581487704));
#143131=CARTESIAN_POINT('Ctrl Pts',(16.1739984722012,19.2009508929684,18.632774129271));
#143132=CARTESIAN_POINT('Ctrl Pts',(16.1740000284928,19.2113819467091,18.6332901097715));
#143133=CARTESIAN_POINT('',(16.1740000028035,19.2111198080496,18.5667098901964));
#143134=CARTESIAN_POINT('Ctrl Pts',(20.2935357313021,17.1808649545431,18.2832318562841));
#143135=CARTESIAN_POINT('Ctrl Pts',(20.2268915890121,17.1296693843687,18.2874094027522));
#143136=CARTESIAN_POINT('Ctrl Pts',(20.157788967903,17.0818088516824,18.2915869492204));
#143137=CARTESIAN_POINT('Ctrl Pts',(20.0866029412604,17.0375085039748,18.2957644956885));
#143138=CARTESIAN_POINT('Ctrl Pts',(20.0153008783135,16.9931359447832,18.2999488517383));
#143139=CARTESIAN_POINT('Ctrl Pts',(19.9419090336255,16.9523353753359,18.304133207788));
#143140=CARTESIAN_POINT('Ctrl Pts',(19.8668262035835,16.9152855594664,18.3083175638377));
#143141=CARTESIAN_POINT('Ctrl Pts',(19.8369284207219,16.9005324215078,18.3099837632673));
#143142=CARTESIAN_POINT('Ctrl Pts',(19.806762721368,16.886373464749,18.3116499626969));
#143143=CARTESIAN_POINT('Ctrl Pts',(19.7763550154481,16.8728177954295,18.3133161621265));
#143144=CARTESIAN_POINT('Ctrl Pts',(19.6999865269337,16.8387729391862,18.3175007965194));
#143145=CARTESIAN_POINT('Ctrl Pts',(19.6218062328668,16.8084101229908,18.3216854309124));
#143146=CARTESIAN_POINT('Ctrl Pts',(19.5422037920521,16.7819247375776,18.3258700653053));
#143147=CARTESIAN_POINT('Ctrl Pts',(19.4627146554591,16.7554770508322,18.3300487433892));
#143148=CARTESIAN_POINT('Ctrl Pts',(19.3818078256877,16.7328959763057,18.334227421473));
#143149=CARTESIAN_POINT('Ctrl Pts',(19.2998943515233,16.7143295005319,18.3384060995568));
#143150=CARTESIAN_POINT('Ctrl Pts',(19.2165126372019,16.6954302340229,18.3426596774423));
#143151=CARTESIAN_POINT('Ctrl Pts',(19.1320882756872,16.6806911015683,18.3469132553277));
#143152=CARTESIAN_POINT('Ctrl Pts',(19.0470726305014,16.6702155683665,18.3511668332132));
#143153=CARTESIAN_POINT('Ctrl Pts',(18.9637051794947,16.6599431238176,18.3553379471911));
#143154=CARTESIAN_POINT('Ctrl Pts',(18.8797696442084,16.6537704962434,18.3595090611689));
#143155=CARTESIAN_POINT('Ctrl Pts',(18.7957017187992,16.6517436826497,18.3636801751467));
#143156=CARTESIAN_POINT('Ctrl Pts',(18.7116620031942,16.649717549173,18.367849889467));
#143157=CARTESIAN_POINT('Ctrl Pts',(18.627490445211,16.6518344778738,18.3720196037873));
#143158=CARTESIAN_POINT('Ctrl Pts',(18.5436254163474,16.6580884234077,18.3761893181075));
#143159=CARTESIAN_POINT('Ctrl Pts',(18.4597633717615,16.6643421463994,18.3803588840515));
#143160=CARTESIAN_POINT('Ctrl Pts',(18.3762082933038,16.6747325584671,18.3845284499954));
#143161=CARTESIAN_POINT('Ctrl Pts',(18.2933947304035,16.6892016344672,18.3886980159393));
#143162=CARTESIAN_POINT('Ctrl Pts',(18.2076695447883,16.7041794253309,18.3930141786784));
#143163=CARTESIAN_POINT('Ctrl Pts',(18.122739507835,16.723527937402,18.3973303414174));
#143164=CARTESIAN_POINT('Ctrl Pts',(18.0390745966233,16.7471252702822,18.4016465041565));
#143165=CARTESIAN_POINT('Ctrl Pts',(17.958135061099,16.7699539225246,18.405822068348));
#143166=CARTESIAN_POINT('Ctrl Pts',(17.8783799255842,16.796758641008,18.4099976325396));
#143167=CARTESIAN_POINT('Ctrl Pts',(17.800216972615,16.8273789609572,18.4141731967312));
#143168=CARTESIAN_POINT('Ctrl Pts',(17.7181061946991,16.8595458404767,18.418559658744));
#143169=CARTESIAN_POINT('Ctrl Pts',(17.6377532005338,16.895923662579,18.4229461207568));
#143170=CARTESIAN_POINT('Ctrl Pts',(17.5596023636775,16.9362714026064,18.4273325827696));
#143171=CARTESIAN_POINT('Ctrl Pts',(17.4814515268212,16.9766191426339,18.4317190447824));
#143172=CARTESIAN_POINT('Ctrl Pts',(17.4055033100763,17.0209364424643,18.4361055067952));
#143173=CARTESIAN_POINT('Ctrl Pts',(17.3321657913463,17.0689307080656,18.4404919688079));
#143174=CARTESIAN_POINT('Ctrl Pts',(17.2622960528831,17.1146555545476,18.4446710160258));
#143175=CARTESIAN_POINT('Ctrl Pts',(17.19453408493,17.1638887348098,18.4488500632436));
#143176=CARTESIAN_POINT('Ctrl Pts',(17.1292545139166,17.2164093339998,18.4530291104615));
#143177=CARTESIAN_POINT('Ctrl Pts',(17.0640679209106,17.2688551278475,18.4572022054423));
#143178=CARTESIAN_POINT('Ctrl Pts',(17.0013570587502,17.3245787540421,18.461375300423));
#143179=CARTESIAN_POINT('Ctrl Pts',(16.9414683281886,17.3833156165374,18.4655483954038));
#143180=CARTESIAN_POINT('Ctrl Pts',(16.8809773183909,17.4426431743496,18.4697634576868));
#143181=CARTESIAN_POINT('Ctrl Pts',(16.8233659292104,17.5050446643084,18.4739785199699));
#143182=CARTESIAN_POINT('Ctrl Pts',(16.7689574885197,17.5702050926227,18.4781935822529));
#143183=CARTESIAN_POINT('Ctrl Pts',(16.7151877112471,17.6346006473008,18.4823591668069));
#143184=CARTESIAN_POINT('Ctrl Pts',(16.6645463875622,17.701690347722,18.4865247513609));
#143185=CARTESIAN_POINT('Ctrl Pts',(16.6173078768048,17.7711338758054,18.4906903359149));
#143186=CARTESIAN_POINT('Ctrl Pts',(16.5700850499658,17.84055434756,18.4948545374302));
#143187=CARTESIAN_POINT('Ctrl Pts',(16.5262630517187,17.9123267137652,18.4990187389455));
#143188=CARTESIAN_POINT('Ctrl Pts',(16.4860739671285,17.9860801859963,18.5031829404608));
#143189=CARTESIAN_POINT('Ctrl Pts',(16.4458860826637,18.0598314558034,18.5073470176248));
#143190=CARTESIAN_POINT('Ctrl Pts',(16.4093311160891,18.1355633083681,18.5115110947889));
#143191=CARTESIAN_POINT('Ctrl Pts',(16.3765953977375,18.2128799965778,18.5156751719529));
#143192=CARTESIAN_POINT('Ctrl Pts',(16.3431614559388,18.2918457802489,18.5199280651398));
#143193=CARTESIAN_POINT('Ctrl Pts',(16.3137117771032,18.3724643312945,18.5241809583268));
#143194=CARTESIAN_POINT('Ctrl Pts',(16.2883925214927,18.4542939401133,18.5284338515138));
#143195=CARTESIAN_POINT('Ctrl Pts',(16.2635663208298,18.534530038676,18.5326039259141));
#143196=CARTESIAN_POINT('Ctrl Pts',(16.2427111716314,18.6159299801766,18.5367740003144));
#143197=CARTESIAN_POINT('Ctrl Pts',(16.2259135016088,18.6980651926532,18.5409440747148));
#143198=CARTESIAN_POINT('Ctrl Pts',(16.2086154222953,18.7826472458752,18.545238377295));
#143199=CARTESIAN_POINT('Ctrl Pts',(16.1956204803926,18.8680085473305,18.5495326798753));
#143200=CARTESIAN_POINT('Ctrl Pts',(16.1869656326132,18.9536754357807,18.5538269824556));
#143201=CARTESIAN_POINT('Ctrl Pts',(16.1783107848339,19.0393423242308,18.5581212850358));
#143202=CARTESIAN_POINT('Ctrl Pts',(16.1739959871027,19.125314270194,18.5624155876161));
#143203=CARTESIAN_POINT('Ctrl Pts',(16.1740000028035,19.2111198080496,18.5667098901964));
#143204=CARTESIAN_POINT('Ctrl Pts',(16.1740000028035,19.2111198086916,18.5667098902285));
#143205=CARTESIAN_POINT('Ctrl Pts',(16.1740003013853,19.2174997239769,18.5670291853155));
#143206=CARTESIAN_POINT('Ctrl Pts',(16.1740244495167,19.223879573923,18.5673484804024));
#143207=CARTESIAN_POINT('Ctrl Pts',(16.1740724460423,19.2302592442234,18.5676677754894));
#143208=CARTESIAN_POINT('Ctrl Pts',(16.1747014814392,19.31387026376,18.5718524098819));
#143209=CARTESIAN_POINT('Ctrl Pts',(16.1794322843349,19.3976060296583,18.5760370442745));
#143210=CARTESIAN_POINT('Ctrl Pts',(16.1882813814472,19.4810309522136,18.580221678667));
#143211=CARTESIAN_POINT('Ctrl Pts',(16.197117882965,19.5643371297178,18.5844003567505));
#143212=CARTESIAN_POINT('Ctrl Pts',(16.2100609870472,19.6473328891642,18.5885790348339));
#143213=CARTESIAN_POINT('Ctrl Pts',(16.2270752140173,19.7295827970784,18.5927577129174));
#143214=CARTESIAN_POINT('Ctrl Pts',(16.2443944087804,19.8133069754922,18.5970112908029));
#143215=CARTESIAN_POINT('Ctrl Pts',(16.2659321081158,19.8962578184692,18.6012648686885));
#143216=CARTESIAN_POINT('Ctrl Pts',(16.2915956147073,19.9779816286607,18.6055184465741));
#143217=CARTESIAN_POINT('Ctrl Pts',(16.3167615841416,20.058121063309,18.6096895605515));
#143218=CARTESIAN_POINT('Ctrl Pts',(16.3458946705845,20.1370801583406,18.613860674529));
#143219=CARTESIAN_POINT('Ctrl Pts',(16.3788563531112,20.2144432731945,18.6180317885065));
#143220=CARTESIAN_POINT('Ctrl Pts',(16.4118069750271,20.2917804281082,18.6222015028263));
#143221=CARTESIAN_POINT('Ctrl Pts',(16.4485834613786,20.3675222435802,18.6263712171462));
#143222=CARTESIAN_POINT('Ctrl Pts',(16.4889988104969,20.4412721890418,18.6305409314661));
#143223=CARTESIAN_POINT('Ctrl Pts',(16.5294127214636,20.5150195101638,18.6347104974097));
#143224=CARTESIAN_POINT('Ctrl Pts',(16.5734650159173,20.5867746991837,18.6388800633532));
#143225=CARTESIAN_POINT('Ctrl Pts',(16.620922959331,20.6561662258016,18.6430496292968));
#143226=CARTESIAN_POINT('Ctrl Pts',(16.6700494655017,20.7279974729095,18.6473657920363));
#143227=CARTESIAN_POINT('Ctrl Pts',(16.7228252639787,20.7972953169818,18.6516819547758));
#143228=CARTESIAN_POINT('Ctrl Pts',(16.7789448088305,20.8636824254772,18.6559981175153));
#143229=CARTESIAN_POINT('Ctrl Pts',(16.8332362653982,20.9279069808804,18.6601736817065));
#143230=CARTESIAN_POINT('Ctrl Pts',(16.8906566126945,20.9894072108734,18.6643492458977));
#143231=CARTESIAN_POINT('Ctrl Pts',(16.9508909514353,21.0478783631277,18.668524810089));
#143232=CARTESIAN_POINT('Ctrl Pts',(17.0141675834551,21.1093027543025,18.6729112721026));
#143233=CARTESIAN_POINT('Ctrl Pts',(17.0805495076474,21.1673836440658,18.6772977341163));
#143234=CARTESIAN_POINT('Ctrl Pts',(17.149633344248,21.2218163268039,18.6816841961299));
#143235=CARTESIAN_POINT('Ctrl Pts',(17.2187171808487,21.276249009542,18.6860706581435));
#143236=CARTESIAN_POINT('Ctrl Pts',(17.2905024122582,21.327033212256,18.6904571201572));
#143237=CARTESIAN_POINT('Ctrl Pts',(17.3645537444777,21.3739186191894,18.6948435821708));
#143238=CARTESIAN_POINT('Ctrl Pts',(17.435197865104,21.4186467590315,18.6990282165633));
#143239=CARTESIAN_POINT('Ctrl Pts',(17.5081670866297,21.4599934843659,18.7032128509557));
#143240=CARTESIAN_POINT('Ctrl Pts',(17.5831040926458,21.497709122393,18.7073974853482));
#143241=CARTESIAN_POINT('Ctrl Pts',(17.6579344351091,21.5353710768775,18.7115761634316));
#143242=CARTESIAN_POINT('Ctrl Pts',(17.7347265911909,21.5694120050826,18.7157548415149));
#143243=CARTESIAN_POINT('Ctrl Pts',(17.8130952257719,21.5996260479204,18.7199335195983));
#143244=CARTESIAN_POINT('Ctrl Pts',(17.8928685618191,21.630381655767,18.7241870974839));
#143245=CARTESIAN_POINT('Ctrl Pts',(17.9742750416619,21.6571715770569,18.7284406753695));
#143246=CARTESIAN_POINT('Ctrl Pts',(18.0568830023299,21.6798281777933,18.732694253255));
#143247=CARTESIAN_POINT('Ctrl Pts',(18.1378894464698,21.7020455361098,18.7368653672324));
#143248=CARTESIAN_POINT('Ctrl Pts',(18.2200507369794,21.7202882813848,18.7410364812097));
#143249=CARTESIAN_POINT('Ctrl Pts',(18.3029424071742,21.734447909442,18.7452075951871));
#143250=CARTESIAN_POINT('Ctrl Pts',(18.3858062622684,21.7486027860993,18.7493773095069));
#143251=CARTESIAN_POINT('Ctrl Pts',(18.469399557216,21.7586771892408,18.7535470238266));
#143252=CARTESIAN_POINT('Ctrl Pts',(18.5532876521045,21.7646137232005,18.7577167381464));
#143253=CARTESIAN_POINT('Ctrl Pts',(18.6371727618945,21.7705500459129,18.7618863040899));
#143254=CARTESIAN_POINT('Ctrl Pts',(18.7213521918226,21.7723487605766,18.7660558700333));
#143255=CARTESIAN_POINT('Ctrl Pts',(18.8053875689174,21.7700044577929,18.7702254359767));
#143256=CARTESIAN_POINT('Ctrl Pts',(18.8923775262288,21.7675777322146,18.7745415987164));
#143257=CARTESIAN_POINT('Ctrl Pts',(18.9792125852182,21.7607112463061,18.778857761456));
#143258=CARTESIAN_POINT('Ctrl Pts',(19.0654100827151,21.7494576728941,18.7831739241956));
#143259=CARTESIAN_POINT('Ctrl Pts',(19.1487997057715,21.7385706834556,18.7873494883867));
#143260=CARTESIAN_POINT('Ctrl Pts',(19.2315922114994,21.7235781663988,18.7915250525778));
#143261=CARTESIAN_POINT('Ctrl Pts',(19.3133609024084,21.7045799455322,18.7957006167688));
#143262=CARTESIAN_POINT('Ctrl Pts',(19.3992595355479,21.6846221696845,18.8000870787827));
#143263=CARTESIAN_POINT('Ctrl Pts',(19.4840276488775,21.6602435606427,18.8044735407967));
#143264=CARTESIAN_POINT('Ctrl Pts',(19.5671906913808,21.6316183655827,18.8088600028106));
#143265=CARTESIAN_POINT('Ctrl Pts',(19.6503537338841,21.6029931705227,18.8132464648245));
#143266=CARTESIAN_POINT('Ctrl Pts',(19.7319111958455,21.5701216768946,18.8176329268384));
#143267=CARTESIAN_POINT('Ctrl Pts',(19.8114169849415,21.5332344068934,18.8220193888523));
#143268=CARTESIAN_POINT('Ctrl Pts',(19.8872645948573,21.4980443748502,18.8262040232484));
#143269=CARTESIAN_POINT('Ctrl Pts',(19.9615275033059,21.4590690053604,18.8303886576445));
#143270=CARTESIAN_POINT('Ctrl Pts',(20.0338023663787,21.4164736018271,18.8345732920406));
#143271=CARTESIAN_POINT('Ctrl Pts',(20.10597435513,21.3739388275784,18.8387519701276));
#143272=CARTESIAN_POINT('Ctrl Pts',(20.1761635263181,21.3277944856882,18.8429306482147));
#143273=CARTESIAN_POINT('Ctrl Pts',(20.243988210436,21.2782531543921,18.8471093263017));
#143274=CARTESIAN_POINT('Ctrl Pts',(20.3130286032089,21.2278238303834,18.8513629041863));
#143275=CARTESIAN_POINT('Ctrl Pts',(20.3796184709323,21.1738747399783,18.855616482071));
#143276=CARTESIAN_POINT('Ctrl Pts',(20.443383208966,21.1166781063194,18.8598700599557));
#143277=CARTESIAN_POINT('Ctrl Pts',(20.5059117431835,21.0605903409627,18.8640411739367));
#143278=CARTESIAN_POINT('Ctrl Pts',(20.5657233532605,21.0013801499083,18.8682122879177));
#143279=CARTESIAN_POINT('Ctrl Pts',(20.6224970485899,20.9393457112126,18.8723834018987));
#143280=CARTESIAN_POINT('Ctrl Pts',(20.6792516929575,20.8773320887721,18.8765531162222));
#143281=CARTESIAN_POINT('Ctrl Pts',(20.7329701367994,20.8124964399258,18.8807228305456));
#143282=CARTESIAN_POINT('Ctrl Pts',(20.7833688571021,20.745173160872,18.884892544869));
#143283=CARTESIAN_POINT('Ctrl Pts',(20.833765784002,20.6778522774696,18.8890621108161));
#143284=CARTESIAN_POINT('Ctrl Pts',(20.8808429472262,20.6080443086443,18.8932316767632));
#143285=CARTESIAN_POINT('Ctrl Pts',(20.9243585153512,20.5361149286867,18.8974012427103));
#143286=CARTESIAN_POINT('Ctrl Pts',(20.9694040370983,20.4616566005815,18.9017174054456));
#143287=CARTESIAN_POINT('Ctrl Pts',(21.0106325794989,20.3849253593978,18.9060335681809));
#143288=CARTESIAN_POINT('Ctrl Pts',(21.0478271756457,20.306355559279,18.9103497309162));
#143289=CARTESIAN_POINT('Ctrl Pts',(21.0838101617912,20.2303451620166,18.9145252951108));
#143290=CARTESIAN_POINT('Ctrl Pts',(21.1160178406327,20.1526146016966,18.9187008593055));
#143291=CARTESIAN_POINT('Ctrl Pts',(21.1443031849367,20.0735766961168,18.9228764235001));
#143292=CARTESIAN_POINT('Ctrl Pts',(21.1740171546712,19.9905467740118,18.9272628855057));
#143293=CARTESIAN_POINT('Ctrl Pts',(21.1994019743872,19.9060745270037,18.9316493475113));
#143294=CARTESIAN_POINT('Ctrl Pts',(21.2203472929199,19.8206532940858,18.9360358095169));
#143295=CARTESIAN_POINT('Ctrl Pts',(21.2412926114527,19.735232061168,18.9404222715225));
#143296=CARTESIAN_POINT('Ctrl Pts',(21.257798394603,19.6488624265219,18.9448087335281));
#143297=CARTESIAN_POINT('Ctrl Pts',(21.2698170137415,19.5620442604844,18.9491951955337));
#143298=CARTESIAN_POINT('Ctrl Pts',(21.2812826384042,19.4792207269144,18.9533798299225));
#143299=CARTESIAN_POINT('Ctrl Pts',(21.2887076244829,19.3956807451278,18.9575644643113));
#143300=CARTESIAN_POINT('Ctrl Pts',(21.2920126435715,19.3118529391169,18.9617490987001));
#143301=CARTESIAN_POINT('Ctrl Pts',(21.2953129583745,19.228144451612,18.9659277767799));
#143302=CARTESIAN_POINT('Ctrl Pts',(21.294504936491,19.1441494093845,18.9701064548596));
#143303=CARTESIAN_POINT('Ctrl Pts',(21.2895607321101,19.0603038006549,18.9742851329393));
#143304=CARTESIAN_POINT('Ctrl Pts',(21.2845279064127,18.9749553195403,18.9785387108258));
#143305=CARTESIAN_POINT('Ctrl Pts',(21.2752090914542,18.8897621593927,18.9827922887123));
#143306=CARTESIAN_POINT('Ctrl Pts',(21.2616304174303,18.8051866526579,18.9870458665988));
#143307=CARTESIAN_POINT('Ctrl Pts',(21.2483149925156,18.7222508072601,18.9912169805726));
#143308=CARTESIAN_POINT('Ctrl Pts',(21.2309034822292,18.6399093552897,18.9953880945464));
#143309=CARTESIAN_POINT('Ctrl Pts',(21.2094728610011,18.5585935971749,18.9995592085202));
#143310=CARTESIAN_POINT('Ctrl Pts',(21.1880494310247,18.4773051253474,19.0037289228364));
#143311=CARTESIAN_POINT('Ctrl Pts',(21.1626096856898,18.3970421082987,19.0078986371526));
#143312=CARTESIAN_POINT('Ctrl Pts',(21.1332813336496,18.3182239463334,19.0120683514689));
#143313=CARTESIAN_POINT('Ctrl Pts',(21.1039540252378,18.2394085890558,19.0162379174088));
#143314=CARTESIAN_POINT('Ctrl Pts',(21.0707385464732,18.1620384154915,19.0204074833488));
#143315=CARTESIAN_POINT('Ctrl Pts',(21.0338114728017,18.0865147001541,19.0245770492887));
#143316=CARTESIAN_POINT('Ctrl Pts',(20.9955860886931,18.0083356639876,19.0288932120326));
#143317=CARTESIAN_POINT('Ctrl Pts',(20.9533834858384,17.9321358186686,19.0332093747765));
#143318=CARTESIAN_POINT('Ctrl Pts',(20.9074514472649,17.8583327066931,19.0375255375203));
#143319=CARTESIAN_POINT('Ctrl Pts',(20.8630156401098,17.7869337234772,19.041701101708));
#143320=CARTESIAN_POINT('Ctrl Pts',(20.8150899458169,17.7177780846045,19.0458766658958));
#143321=CARTESIAN_POINT('Ctrl Pts',(20.7639418957711,17.6512128671536,19.0500522300835));
#143322=CARTESIAN_POINT('Ctrl Pts',(20.7102104791443,17.5812855985968,19.0544386921054));
#143323=CARTESIAN_POINT('Ctrl Pts',(20.6529230087042,17.5142177570107,19.0588251541274));
#143324=CARTESIAN_POINT('Ctrl Pts',(20.5924345734847,17.4503691653055,19.0632116161493));
#143325=CARTESIAN_POINT('Ctrl Pts',(20.5319461382652,17.3865205736004,19.0675980781713));
#143326=CARTESIAN_POINT('Ctrl Pts',(20.468257210959,17.3258915767387,19.0719845401932));
#143327=CARTESIAN_POINT('Ctrl Pts',(20.4017623229458,17.2687927931958,19.0763710022152));
#143328=CARTESIAN_POINT('Ctrl Pts',(20.3665290189526,17.2385381547066,19.0786952342651));
#143329=CARTESIAN_POINT('Ctrl Pts',(20.3304358403751,17.2092113636734,19.0810194663149));
#143330=CARTESIAN_POINT('Ctrl Pts',(20.2935357313021,17.1808649545431,19.0833436983648));
#143331=CARTESIAN_POINT('Origin',(18.734,19.211,-1.76670989022852));
#143332=CARTESIAN_POINT('',(20.2935357313021,17.1808649545432,19.9498236335591));
#143333=CARTESIAN_POINT('',(20.2935357313021,17.1808649545432,19.8833624920292));
#143334=CARTESIAN_POINT('',(20.2935357313021,17.1808649545432,-1.76670989022852));
#143335=CARTESIAN_POINT('',(16.1740009418753,19.2131959965388,19.4332901097715));
#143336=CARTESIAN_POINT('Ctrl Pts',(16.1740009418753,19.2131959965388,19.4332901097715));
#143337=CARTESIAN_POINT('Ctrl Pts',(16.1741094126172,19.3396465587508,19.4395926510338));
#143338=CARTESIAN_POINT('Ctrl Pts',(16.1835900621655,19.4657089276735,19.4458951922961));
#143339=CARTESIAN_POINT('Ctrl Pts',(16.2022529884087,19.5902849447293,19.4521977335585));
#143340=CARTESIAN_POINT('Ctrl Pts',(16.2064836512067,19.6185248420538,19.4536264444961));
#143341=CARTESIAN_POINT('Ctrl Pts',(16.2111860003675,19.6466884926971,19.4550551554337));
#143342=CARTESIAN_POINT('Ctrl Pts',(16.2163575306344,19.6747632978648,19.4564838663713));
#143343=CARTESIAN_POINT('Ctrl Pts',(16.2315047248246,19.7569932189491,19.4606685004926));
#143344=CARTESIAN_POINT('Ctrl Pts',(16.2507129697403,19.838633291604,19.4648531346138));
#143345=CARTESIAN_POINT('Ctrl Pts',(16.273922855402,19.9192516802849,19.4690377687351));
#143346=CARTESIAN_POINT('Ctrl Pts',(16.2970997046635,19.9997553186653,19.4732164465475));
#143347=CARTESIAN_POINT('Ctrl Pts',(16.3242667547551,20.0792397233557,19.4773951243598));
#143348=CARTESIAN_POINT('Ctrl Pts',(16.3553134075107,20.1572822489679,19.4815738021722));
#143349=CARTESIAN_POINT('Ctrl Pts',(16.3869165517625,20.2367236371946,19.4858273801256));
#143350=CARTESIAN_POINT('Ctrl Pts',(16.4225396637635,20.31467047214,19.4900809580789));
#143351=CARTESIAN_POINT('Ctrl Pts',(16.4620126245789,20.3906920640265,19.4943345360323));
#143352=CARTESIAN_POINT('Ctrl Pts',(16.500720321909,20.4652398230115,19.4985056497412));
#143353=CARTESIAN_POINT('Ctrl Pts',(16.543129704132,20.537935895187,19.5026767634501));
#143354=CARTESIAN_POINT('Ctrl Pts',(16.5890321382678,20.6083950308112,19.506847877159));
#143355=CARTESIAN_POINT('Ctrl Pts',(16.6349191694141,20.678830523216,19.5110175912119));
#143356=CARTESIAN_POINT('Ctrl Pts',(16.6842966737088,20.7470301846918,19.5151873052647));
#143357=CARTESIAN_POINT('Ctrl Pts',(16.7369115952943,20.8126360085207,19.5193570193175));
#143358=CARTESIAN_POINT('Ctrl Pts',(16.7895246446383,20.8782394978417,19.5235265849959));
#143359=CARTESIAN_POINT('Ctrl Pts',(16.845374593747,20.9412489746849,19.5276961506742));
#143360=CARTESIAN_POINT('Ctrl Pts',(16.9041676934323,21.0013389985813,19.5318657163526));
#143361=CARTESIAN_POINT('Ctrl Pts',(16.9650278943555,21.0635417221558,19.5361818794109));
#143362=CARTESIAN_POINT('Ctrl Pts',(17.0290416909492,21.1226154992726,19.5404980424693));
#143363=CARTESIAN_POINT('Ctrl Pts',(17.0958426218354,21.1782418266103,19.5448142055276));
#143364=CARTESIAN_POINT('Ctrl Pts',(17.1604675106422,21.2320561248729,19.5489897694609));
#143365=CARTESIAN_POINT('Ctrl Pts',(17.2277003349656,21.2826438809482,19.5531653333942));
#143366=CARTESIAN_POINT('Ctrl Pts',(17.2971780335787,21.3297596930302,19.5573408973275));
#143367=CARTESIAN_POINT('Ctrl Pts',(17.3701649002202,21.3792552227006,19.5617273599483));
#143368=CARTESIAN_POINT('Ctrl Pts',(17.4456288796132,21.4249185512742,19.5661138225692));
#143369=CARTESIAN_POINT('Ctrl Pts',(17.5231197837688,21.466519696642,19.5705002851901));
#143370=CARTESIAN_POINT('Ctrl Pts',(17.6006106879243,21.5081208420097,19.574886747811));
#143371=CARTESIAN_POINT('Ctrl Pts',(17.6801279596808,21.54565962526,19.5792732104319));
#143372=CARTESIAN_POINT('Ctrl Pts',(17.7611994326903,21.5789651720923,19.5836596730527));
#143373=CARTESIAN_POINT('Ctrl Pts',(17.8385406770856,21.6107382772506,19.587844307487));
#143374=CARTESIAN_POINT('Ctrl Pts',(17.9175841221713,21.6387774071546,19.5920289419213));
#143375=CARTESIAN_POINT('Ctrl Pts',(17.9979345050497,21.6628987717978,19.5962135763555));
#143376=CARTESIAN_POINT('Ctrl Pts',(18.0781705190567,21.6869858026501,19.6003922544782));
#143377=CARTESIAN_POINT('Ctrl Pts',(18.1597093389463,21.7071660136985,19.6045709326009));
#143378=CARTESIAN_POINT('Ctrl Pts',(18.2421357220941,21.723303630559,19.6087496107235));
#143379=CARTESIAN_POINT('Ctrl Pts',(18.3260395379464,21.7397305024131,19.613003188599));
#143380=CARTESIAN_POINT('Ctrl Pts',(18.4108626031778,21.751968244467,19.6172567664744));
#143381=CARTESIAN_POINT('Ctrl Pts',(18.4961506937664,21.7599267756301,19.6215103443499));
#143382=CARTESIAN_POINT('Ctrl Pts',(18.5797853091396,21.7677310152159,19.6256814583602));
#143383=CARTESIAN_POINT('Ctrl Pts',(18.6638666007977,21.7714204401678,19.6298525723706));
#143384=CARTESIAN_POINT('Ctrl Pts',(18.7479577055539,21.7709619494156,19.634023686381));
#143385=CARTESIAN_POINT('Ctrl Pts',(18.8320205926795,21.7705036125146,19.6381934007314));
#143386=CARTESIAN_POINT('Ctrl Pts',(18.9160928267202,21.7659001267025,19.6423631150818));
#143387=CARTESIAN_POINT('Ctrl Pts',(18.9997364062976,21.7571704896507,19.6465328294322));
#143388=CARTESIAN_POINT('Ctrl Pts',(19.0833770094289,21.7484411632419,19.6507023954039));
#143389=CARTESIAN_POINT('Ctrl Pts',(19.1665885309657,21.7355860261267,19.6548719613755));
#143390=CARTESIAN_POINT('Ctrl Pts',(19.2489383260605,21.7186759201209,19.6590415273471));
#143391=CARTESIAN_POINT('Ctrl Pts',(19.334183437007,21.7011712759268,19.6633576900461));
#143392=CARTESIAN_POINT('Ctrl Pts',(19.4185045808363,21.6793213182574,19.667673852745));
#143393=CARTESIAN_POINT('Ctrl Pts',(19.501435588217,21.653261783253,19.6719900154439));
#143394=CARTESIAN_POINT('Ctrl Pts',(19.581665127909,21.6280511344977,19.6761655796569));
#143395=CARTESIAN_POINT('Ctrl Pts',(19.6605932821677,21.5989011580776,19.68034114387));
#143396=CARTESIAN_POINT('Ctrl Pts',(19.737817188692,21.5659842996688,19.684516708083));
#143397=CARTESIAN_POINT('Ctrl Pts',(19.8189414894304,21.5314048897282,19.6889031700249));
#143398=CARTESIAN_POINT('Ctrl Pts',(19.8981843303167,21.4926683234582,19.6932896319667));
#143399=CARTESIAN_POINT('Ctrl Pts',(19.9751086547793,21.4500286525705,19.6976760939086));
#143400=CARTESIAN_POINT('Ctrl Pts',(20.052032979242,21.4073889816829,19.7020625558505));
#143401=CARTESIAN_POINT('Ctrl Pts',(20.1266383352643,21.3608465778203,19.7064490177923));
#143402=CARTESIAN_POINT('Ctrl Pts',(20.1985254700751,21.3107059669157,19.7108354797342));
#143403=CARTESIAN_POINT('Ctrl Pts',(20.2671049874815,21.2628723885244,19.7150201150502));
#143404=CARTESIAN_POINT('Ctrl Pts',(20.333466190131,21.2115863975067,19.7192047503662));
#143405=CARTESIAN_POINT('Ctrl Pts',(20.397240591338,21.1570808655669,19.7233893856822));
#143406=CARTESIAN_POINT('Ctrl Pts',(20.4609242176641,21.1026529154322,19.7275680646934));
#143407=CARTESIAN_POINT('Ctrl Pts',(20.5220280094148,21.0450148232166,19.7317467437045));
#143408=CARTESIAN_POINT('Ctrl Pts',(20.5802130388127,20.9844422503476,19.7359254227157));
#143409=CARTESIAN_POINT('Ctrl Pts',(20.6394409766828,20.922783974677,19.7401790003699));
#143410=CARTESIAN_POINT('Ctrl Pts',(20.6956440915829,20.8580852599725,19.7444325780241));
#143411=CARTESIAN_POINT('Ctrl Pts',(20.748500776934,20.7906792774903,19.7486861556782));
#143412=CARTESIAN_POINT('Ctrl Pts',(20.8003327466861,20.7245800731623,19.7528572705872));
#143413=CARTESIAN_POINT('Ctrl Pts',(20.8489465843895,20.655878012879,19.7570283854962));
#143414=CARTESIAN_POINT('Ctrl Pts',(20.8940779914836,20.5849225126288,19.7611995004052));
#143415=CARTESIAN_POINT('Ctrl Pts',(20.939194254295,20.5139908221869,19.7653692156561));
#143416=CARTESIAN_POINT('Ctrl Pts',(20.9808301605939,20.4408075813748,19.7695389309069));
#143417=CARTESIAN_POINT('Ctrl Pts',(21.0187646025393,20.3657513632741,19.7737086461577));
#143418=CARTESIAN_POINT('Ctrl Pts',(21.0566976945983,20.2906978160278,19.7778782130304));
#143419=CARTESIAN_POINT('Ctrl Pts',(21.0909293774397,20.2137718349661,19.7820477799031));
#143420=CARTESIAN_POINT('Ctrl Pts',(21.1212850353342,20.1353755514236,19.7862173467758));
#143421=CARTESIAN_POINT('Ctrl Pts',(21.1527079456892,20.0542229900628,19.7905335084124));
#143422=CARTESIAN_POINT('Ctrl Pts',(21.1799770112795,19.9714953041982,19.7948496700491));
#143423=CARTESIAN_POINT('Ctrl Pts',(21.2029540362409,19.887657939383,19.7991658316857));
#143424=CARTESIAN_POINT('Ctrl Pts',(21.2251825975767,19.8065515294293,19.8033413967921));
#143425=CARTESIAN_POINT('Ctrl Pts',(21.2433943908868,19.7244070949879,19.8075169618984));
#143426=CARTESIAN_POINT('Ctrl Pts',(21.257516353913,19.6416567212221,19.8116925270047));
#143427=CARTESIAN_POINT('Ctrl Pts',(21.2723515733316,19.5547268836692,19.8160789869065));
#143428=CARTESIAN_POINT('Ctrl Pts',(21.2826728879128,19.4671288669274,19.8204654468084));
#143429=CARTESIAN_POINT('Ctrl Pts',(21.2884573444648,19.3793676789345,19.8248519067102));
#143430=CARTESIAN_POINT('Ctrl Pts',(21.2942418010168,19.2916064909416,19.829238366612));
#143431=CARTESIAN_POINT('Ctrl Pts',(21.2954894673636,19.2036827129334,19.8336248265138));
#143432=CARTESIAN_POINT('Ctrl Pts',(21.2922402934572,19.1160968866051,19.8380112864157));
#143433=CARTESIAN_POINT('Ctrl Pts',(21.2891403572396,19.0325339616877,19.8421962719869));
#143434=CARTESIAN_POINT('Ctrl Pts',(21.281936068755,18.9489675609148,19.8463812575582));
#143435=CARTESIAN_POINT('Ctrl Pts',(21.27062378234,18.865833682311,19.8505662431294));
#143436=CARTESIAN_POINT('Ctrl Pts',(21.2593308428941,18.7828419843874,19.8547440712805));
#143437=CARTESIAN_POINT('Ctrl Pts',(21.2439439373047,18.7002817896674,19.8589218994317));
#143438=CARTESIAN_POINT('Ctrl Pts',(21.2245113674061,18.6185870284835,19.8630997275828));
#143439=CARTESIAN_POINT('Ctrl Pts',(21.205097707692,18.5369717659459,19.867273490214));
#143440=CARTESIAN_POINT('Ctrl Pts',(21.1816463054595,18.4562207098548,19.8714472528451));
#143441=CARTESIAN_POINT('Ctrl Pts',(21.1542568723911,18.3767598237656,19.8756210154763));
#143442=CARTESIAN_POINT('Ctrl Pts',(21.1268858754456,18.2973524236562,19.8797919687028));
#143443=CARTESIAN_POINT('Ctrl Pts',(21.0955822614867,18.219233902462,19.8839629219293));
#143444=CARTESIAN_POINT('Ctrl Pts',(21.0604958059402,18.1428159030661,19.8881338751558));
#143445=CARTESIAN_POINT('Ctrl Pts',(21.0254224420134,18.0664264171056,19.8923032720971));
#143446=CARTESIAN_POINT('Ctrl Pts',(20.9865692332511,17.9917366095586,19.8964726690383));
#143447=CARTESIAN_POINT('Ctrl Pts',(20.9441338701527,17.9191376714201,19.9006420659796));
#143448=CARTESIAN_POINT('Ctrl Pts',(20.9016818644379,17.84651026089,19.904813098106));
#143449=CARTESIAN_POINT('Ctrl Pts',(20.8556451221797,17.7759757602288,19.9089841302323));
#143450=CARTESIAN_POINT('Ctrl Pts',(20.8062666824223,17.7078996051752,19.9131551623587));
#143451=CARTESIAN_POINT('Ctrl Pts',(20.756880639062,17.6398129673268,19.9173268367668));
#143452=CARTESIAN_POINT('Ctrl Pts',(20.7041521537383,17.5741857944587,19.921498511175));
#143453=CARTESIAN_POINT('Ctrl Pts',(20.6483656429806,17.5113517466913,19.9256701855831));
#143454=CARTESIAN_POINT('Ctrl Pts',(20.5925104930342,17.448440388513,19.9298469927795));
#143455=CARTESIAN_POINT('Ctrl Pts',(20.5335901157611,17.3883293580182,19.9340237999759));
#143456=CARTESIAN_POINT('Ctrl Pts',(20.4719267477955,17.3313163512716,19.9382006071723));
#143457=CARTESIAN_POINT('Ctrl Pts',(20.4147287558635,17.278431962898,19.9420749493012));
#143458=CARTESIAN_POINT('Ctrl Pts',(20.3551712638459,17.2282129452766,19.9459492914302));
#143459=CARTESIAN_POINT('Ctrl Pts',(20.2935357313021,17.1808649545432,19.9498236335591));
#143460=CARTESIAN_POINT('Ctrl Pts',(20.2912840337091,17.1837659559064,19.1498287221711));
#143461=CARTESIAN_POINT('Ctrl Pts',(20.0133685819973,16.9682014306898,19.1672632324502));
#143462=CARTESIAN_POINT('Ctrl Pts',(18.916759280455,16.4174581264604,19.2270896782898));
#143463=CARTESIAN_POINT('Ctrl Pts',(16.8320816456072,16.9602242617438,19.3215765971066));
#143464=CARTESIAN_POINT('Ctrl Pts',(16.1790132394519,18.5174132428891,19.3986290056444));
#143465=CARTESIAN_POINT('Ctrl Pts',(16.1726852608311,19.213184455598,19.4332894786216));
#143466=CARTESIAN_POINT('',(16.1740010149448,19.2087204131752,19.3667098901939));
#143467=CARTESIAN_POINT('Ctrl Pts',(20.2935357313021,17.1808649545431,19.0833436983648));
#143468=CARTESIAN_POINT('Ctrl Pts',(20.227154634791,17.1298714543207,19.0875248532691));
#143469=CARTESIAN_POINT('Ctrl Pts',(20.1581601772516,17.082052917846,19.0917060081733));
#143470=CARTESIAN_POINT('Ctrl Pts',(20.0868893350051,17.0376867581433,19.0958871630776));
#143471=CARTESIAN_POINT('Ctrl Pts',(20.0157068252627,16.9933755854993,19.1000631358923));
#143472=CARTESIAN_POINT('Ctrl Pts',(19.9422539237334,16.9525085306642,19.1042391087071));
#143473=CARTESIAN_POINT('Ctrl Pts',(19.8668988922355,16.9153214292999,19.1084150815218));
#143474=CARTESIAN_POINT('Ctrl Pts',(19.7916121501407,16.8781680282063,19.1125872699219));
#143475=CARTESIAN_POINT('Ctrl Pts',(19.7144271146915,16.8446881560225,19.1167594583219));
#143476=CARTESIAN_POINT('Ctrl Pts',(19.6357379644307,16.8150724878444,19.1209316467219));
#143477=CARTESIAN_POINT('Ctrl Pts',(19.5570861679343,16.7854708782332,19.1251018545828));
#143478=CARTESIAN_POINT('Ctrl Pts',(19.4769321042154,16.7597299921337,19.1292720624437));
#143479=CARTESIAN_POINT('Ctrl Pts',(19.3956902142815,16.7379925070222,19.1334422703046));
#143480=CARTESIAN_POINT('Ctrl Pts',(19.3144625191379,16.7162588199397,19.1376117495361));
#143481=CARTESIAN_POINT('Ctrl Pts',(19.232147819739,16.6985272628336,19.1417812287676));
#143482=CARTESIAN_POINT('Ctrl Pts',(19.1491746923774,16.6848903478255,19.1459507079991));
#143483=CARTESIAN_POINT('Ctrl Pts',(19.0661911726319,16.6712517247938,19.1501207094579));
#143484=CARTESIAN_POINT('Ctrl Pts',(18.9825495153131,16.6617088355055,19.1542907109167));
#143485=CARTESIAN_POINT('Ctrl Pts',(18.8986860774795,16.6563026606104,19.1584607123754));
#143486=CARTESIAN_POINT('Ctrl Pts',(18.8147324189666,16.650890669727,19.1626351999413));
#143487=CARTESIAN_POINT('Ctrl Pts',(18.7305569635541,16.6496243068978,19.1668096875072));
#143488=CARTESIAN_POINT('Ctrl Pts',(18.6465982265326,16.6524924408955,19.1709841750731));
#143489=CARTESIAN_POINT('Ctrl Pts',(18.5625903672273,16.6553622529711,19.1751611050336));
#143490=CARTESIAN_POINT('Ctrl Pts',(18.4787999371148,16.6623713392017,19.179338034994));
#143491=CARTESIAN_POINT('Ctrl Pts',(18.3956600675484,16.6734566821217,19.1835149649545));
#143492=CARTESIAN_POINT('Ctrl Pts',(18.3123797908189,16.6845607460424,19.1876989489419));
#143493=CARTESIAN_POINT('Ctrl Pts',(18.2297527206121,16.6997547284267,19.1918829329294));
#143494=CARTESIAN_POINT('Ctrl Pts',(18.1482012114888,16.7189246039939,19.1960669169169));
#143495=CARTESIAN_POINT('Ctrl Pts',(18.0996034729978,16.7303482135597,19.1985602142434));
#143496=CARTESIAN_POINT('Ctrl Pts',(18.0513874007896,16.7431827575916,19.20105351157));
#143497=CARTESIAN_POINT('Ctrl Pts',(18.0036392138284,16.7573958913421,19.2035468088965));
#143498=CARTESIAN_POINT('Ctrl Pts',(17.9235008748349,16.7812505547995,19.2077314433106));
#143499=CARTESIAN_POINT('Ctrl Pts',(17.8443833236132,16.8090798944622,19.2119160777247));
#143500=CARTESIAN_POINT('Ctrl Pts',(17.7667095652053,16.8407786570123,19.2161007121388));
#143501=CARTESIAN_POINT('Ctrl Pts',(17.6891463657766,16.8724323002981,19.2202793902438));
#143502=CARTESIAN_POINT('Ctrl Pts',(17.6130232994518,16.9079442542207,19.2244580683488));
#143503=CARTESIAN_POINT('Ctrl Pts',(17.5387487593373,16.9471593537322,19.2286367464538));
#143504=CARTESIAN_POINT('Ctrl Pts',(17.4631429019463,16.9870773554683,19.232890324334));
#143505=CARTESIAN_POINT('Ctrl Pts',(17.3894529543325,17.0308324287606,19.2371439022142));
#143506=CARTESIAN_POINT('Ctrl Pts',(17.3180889421074,17.0782093688931,19.2413974800944));
#143507=CARTESIAN_POINT('Ctrl Pts',(17.2481084600744,17.1246678148849,19.2455685940934));
#143508=CARTESIAN_POINT('Ctrl Pts',(17.1803649335802,17.1746086808986,19.2497397080924));
#143509=CARTESIAN_POINT('Ctrl Pts',(17.1152190899139,17.2277833287458,19.2539108220915));
#143510=CARTESIAN_POINT('Ctrl Pts',(17.0500951065651,17.2809401333258,19.2580805364329));
#143511=CARTESIAN_POINT('Ctrl Pts',(16.9875674309667,17.337328274007,19.2622502507743));
#143512=CARTESIAN_POINT('Ctrl Pts',(16.9279649526866,17.3966578580996,19.2664199651157));
#143513=CARTESIAN_POINT('Ctrl Pts',(16.8683645953195,17.45598533099,19.2705895310807));
#143514=CARTESIAN_POINT('Ctrl Pts',(16.8116895537474,17.5182537140333,19.2747590970458));
#143515=CARTESIAN_POINT('Ctrl Pts',(16.7582319859915,17.5831361375039,19.2789286630108));
#143516=CARTESIAN_POINT('Ctrl Pts',(16.702894916699,17.6502997462159,19.2832448257247));
#143517=CARTESIAN_POINT('Ctrl Pts',(16.6510061189344,17.7202642276924,19.2875609884387));
#143518=CARTESIAN_POINT('Ctrl Pts',(16.6028430768051,17.7926311591414,19.2918771511526));
#143519=CARTESIAN_POINT('Ctrl Pts',(16.556248940208,17.8626407461605,19.2960527153649));
#143520=CARTESIAN_POINT('Ctrl Pts',(16.5131417547257,17.9348982385108,19.3002282795771));
#143521=CARTESIAN_POINT('Ctrl Pts',(16.4737266859811,18.0090164119531,19.3044038437894));
#143522=CARTESIAN_POINT('Ctrl Pts',(16.4323208564697,18.086878116905,19.3087903057542));
#143523=CARTESIAN_POINT('Ctrl Pts',(16.3949901703488,18.1667928797147,19.3131767677189));
#143524=CARTESIAN_POINT('Ctrl Pts',(16.3619151438302,18.2482884984951,19.3175632296837));
#143525=CARTESIAN_POINT('Ctrl Pts',(16.3288401173116,18.3297841172754,19.3219496916485));
#143526=CARTESIAN_POINT('Ctrl Pts',(16.3000208686933,18.4128600189268,19.3263361536133));
#143527=CARTESIAN_POINT('Ctrl Pts',(16.2755767948946,18.4970284707363,19.330722615578));
#143528=CARTESIAN_POINT('Ctrl Pts',(16.2465257453506,18.5970601546401,19.3359357942368));
#143529=CARTESIAN_POINT('Ctrl Pts',(16.2235642356451,18.6989346521906,19.3411489728956));
#143530=CARTESIAN_POINT('Ctrl Pts',(16.2068848499389,18.8019901977558,19.3463621515544));
#143531=CARTESIAN_POINT('Ctrl Pts',(16.1904712789818,18.9034033756426,19.3514922492292));
#143532=CARTESIAN_POINT('Ctrl Pts',(16.1801412136981,19.0059603454969,19.356622346904));
#143533=CARTESIAN_POINT('Ctrl Pts',(16.1760324691886,19.1090092586819,19.3617524445787));
#143534=CARTESIAN_POINT('Ctrl Pts',(16.1747089805831,19.1422028685768,19.3634049264505));
#143535=CARTESIAN_POINT('Ctrl Pts',(16.1740306434087,19.1754473495068,19.3650574083222));
#143536=CARTESIAN_POINT('Ctrl Pts',(16.1740010149447,19.2087204131752,19.3667098901939));
#143537=CARTESIAN_POINT('Ctrl Pts',(16.1740010149441,19.2087204138715,19.3667098902285));
#143538=CARTESIAN_POINT('Ctrl Pts',(16.173926819566,19.2920425969752,19.3708480242598));
#143539=CARTESIAN_POINT('Ctrl Pts',(16.1779248169782,19.3754486069208,19.374986158291));
#143540=CARTESIAN_POINT('Ctrl Pts',(16.1859928190663,19.4585063754938,19.3791242923223));
#143541=CARTESIAN_POINT('Ctrl Pts',(16.1940571655297,19.5415265104593,19.3832605513584));
#143542=CARTESIAN_POINT('Ctrl Pts',(16.2061878113245,19.6241982519121,19.3873968103945));
#143543=CARTESIAN_POINT('Ctrl Pts',(16.2223305526748,19.7060925038549,19.3915330694306));
#143544=CARTESIAN_POINT('Ctrl Pts',(16.2384710163523,19.7879752008633,19.395668744858));
#143545=CARTESIAN_POINT('Ctrl Pts',(16.2586223602412,19.8690801670325,19.3998044202854));
#143546=CARTESIAN_POINT('Ctrl Pts',(16.2826791433891,19.9489878440355,19.4039400957128));
#143547=CARTESIAN_POINT('Ctrl Pts',(16.3067400382207,20.0289091785212,19.4080764779923));
#143548=CARTESIAN_POINT('Ctrl Pts',(16.3347075604893,20.1076323699276,19.4122128602718));
#143549=CARTESIAN_POINT('Ctrl Pts',(16.3664266589092,20.1847538059263,19.4163492425514));
#143550=CARTESIAN_POINT('Ctrl Pts',(16.3981808282506,20.2619605129437,19.4204901983133));
#143551=CARTESIAN_POINT('Ctrl Pts',(16.4336946710478,20.3375614976538,19.4246311540753));
#143552=CARTESIAN_POINT('Ctrl Pts',(16.4727655806453,20.4111745292772,19.4287721098372));
#143553=CARTESIAN_POINT('Ctrl Pts',(16.5118617772824,20.4848352039083,19.4329157456625));
#143554=CARTESIAN_POINT('Ctrl Pts',(16.5545193804039,20.556504964772,19.4370593814878));
#143555=CARTESIAN_POINT('Ctrl Pts',(16.6004918491551,20.6258296612236,19.4412030173131));
#143556=CARTESIAN_POINT('Ctrl Pts',(16.6465392454204,20.6952673454551,19.4453534065789));
#143557=CARTESIAN_POINT('Ctrl Pts',(16.6959120078414,20.7623519651714,19.4495037958447));
#143558=CARTESIAN_POINT('Ctrl Pts',(16.7483230702952,20.826762089801,19.4536541851104));
#143559=CARTESIAN_POINT('Ctrl Pts',(16.7661884610687,20.848717608205,19.4550689308268));
#143560=CARTESIAN_POINT('Ctrl Pts',(16.7844065661404,20.8703626874017,19.4564836765431));
#143561=CARTESIAN_POINT('Ctrl Pts',(16.8029650799464,20.891685615317,19.4578984222595));
#143562=CARTESIAN_POINT('Ctrl Pts',(16.8578587574058,20.9547560712656,19.4620830566462));
#143563=CARTESIAN_POINT('Ctrl Pts',(16.915947800584,21.0152517076035,19.466267691033));
#143564=CARTESIAN_POINT('Ctrl Pts',(16.9769612646036,21.0728310563305,19.4704523254198));
#143565=CARTESIAN_POINT('Ctrl Pts',(17.0378878835037,21.1303284479763,19.4746310034971));
#143566=CARTESIAN_POINT('Ctrl Pts',(17.1017303233983,21.1849174841133,19.4788096815744));
#143567=CARTESIAN_POINT('Ctrl Pts',(17.1681782563646,21.2362906623887,19.4829883596517));
#143568=CARTESIAN_POINT('Ctrl Pts',(17.2358172209073,21.2885846680663,19.4872419375387));
#143569=CARTESIAN_POINT('Ctrl Pts',(17.306155687672,21.3375460297098,19.4914955154258));
#143570=CARTESIAN_POINT('Ctrl Pts',(17.3788280009098,21.382890617154,19.4957490933129));
#143571=CARTESIAN_POINT('Ctrl Pts',(17.4500914193923,21.4273561111915,19.4999202072833));
#143572=CARTESIAN_POINT('Ctrl Pts',(17.5235985912763,21.46834356131,19.5040913212538));
#143573=CARTESIAN_POINT('Ctrl Pts',(17.5989738385243,21.5056275542592,19.5082624352243));
#143574=CARTESIAN_POINT('Ctrl Pts',(17.6743237928747,21.5428990362019,19.5124321495369));
#143575=CARTESIAN_POINT('Ctrl Pts',(17.7515401656511,21.5764693252641,19.5166018638495));
#143576=CARTESIAN_POINT('Ctrl Pts',(17.8302229081156,21.6061590694952,19.5207715781621));
#143577=CARTESIAN_POINT('Ctrl Pts',(17.9089028507052,21.6358477572358,19.5249411440981));
#143578=CARTESIAN_POINT('Ctrl Pts',(17.9890486285244,21.6616560130853,19.5291107100341));
#143579=CARTESIAN_POINT('Ctrl Pts',(18.0702417419437,21.6834532300656,19.5332802759701));
#143580=CARTESIAN_POINT('Ctrl Pts',(18.1542895053988,21.7060168103939,19.5375964387177));
#143581=CARTESIAN_POINT('Ctrl Pts',(18.2394591140179,21.724281910891,19.5419126014652));
#143582=CARTESIAN_POINT('Ctrl Pts',(18.3252730114509,21.7381609067947,19.5462287642128));
#143583=CARTESIAN_POINT('Ctrl Pts',(18.4082915298627,21.751587795812,19.5504043283958));
#143584=CARTESIAN_POINT('Ctrl Pts',(18.4919125329025,21.7609099414411,19.5545798925789));
#143585=CARTESIAN_POINT('Ctrl Pts',(18.5756985998726,21.7661009112592,19.5587554567619));
#143586=CARTESIAN_POINT('Ctrl Pts',(18.6637165024322,21.7715540646553,19.5631419187917));
#143587=CARTESIAN_POINT('Ctrl Pts',(18.7519159980506,21.7724477372193,19.5675283808216));
#143588=CARTESIAN_POINT('Ctrl Pts',(18.8397925195448,21.7688131172563,19.5719148428514));
#143589=CARTESIAN_POINT('Ctrl Pts',(18.9276690410391,21.7651784972933,19.5763013048812));
#143590=CARTESIAN_POINT('Ctrl Pts',(19.0152220177587,21.7570157144011,19.5806877669111));
#143591=CARTESIAN_POINT('Ctrl Pts',(19.1019580505816,21.7444180217667,19.5850742289409));
#143592=CARTESIAN_POINT('Ctrl Pts',(19.1847032324206,21.7323999672873,19.5892588634748));
#143593=CARTESIAN_POINT('Ctrl Pts',(19.2670129891846,21.7163014146095,19.5934434980088));
#143594=CARTESIAN_POINT('Ctrl Pts',(19.3484535429759,21.6961653553686,19.5976281325427));
#143595=CARTESIAN_POINT('Ctrl Pts',(19.4297781762334,21.6760579573122,19.6018068107681));
#143596=CARTESIAN_POINT('Ctrl Pts',(19.5102356212268,21.6519245772983,19.6059854889935));
#143597=CARTESIAN_POINT('Ctrl Pts',(19.5893993424999,21.6238597068315,19.6101641672189));
#143598=CARTESIAN_POINT('Ctrl Pts',(19.6699820131869,21.5952917949353,19.614417745069));
#143599=CARTESIAN_POINT('Ctrl Pts',(19.7492236469471,21.562650131979,19.6186713229191));
#143600=CARTESIAN_POINT('Ctrl Pts',(19.8266874127913,21.5260883823145,19.6229249007693));
#143601=CARTESIAN_POINT('Ctrl Pts',(19.9026493955877,21.490235451996,19.627096014889));
#143602=CARTESIAN_POINT('Ctrl Pts',(19.9769013948568,21.4506132807146,19.6312671290086));
#143603=CARTESIAN_POINT('Ctrl Pts',(20.0490505263125,21.4074157423505,19.6354382431283));
#143604=CARTESIAN_POINT('Ctrl Pts',(20.1211754474276,21.3642326993392,19.6396079575902));
#143605=CARTESIAN_POINT('Ctrl Pts',(20.1911985077687,21.3174769080841,19.6437776720521));
#143606=CARTESIAN_POINT('Ctrl Pts',(20.2587523619162,21.2673876664751,19.6479473865139));
#143607=CARTESIAN_POINT('Ctrl Pts',(20.3263038122014,21.2173002072608,19.6521169525991));
#143608=CARTESIAN_POINT('Ctrl Pts',(20.3913858619656,21.1638798082203,19.6562865186843));
#143609=CARTESIAN_POINT('Ctrl Pts',(20.4536621654798,21.1074076662515,19.6604560847694));
#143610=CARTESIAN_POINT('Ctrl Pts',(20.5181280223105,21.0489500376889,19.6647722473405));
#143611=CARTESIAN_POINT('Ctrl Pts',(20.5795867715906,20.9872224295952,19.6690884099116));
#143612=CARTESIAN_POINT('Ctrl Pts',(20.6377062426226,20.9225789616024,19.6734045724827));
#143613=CARTESIAN_POINT('Ctrl Pts',(20.6939324820534,20.8600412432703,19.6775801368131));
#143614=CARTESIAN_POINT('Ctrl Pts',(20.7470333951756,20.7947751107948,19.6817557011435));
#143615=CARTESIAN_POINT('Ctrl Pts',(20.7967499889561,20.7271340584069,19.6859312654739));
#143616=CARTESIAN_POINT('Ctrl Pts',(20.8489776441397,20.6560766248273,19.6903177271653));
#143617=CARTESIAN_POINT('Ctrl Pts',(20.8974697909607,20.5823985401433,19.6947041888567));
#143618=CARTESIAN_POINT('Ctrl Pts',(20.9419795412567,20.5065409470147,19.6990906505481));
#143619=CARTESIAN_POINT('Ctrl Pts',(20.9864892915527,20.4306833538862,19.7034771122395));
#143620=CARTESIAN_POINT('Ctrl Pts',(21.0270164454128,20.3526468022886,19.7078635739309));
#143621=CARTESIAN_POINT('Ctrl Pts',(21.0633723464503,20.2728966388461,19.7122500356223));
#143622=CARTESIAN_POINT('Ctrl Pts',(21.0980554588848,20.1968158979922,19.7164346697447));
#143623=CARTESIAN_POINT('Ctrl Pts',(21.1290718315298,20.1188925846167,19.7206193038671));
#143624=CARTESIAN_POINT('Ctrl Pts',(21.1562228177911,20.0395147077584,19.7248039379896));
#143625=CARTESIAN_POINT('Ctrl Pts',(21.1833351579832,19.9602498154855,19.7289826158031));
#143626=CARTESIAN_POINT('Ctrl Pts',(21.2065928926838,19.8795349037293,19.7331612936167));
#143627=CARTESIAN_POINT('Ctrl Pts',(21.2258445987322,19.797779767689,19.7373399714302));
#143628=CARTESIAN_POINT('Ctrl Pts',(21.2454413793552,19.7145592228834,19.7415935493833));
#143629=CARTESIAN_POINT('Ctrl Pts',(21.2608869019344,19.6302612334803,19.7458471273363));
#143630=CARTESIAN_POINT('Ctrl Pts',(21.2720739254944,19.5453362808994,19.7501007052894));
#143631=CARTESIAN_POINT('Ctrl Pts',(21.283044065894,19.4620577709145,19.7542718189995));
#143632=CARTESIAN_POINT('Ctrl Pts',(21.2899192902207,19.3781768678188,19.7584429327095));
#143633=CARTESIAN_POINT('Ctrl Pts',(21.2926499549084,19.2941288653065,19.7626140464196));
#143634=CARTESIAN_POINT('Ctrl Pts',(21.2953797032962,19.2101090658848,19.7667837604736));
#143635=CARTESIAN_POINT('Ctrl Pts',(21.2939676391619,19.1259227378138,19.7709534745275));
#143636=CARTESIAN_POINT('Ctrl Pts',(21.2884161370472,19.0420082877982,19.7751231885815));
#143637=CARTESIAN_POINT('Ctrl Pts',(21.2828648324763,18.958096823782,19.779292754261));
#143638=CARTESIAN_POINT('Ctrl Pts',(21.2731744140079,18.8744576775594,19.7834623199405));
#143639=CARTESIAN_POINT('Ctrl Pts',(21.2593992661634,18.7915258691394,19.78763188562));
#143640=CARTESIAN_POINT('Ctrl Pts',(21.2451397991587,18.7056782688699,19.791948048677));
#143641=CARTESIAN_POINT('Ctrl Pts',(21.2265031054902,18.620589192361,19.796264211734));
#143642=CARTESIAN_POINT('Ctrl Pts',(21.2036071461028,18.5367296210585,19.800580374791));
#143643=CARTESIAN_POINT('Ctrl Pts',(21.1814570231814,18.4556017774482,19.8047559387253));
#143644=CARTESIAN_POINT('Ctrl Pts',(21.1553210566048,18.3756249996566,19.8089315026597));
#143645=CARTESIAN_POINT('Ctrl Pts',(21.1253562910671,18.2972083994839,19.8131070665941));
#143646=CARTESIAN_POINT('Ctrl Pts',(21.09387807017,18.2148311468024,19.8174935292124));
#143647=CARTESIAN_POINT('Ctrl Pts',(21.0581743347953,18.1341763575253,19.8218799918307));
#143648=CARTESIAN_POINT('Ctrl Pts',(21.0184823804552,18.0556904079903,19.8262664544489));
#143649=CARTESIAN_POINT('Ctrl Pts',(20.9787904261151,17.9772044584552,19.8306529170672));
#143650=CARTESIAN_POINT('Ctrl Pts',(20.9351106070445,17.9008878144474,19.8350393796855));
#143651=CARTESIAN_POINT('Ctrl Pts',(20.8877320902706,17.827150989689,19.8394258423038));
#143652=CARTESIAN_POINT('Ctrl Pts',(20.8425432910205,17.7568220980682,19.8436095735004));
#143653=CARTESIAN_POINT('Ctrl Pts',(20.7938219698918,17.6885781039191,19.847793304697));
#143654=CARTESIAN_POINT('Ctrl Pts',(20.7417867108851,17.6227958180407,19.8519770358936));
#143655=CARTESIAN_POINT('Ctrl Pts',(20.6898163394592,17.5570955621832,19.8561555500085));
#143656=CARTESIAN_POINT('Ctrl Pts',(20.6345405135866,17.4938512802473,19.8603340641234));
#143657=CARTESIAN_POINT('Ctrl Pts',(20.5762218026546,17.4334120753606,19.8645125782384));
#143658=CARTESIAN_POINT('Ctrl Pts',(20.5179688787998,17.373041049598,19.8686863787335));
#143659=CARTESIAN_POINT('Ctrl Pts',(20.456680209176,17.3154691416453,19.8728601792286));
#143660=CARTESIAN_POINT('Ctrl Pts',(20.3926584428866,17.2610122641819,19.8770339797238));
#143661=CARTESIAN_POINT('Ctrl Pts',(20.3603008400853,17.2334889059104,19.8791434838256));
#143662=CARTESIAN_POINT('Ctrl Pts',(20.3272457056729,17.2067607242114,19.8812529879274));
#143663=CARTESIAN_POINT('Ctrl Pts',(20.2935357313021,17.1808649545432,19.8833624920292));
#143664=CARTESIAN_POINT('Origin',(18.734,19.211,-1.76670989022852));
#143665=CARTESIAN_POINT('',(20.2935357313021,17.1808649545431,20.7499611463308));
#143666=CARTESIAN_POINT('',(20.2916962192317,17.183223495321,20.6832232112625));
#143667=CARTESIAN_POINT('',(20.2935357313021,17.1808649545432,-1.76670989022852));
#143668=CARTESIAN_POINT('',(16.1740004726297,19.2094444088938,20.2332901098006));
#143669=CARTESIAN_POINT('Ctrl Pts',(16.1740004726297,19.2094444088938,20.2332901098006));
#143670=CARTESIAN_POINT('Ctrl Pts',(16.1739502760983,19.2920516545602,20.2374173417146));
#143671=CARTESIAN_POINT('Ctrl Pts',(16.1779027082651,19.3748187791154,20.2415445736285));
#143672=CARTESIAN_POINT('Ctrl Pts',(16.1858778001794,19.4573194161684,20.2456718055424));
#143673=CARTESIAN_POINT('Ctrl Pts',(16.1940130436991,19.5414767876655,20.249881918359));
#143674=CARTESIAN_POINT('Ctrl Pts',(16.2063343518328,19.6253563595504,20.2540920311757));
#143675=CARTESIAN_POINT('Ctrl Pts',(16.222807033423,19.7085036528651,20.2583021439923));
#143676=CARTESIAN_POINT('Ctrl Pts',(16.2389199317254,19.7898349087365,20.2624203028533));
#143677=CARTESIAN_POINT('Ctrl Pts',(16.2590046102348,19.8704650577792,20.2665384617144));
#143678=CARTESIAN_POINT('Ctrl Pts',(16.2829763020121,19.9499741753957,20.2706566205754));
#143679=CARTESIAN_POINT('Ctrl Pts',(16.3069370246241,20.0294469105714,20.2747728950152));
#143680=CARTESIAN_POINT('Ctrl Pts',(16.334781094809,20.1077991798405,20.278889169455));
#143681=CARTESIAN_POINT('Ctrl Pts',(16.3663732871992,20.1846240284793,20.2830054438948));
#143682=CARTESIAN_POINT('Ctrl Pts',(16.3979610861523,20.2614381933028,20.2871211458959));
#143683=CARTESIAN_POINT('Ctrl Pts',(16.4332957916267,20.3367249220046,20.291236847897));
#143684=CARTESIAN_POINT('Ctrl Pts',(16.4721937795329,20.4100965853743,20.2953525498981));
#143685=CARTESIAN_POINT('Ctrl Pts',(16.5126461135564,20.4864001474415,20.2996327135017));
#143686=CARTESIAN_POINT('Ctrl Pts',(16.5569522565608,20.5606318773211,20.3039128771053));
#143687=CARTESIAN_POINT('Ctrl Pts',(16.6048536565745,20.6323851864564,20.3081930407089));
#143688=CARTESIAN_POINT('Ctrl Pts',(16.6509736168395,20.7014700099742,20.3123140262181));
#143689=CARTESIAN_POINT('Ctrl Pts',(16.700425807859,20.7682571429841,20.3164350117273));
#143690=CARTESIAN_POINT('Ctrl Pts',(16.7529371454851,20.832416037438,20.3205559972365));
#143691=CARTESIAN_POINT('Ctrl Pts',(16.8054841275711,20.8966184826611,20.3246797800521));
#143692=CARTESIAN_POINT('Ctrl Pts',(16.8610940675905,20.9581887928557,20.3288035628677));
#143693=CARTESIAN_POINT('Ctrl Pts',(16.9194565998598,21.0168328408266,20.3329273456833));
#143694=CARTESIAN_POINT('Ctrl Pts',(16.9779086865543,21.0755668751946,20.3370574562401));
#143695=CARTESIAN_POINT('Ctrl Pts',(17.0391214360201,21.1313653808553,20.3411875667969));
#143696=CARTESIAN_POINT('Ctrl Pts',(17.102751683912,21.1839746402982,20.3453176773537));
#143697=CARTESIAN_POINT('Ctrl Pts',(17.1099251002331,21.189905595038,20.3457832892829));
#143698=CARTESIAN_POINT('Ctrl Pts',(17.1171292123955,21.1957960624817,20.3462489012121));
#143699=CARTESIAN_POINT('Ctrl Pts',(17.1243635072226,21.201645714616,20.3467145131413));
#143700=CARTESIAN_POINT('Ctrl Pts',(17.189381078246,21.254218934563,20.3508991582794));
#143701=CARTESIAN_POINT('Ctrl Pts',(17.2570980356913,21.3037012786361,20.3550838034176));
#143702=CARTESIAN_POINT('Ctrl Pts',(17.3271882231611,21.349803549779,20.3592684485557));
#143703=CARTESIAN_POINT('Ctrl Pts',(17.3971786443956,21.3958401990397,20.3634471372781));
#143704=CARTESIAN_POINT('Ctrl Pts',(17.469535204727,21.4385060812658,20.3676258260006));
#143705=CARTESIAN_POINT('Ctrl Pts',(17.5438988654553,21.477552291379,20.371804514723));
#143706=CARTESIAN_POINT('Ctrl Pts',(17.619595201075,21.5172982505808,20.3760580899355));
#143707=CARTESIAN_POINT('Ctrl Pts',(17.6973709112596,21.5532932167484,20.380311665148));
#143708=CARTESIAN_POINT('Ctrl Pts',(17.7768165359119,21.5853209168257,20.3845652403605));
#143709=CARTESIAN_POINT('Ctrl Pts',(17.8547221935262,21.6167277947667,20.3887363646432));
#143710=CARTESIAN_POINT('Ctrl Pts',(17.9342331579703,21.6443196566906,20.3929074889259));
#143711=CARTESIAN_POINT('Ctrl Pts',(18.0149402978302,21.6679397926517,20.3970786132086));
#143712=CARTESIAN_POINT('Ctrl Pts',(18.0956203528785,21.6915520018428,20.401248337688));
#143713=CARTESIAN_POINT('Ctrl Pts',(18.1774953449549,21.711195003098,20.4054180621675));
#143714=CARTESIAN_POINT('Ctrl Pts',(18.2601401458989,21.7267616816128,20.409587786647));
#143715=CARTESIAN_POINT('Ctrl Pts',(18.3427820028614,21.7423278056098,20.4137573625921));
#143716=CARTESIAN_POINT('Ctrl Pts',(18.4261931619305,21.7538178112606,20.4179269385372));
#143717=CARTESIAN_POINT('Ctrl Pts',(18.5099387942264,21.7611757931694,20.4220965144823));
#143718=CARTESIAN_POINT('Ctrl Pts',(18.5966283647877,21.7687924326811,20.4264126649273));
#143719=CARTESIAN_POINT('Ctrl Pts',(18.6836758371975,21.7719810786796,20.4307288153724));
#143720=CARTESIAN_POINT('Ctrl Pts',(18.7705956997401,21.7707384152996,20.4350449658174));
#143721=CARTESIAN_POINT('Ctrl Pts',(18.8546845879267,21.7695362253863,20.4392205395189));
#143722=CARTESIAN_POINT('Ctrl Pts',(18.9386535840454,21.7641870268946,20.4433961132204));
#143723=CARTESIAN_POINT('Ctrl Pts',(19.0220673263575,21.7547407917249,20.4475716869219));
#143724=CARTESIAN_POINT('Ctrl Pts',(19.1096934355563,21.7448175247481,20.4519581257387));
#143725=CARTESIAN_POINT('Ctrl Pts',(19.1967061584005,21.7303726255243,20.4563445645555));
#143726=CARTESIAN_POINT('Ctrl Pts',(19.2826140302886,21.7115244741395,20.4607310033723));
#143727=CARTESIAN_POINT('Ctrl Pts',(19.3685219021767,21.6926763227546,20.4651174421892));
#143728=CARTESIAN_POINT('Ctrl Pts',(19.4533243836773,21.6694251459735,20.469503881006));
#143729=CARTESIAN_POINT('Ctrl Pts',(19.5365517912822,21.6419485026034,20.4738903198228));
#143730=CARTESIAN_POINT('Ctrl Pts',(19.6159508693926,21.6157357414958,20.4780749893718));
#143731=CARTESIAN_POINT('Ctrl Pts',(19.6942121038407,21.5855801437023,20.4822596589207));
#143732=CARTESIAN_POINT('Ctrl Pts',(19.770915780013,21.551599424327,20.4864443284697));
#143733=CARTESIAN_POINT('Ctrl Pts',(19.8475102835633,21.5176670698335,20.4906230419632));
#143734=CARTESIAN_POINT('Ctrl Pts',(19.9225512152564,21.4799205926128,20.4948017554568));
#143735=CARTESIAN_POINT('Ctrl Pts',(19.9956349417348,21.4385271656691,20.4989804689503));
#143736=CARTESIAN_POINT('Ctrl Pts',(20.0700278568189,21.3963922357189,20.5032340380151));
#143737=CARTESIAN_POINT('Ctrl Pts',(20.1423922957485,21.3504785578701,20.5074876070798));
#143738=CARTESIAN_POINT('Ctrl Pts',(20.2123247807266,21.3010133594524,20.5117411761446));
#143739=CARTESIAN_POINT('Ctrl Pts',(20.2809022183518,21.2525066238464,20.5159123258944));
#143740=CARTESIAN_POINT('Ctrl Pts',(20.3471407141715,21.2005850501782,20.5200834756442));
#143741=CARTESIAN_POINT('Ctrl Pts',(20.4106870428273,21.1455078341571,20.5242546253941));
#143742=CARTESIAN_POINT('Ctrl Pts',(20.4742120489457,21.0904490989203,20.528424375543));
#143743=CARTESIAN_POINT('Ctrl Pts',(20.5350463346099,21.032237125278,20.532594125692));
#143744=CARTESIAN_POINT('Ctrl Pts',(20.5928697176814,20.9711714043487,20.536763875841));
#143745=CARTESIAN_POINT('Ctrl Pts',(20.650691043295,20.9101078562456,20.5409334776229));
#143746=CARTESIAN_POINT('Ctrl Pts',(20.705501363646,20.8461910973649,20.5451030794048));
#143747=CARTESIAN_POINT('Ctrl Pts',(20.7570183049857,20.7797564940719,20.5492726811867));
#143748=CARTESIAN_POINT('Ctrl Pts',(20.8103455374923,20.7109873970688,20.5535888016298));
#143749=CARTESIAN_POINT('Ctrl Pts',(20.8601432984269,20.639520622689,20.557904922073));
#143750=CARTESIAN_POINT('Ctrl Pts',(20.9061460099819,20.5657626033071,20.5622210425161));
#143751=CARTESIAN_POINT('Ctrl Pts',(20.9506510024677,20.4944059378543,20.5663966422013));
#143752=CARTESIAN_POINT('Ctrl Pts',(20.9916040779513,20.4209053655083,20.5705722418866));
#143753=CARTESIAN_POINT('Ctrl Pts',(21.0288115998389,20.3456540094871,20.5747478415718));
#143754=CARTESIAN_POINT('Ctrl Pts',(21.0678973294938,20.2666040215169,20.5791342223939));
#143755=CARTESIAN_POINT('Ctrl Pts',(21.1028491780513,20.185622378127,20.583520603216));
#143756=CARTESIAN_POINT('Ctrl Pts',(21.1335006707343,20.1031863769111,20.5879069840381));
#143757=CARTESIAN_POINT('Ctrl Pts',(21.1641521634173,20.0207503756951,20.5922933648601));
#143758=CARTESIAN_POINT('Ctrl Pts',(21.190503198923,19.9368605929086,20.5966797456822));
#143759=CARTESIAN_POINT('Ctrl Pts',(21.2124488472496,19.8520080432935,20.6010661265043));
#143760=CARTESIAN_POINT('Ctrl Pts',(21.2333845649191,19.7710603767749,20.6052506476957));
#143761=CARTESIAN_POINT('Ctrl Pts',(21.2503893834586,19.6889352855203,20.6094351688871));
#143762=CARTESIAN_POINT('Ctrl Pts',(21.2633350895848,19.6060493698199,20.6136196900785));
#143763=CARTESIAN_POINT('Ctrl Pts',(21.2762623681897,19.5232814377935,20.6177982548275));
#143764=CARTESIAN_POINT('Ctrl Pts',(21.2851419407632,19.4397552831427,20.6219768195765));
#143765=CARTESIAN_POINT('Ctrl Pts',(21.2898958841357,19.3559007572727,20.6261553843255));
#143766=CARTESIAN_POINT('Ctrl Pts',(21.294735201995,19.2705403158831,20.630408990528));
#143767=CARTESIAN_POINT('Ctrl Pts',(21.2952991221744,19.1848400591972,20.6346625967305));
#143768=CARTESIAN_POINT('Ctrl Pts',(21.291560298618,19.0992622761417,20.638916202933));
#143769=CARTESIAN_POINT('Ctrl Pts',(21.2878940830536,19.015346414515,20.6430872040592));
#143770=CARTESIAN_POINT('Ctrl Pts',(21.2800907693894,18.9315487929963,20.6472582051854));
#143771=CARTESIAN_POINT('Ctrl Pts',(21.2681770979566,18.848306691277,20.6514292063116));
#143772=CARTESIAN_POINT('Ctrl Pts',(21.2562674231734,18.7650925145781,20.6555988082025));
#143773=CARTESIAN_POINT('Ctrl Pts',(21.2402501942426,18.6824339426084,20.6597684100934));
#143774=CARTESIAN_POINT('Ctrl Pts',(21.2202039193129,18.6007622827183,20.6639380119843));
#143775=CARTESIAN_POINT('Ctrl Pts',(21.200158355009,18.5190935180289,20.6681074660658));
#143776=CARTESIAN_POINT('Ctrl Pts',(21.1760841391767,18.4384120424545,20.6722769201474));
#143777=CARTESIAN_POINT('Ctrl Pts',(21.1481104103813,18.3591367912108,20.6764463742289));
#143778=CARTESIAN_POINT('Ctrl Pts',(21.1191514849296,18.2770695735106,20.6807626708086));
#143779=CARTESIAN_POINT('Ctrl Pts',(21.0860134223638,18.1965099777348,20.6850789673884));
#143780=CARTESIAN_POINT('Ctrl Pts',(21.0488942540617,18.1179013802442,20.6893952639681));
#143781=CARTESIAN_POINT('Ctrl Pts',(21.0129862924117,18.0418577986347,20.693570718838));
#143782=CARTESIAN_POINT('Ctrl Pts',(20.9733533011739,17.9676402439561,20.697746173708));
#143783=CARTESIAN_POINT('Ctrl Pts',(20.9302210181299,17.895624297197,20.7019216285779));
#143784=CARTESIAN_POINT('Ctrl Pts',(20.8849064011797,17.8199646100351,20.7063083460125));
#143785=CARTESIAN_POINT('Ctrl Pts',(20.8357293767457,17.7467356778435,20.7106950634472));
#143786=CARTESIAN_POINT('Ctrl Pts',(20.7830012664589,17.6763359292504,20.7150817808818));
#143787=CARTESIAN_POINT('Ctrl Pts',(20.7302731561721,17.6059361806573,20.7194684983164));
#143788=CARTESIAN_POINT('Ctrl Pts',(20.6739943900424,17.5383660129748,20.723855215751));
#143789=CARTESIAN_POINT('Ctrl Pts',(20.6145211534981,17.4739795075341,20.7282419331856));
#143790=CARTESIAN_POINT('Ctrl Pts',(20.5577980728116,17.4125703568735,20.7324258004418));
#143791=CARTESIAN_POINT('Ctrl Pts',(20.497958300527,17.3538283604302,20.7366096676979));
#143792=CARTESIAN_POINT('Ctrl Pts',(20.4352825901188,17.2980866332845,20.740793534954));
#143793=CARTESIAN_POINT('Ctrl Pts',(20.3895046434955,17.2573732246395,20.7438494054129));
#143794=CARTESIAN_POINT('Ctrl Pts',(20.3422147220435,17.2182598192813,20.7469052758719));
#143795=CARTESIAN_POINT('Ctrl Pts',(20.2935357313021,17.1808649545431,20.7499611463308));
#143796=CARTESIAN_POINT('Ctrl Pts',(20.2935357313021,17.1808649545432,19.9498236335591));
#143797=CARTESIAN_POINT('Ctrl Pts',(20.2269623905211,17.1297237735993,19.9540083609104));
#143798=CARTESIAN_POINT('Ctrl Pts',(20.1579647730342,17.081932789023,19.9581930882618));
#143799=CARTESIAN_POINT('Ctrl Pts',(20.0869226296604,17.0377074844483,19.9623778156132));
#143800=CARTESIAN_POINT('Ctrl Pts',(20.0710253698527,17.0278110888231,19.9633142414411));
#143801=CARTESIAN_POINT('Ctrl Pts',(20.0550258220092,17.0180930547612,19.9642506672691));
#143802=CARTESIAN_POINT('Ctrl Pts',(20.0389283877504,17.0085554711087,19.965187093097));
#143803=CARTESIAN_POINT('Ctrl Pts',(19.9669932812562,16.9659345735974,19.9693717283982));
#143804=CARTESIAN_POINT('Ctrl Pts',(19.8928340180633,16.9267623273783,19.9735563636994));
#143805=CARTESIAN_POINT('Ctrl Pts',(19.8168151370682,16.8912777366814,19.9777409990006));
#143806=CARTESIAN_POINT('Ctrl Pts',(19.7409044598177,16.8558436540364,19.9819196779762));
#143807=CARTESIAN_POINT('Ctrl Pts',(19.6631398357153,16.8240869937955,19.9860983569517));
#143808=CARTESIAN_POINT('Ctrl Pts',(19.5839125153273,16.796202137592,19.9902770359273));
#143809=CARTESIAN_POINT('Ctrl Pts',(19.5032651236343,16.7678174729394,19.9945306135878));
#143810=CARTESIAN_POINT('Ctrl Pts',(19.4211024978258,16.7434450253959,19.9987841912482));
#143811=CARTESIAN_POINT('Ctrl Pts',(19.337861066102,16.7232395989874,20.0030377689087));
#143812=CARTESIAN_POINT('Ctrl Pts',(19.2562334111056,16.7034258891344,20.0072088837319));
#143813=CARTESIAN_POINT('Ctrl Pts',(19.1735688735385,16.6876191861435,20.0113799985551));
#143814=CARTESIAN_POINT('Ctrl Pts',(19.0902949413653,16.6759154028401,20.0155511133783));
#143815=CARTESIAN_POINT('Ctrl Pts',(19.0070489529371,16.6642155469066,20.019720828525));
#143816=CARTESIAN_POINT('Ctrl Pts',(18.9231944312015,16.6566159403015,20.0238905436717));
#143817=CARTESIAN_POINT('Ctrl Pts',(18.8391675225352,16.6531611090212,20.0280602588184));
#143818=CARTESIAN_POINT('Ctrl Pts',(18.7551436043077,16.649706400695,20.0322298255688));
#143819=CARTESIAN_POINT('Ctrl Pts',(18.6709477710271,16.6503961924556,20.0363993923192));
#143820=CARTESIAN_POINT('Ctrl Pts',(18.5870183641888,16.6552229364175,20.0405689590696));
#143821=CARTESIAN_POINT('Ctrl Pts',(18.500138140141,16.6602193806036,20.0448851207954));
#143822=CARTESIAN_POINT('Ctrl Pts',(18.4135439525353,16.6696490660532,20.0492012825211));
#143823=CARTESIAN_POINT('Ctrl Pts',(18.3277166966719,16.6834450792442,20.0535174442468));
#143824=CARTESIAN_POINT('Ctrl Pts',(18.2446852202539,16.696791694284,20.0576930091876));
#143825=CARTESIAN_POINT('Ctrl Pts',(18.1623719289201,16.7142243989078,20.0618685741284));
#143826=CARTESIAN_POINT('Ctrl Pts',(18.0812003839193,16.7356308030427,20.0660441390692));
#143827=CARTESIAN_POINT('Ctrl Pts',(17.9959291092702,16.7581183800159,20.0704305991874));
#143828=CARTESIAN_POINT('Ctrl Pts',(17.9119185059183,16.7849914459601,20.0748170593056));
#143829=CARTESIAN_POINT('Ctrl Pts',(17.8296377675515,16.8160618061167,20.0792035194238));
#143830=CARTESIAN_POINT('Ctrl Pts',(17.7473570291847,16.8471321662734,20.0835899795421));
#143831=CARTESIAN_POINT('Ctrl Pts',(17.6668066567997,16.8823995182561,20.0879764396603));
#143832=CARTESIAN_POINT('Ctrl Pts',(17.5884257348687,16.9216202580024,20.0923628997785));
#143833=CARTESIAN_POINT('Ctrl Pts',(17.5136510990685,16.9590364615644,20.0965475399908));
#143834=CARTESIAN_POINT('Ctrl Pts',(17.44057234666,17.0001895266255,20.1007321802031));
#143835=CARTESIAN_POINT('Ctrl Pts',(17.369587760884,17.0449023009683,20.1049168204155));
#143836=CARTESIAN_POINT('Ctrl Pts',(17.2987042121717,17.0895514326572,20.1090955043522));
#143837=CARTESIAN_POINT('Ctrl Pts',(17.2299092952701,17.1377499663397,20.1132741882888));
#143838=CARTESIAN_POINT('Ctrl Pts',(17.1635782312953,17.1892741361949,20.1174528722255));
#143839=CARTESIAN_POINT('Ctrl Pts',(17.0960583483994,17.241721748316,20.1217064486519));
#143840=CARTESIAN_POINT('Ctrl Pts',(17.0310919386145,17.2976151655664,20.1259600250784));
#143841=CARTESIAN_POINT('Ctrl Pts',(16.969045396673,17.3566712135668,20.1302136015048));
#143842=CARTESIAN_POINT('Ctrl Pts',(16.9082016412034,17.4145824465075,20.1343847213749));
#143843=CARTESIAN_POINT('Ctrl Pts',(16.8501659076493,17.4755344558904,20.138555841245));
#143844=CARTESIAN_POINT('Ctrl Pts',(16.7952502349704,17.5392197068402,20.142726961115));
#143845=CARTESIAN_POINT('Ctrl Pts',(16.7403529897255,17.6028835876472,20.1468966813293));
#143846=CARTESIAN_POINT('Ctrl Pts',(16.6885740262376,17.6692785404175,20.1510664015437));
#143847=CARTESIAN_POINT('Ctrl Pts',(16.6401868618722,17.7380619352452,20.155236121758));
#143848=CARTESIAN_POINT('Ctrl Pts',(16.5918014193961,17.8068428823705,20.1594056935901));
#143849=CARTESIAN_POINT('Ctrl Pts',(16.5468078000507,17.8780117258147,20.1635752654222));
#143850=CARTESIAN_POINT('Ctrl Pts',(16.5054369234628,17.9511958033507,20.1677448372542));
#143851=CARTESIAN_POINT('Ctrl Pts',(16.462611627541,18.0269527134222,20.1720609930214));
#143852=CARTESIAN_POINT('Ctrl Pts',(16.4236688015505,18.104868733296,20.1763771487885));
#143853=CARTESIAN_POINT('Ctrl Pts',(16.3888124800775,18.1845032896303,20.1806933045556));
#143854=CARTESIAN_POINT('Ctrl Pts',(16.3550914981959,18.2615439903646,20.1848688745605));
#143855=CARTESIAN_POINT('Ctrl Pts',(16.3251950198591,18.3401925369042,20.1890444445653));
#143856=CARTESIAN_POINT('Ctrl Pts',(16.2992578088608,18.4200319458494,20.1932200145702));
#143857=CARTESIAN_POINT('Ctrl Pts',(16.2720106919424,18.5039034812422,20.1976064632185));
#143858=CARTESIAN_POINT('Ctrl Pts',(16.2491334314256,18.5890887659587,20.2019929118667));
#143859=CARTESIAN_POINT('Ctrl Pts',(16.2307217504257,18.6750914208485,20.206379360515));
#143860=CARTESIAN_POINT('Ctrl Pts',(16.2123100694257,18.7610940757384,20.2107658091633));
#143861=CARTESIAN_POINT('Ctrl Pts',(16.198363984864,18.8479135158795,20.2151522578116));
#143862=CARTESIAN_POINT('Ctrl Pts',(16.1889163328193,18.9350486871749,20.2195387064599));
#143863=CARTESIAN_POINT('Ctrl Pts',(16.1790436177041,19.0261041916152,20.2241225075637));
#143864=CARTESIAN_POINT('Ctrl Pts',(16.1740562221026,19.1176988529932,20.2287063086676));
#143865=CARTESIAN_POINT('Ctrl Pts',(16.17400047263,19.2094444083109,20.2332901097715));
#143866=CARTESIAN_POINT('',(16.1742339579337,19.2120076676078,20.1667099326005));
#143867=CARTESIAN_POINT('Ctrl Pts',(20.2935357313021,17.1808649545432,19.8833624920292));
#143868=CARTESIAN_POINT('Ctrl Pts',(20.2268945096768,17.1296716280032,19.8875327690168));
#143869=CARTESIAN_POINT('Ctrl Pts',(20.1576921849675,17.0817340977654,19.8917030460043));
#143870=CARTESIAN_POINT('Ctrl Pts',(20.0862835185508,17.0373097540229,19.8958733229919));
#143871=CARTESIAN_POINT('Ctrl Pts',(20.0148883970778,16.992893836782,19.9000428089526));
#143872=CARTESIAN_POINT('Ctrl Pts',(19.9412881559087,16.9519900249486,19.9042122949134));
#143873=CARTESIAN_POINT('Ctrl Pts',(19.8658657268991,16.9148118595657,19.9083817808741));
#143874=CARTESIAN_POINT('Ctrl Pts',(19.7904349794946,16.8776295937757,19.9125517266905));
#143875=CARTESIAN_POINT('Ctrl Pts',(19.7131820583974,16.8441739925523,19.916721672507));
#143876=CARTESIAN_POINT('Ctrl Pts',(19.6345123880327,16.8146115842795,19.9208916183234));
#143877=CARTESIAN_POINT('Ctrl Pts',(19.5557587743145,16.7850176318591,19.9250660136212));
#143878=CARTESIAN_POINT('Ctrl Pts',(19.4755858247082,16.7593253280965,19.929240408919));
#143879=CARTESIAN_POINT('Ctrl Pts',(19.3944162566998,16.7376519921599,19.9334148042169));
#143880=CARTESIAN_POINT('Ctrl Pts',(19.3132002871327,16.7159662664004,19.9375915858579));
#143881=CARTESIAN_POINT('Ctrl Pts',(19.2309870146835,16.6983041792189,19.941768367499));
#143882=CARTESIAN_POINT('Ctrl Pts',(19.1482091649662,16.6847318496133,19.94594514914));
#143883=CARTESIAN_POINT('Ctrl Pts',(19.0652902625141,16.6711363928764,19.9501290479806));
#143884=CARTESIAN_POINT('Ctrl Pts',(18.9818053188629,16.6616446617399,19.9543129468212));
#143885=CARTESIAN_POINT('Ctrl Pts',(18.8981916908115,16.6562708384902,19.9584968456618));
#143886=CARTESIAN_POINT('Ctrl Pts',(18.8442012195363,16.6528008868022,19.9611984467696));
#143887=CARTESIAN_POINT('Ctrl Pts',(18.7901571239054,16.6510468154871,19.9639000478774));
#143888=CARTESIAN_POINT('Ctrl Pts',(18.7361763184546,16.6510009250709,19.9666016489852));
#143889=CARTESIAN_POINT('Ctrl Pts',(18.6525629441495,16.6509298432758,19.970786284297));
#143890=CARTESIAN_POINT('Ctrl Pts',(18.5687904831979,16.6549593424975,19.9749709196088));
#143891=CARTESIAN_POINT('Ctrl Pts',(18.4852943718232,16.6631095960554,19.9791555549207));
#143892=CARTESIAN_POINT('Ctrl Pts',(18.4019171067169,16.6712482487469,19.9833342339277));
#143893=CARTESIAN_POINT('Ctrl Pts',(18.3188158638129,16.6834959609775,19.9875129129346));
#143894=CARTESIAN_POINT('Ctrl Pts',(18.2364263585556,16.6998209001866,19.9916915919416));
#143895=CARTESIAN_POINT('Ctrl Pts',(18.1525601036937,16.7164384476283,19.9959451695968));
#143896=CARTESIAN_POINT('Ctrl Pts',(18.0694318349778,16.7372808264266,20.0001987472521));
#143897=CARTESIAN_POINT('Ctrl Pts',(17.9874960098027,16.7622591413913,20.0044523249073));
#143898=CARTESIAN_POINT('Ctrl Pts',(17.9071486482808,16.7867532097478,20.0086234398121));
#143899=CARTESIAN_POINT('Ctrl Pts',(17.8279483681478,16.8152241408414,20.0127945547169));
#143900=CARTESIAN_POINT('Ctrl Pts',(17.750311955398,16.8475368987634,20.0169656696217));
#143901=CARTESIAN_POINT('Ctrl Pts',(17.6727015943016,16.8798388138251,20.0211353848683));
#143902=CARTESIAN_POINT('Ctrl Pts',(17.5966544827465,16.9159798187964,20.0253051001149));
#143903=CARTESIAN_POINT('Ctrl Pts',(17.5225687033401,16.9557762387131,20.0294748153615));
#143904=CARTESIAN_POINT('Ctrl Pts',(17.448485560255,16.9955712424856,20.03364438223));
#143905=CARTESIAN_POINT('Ctrl Pts',(17.3763640154123,17.039021184132,20.0378139490985));
#143906=CARTESIAN_POINT('Ctrl Pts',(17.306577534957,17.0858964481018,20.041983515967));
#143907=CARTESIAN_POINT('Ctrl Pts',(17.2343374823217,17.1344197654316,20.0462996776086));
#143908=CARTESIAN_POINT('Ctrl Pts',(17.164600186369,17.1866134577584,20.0506158392503));
#143909=CARTESIAN_POINT('Ctrl Pts',(17.0977455244308,17.2421751496947,20.0549320008919));
#143910=CARTESIAN_POINT('Ctrl Pts',(17.0330686155273,17.2959269507464,20.0591075659941));
#143911=CARTESIAN_POINT('Ctrl Pts',(16.9710897386949,17.3528303455362,20.0632831310963));
#143912=CARTESIAN_POINT('Ctrl Pts',(16.9121162724542,17.4125729975048,20.0674586961985));
#143913=CARTESIAN_POINT('Ctrl Pts',(16.8501642398151,17.475333065051,20.0718451561099));
#143914=CARTESIAN_POINT('Ctrl Pts',(16.7915295867846,17.5412263087857,20.0762316160212));
#143915=CARTESIAN_POINT('Ctrl Pts',(16.7365203854444,17.6098519152075,20.0806180759326));
#143916=CARTESIAN_POINT('Ctrl Pts',(16.6815111841042,17.6784775216293,20.085004535844));
#143917=CARTESIAN_POINT('Ctrl Pts',(16.6301277117767,17.749834975445,20.0893909957553));
#143918=CARTESIAN_POINT('Ctrl Pts',(16.5826239199814,17.8234910946867,20.0937774556667));
#143919=CARTESIAN_POINT('Ctrl Pts',(16.5362791661082,17.8953500892742,20.0980568909977));
#143920=CARTESIAN_POINT('Ctrl Pts',(16.4934601213733,17.96965463442,20.1023363263287));
#143921=CARTESIAN_POINT('Ctrl Pts',(16.4544271375725,18.0460332344294,20.1066157616597));
#143922=CARTESIAN_POINT('Ctrl Pts',(16.4154575008457,18.1222878787389,20.1108882518464));
#143923=CARTESIAN_POINT('Ctrl Pts',(16.3802619050974,18.2006095046636,20.1151607420331));
#143924=CARTESIAN_POINT('Ctrl Pts',(16.3490570392734,18.2805984339648,20.1194332322197));
#143925=CARTESIAN_POINT('Ctrl Pts',(16.3179055659637,18.3604504996733,20.1236984120403));
#143926=CARTESIAN_POINT('Ctrl Pts',(16.2907313869123,18.4419637898502,20.1279635918609));
#143927=CARTESIAN_POINT('Ctrl Pts',(16.267704287416,18.5247161971242,20.1322287716815));
#143928=CARTESIAN_POINT('Ctrl Pts',(16.2447004012398,18.6073851827702,20.1364896518296));
#143929=CARTESIAN_POINT('Ctrl Pts',(16.2258353998839,18.6912903879612,20.1407505319778));
#143930=CARTESIAN_POINT('Ctrl Pts',(16.2112300227061,18.7759923659696,20.1450114121259));
#143931=CARTESIAN_POINT('Ctrl Pts',(16.1966372355967,18.8606213295208,20.1492686193273));
#143932=CARTESIAN_POINT('Ctrl Pts',(16.1862968405217,18.946045274463,20.1535258265288));
#143933=CARTESIAN_POINT('Ctrl Pts',(16.1802787590545,19.0318134392765,20.1577830337302));
#143934=CARTESIAN_POINT('Ctrl Pts',(16.1760723590125,19.0917619816882,20.160758652563));
#143935=CARTESIAN_POINT('Ctrl Pts',(16.1739765481557,19.1518784238251,20.1637342713957));
#143936=CARTESIAN_POINT('Ctrl Pts',(16.1740001980189,19.2120069046219,20.1667098902285));
#143937=CARTESIAN_POINT('Ctrl Pts',(16.1778405256925,19.2120194393453,20.1667105863375));
#143938=CARTESIAN_POINT('Ctrl Pts',(16.17655676437,19.5768333952661,20.1847914783409));
#143939=CARTESIAN_POINT('Ctrl Pts',(16.4202751262482,20.7953392457516,20.245264305905));
#143940=CARTESIAN_POINT('Ctrl Pts',(18.293812263991,22.2059164112385,20.3481290690295));
#143941=CARTESIAN_POINT('Ctrl Pts',(21.0139857695323,21.202220683841,20.4753048757109));
#143942=CARTESIAN_POINT('Ctrl Pts',(21.565931958902,18.716185413598,20.5870029231219));
#143943=CARTESIAN_POINT('Ctrl Pts',(20.719740363017,17.5166786165403,20.6563090349724));
#143944=CARTESIAN_POINT('Ctrl Pts',(20.2916962192318,17.1832234953211,20.6832232112625));
#143945=CARTESIAN_POINT('Origin',(18.734,19.211,-1.76670989022852));
#143946=CARTESIAN_POINT('',(20.2910035798173,17.1841778967012,21.5499225020685));
#143947=CARTESIAN_POINT('',(20.2957383339893,17.178031980842,21.4832513393832));
#143948=CARTESIAN_POINT('',(20.2935357313021,17.1808649545432,-1.76670989022852));
#143949=CARTESIAN_POINT('',(16.1741052590002,19.209658325614,21.0332900820446));
#143950=CARTESIAN_POINT('Ctrl Pts',(16.1775161339837,19.2096606725892,21.0332901097715));
#143951=CARTESIAN_POINT('Ctrl Pts',(16.1799699186122,19.7238724897518,21.0587831909243));
#143952=CARTESIAN_POINT('Ctrl Pts',(16.5801691862074,21.0966582496844,21.1266682076376));
#143953=CARTESIAN_POINT('Ctrl Pts',(18.8208064662072,22.2367206740717,21.2369451599114));
#143954=CARTESIAN_POINT('Ctrl Pts',(21.3254400167184,20.7760162000723,21.3641209665928));
#143955=CARTESIAN_POINT('Ctrl Pts',(21.4293000776619,18.3992335115625,21.4684467473119));
#143956=CARTESIAN_POINT('Ctrl Pts',(20.6042288382577,17.4236622121578,21.5303805924704));
#143957=CARTESIAN_POINT('Ctrl Pts',(20.2910035798173,17.1841778967012,21.5499225020685));
#143958=CARTESIAN_POINT('Ctrl Pts',(20.2935357313021,17.1808649545431,20.7499611463308));
#143959=CARTESIAN_POINT('Ctrl Pts',(20.2235403921486,17.1270950180659,20.7543551710615));
#143960=CARTESIAN_POINT('Ctrl Pts',(20.1506714606626,17.0768804970143,20.7587491957922));
#143961=CARTESIAN_POINT('Ctrl Pts',(20.0753314078174,17.0305344409043,20.7631432205228));
#143962=CARTESIAN_POINT('Ctrl Pts',(20.0038028427435,16.9865330529945,20.7673149495304));
#143963=CARTESIAN_POINT('Ctrl Pts',(19.9300475351787,16.9460185369239,20.7714866785379));
#143964=CARTESIAN_POINT('Ctrl Pts',(19.8544414196889,16.9092156866801,20.7756584075455));
#143965=CARTESIAN_POINT('Ctrl Pts',(19.7788660377839,16.8724277966484,20.7798284407618));
#143966=CARTESIAN_POINT('Ctrl Pts',(19.7014417550698,16.8393487774228,20.7839984739781));
#143967=CARTESIAN_POINT('Ctrl Pts',(19.6225688678681,16.8101573631211,20.7881685071945));
#143968=CARTESIAN_POINT('Ctrl Pts',(19.5437043851342,16.7809690593725,20.7923380960641));
#143969=CARTESIAN_POINT('Ctrl Pts',(19.463392036181,16.7556676965775,20.7965076849337));
#143970=CARTESIAN_POINT('Ctrl Pts',(19.3820505615475,16.7343832614476,20.8006772738032));
#143971=CARTESIAN_POINT('Ctrl Pts',(19.3006933573855,16.7130947104084,20.8048476689733));
#143972=CARTESIAN_POINT('Ctrl Pts',(19.2183070776701,16.6958247446206,20.8090180641433));
#143973=CARTESIAN_POINT('Ctrl Pts',(19.1353226944306,16.6826526949537,20.8131884593133));
#143974=CARTESIAN_POINT('Ctrl Pts',(19.0522458413061,16.6694659676104,20.8173635015742));
#143975=CARTESIAN_POINT('Ctrl Pts',(18.9685700096491,16.6603863408392,20.821538543835));
#143976=CARTESIAN_POINT('Ctrl Pts',(18.884732812933,16.6554414271817,20.8257135860958));
#143977=CARTESIAN_POINT('Ctrl Pts',(18.8008414473993,16.6504933185207,20.8298913259313));
#143978=CARTESIAN_POINT('Ctrl Pts',(18.7167889688217,16.6496852442149,20.8340690657669));
#143979=CARTESIAN_POINT('Ctrl Pts',(18.6330121303373,16.6529926798031,20.8382468056024));
#143980=CARTESIAN_POINT('Ctrl Pts',(18.5490995249123,16.6563054753502,20.8424313157932));
#143981=CARTESIAN_POINT('Ctrl Pts',(18.4654639082309,16.6637470495906,20.8466158259839));
#143982=CARTESIAN_POINT('Ctrl Pts',(18.3825355613592,16.6752411888409,20.8508003361747));
#143983=CARTESIAN_POINT('Ctrl Pts',(18.352033094117,16.6794689302488,20.8523394707388));
#143984=CARTESIAN_POINT('Ctrl Pts',(18.3216261951854,16.6842444455182,20.853878605303));
#143985=CARTESIAN_POINT('Ctrl Pts',(18.291335798662,16.6895622345864,20.8554177398671));
#143986=CARTESIAN_POINT('Ctrl Pts',(18.2089776381982,16.7040210524186,20.8596025742027));
#143987=CARTESIAN_POINT('Ctrl Pts',(18.1271754855616,16.7225461173931,20.8637874085383));
#143988=CARTESIAN_POINT('Ctrl Pts',(18.0463616920216,16.7450815996062,20.8679722428739));
#143989=CARTESIAN_POINT('Ctrl Pts',(17.9656628851169,16.7675850170052,20.8721511227802));
#143990=CARTESIAN_POINT('Ctrl Pts',(17.8859500832465,16.7940873946836,20.8763300026864));
#143991=CARTESIAN_POINT('Ctrl Pts',(17.807646872009,16.8244816400745,20.8805088825927));
#143992=CARTESIAN_POINT('Ctrl Pts',(17.7279449225123,16.855418820975,20.8847624102575));
#143993=CARTESIAN_POINT('Ctrl Pts',(17.6497038935229,16.8903881967177,20.8890159379224));
#143994=CARTESIAN_POINT('Ctrl Pts',(17.573355832904,16.929223254263,20.8932694655872));
#143995=CARTESIAN_POINT('Ctrl Pts',(17.4984833659801,16.96730773916,20.8974407845023));
#143996=CARTESIAN_POINT('Ctrl Pts',(17.4254317755321,17.0091095912712,20.9016121034175));
#143997=CARTESIAN_POINT('Ctrl Pts',(17.3545880686225,17.0544233786917,20.9057834223326));
#143998=CARTESIAN_POINT('Ctrl Pts',(17.2837681207943,17.0997219690819,20.9099533422992));
#143999=CARTESIAN_POINT('Ctrl Pts',(17.2151549730969,17.1485299079787,20.9141232622657));
#144000=CARTESIAN_POINT('Ctrl Pts',(17.1491087606968,17.2005971151085,20.9182931822322));
#144001=CARTESIAN_POINT('Ctrl Pts',(17.0830648915168,17.2526624749723,20.9224629542563));
#144002=CARTESIAN_POINT('Ctrl Pts',(17.0195881372629,17.3079865877146,20.9266327262803));
#144003=CARTESIAN_POINT('Ctrl Pts',(16.9590064076381,17.3662784093326,20.9308024983044));
#144004=CARTESIAN_POINT('Ctrl Pts',(16.8963013152172,17.4266133334852,20.9351184189914));
#144005=CARTESIAN_POINT('Ctrl Pts',(16.8366983378617,17.4901275013993,20.9394343396784));
#144006=CARTESIAN_POINT('Ctrl Pts',(16.7805189594492,17.5564572159631,20.9437502603654));
#144007=CARTESIAN_POINT('Ctrl Pts',(16.7261639013725,17.6206329969918,20.9479260295929));
#144008=CARTESIAN_POINT('Ctrl Pts',(16.6750137437496,17.6874438611066,20.9521017988205));
#144009=CARTESIAN_POINT('Ctrl Pts',(16.627316944944,17.7565287883427,20.956277568048));
#144010=CARTESIAN_POINT('Ctrl Pts',(16.5772188726481,17.8290917645988,20.9606635644648));
#144011=CARTESIAN_POINT('Ctrl Pts',(16.5309313071797,17.9041632904909,20.9650495608815));
#144012=CARTESIAN_POINT('Ctrl Pts',(16.4886879176914,17.9812952984399,20.9694355572982));
#144013=CARTESIAN_POINT('Ctrl Pts',(16.4464445282031,18.0584273063889,20.973821553715));
#144014=CARTESIAN_POINT('Ctrl Pts',(16.4082454981439,18.1376192412558,20.9782075501317));
#144015=CARTESIAN_POINT('Ctrl Pts',(16.3742656129549,18.2184005729416,20.9825935465485));
#144016=CARTESIAN_POINT('Ctrl Pts',(16.3382155097944,18.3041034917275,20.9872467589536));
#144017=CARTESIAN_POINT('Ctrl Pts',(16.306798874077,18.3918657738651,20.9918999713587));
#144018=CARTESIAN_POINT('Ctrl Pts',(16.2802296051744,18.4811980751755,20.9965531837637));
#144019=CARTESIAN_POINT('Ctrl Pts',(16.2537435497692,18.5702505926029,21.001191822562));
#144020=CARTESIAN_POINT('Ctrl Pts',(16.2320746945689,18.6608630689237,21.0058304613603));
#144021=CARTESIAN_POINT('Ctrl Pts',(16.2153886002422,18.752527953949,21.0104691001586));
#144022=CARTESIAN_POINT('Ctrl Pts',(16.1987928060345,18.8436967762135,21.0150826360402));
#144023=CARTESIAN_POINT('Ctrl Pts',(16.1871261070645,18.9359063886952,21.0196961719218));
#144024=CARTESIAN_POINT('Ctrl Pts',(16.1805035110245,19.0286385984106,21.0243097078035));
#144025=CARTESIAN_POINT('Ctrl Pts',(16.1762064897689,19.0888071899736,21.0273031655996));
#144026=CARTESIAN_POINT('Ctrl Pts',(16.1740320413884,19.1491954186321,21.0302966233957));
#144027=CARTESIAN_POINT('Ctrl Pts',(16.174000351618,19.2096582534287,21.0332900811918));
#144028=CARTESIAN_POINT('',(16.1715627854608,19.2128544306465,20.9667098902285));
#144029=CARTESIAN_POINT('Ctrl Pts',(20.2916962192318,17.1832234953211,20.6832232112625));
#144030=CARTESIAN_POINT('Ctrl Pts',(20.0455373123707,16.9914606845963,20.6987009705329));
#144031=CARTESIAN_POINT('Ctrl Pts',(19.0022218457995,16.4381424631027,20.7565706653639));
#144032=CARTESIAN_POINT('Ctrl Pts',(16.8944629772976,16.8838679918332,20.8510662250192));
#144033=CARTESIAN_POINT('Ctrl Pts',(16.1775450542205,18.4784656881504,20.9300840254041));
#144034=CARTESIAN_POINT('Ctrl Pts',(16.1715627854608,19.2128544306465,20.9667098902285));
#144035=CARTESIAN_POINT('Ctrl Pts',(16.1715627854608,19.2128544306465,20.9667098902285));
#144036=CARTESIAN_POINT('Ctrl Pts',(16.1706209869532,19.3284704702211,20.9724759609646));
#144037=CARTESIAN_POINT('Ctrl Pts',(16.2303035804914,20.2931122226394,21.0206339672611));
#144038=CARTESIAN_POINT('Ctrl Pts',(17.4553333859632,21.9547543997083,21.1111839091181));
#144039=CARTESIAN_POINT('Ctrl Pts',(20.3489604234473,21.7713501510339,21.2383597157995));
#144040=CARTESIAN_POINT('Ctrl Pts',(21.7259567294576,19.3016368932709,21.3623821925546));
#144041=CARTESIAN_POINT('Ctrl Pts',(20.9160604073402,17.6604732139873,21.4440127337491));
#144042=CARTESIAN_POINT('Ctrl Pts',(20.2957383339893,17.178031980842,21.4832513393832));
#144043=CARTESIAN_POINT('Origin',(18.734,-18.952,-1.76670989022851));
#144044=CARTESIAN_POINT('',(20.2955776483338,-20.9847559318741,0.749817810273507));
#144045=CARTESIAN_POINT('',(20.2916906430028,-20.9796979674239,0.683386616606776));
#144046=CARTESIAN_POINT('',(20.2935357468249,-20.9821350335323,-1.76670989022851));
#144047=CARTESIAN_POINT('',(16.1740007446509,-18.9500474088581,0.233290109771496));
#144048=CARTESIAN_POINT('Ctrl Pts',(16.1719919811635,-18.9500458767116,
0.233290109771496));
#144049=CARTESIAN_POINT('Ctrl Pts',(16.1708576376271,-18.8187090077496,
0.239839092339242));
#144050=CARTESIAN_POINT('Ctrl Pts',(16.2398215302323,-17.838374208454,0.288780010467466));
#144051=CARTESIAN_POINT('Ctrl Pts',(17.5061738910726,-16.184820909787,0.380112864156167));
#144052=CARTESIAN_POINT('Ctrl Pts',(20.3959079738877,-16.4220626898431,
0.507288670837602));
#144053=CARTESIAN_POINT('Ctrl Pts',(21.7186679417731,-18.9005846219903,
0.630523652876716));
#144054=CARTESIAN_POINT('Ctrl Pts',(20.9031377956339,-20.5111939695708,
0.711366699355352));
#144055=CARTESIAN_POINT('Ctrl Pts',(20.2955776483338,-20.9847559318741,
0.749817810273507));
#144056=CARTESIAN_POINT('',(19.3957675194894,-21.4249868075161,1.730088294849E-11));
#144057=CARTESIAN_POINT('Ctrl Pts',(19.3957675194894,-21.4249868075161,
1.73008274373387E-11));
#144058=CARTESIAN_POINT('Ctrl Pts',(19.3150528143647,-21.4465859402064,
0.00418159702990585));
#144059=CARTESIAN_POINT('Ctrl Pts',(19.2331283755591,-21.4642697491679,
0.0083631940425111));
#144060=CARTESIAN_POINT('Ctrl Pts',(19.1504091626665,-21.4779064529882,
0.0125447910551162));
#144061=CARTESIAN_POINT('Ctrl Pts',(19.0678077425558,-21.4915237380395,
0.0167204334420983));
#144062=CARTESIAN_POINT('Ctrl Pts',(18.9844142470727,-21.501105290632,0.0208960758290806));
#144063=CARTESIAN_POINT('Ctrl Pts',(18.9006573352602,-21.506569500445,0.0250717182160627));
#144064=CARTESIAN_POINT('Ctrl Pts',(18.8165041727153,-21.5120595612247,
0.029267115406781));
#144065=CARTESIAN_POINT('Ctrl Pts',(18.7319846004062,-21.5133930928997,
0.0334625125974991));
#144066=CARTESIAN_POINT('Ctrl Pts',(18.6475423362417,-21.5105396366634,
0.0376579097882175));
#144067=CARTESIAN_POINT('Ctrl Pts',(18.5636493303861,-21.5077047408548,
0.041826017838971));
#144068=CARTESIAN_POINT('Ctrl Pts',(18.4798330960835,-21.5007371781061,
0.0459941258897243));
#144069=CARTESIAN_POINT('Ctrl Pts',(18.3965306502634,-21.4896592438679,
0.0501622339404779));
#144070=CARTESIAN_POINT('Ctrl Pts',(18.3132562868314,-21.4785850441522,
0.0543289368652889));
#144071=CARTESIAN_POINT('Ctrl Pts',(18.2304958242585,-21.4634032856077,
0.0584956397901002));
#144072=CARTESIAN_POINT('Ctrl Pts',(18.1486808249577,-21.4441880874701,
0.0626623427149111));
#144073=CARTESIAN_POINT('Ctrl Pts',(18.0668687681529,-21.4249735804117,
0.0668288957832525));
#144074=CARTESIAN_POINT('Ctrl Pts',(17.9860025553434,-21.4017260285035,
0.0709954488515935));
#144075=CARTESIAN_POINT('Ctrl Pts',(17.9065018743522,-21.3745702986806,
0.0751620019199348));
#144076=CARTESIAN_POINT('Ctrl Pts',(17.8260461859792,-21.3470883587911,
0.0793786059927156));
#144077=CARTESIAN_POINT('Ctrl Pts',(17.7469895187101,-21.3156038569086,
0.0835952100654965));
#144078=CARTESIAN_POINT('Ctrl Pts',(17.6697476372837,-21.2802969974753,
0.0878118141382773));
#144079=CARTESIAN_POINT('Ctrl Pts',(17.5933153937669,-21.24536021929,0.0919842203944796));
#144080=CARTESIAN_POINT('Ctrl Pts',(17.5186604552654,-21.2066811083584,
0.0961566266506819));
#144081=CARTESIAN_POINT('Ctrl Pts',(17.4461606843492,-21.1644804851262,
0.100329032906884));
#144082=CARTESIAN_POINT('Ctrl Pts',(17.3725089409092,-21.1216093224172,
0.104567735887954));
#144083=CARTESIAN_POINT('Ctrl Pts',(17.3010818658164,-21.0751040329196,
0.108806438869025));
#144084=CARTESIAN_POINT('Ctrl Pts',(17.2322432557832,-21.0252406230824,
0.113045141850095));
#144085=CARTESIAN_POINT('Ctrl Pts',(17.1634046457499,-20.9753772132452,
0.117283844831166));
#144086=CARTESIAN_POINT('Ctrl Pts',(17.0971548434137,-20.922156041386,0.121522547812235));
#144087=CARTESIAN_POINT('Ctrl Pts',(17.0338195258261,-20.8658929842699,
0.125761250793306));
#144088=CARTESIAN_POINT('Ctrl Pts',(16.9721381141262,-20.8110991516714,
0.129889266466191));
#144089=CARTESIAN_POINT('Ctrl Pts',(16.9129812124539,-20.7532072684117,
0.134017282139077));
#144090=CARTESIAN_POINT('Ctrl Pts',(16.8566825230424,-20.6924824304513,
0.138145297811962));
#144091=CARTESIAN_POINT('Ctrl Pts',(16.8004749041019,-20.6318558228343,
0.142266635881243));
#144092=CARTESIAN_POINT('Ctrl Pts',(16.7471166297386,-20.5684057102785,
0.146387973950524));
#144093=CARTESIAN_POINT('Ctrl Pts',(16.6969071781283,-20.5024363369964,
0.150509312019806));
#144094=CARTESIAN_POINT('Ctrl Pts',(16.6467433529369,-20.4365269115162,
0.154626904939698));
#144095=CARTESIAN_POINT('Ctrl Pts',(16.5997229596986,-20.3681031412178,
0.158744497859592));
#144096=CARTESIAN_POINT('Ctrl Pts',(16.556106820746,-20.2975041061843,0.162862090779484));
#144097=CARTESIAN_POINT('Ctrl Pts',(16.5125163940206,-20.2269466901128,
0.166977256329893));
#144098=CARTESIAN_POINT('Ctrl Pts',(16.4723264872833,-20.1542169560892,
0.171092421880302));
#144099=CARTESIAN_POINT('Ctrl Pts',(16.4357550860861,-20.0796836061897,
0.175207587430711));
#144100=CARTESIAN_POINT('Ctrl Pts',(16.3991935731796,-20.005170408852,0.179321640309701));
#144101=CARTESIAN_POINT('Ctrl Pts',(16.3662488306016,-19.9288549893914,
0.18343569318869));
#144102=CARTESIAN_POINT('Ctrl Pts',(16.3370925482441,-19.8511299504059,
0.18754974606768));
#144103=CARTESIAN_POINT('Ctrl Pts',(16.3079200305593,-19.7733616311617,
0.191666089807838));
#144104=CARTESIAN_POINT('Ctrl Pts',(16.2825403576348,-19.694182567114,0.195782433547997));
#144105=CARTESIAN_POINT('Ctrl Pts',(16.2610764230542,-19.6140037632713,
0.199898777288155));
#144106=CARTESIAN_POINT('Ctrl Pts',(16.239606571648,-19.5338028570508,0.204016255754456));
#144107=CARTESIAN_POINT('Ctrl Pts',(16.2220547122219,-19.4526021247793,
0.208133734220756));
#144108=CARTESIAN_POINT('Ctrl Pts',(16.2084928022863,-19.3708238225034,
0.212251212687057));
#144109=CARTESIAN_POINT('Ctrl Pts',(16.1949128185011,-19.2889365349339,
0.216374178484198));
#144110=CARTESIAN_POINT('Ctrl Pts',(16.1853334601433,-19.2064706109328,
0.22049714428134));
#144111=CARTESIAN_POINT('Ctrl Pts',(16.1797748249049,-19.1238538766228,
0.224620110078481));
#144112=CARTESIAN_POINT('Ctrl Pts',(16.1758784900672,-19.0659435359969,
0.227510109976153));
#144113=CARTESIAN_POINT('Ctrl Pts',(16.1739565735353,-19.0079591859799,
0.230400109873824));
#144114=CARTESIAN_POINT('Ctrl Pts',(16.1740007446509,-18.9500474088581,
0.233290109771496));
#144115=CARTESIAN_POINT('',(18.0722627314315,-21.4249949024184,0.));
#144116=CARTESIAN_POINT('Origin',(18.734,-18.952,0.));
#144117=CARTESIAN_POINT('',(16.1765334791563,-18.9551432954109,0.166709890228505));
#144118=CARTESIAN_POINT('Ctrl Pts',(18.0722627314315,-21.4249949024184,
-8.32667268468867E-16));
#144119=CARTESIAN_POINT('Ctrl Pts',(17.2488902483963,-21.2046724677036,
0.0423919355604773));
#144120=CARTESIAN_POINT('Ctrl Pts',(16.3345567445347,-20.3367913268265,
0.0979618989699792));
#144121=CARTESIAN_POINT('Ctrl Pts',(16.174495607841,-19.2205924221476,0.153531862379481));
#144122=CARTESIAN_POINT('Ctrl Pts',(16.1765334791563,-18.9551432954109,
0.166709890228505));
#144123=CARTESIAN_POINT('Ctrl Pts',(16.1765334791563,-18.9551432954109,
0.166709890228505));
#144124=CARTESIAN_POINT('Ctrl Pts',(16.1810511645957,-18.366678437132,0.195923797939959));
#144125=CARTESIAN_POINT('Ctrl Pts',(16.6739009874383,-16.9152607583549,
0.267529641211892));
#144126=CARTESIAN_POINT('Ctrl Pts',(19.0860575095572,-15.9462785509947,
0.381527420044301));
#144127=CARTESIAN_POINT('Ctrl Pts',(21.4520483087009,-17.6196576192121,
0.508703226725736));
#144128=CARTESIAN_POINT('Ctrl Pts',(21.3518776905422,-19.9120072668099,
0.60932295891323));
#144129=CARTESIAN_POINT('Ctrl Pts',(20.5461545388389,-20.7868242253756,
0.667550755540244));
#144130=CARTESIAN_POINT('Ctrl Pts',(20.2916906430027,-20.979697967424,0.683386616606783));
#144131=CARTESIAN_POINT('Origin',(18.734,-18.952,-1.76670989022851));
#144132=CARTESIAN_POINT('',(20.2940723489731,-20.982845288132,1.55000082941896));
#144133=CARTESIAN_POINT('',(20.2935357468249,-20.9821350335323,1.48324950709828));
#144134=CARTESIAN_POINT('',(20.2935357468249,-20.9821350335323,-1.76670989022851));
#144135=CARTESIAN_POINT('',(16.1715629797346,-18.9538544393498,1.0332901097715));
#144136=CARTESIAN_POINT('Ctrl Pts',(16.1715629797346,-18.9538544393498,
1.0332901097715));
#144137=CARTESIAN_POINT('Ctrl Pts',(16.1775452476667,-18.2194657538418,
1.06991597459592));
#144138=CARTESIAN_POINT('Ctrl Pts',(16.8944631229174,-16.6248681563667,
1.14893377498083));
#144139=CARTESIAN_POINT('Ctrl Pts',(19.6025525643745,-16.052191380828,1.27034351092621));
#144140=CARTESIAN_POINT('Ctrl Pts',(21.6424137382259,-18.1127008887664,
1.39751931760764));
#144141=CARTESIAN_POINT('Ctrl Pts',(21.1817796643434,-20.1874548702378,
1.4907384237719));
#144142=CARTESIAN_POINT('Ctrl Pts',(20.4294541422046,-20.881008060679,1.54156559437567));
#144143=CARTESIAN_POINT('Ctrl Pts',(20.294072348973,-20.9828452881321,1.55000082941897));
#144144=CARTESIAN_POINT('Ctrl Pts',(20.2955776483338,-20.9847559318741,
0.749817810273507));
#144145=CARTESIAN_POINT('Ctrl Pts',(20.23330927837,-21.0332909314137,0.753758634915827));
#144146=CARTESIAN_POINT('Ctrl Pts',(19.4740834602792,-21.567801555079,0.800091395118626));
#144147=CARTESIAN_POINT('Ctrl Pts',(17.4553335005934,-21.6957541409811,
0.888816090881904));
#144148=CARTESIAN_POINT('Ctrl Pts',(16.230303771566,-20.0341121451265,0.979366032738913));
#144149=CARTESIAN_POINT('Ctrl Pts',(16.1706211813573,-19.0694704699527,
1.02752403903544));
#144150=CARTESIAN_POINT('Ctrl Pts',(16.1715629797346,-18.9538544393498,
1.0332901097715));
#144151=CARTESIAN_POINT('',(16.1740711676982,-18.9506582890571,0.966709918231089));
#144152=CARTESIAN_POINT('Ctrl Pts',(20.2916906430027,-20.979697967424,0.683386616606783));
#144153=CARTESIAN_POINT('Ctrl Pts',(19.8649653676639,-21.3031391393463,
0.709942691100723));
#144154=CARTESIAN_POINT('Ctrl Pts',(18.4990491243427,-21.814007150788,0.778890701155144));
#144155=CARTESIAN_POINT('Ctrl Pts',(16.5801690201362,-20.8376582933814,
0.873331792362383));
#144156=CARTESIAN_POINT('Ctrl Pts',(16.1799697387475,-19.4648724906692,
0.941216809075683));
#144157=CARTESIAN_POINT('Ctrl Pts',(16.1775159588735,-18.9506606593868,
0.966709890228505));
#144158=CARTESIAN_POINT('Ctrl Pts',(16.1740003516248,-18.9506582403292,
0.96670991880675));
#144159=CARTESIAN_POINT('Ctrl Pts',(16.1740492156647,-18.8574284856305,
0.971325636022637));
#144160=CARTESIAN_POINT('Ctrl Pts',(16.1791950640212,-18.7643768125493,
0.975941353238524));
#144161=CARTESIAN_POINT('Ctrl Pts',(16.1893550102722,-18.6720323657042,
0.980557070454411));
#144162=CARTESIAN_POINT('Ctrl Pts',(16.1995507619901,-18.57936248052,0.985189054282917));
#144163=CARTESIAN_POINT('Ctrl Pts',(16.2147958864483,-18.487405080462,0.989821038111424));
#144164=CARTESIAN_POINT('Ctrl Pts',(16.234956622384,-18.3966782943254,0.994453021939931));
#144165=CARTESIAN_POINT('Ctrl Pts',(16.25521618901,-18.3055067530499,0.999107712387932));
#144166=CARTESIAN_POINT('Ctrl Pts',(16.2804395488529,-18.2155781794355,
1.00376240283593));
#144167=CARTESIAN_POINT('Ctrl Pts',(16.3104425025438,-18.1273976373283,
1.00841709328394));
#144168=CARTESIAN_POINT('Ctrl Pts',(16.3297568808632,-18.0706314812951,
1.01141354667312));
#144169=CARTESIAN_POINT('Ctrl Pts',(16.3510510092264,-18.0145893008769,
1.0144100000623));
#144170=CARTESIAN_POINT('Ctrl Pts',(16.3742656062904,-17.9594005887852,
1.01740645345148));
#144171=CARTESIAN_POINT('Ctrl Pts',(16.4066870283893,-17.8823242335553,
1.02159128939168));
#144172=CARTESIAN_POINT('Ctrl Pts',(16.442949046845,-17.806694695872,1.02577612533188));
#144173=CARTESIAN_POINT('Ctrl Pts',(16.4829010339938,-17.7329210668517,
1.02996096127207));
#144174=CARTESIAN_POINT('Ctrl Pts',(16.5227961707087,-17.6592524154088,
1.03413984232102));
#144175=CARTESIAN_POINT('Ctrl Pts',(16.5663706293486,-17.5874348279767,
1.03831872336996));
#144176=CARTESIAN_POINT('Ctrl Pts',(16.6134257549123,-17.517857443951,1.0424976044189));
#144177=CARTESIAN_POINT('Ctrl Pts',(16.6613214140263,-17.4470372170912,
1.04675113174031));
#144178=CARTESIAN_POINT('Ctrl Pts',(16.7128231258243,-17.378538458199,1.05100465906173));
#144179=CARTESIAN_POINT('Ctrl Pts',(16.767672421654,-17.312745335637,1.05525818638315));
#144180=CARTESIAN_POINT('Ctrl Pts',(16.8214616389431,-17.2482238041918,
1.05942950530122));
#144181=CARTESIAN_POINT('Ctrl Pts',(16.8784698848833,-17.1863046245575,
1.06360082421929));
#144182=CARTESIAN_POINT('Ctrl Pts',(16.9384107688485,-17.1273193942576,
1.06777214313735));
#144183=CARTESIAN_POINT('Ctrl Pts',(16.9983315441488,-17.0683539520246,
1.07194206268243));
#144184=CARTESIAN_POINT('Ctrl Pts',(17.0611826759855,-17.0123208267143,
1.07611198222751));
#144185=CARTESIAN_POINT('Ctrl Pts',(17.1266402234641,-16.9595154834292,
1.08028190177259));
#144186=CARTESIAN_POINT('Ctrl Pts',(17.192095441962,-16.9067120189591,1.08445167295186));
#144187=CARTESIAN_POINT('Ctrl Pts',(17.2601565331721,-16.8571363963205,
1.08862144413112));
#144188=CARTESIAN_POINT('Ctrl Pts',(17.3304667893585,-16.8110435486385,
1.09279121531039));
#144189=CARTESIAN_POINT('Ctrl Pts',(17.4032413988251,-16.7633351605427,
1.09710713571227));
#144190=CARTESIAN_POINT('Ctrl Pts',(17.4784253279814,-16.7193585145734,
1.10142305611414));
#144191=CARTESIAN_POINT('Ctrl Pts',(17.5555924665286,-16.6793461141085,
1.10573897651602));
#144192=CARTESIAN_POINT('Ctrl Pts',(17.6302537175966,-16.6406330565404,
1.10991474385404));
#144193=CARTESIAN_POINT('Ctrl Pts',(17.7067708977367,-16.6056308716597,
1.11409051119206));
#144194=CARTESIAN_POINT('Ctrl Pts',(17.7847367550312,-16.5745014633546,
1.11826627853008));
#144195=CARTESIAN_POINT('Ctrl Pts',(17.8666278144112,-16.5418048405963,
1.12265227546389));
#144196=CARTESIAN_POINT('Ctrl Pts',(17.950116694982,-16.5133813683478,1.12703827239769));
#144197=CARTESIAN_POINT('Ctrl Pts',(18.0347145687176,-16.4893591643124,
1.13142426933149));
#144198=CARTESIAN_POINT('Ctrl Pts',(18.1193124424532,-16.465336960277,1.1358102662653));
#144199=CARTESIAN_POINT('Ctrl Pts',(18.2050187273114,-16.445716079792,1.1401962631991));
#144200=CARTESIAN_POINT('Ctrl Pts',(18.2913357970735,-16.4305622348653,
1.14458226013291));
#144201=CARTESIAN_POINT('Ctrl Pts',(18.3736918330588,-16.4161037899536,
1.14876698654111));
#144202=CARTESIAN_POINT('Ctrl Pts',(18.4569101597461,-16.4056576064885,
1.1529517129493));
#144203=CARTESIAN_POINT('Ctrl Pts',(18.5405652843443,-16.3993184666357,
1.1571364393575));
#144204=CARTESIAN_POINT('Ctrl Pts',(18.6241013829374,-16.3929883462242,
1.16131521166224));
#144205=CARTESIAN_POINT('Ctrl Pts',(18.7080725902024,-16.3907536966889,
1.16549398396698));
#144206=CARTESIAN_POINT('Ctrl Pts',(18.7920441924572,-16.3926581174603,
1.16967275627172));
#144207=CARTESIAN_POINT('Ctrl Pts',(18.8775185302511,-16.3945966192864,
1.17392631087766));
#144208=CARTESIAN_POINT('Ctrl Pts',(18.9629928024743,-16.4008238793069,
1.1781798654836));
#144209=CARTESIAN_POINT('Ctrl Pts',(19.0480040551094,-16.4113305107955,
1.18243342008954));
#144210=CARTESIAN_POINT('Ctrl Pts',(19.1313696330155,-16.421633751587,1.18660463303945));
#144211=CARTESIAN_POINT('Ctrl Pts',(19.2142894806513,-16.4360520981611,
1.19077584598936));
#144212=CARTESIAN_POINT('Ctrl Pts',(19.2963297776568,-16.4545242301154,
1.19494705893927));
#144213=CARTESIAN_POINT('Ctrl Pts',(19.3783425766114,-16.4729901706292,
1.199116873793));
#144214=CARTESIAN_POINT('Ctrl Pts',(19.4594759620237,-16.4955070970836,
1.20328668864672));
#144215=CARTESIAN_POINT('Ctrl Pts',(19.5393061703828,-16.5219625575018,
1.20745650350045));
#144216=CARTESIAN_POINT('Ctrl Pts',(19.6191335655528,-16.5484170856385,
1.21162617141134));
#144217=CARTESIAN_POINT('Ctrl Pts',(19.6976574385902,-16.5788097262656,
1.21579583932222));
#144218=CARTESIAN_POINT('Ctrl Pts',(19.7744703716763,-16.6129785367244,
1.2199655072331));
#144219=CARTESIAN_POINT('Ctrl Pts',(19.853979869365,-16.6483468639975,1.22428155386487));
#144220=CARTESIAN_POINT('Ctrl Pts',(19.9316555820171,-16.6877612115752,
1.22859760049664));
#144221=CARTESIAN_POINT('Ctrl Pts',(20.0070713209912,-16.7309891014068,
1.23291364712841));
#144222=CARTESIAN_POINT('Ctrl Pts',(20.080034189258,-16.772811019141,1.23708931584307));
#144223=CARTESIAN_POINT('Ctrl Pts',(20.1508814689922,-16.8182019195625,
1.24126498455773));
#144224=CARTESIAN_POINT('Ctrl Pts',(20.2192566105122,-16.866907004249,1.24544065327239));
#144225=CARTESIAN_POINT('Ctrl Pts',(20.2910797123248,-16.9180681452494,
1.24982688886272));
#144226=CARTESIAN_POINT('Ctrl Pts',(20.3601743388774,-16.9728861439699,
1.25421312445304));
#144227=CARTESIAN_POINT('Ctrl Pts',(20.4261681146539,-17.0310192422232,
1.25859936004337));
#144228=CARTESIAN_POINT('Ctrl Pts',(20.4921618904303,-17.0891523404765,
1.26298559563369));
#144229=CARTESIAN_POINT('Ctrl Pts',(20.5550544537331,-17.1506000785723,
1.26737183122402));
#144230=CARTESIAN_POINT('Ctrl Pts',(20.614521157858,-17.2149795122542,1.27175806681434));
#144231=CARTESIAN_POINT('Ctrl Pts',(20.6712532028065,-17.2763983680518,
1.2759425952547));
#144232=CARTESIAN_POINT('Ctrl Pts',(20.7250787526129,-17.3407138524111,
1.28012712369507));
#144233=CARTESIAN_POINT('Ctrl Pts',(20.7756877943714,-17.4076195577789,
1.28431165213543));
#144234=CARTESIAN_POINT('Ctrl Pts',(20.8262247790096,-17.4744300028477,
1.28849022264697));
#144235=CARTESIAN_POINT('Ctrl Pts',(20.873554077068,-17.5438229797257,1.29266879315851));
#144236=CARTESIAN_POINT('Ctrl Pts',(20.9174037166616,-17.6154566187107,
1.29684736367005));
#144237=CARTESIAN_POINT('Ctrl Pts',(20.9620407587122,-17.6883765739312,
1.30110096824612));
#144238=CARTESIAN_POINT('Ctrl Pts',(21.0030716111862,-17.7636181037575,
1.30535457282219));
#144239=CARTESIAN_POINT('Ctrl Pts',(21.04025352208,-17.8407868377788,1.30960817739826));
#144240=CARTESIAN_POINT('Ctrl Pts',(21.0767133920066,-17.9164570208649,
1.3137791806048));
#144241=CARTESIAN_POINT('Ctrl Pts',(21.1094722614084,-17.9939797943654,
1.31795018381133));
#144242=CARTESIAN_POINT('Ctrl Pts',(21.1383468600458,-18.0729572384759,
1.32212118701786));
#144243=CARTESIAN_POINT('Ctrl Pts',(21.1672117626761,-18.1519081621879,
1.32629078961353));
#144244=CARTESIAN_POINT('Ctrl Pts',(21.1921948271095,-18.2323123546667,
1.33046039220919));
#144245=CARTESIAN_POINT('Ctrl Pts',(21.2131612187129,-18.3137526720542,
1.33462999480485));
#144246=CARTESIAN_POINT('Ctrl Pts',(21.2341268601602,-18.3951900755901,
1.33879944821638));
#144247=CARTESIAN_POINT('Ctrl Pts',(21.2510760006384,-18.4776630845828,
1.34296890162792));
#144248=CARTESIAN_POINT('Ctrl Pts',(21.263924266104,-18.560741507724,1.34713835503945));
#144249=CARTESIAN_POINT('Ctrl Pts',(21.2772250217302,-18.6467457864309,
1.35145464824414));
#144250=CARTESIAN_POINT('Ctrl Pts',(21.2861305792208,-18.7333983970714,
1.35577094144884));
#144251=CARTESIAN_POINT('Ctrl Pts',(21.2906057031231,-18.8202150283277,
1.36008723465353));
#144252=CARTESIAN_POINT('Ctrl Pts',(21.2949348018955,-18.90419879727,1.36426268543923));
#144253=CARTESIAN_POINT('Ctrl Pts',(21.2951181997827,-18.9883355761622,
1.36843813622492));
#144254=CARTESIAN_POINT('Ctrl Pts',(21.2911771392428,-19.0721876804587,
1.37261358701061));
#144255=CARTESIAN_POINT('Ctrl Pts',(21.2870366744248,-19.1602824164424,
1.3770003014248));
#144256=CARTESIAN_POINT('Ctrl Pts',(21.2783434340466,-19.2480623296263,
1.381387015839));
#144257=CARTESIAN_POINT('Ctrl Pts',(21.2651832590201,-19.3350291232486,
1.38577373025319));
#144258=CARTESIAN_POINT('Ctrl Pts',(21.2520230839935,-19.421995916871,1.39016044466739));
#144259=CARTESIAN_POINT('Ctrl Pts',(21.2343961652463,-19.5081490374756,
1.39454715908158));
#144260=CARTESIAN_POINT('Ctrl Pts',(21.2124488480671,-19.5930080401328,
1.39893387349578));
#144261=CARTESIAN_POINT('Ctrl Pts',(21.1915163486012,-19.6739432639369,
1.40311775147879));
#144262=CARTESIAN_POINT('Ctrl Pts',(21.1665762580736,-19.7540026330353,
1.40730162946179));
#144263=CARTESIAN_POINT('Ctrl Pts',(21.1377183899587,-19.8327598434161,
1.4114855074448));
#144264=CARTESIAN_POINT('Ctrl Pts',(21.1088989075933,-19.9114122936482,
1.41566382017635));
#144265=CARTESIAN_POINT('Ctrl Pts',(21.0761721509734,-19.988765596162,1.4198421329079));
#144266=CARTESIAN_POINT('Ctrl Pts',(21.0396783452697,-20.0644061165575,
1.42402044563945));
#144267=CARTESIAN_POINT('Ctrl Pts',(21.0032221304776,-20.1399687224669,
1.4281944544465));
#144268=CARTESIAN_POINT('Ctrl Pts',(20.9630067721328,-20.2138216382969,
1.43236846325355));
#144269=CARTESIAN_POINT('Ctrl Pts',(20.9192209903055,-20.285570104467,1.4365424720606));
#144270=CARTESIAN_POINT('Ctrl Pts',(20.8754640550467,-20.3572713019358,
1.44071373098342));
#144271=CARTESIAN_POINT('Ctrl Pts',(20.8281416060815,-20.4268704111564,
1.44488498990625));
#144272=CARTESIAN_POINT('Ctrl Pts',(20.7774882140691,-20.4939973796867,
1.44905624882907));
#144273=CARTESIAN_POINT('Ctrl Pts',(20.7268554189014,-20.5610970528337,
1.45322581162121));
#144274=CARTESIAN_POINT('Ctrl Pts',(20.6728946507595,-20.6257262172986,
1.45739537441335));
#144275=CARTESIAN_POINT('Ctrl Pts',(20.6158828807294,-20.6875451083788,
1.46156493720549));
#144276=CARTESIAN_POINT('Ctrl Pts',(20.5588584185249,-20.7493777618128,
1.46573542824136));
#144277=CARTESIAN_POINT('Ctrl Pts',(20.4987819053236,-20.8083985496803,
1.46990591927723));
#144278=CARTESIAN_POINT('Ctrl Pts',(20.4359689278453,-20.8643027398006,
1.47407641031309));
#144279=CARTESIAN_POINT('Ctrl Pts',(20.3899160356864,-20.9052902831747,
1.47713410924149));
#144280=CARTESIAN_POINT('Ctrl Pts',(20.3423929948226,-20.9446032322061,
1.48019180816988));
#144281=CARTESIAN_POINT('Ctrl Pts',(20.2935357468249,-20.9821350335323,
1.48324950709828));
#144282=CARTESIAN_POINT('Origin',(18.734,-18.952,-1.76670989022851));
#144283=CARTESIAN_POINT('',(20.2935357468249,-20.9821350335323,2.34989189284213));
#144284=CARTESIAN_POINT('',(20.2935357468249,-20.9821350335323,2.28327545627391));
#144285=CARTESIAN_POINT('',(20.2935357468249,-20.9821350335323,-1.76670989022851));
#144286=CARTESIAN_POINT('',(16.1742339454204,-18.95300766776,1.83329006740176));
#144287=CARTESIAN_POINT('Ctrl Pts',(16.174000198019,-18.953006904815,1.8332901097715));
#144288=CARTESIAN_POINT('Ctrl Pts',(16.1739663681252,-18.8669962708809,
1.83754657623655));
#144289=CARTESIAN_POINT('Ctrl Pts',(16.1782715498346,-18.7810104795588,
1.8418030427016));
#144290=CARTESIAN_POINT('Ctrl Pts',(16.186881959491,-18.6955049947587,1.84605950916664));
#144291=CARTESIAN_POINT('Ctrl Pts',(16.1954973714571,-18.6099498346313,
1.85031844847147));
#144292=CARTESIAN_POINT('Ctrl Pts',(16.2084229438518,-18.5248759665389,
1.85457738777631));
#144293=CARTESIAN_POINT('Ctrl Pts',(16.2255732751413,-18.4407316105854,
1.85883632708114));
#144294=CARTESIAN_POINT('Ctrl Pts',(16.242752034236,-18.3564477798121,1.86310232585877));
#144295=CARTESIAN_POINT('Ctrl Pts',(16.2641694501873,-18.273096962922,1.86736832463641));
#144296=CARTESIAN_POINT('Ctrl Pts',(16.2896893999554,-18.1911151923519,
1.87163432341404));
#144297=CARTESIAN_POINT('Ctrl Pts',(16.315231796287,-18.1090613131363,1.87590407443307));
#144298=CARTESIAN_POINT('Ctrl Pts',(16.3448837660304,-18.02837928517,1.88017382545211));
#144299=CARTESIAN_POINT('Ctrl Pts',(16.3784607475836,-17.9494857455749,
1.88444357647114));
#144300=CARTESIAN_POINT('Ctrl Pts',(16.4121081360754,-17.8704267756062,
1.88872228065047));
#144301=CARTESIAN_POINT('Ctrl Pts',(16.4496967908486,-17.7931641763823,
1.89300098482979));
#144302=CARTESIAN_POINT('Ctrl Pts',(16.4909957508862,-17.7180907900264,
1.89727968900912));
#144303=CARTESIAN_POINT('Ctrl Pts',(16.5197685295266,-17.6657875377064,
1.90026064078387));
#144304=CARTESIAN_POINT('Ctrl Pts',(16.550341278611,-17.6145463427439,1.90324159255863));
#144305=CARTESIAN_POINT('Ctrl Pts',(16.582623920045,-17.5644910945881,1.90622254433338));
#144306=CARTESIAN_POINT('Ctrl Pts',(16.6279420233621,-17.494223953898,1.91040717962067));
#144307=CARTESIAN_POINT('Ctrl Pts',(16.6767906254559,-17.4260486191802,
1.91459181490796));
#144308=CARTESIAN_POINT('Ctrl Pts',(16.7289503547201,-17.3603417703656,
1.91877645019526));
#144309=CARTESIAN_POINT('Ctrl Pts',(16.7810358412115,-17.2947284469338,
1.92295512918386));
#144310=CARTESIAN_POINT('Ctrl Pts',(16.8364228098559,-17.2315769875612,
1.92713380817247));
#144311=CARTESIAN_POINT('Ctrl Pts',(16.8948480567242,-17.1712360825912,
1.93131248716107));
#144312=CARTESIAN_POINT('Ctrl Pts',(16.9543205181338,-17.1098136268106,
1.93556606482165));
#144313=CARTESIAN_POINT('Ctrl Pts',(17.0169409883808,-17.0513038784722,
1.93981964248222));
#144314=CARTESIAN_POINT('Ctrl Pts',(17.0823881640358,-16.9960403012069,
1.94407322014279));
#144315=CARTESIAN_POINT('Ctrl Pts',(17.1465665360848,-16.9418481013602,
1.94824433504435));
#144316=CARTESIAN_POINT('Ctrl Pts',(17.2134626230333,-16.8907776412553,
1.95241544994592));
#144317=CARTESIAN_POINT('Ctrl Pts',(17.2827368115807,-16.8431057025211,
1.95658656484748));
#144318=CARTESIAN_POINT('Ctrl Pts',(17.3519877545941,-16.795449760505,1.96075628009652));
#144319=CARTESIAN_POINT('Ctrl Pts',(17.4236148357283,-16.7511903355778,
1.96492599534557));
#144320=CARTESIAN_POINT('Ctrl Pts',(17.4972477392743,-16.7105621031155,
1.96909571059461));
#144321=CARTESIAN_POINT('Ctrl Pts',(17.570878022714,-16.6699353163424,1.97326527747115));
#144322=CARTESIAN_POINT('Ctrl Pts',(17.6465135834573,-16.63293968663,1.9774348443477));
#144323=CARTESIAN_POINT('Ctrl Pts',(17.7237588789708,-16.599764281076,1.98160441122425));
#144324=CARTESIAN_POINT('Ctrl Pts',(17.8037199857115,-16.5654224855398,
1.98592057287346));
#144325=CARTESIAN_POINT('Ctrl Pts',(17.8854056436378,-16.5351747548241,
1.99023673452268));
#144326=CARTESIAN_POINT('Ctrl Pts',(17.9683557183505,-16.5091760534215,
1.99455289617189));
#144327=CARTESIAN_POINT('Ctrl Pts',(18.0486037412862,-16.4840242450153,
1.9987284612961));
#144328=CARTESIAN_POINT('Ctrl Pts',(18.1300346026626,-16.4628489694374,
2.0029040264203));
#144329=CARTESIAN_POINT('Ctrl Pts',(18.2122191473171,-16.4457388919401,
2.0070795915445));
#144330=CARTESIAN_POINT('Ctrl Pts',(18.2985545773168,-16.4277646377265,
2.01146605145622));
#144331=CARTESIAN_POINT('Ctrl Pts',(18.3857212504154,-16.414277123386,2.01585251136794));
#144332=CARTESIAN_POINT('Ctrl Pts',(18.4732153214913,-16.4053175793878,
2.02023897127966));
#144333=CARTESIAN_POINT('Ctrl Pts',(18.5607093925672,-16.3963580353896,
2.02462543119138));
#144334=CARTESIAN_POINT('Ctrl Pts',(18.6485302783096,-16.3919264150074,
2.0290118911031));
#144335=CARTESIAN_POINT('Ctrl Pts',(18.7361763184416,-16.3920009250709,
2.03339835101482));
#144336=CARTESIAN_POINT('Ctrl Pts',(18.8197896747137,-16.3920720068501,
2.03758298542408));
#144337=CARTESIAN_POINT('Ctrl Pts',(18.9035551457573,-16.3962439324391,
2.04176761983334));
#144338=CARTESIAN_POINT('Ctrl Pts',(18.9870372618429,-16.4045361348747,
2.0459522542426));
#144339=CARTESIAN_POINT('Ctrl Pts',(19.0704005515259,-16.4128165343922,
2.05013093234557));
#144340=CARTESIAN_POINT('Ctrl Pts',(19.1534808335077,-16.4252055165322,
2.05430961044854));
#144341=CARTESIAN_POINT('Ctrl Pts',(19.2358424472477,-16.4416705080527,
2.05848828855151));
#144342=CARTESIAN_POINT('Ctrl Pts',(19.3196803332532,-16.4584306226193,
2.06274186643254));
#144343=CARTESIAN_POINT('Ctrl Pts',(19.4027730512138,-16.4794143083236,
2.06699544431357));
#144344=CARTESIAN_POINT('Ctrl Pts',(19.4846662953171,-16.5045318974346,
2.0712490221946));
#144345=CARTESIAN_POINT('Ctrl Pts',(19.5649718796635,-16.5291625332462,
2.07542013619845));
#144346=CARTESIAN_POINT('Ctrl Pts',(19.6441236233212,-16.5577680742246,
2.07959125020228));
#144347=CARTESIAN_POINT('Ctrl Pts',(19.721704970629,-16.5902127760963,2.08376236420613));
#144348=CARTESIAN_POINT('Ctrl Pts',(19.7992602848132,-16.6226465908545,
2.0879320785549));
#144349=CARTESIAN_POINT('Ctrl Pts',(19.8752458251392,-16.6589168306477,
2.09210179290367));
#144350=CARTESIAN_POINT('Ctrl Pts',(19.949263822001,-16.6988391440167,2.09627150725245));
#144351=CARTESIAN_POINT('Ctrl Pts',(20.0232791850289,-16.7387600368021,
2.10044107322737));
#144352=CARTESIAN_POINT('Ctrl Pts',(20.0953267393063,-16.7823325256475,
2.1046106392023));
#144353=CARTESIAN_POINT('Ctrl Pts',(20.1650334097648,-16.8293263604273,
2.10878020517723));
#144354=CARTESIAN_POINT('Ctrl Pts',(20.2371908797447,-16.8779724397775,
2.11309636788714));
#144355=CARTESIAN_POINT('Ctrl Pts',(20.30683935496,-16.9302846355633,2.11741253059706));
#144356=CARTESIAN_POINT('Ctrl Pts',(20.3735994723764,-16.9859599266081,
2.12172869330698));
#144357=CARTESIAN_POINT('Ctrl Pts',(20.4381848869935,-17.03982160174,2.12590425753548));
#144358=CARTESIAN_POINT('Ctrl Pts',(20.5000669160013,-17.0968302774532,
2.13007982176398));
#144359=CARTESIAN_POINT('Ctrl Pts',(20.5589387125302,-17.1566730950859,
2.13425538599248));
#144360=CARTESIAN_POINT('Ctrl Pts',(20.6207839821291,-17.2195384297327,
2.13864184794311));
#144361=CARTESIAN_POINT('Ctrl Pts',(20.6793065465875,-17.2855312985542,
2.14302830989374));
#144362=CARTESIAN_POINT('Ctrl Pts',(20.7341990153404,-17.354250364096,2.14741477184436));
#144363=CARTESIAN_POINT('Ctrl Pts',(20.7890914840933,-17.4229694296379,
2.15180123379499));
#144364=CARTESIAN_POINT('Ctrl Pts',(20.840353580694,-17.4944141761338,2.15618769574562));
#144365=CARTESIAN_POINT('Ctrl Pts',(20.8877320902557,-17.5681509896658,
2.16057415769624));
#144366=CARTESIAN_POINT('Ctrl Pts',(20.9329306422981,-17.638495059893,2.16475879183927));
#144367=CARTESIAN_POINT('Ctrl Pts',(20.9747633711847,-17.7111867434279,
2.16894342598229));
#144368=CARTESIAN_POINT('Ctrl Pts',(21.0129782252709,-17.7858703979656,
2.17312806012532));
#144369=CARTESIAN_POINT('Ctrl Pts',(21.0511386851992,-17.8604477494804,
2.17730673795485));
#144370=CARTESIAN_POINT('Ctrl Pts',(21.0856912912936,-17.9370110341171,
2.18148541578439));
#144371=CARTESIAN_POINT('Ctrl Pts',(21.116427617672,-18.0151762991077,2.18566409361392));
#144372=CARTESIAN_POINT('Ctrl Pts',(21.1477148729796,-18.0947426263206,
2.18991767156241));
#144373=CARTESIAN_POINT('Ctrl Pts',(21.1750474280233,-18.1759685243987,
2.1941712495109));
#144374=CARTESIAN_POINT('Ctrl Pts',(21.1982547719715,-18.2584234585746,
2.19842482745939));
#144375=CARTESIAN_POINT('Ctrl Pts',(21.2210121944976,-18.33927983665,2.20259594117397));
#144376=CARTESIAN_POINT('Ctrl Pts',(21.2398027993344,-18.421317558152,2.20676705488855));
#144377=CARTESIAN_POINT('Ctrl Pts',(21.2545152522161,-18.504112889953,2.21093816860314));
#144378=CARTESIAN_POINT('Ctrl Pts',(21.269222768182,-18.5868804389239,2.21510788265736));
#144379=CARTESIAN_POINT('Ctrl Pts',(21.2798547695695,-18.6704046407403,
2.21927759671159));
#144380=CARTESIAN_POINT('Ctrl Pts',(21.2863509615978,-18.7542512482193,
2.22344731076582));
#144381=CARTESIAN_POINT('Ctrl Pts',(21.2928469224598,-18.838094872027,2.22761687644128));
#144382=CARTESIAN_POINT('Ctrl Pts',(21.2952073318929,-18.9222604199623,
2.23178644211675));
#144383=CARTESIAN_POINT('Ctrl Pts',(21.2934238553148,-19.0063095649563,
2.23595600779222));
#144384=CARTESIAN_POINT('Ctrl Pts',(21.2915776736488,-19.0933137860529,
2.240272170841));
#144385=CARTESIAN_POINT('Ctrl Pts',(21.2852907961481,-19.1801927391156,
2.24458833388979));
#144386=CARTESIAN_POINT('Ctrl Pts',(21.2746126736341,-19.2664634200821,
2.24890449693858));
#144387=CARTESIAN_POINT('Ctrl Pts',(21.2642823912523,-19.3499238312635,
2.25308006085835));
#144388=CARTESIAN_POINT('Ctrl Pts',(21.2498426885289,-19.432814534908,2.25725562477812));
#144389=CARTESIAN_POINT('Ctrl Pts',(21.2313905396644,-19.5147081769395,
2.26143118869789));
#144390=CARTESIAN_POINT('Ctrl Pts',(21.2120064127096,-19.6007380895309,
2.26581765131119));
#144391=CARTESIAN_POINT('Ctrl Pts',(21.1881940056837,-19.6856670076436,
2.27020411392449));
#144392=CARTESIAN_POINT('Ctrl Pts',(21.1601243952761,-19.7690192278315,
2.27459057653779));
#144393=CARTESIAN_POINT('Ctrl Pts',(21.1320547848684,-19.8523714480194,
2.27897703915109));
#144394=CARTESIAN_POINT('Ctrl Pts',(21.0997282551217,-19.9341464586594,
2.28336350176438));
#144395=CARTESIAN_POINT('Ctrl Pts',(21.0633723464422,-20.0138966388639,
2.28774996437768));
#144396=CARTESIAN_POINT('Ctrl Pts',(21.028688700058,-20.0899785509864,2.29193466292279));
#144397=CARTESIAN_POINT('Ctrl Pts',(20.9902091092465,-20.1645010086708,
2.2961193614679));
#144398=CARTESIAN_POINT('Ctrl Pts',(20.9480961900739,-20.2370595554683,
2.30030406001301));
#144399=CARTESIAN_POINT('Ctrl Pts',(20.9060523787106,-20.3094990328135,
2.30448189141722));
#144400=CARTESIAN_POINT('Ctrl Pts',(20.8603873210434,-20.3799806118459,
2.30865972282143));
#144401=CARTESIAN_POINT('Ctrl Pts',(20.811310912052,-20.4481214438239,2.31283755422565));
#144402=CARTESIAN_POINT('Ctrl Pts',(20.7622817553052,-20.5161966677566,
2.31701136308795));
#144403=CARTESIAN_POINT('Ctrl Pts',(20.7098480348053,-20.5819352475709,
2.32118517195026));
#144404=CARTESIAN_POINT('Ctrl Pts',(20.6542641570203,-20.6449812660698,
2.32535898081256));
#144405=CARTESIAN_POINT('Ctrl Pts',(20.5987134202835,-20.7079896943315,
2.32953030110432));
#144406=CARTESIAN_POINT('Ctrl Pts',(20.5400165562304,-20.7683084024141,
2.33370162139608));
#144407=CARTESIAN_POINT('Ctrl Pts',(20.4784688818988,-20.825613706207,2.33787294168784));
#144408=CARTESIAN_POINT('Ctrl Pts',(20.4193558241849,-20.8806522071286,
2.34187925873927));
#144409=CARTESIAN_POINT('Ctrl Pts',(20.3576135312872,-20.9329109209508,
2.3458855757907));
#144410=CARTESIAN_POINT('Ctrl Pts',(20.2935357468249,-20.9821350335323,
2.34989189284213));
#144411=CARTESIAN_POINT('Ctrl Pts',(20.294072348973,-20.9828452881321,1.55000082941897));
#144412=CARTESIAN_POINT('Ctrl Pts',(19.7490823179128,-21.3927990376574,
1.58395752993615));
#144413=CARTESIAN_POINT('Ctrl Pts',(18.1401763549456,-21.8312444115751,
1.6603061660138));
#144414=CARTESIAN_POINT('Ctrl Pts',(16.4202753042621,-20.536339124494,1.75473569408312));
#144415=CARTESIAN_POINT('Ctrl Pts',(16.1765569610219,-19.3178333678849,
1.81520852163526));
#144416=CARTESIAN_POINT('Ctrl Pts',(16.1778407221624,-18.9530194401788,
1.83328941362691));
#144417=CARTESIAN_POINT('',(16.1740004726294,-18.9504444093098,1.76670989019937));
#144418=CARTESIAN_POINT('Ctrl Pts',(20.2935357468249,-20.9821350335323,
1.48324950709828));
#144419=CARTESIAN_POINT('Ctrl Pts',(20.2268277705136,-21.0333796413724,
1.48742438218933));
#144420=CARTESIAN_POINT('Ctrl Pts',(20.1576316687033,-21.0813019538135,
1.49159925728038));
#144421=CARTESIAN_POINT('Ctrl Pts',(20.0863185925296,-21.1256684255651,
1.49577413237143));
#144422=CARTESIAN_POINT('Ctrl Pts',(20.0149603823384,-21.170062976839,1.49995164973925));
#144423=CARTESIAN_POINT('Ctrl Pts',(19.9414829328826,-21.2108969849863,
1.50412916710708));
#144424=CARTESIAN_POINT('Ctrl Pts',(19.8662815900183,-21.2479831011803,
1.50830668447491));
#144425=CARTESIAN_POINT('Ctrl Pts',(19.7909572329255,-21.28512988278,1.51249103541853));
#144426=CARTESIAN_POINT('Ctrl Pts',(19.7139037757318,-21.3185163539148,
1.51667538636215));
#144427=CARTESIAN_POINT('Ctrl Pts',(19.6355356527249,-21.3480036450026,
1.52085973730577));
#144428=CARTESIAN_POINT('Ctrl Pts',(19.6027605043788,-21.3603358319002,
1.52260971826292));
#144429=CARTESIAN_POINT('Ctrl Pts',(19.569755577939,-21.3719866256104,1.52435969922007));
#144430=CARTESIAN_POINT('Ctrl Pts',(19.5365517913642,-21.3829485025763,
1.52610968017722));
#144431=CARTESIAN_POINT('Ctrl Pts',(19.4571532093435,-21.4091610999082,
1.53029432358371));
#144432=CARTESIAN_POINT('Ctrl Pts',(19.376321311697,-21.4315284613918,1.53447896699021));
#144433=CARTESIAN_POINT('Ctrl Pts',(19.294463394386,-21.4498952707336,1.53866361039671));
#144434=CARTESIAN_POINT('Ctrl Pts',(19.2127219863795,-21.4682359383869,
1.54284229775267));
#144435=CARTESIAN_POINT('Ctrl Pts',(19.1299579044461,-21.4825872641847,
1.54702098510862));
#144436=CARTESIAN_POINT('Ctrl Pts',(19.0465949711256,-21.4928432427104,
1.55119967246457));
#144437=CARTESIAN_POINT('Ctrl Pts',(18.9617380510235,-21.5032830235057,
1.55545324806433));
#144438=CARTESIAN_POINT('Ctrl Pts',(18.8762610608014,-21.5094790670078,
1.55970682366408));
#144439=CARTESIAN_POINT('Ctrl Pts',(18.7906234643,-21.5113737091896,1.56396039926383));
#144440=CARTESIAN_POINT('Ctrl Pts',(18.7066458764304,-21.5132316254179,
1.56813152308422));
#144441=CARTESIAN_POINT('Ctrl Pts',(18.6225143342412,-21.5109533994767,
1.5723026469046));
#144442=CARTESIAN_POINT('Ctrl Pts',(18.5386669500421,-21.5045369732081,
1.57647377072499));
#144443=CARTESIAN_POINT('Ctrl Pts',(18.4548476977165,-21.4981226997328,
1.5806434950798));
#144444=CARTESIAN_POINT('Ctrl Pts',(18.3713128723448,-21.4875730184253,
1.58481321943461));
#144445=CARTESIAN_POINT('Ctrl Pts',(18.2884980293892,-21.4729379195414,
1.58898294378941));
#144446=CARTESIAN_POINT('Ctrl Pts',(18.2056861297709,-21.4583033408063,
1.59315251994729));
#144447=CARTESIAN_POINT('Ctrl Pts',(18.1235946145539,-21.4395837140867,
1.59732209610518));
#144448=CARTESIAN_POINT('Ctrl Pts',(18.0426500220353,-21.4168803638246,
1.60149167226306));
#144449=CARTESIAN_POINT('Ctrl Pts',(17.9588599464441,-21.3933789120853,
1.60580782347935));
#144450=CARTESIAN_POINT('Ctrl Pts',(17.8762994409707,-21.3656085753716,
1.61012397469565));
#144451=CARTESIAN_POINT('Ctrl Pts',(17.7954238784078,-21.3337377823717,
1.61444012591195));
#144452=CARTESIAN_POINT('Ctrl Pts',(17.7171824220401,-21.3029050168134,
1.61861570066365));
#144453=CARTESIAN_POINT('Ctrl Pts',(17.6405182464777,-21.2682350343783,
1.62279127541534));
#144454=CARTESIAN_POINT('Ctrl Pts',(17.5658209821028,-21.2299283970627,
1.62696685016703));
#144455=CARTESIAN_POINT('Ctrl Pts',(17.4873515385791,-21.1896872913332,
1.63135328961563));
#144456=CARTESIAN_POINT('Ctrl Pts',(17.4110533971718,-21.1454328556654,
1.63573972906424));
#144457=CARTESIAN_POINT('Ctrl Pts',(17.3373445042313,-21.097449469491,1.64012616851284));
#144458=CARTESIAN_POINT('Ctrl Pts',(17.2636356112909,-21.0494660833166,
1.64451260796144));
#144459=CARTESIAN_POINT('Ctrl Pts',(17.1925163913427,-20.9977541493591,
1.64889904741004));
#144460=CARTESIAN_POINT('Ctrl Pts',(17.1243635064003,-20.9426457139511,
1.65328548685865));
#144461=CARTESIAN_POINT('Ctrl Pts',(17.0601943718463,-20.8907585398463,
1.6574155251311));
#144462=CARTESIAN_POINT('Ctrl Pts',(16.9984022164044,-20.8356563912925,
1.66154556340355));
#144463=CARTESIAN_POINT('Ctrl Pts',(16.9393333497915,-20.7775880188667,
1.66567560167601));
#144464=CARTESIAN_POINT('Ctrl Pts',(16.8791242536685,-20.7183987298625,
1.66988536369781));
#144465=CARTESIAN_POINT('Ctrl Pts',(16.8217451259872,-20.6561277338344,
1.67409512571962));
#144466=CARTESIAN_POINT('Ctrl Pts',(16.7675298313412,-20.5910836085371,
1.67830488774143));
#144467=CARTESIAN_POINT('Ctrl Pts',(16.7144792342514,-20.5274368146437,
1.6824242121926));
#144468=CARTESIAN_POINT('Ctrl Pts',(16.6644582227548,-20.4611352262018,
1.68654353664378));
#144469=CARTESIAN_POINT('Ctrl Pts',(16.6177431437369,-20.3925057855904,
1.69066286109495));
#144470=CARTESIAN_POINT('Ctrl Pts',(16.5710563620564,-20.3239179167901,
1.69477969029369));
#144471=CARTESIAN_POINT('Ctrl Pts',(16.5276718049372,-20.2530053838409,
1.69889651949243));
#144472=CARTESIAN_POINT('Ctrl Pts',(16.4878244177667,-20.1801267254559,
1.70301334869118));
#144473=CARTESIAN_POINT('Ctrl Pts',(16.4479884749074,-20.1072689980804,
1.70712899552195));
#144474=CARTESIAN_POINT('Ctrl Pts',(16.4116879114515,-20.0324466815215,
1.71124464235271));
#144475=CARTESIAN_POINT('Ctrl Pts',(16.3791125478311,-19.9560443653632,
1.71536028918348));
#144476=CARTESIAN_POINT('Ctrl Pts',(16.3452431871199,-19.8766071061112,
1.71963942260147));
#144477=CARTESIAN_POINT('Ctrl Pts',(16.3154014154543,-19.795462185038,1.72391855601946));
#144478=CARTESIAN_POINT('Ctrl Pts',(16.28974541526,-19.7130647311349,1.72819768943746));
#144479=CARTESIAN_POINT('Ctrl Pts',(16.2650470315947,-19.6337427825017,
1.73231710314623));
#144480=CARTESIAN_POINT('Ctrl Pts',(16.2442275676729,-19.5532606331567,
1.736436516855));
#144481=CARTESIAN_POINT('Ctrl Pts',(16.2273766226977,-19.4720377335941,
1.74055593056377));
#144482=CARTESIAN_POINT('Ctrl Pts',(16.2105163820987,-19.3907700283831,
1.74467761669822));
#144483=CARTESIAN_POINT('Ctrl Pts',(16.1976290876222,-19.3087612270287,
1.74879930283266));
#144484=CARTESIAN_POINT('Ctrl Pts',(16.1887526585032,-19.2264375531951,
1.7529209889671));
#144485=CARTESIAN_POINT('Ctrl Pts',(16.1798641546722,-19.1440018934889,
1.75704828188022));
#144486=CARTESIAN_POINT('Ctrl Pts',(16.1749974203025,-19.0612509779236,
1.76117557479333));
#144487=CARTESIAN_POINT('Ctrl Pts',(16.174138321227,-18.9786117558525,1.76530286770644));
#144488=CARTESIAN_POINT('Ctrl Pts',(16.1740406969692,-18.9692209964452,
1.76577187520409));
#144489=CARTESIAN_POINT('Ctrl Pts',(16.1739947684326,-18.9598316737892,
1.76624088270173));
#144490=CARTESIAN_POINT('Ctrl Pts',(16.1740004726294,-18.9504444093098,
1.76670989019937));
#144491=CARTESIAN_POINT('Ctrl Pts',(16.1740004726298,-18.9504444087268,
1.7667098902285));
#144492=CARTESIAN_POINT('Ctrl Pts',(16.1740562220874,-18.8586988534878,
1.77129369133236));
#144493=CARTESIAN_POINT('Ctrl Pts',(16.1790436176654,-18.7671041921699,
1.77587749243622));
#144494=CARTESIAN_POINT('Ctrl Pts',(16.1889163327552,-18.6760486877659,
1.78046129354008));
#144495=CARTESIAN_POINT('Ctrl Pts',(16.1979293239818,-18.5929223689306,
1.78464593360694));
#144496=CARTESIAN_POINT('Ctrl Pts',(16.2110359189735,-18.510083390536,1.78883057367379));
#144497=CARTESIAN_POINT('Ctrl Pts',(16.2282088655394,-18.4279668040492,
1.79301521374065));
#144498=CARTESIAN_POINT('Ctrl Pts',(16.24535736882,-18.3459670990266,1.79719389755824));
#144499=CARTESIAN_POINT('Ctrl Pts',(16.2665606337553,-18.2646881899744,
1.80137258137583));
#144500=CARTESIAN_POINT('Ctrl Pts',(16.2917396797569,-18.184559755964,1.80555126519342));
#144501=CARTESIAN_POINT('Ctrl Pts',(16.3173699983022,-18.1029952166205,
1.80980484165292));
#144502=CARTESIAN_POINT('Ctrl Pts',(16.3471199655449,-18.0226232777798,
1.81405841811242));
#144503=CARTESIAN_POINT('Ctrl Pts',(16.3808518405096,-17.9438860483621,
1.81831199457193));
#144504=CARTESIAN_POINT('Ctrl Pts',(16.4139298146452,-17.8666751598207,
1.82248311438838));
#144505=CARTESIAN_POINT('Ctrl Pts',(16.4508365039862,-17.7910366100589,
1.82665423420484));
#144506=CARTESIAN_POINT('Ctrl Pts',(16.4913923920135,-17.7173700487186,
1.8308253540213));
#144507=CARTESIAN_POINT('Ctrl Pts',(16.531934671396,-17.6437282064046,1.83499507420651));
#144508=CARTESIAN_POINT('Ctrl Pts',(16.5761234959118,-17.5720574410135,
1.83916479439172));
#144509=CARTESIAN_POINT('Ctrl Pts',(16.6237330298035,-17.5027335253662,
1.84333451457693));
#144510=CARTESIAN_POINT('Ctrl Pts',(16.6713408697582,-17.4334120762489,
1.8475040864044));
#144511=CARTESIAN_POINT('Ctrl Pts',(16.7223689159663,-17.3664376895872,
1.85167365823187));
#144512=CARTESIAN_POINT('Ctrl Pts',(16.7765483383152,-17.3021566764789,
1.85584323005933));
#144513=CARTESIAN_POINT('Ctrl Pts',(16.8326324736236,-17.2356158223938,
1.86015938590618));
#144514=CARTESIAN_POINT('Ctrl Pts',(16.8920933527671,-17.1719616497153,
1.86447554175303));
#144515=CARTESIAN_POINT('Ctrl Pts',(16.9545891225287,-17.1115389357183,
1.86879169759988));
#144516=CARTESIAN_POINT('Ctrl Pts',(17.0150492806953,-17.0530843097644,
1.87296726766114));
#144517=CARTESIAN_POINT('Ctrl Pts',(17.0783492743462,-16.9976541389962,
1.87714283772241));
#144518=CARTESIAN_POINT('Ctrl Pts',(17.1441452217407,-16.9455200514219,
1.88131840778368));
#144519=CARTESIAN_POINT('Ctrl Pts',(17.2132640597166,-16.8907530377263,
1.88570485652332));
#144520=CARTESIAN_POINT('Ctrl Pts',(17.2851371188669,-16.8396241343394,
1.89009130526296));
#144521=CARTESIAN_POINT('Ctrl Pts',(17.3593324936003,-16.792396043982,1.89447775400259));
#144522=CARTESIAN_POINT('Ctrl Pts',(17.4335278683337,-16.7451679536245,
1.89886420274223));
#144523=CARTESIAN_POINT('Ctrl Pts',(17.5100450162907,-16.7018408959928,
1.90325065148187));
#144524=CARTESIAN_POINT('Ctrl Pts',(17.5884257348914,-16.662620257991,1.90763710022151));
#144525=CARTESIAN_POINT('Ctrl Pts',(17.6632002791341,-16.6252041002441,
1.91182173531041));
#144526=CARTESIAN_POINT('Ctrl Pts',(17.7399490034736,-16.5913855369184,
1.91600637039932));
#144527=CARTESIAN_POINT('Ctrl Pts',(17.8182913485561,-16.5613771385535,
1.92019100548822));
#144528=CARTESIAN_POINT('Ctrl Pts',(17.8965221835584,-16.5314114532182,
1.92436968429646));
#144529=CARTESIAN_POINT('Ctrl Pts',(17.9763417078038,-16.5052453236658,
1.92854836310471));
#144530=CARTESIAN_POINT('Ctrl Pts',(18.0573458795832,-16.4830449171111,
1.93272704191295));
#144531=CARTESIAN_POINT('Ctrl Pts',(18.1398019751916,-16.4604465890842,
1.93698061962087));
#144532=CARTESIAN_POINT('Ctrl Pts',(18.2234851739771,-16.4419577675956,
1.94123419732878));
#144533=CARTESIAN_POINT('Ctrl Pts',(18.3079491747708,-16.427701940277,1.9454877750367));
#144534=CARTESIAN_POINT('Ctrl Pts',(18.3907756952209,-16.4137224867601,
1.94965888980394));
#144535=CARTESIAN_POINT('Ctrl Pts',(18.4743525389444,-16.403813444343,1.95383000457117));
#144536=CARTESIAN_POINT('Ctrl Pts',(18.5582464958779,-16.3980401910389,
1.95800111933841));
#144537=CARTESIAN_POINT('Ctrl Pts',(18.6421123018441,-16.392268874974,1.96217083447069));
#144538=CARTESIAN_POINT('Ctrl Pts',(18.7262945511255,-16.390630623423,1.96634054960296));
#144539=CARTESIAN_POINT('Ctrl Pts',(18.8103550385198,-16.3931389431834,
1.97051026473523));
#144540=CARTESIAN_POINT('Ctrl Pts',(18.8944125351178,-16.3956471737001,
1.9746798315128));
#144541=CARTESIAN_POINT('Ctrl Pts',(18.9783478186396,-16.4023016676252,
1.97884939829037));
#144542=CARTESIAN_POINT('Ctrl Pts',(19.0617241844762,-16.4130638332346,
1.98301896506794));
#144543=CARTESIAN_POINT('Ctrl Pts',(19.1480319248428,-16.4242043787102,
1.98733512688752));
#144544=CARTESIAN_POINT('Ctrl Pts',(19.2337401905731,-16.4397467505396,
1.99165128870711));
#144545=CARTESIAN_POINT('Ctrl Pts',(19.3183740371495,-16.4595901250586,
1.99596745052669));
#144546=CARTESIAN_POINT('Ctrl Pts',(19.400250979758,-16.4787871118715,2.00014301559772));
#144547=CARTESIAN_POINT('Ctrl Pts',(19.4811219861016,-16.5020090222104,
2.00431858066876));
#144548=CARTESIAN_POINT('Ctrl Pts',(19.5605725242511,-16.529113733137,2.00849414573979));
#144549=CARTESIAN_POINT('Ctrl Pts',(19.644035868025,-16.5575874207753,2.01288060593365));
#144550=CARTESIAN_POINT('Ctrl Pts',(19.7259309366168,-16.590346235569,2.01726706612751));
#144551=CARTESIAN_POINT('Ctrl Pts',(19.8058030522791,-16.6271692067754,
2.02165352632137));
#144552=CARTESIAN_POINT('Ctrl Pts',(19.8856751679415,-16.6639921779819,
2.02603998651523));
#144553=CARTESIAN_POINT('Ctrl Pts',(19.9635238523658,-16.7048789684718,
2.03042644670909));
#144554=CARTESIAN_POINT('Ctrl Pts',(20.0389283878907,-16.7495554711919,
2.03481290690295));
#144555=CARTESIAN_POINT('Ctrl Pts',(20.1108634458004,-16.7921763399234,
2.03899753937721));
#144556=CARTESIAN_POINT('Ctrl Pts',(20.1808420875151,-16.8384044873328,
2.04318217185146));
#144557=CARTESIAN_POINT('Ctrl Pts',(20.2484795854365,-16.8880349844786,
2.04736680432571));
#144558=CARTESIAN_POINT('Ctrl Pts',(20.3160208091885,-16.9375948383417,
2.05154548045877));
#144559=CARTESIAN_POINT('Ctrl Pts',(20.3812271405152,-16.9905471526885,
2.05572415659182));
#144560=CARTESIAN_POINT('Ctrl Pts',(20.4437401590352,-17.0466421363476,
2.05990283272488));
#144561=CARTESIAN_POINT('Ctrl Pts',(20.5073737154297,-17.1037426154257,
2.06415641109403));
#144562=CARTESIAN_POINT('Ctrl Pts',(20.568216035996,-17.1640992946966,2.06840998946317));
#144563=CARTESIAN_POINT('Ctrl Pts',(20.625921711991,-17.2274037470478,2.07266356783232));
#144564=CARTESIAN_POINT('Ctrl Pts',(20.6825086170737,-17.2894808820044,
2.07683467979464));
#144565=CARTESIAN_POINT('Ctrl Pts',(20.7360790916418,-17.3543921543138,
2.08100579175696));
#144566=CARTESIAN_POINT('Ctrl Pts',(20.7863436747178,-17.4218086914226,
2.08517690371928));
#144567=CARTESIAN_POINT('Ctrl Pts',(20.8365913907808,-17.4892026059304,
2.08934661600422));
#144568=CARTESIAN_POINT('Ctrl Pts',(20.8835351437711,-17.5590997471374,
2.09351632828917));
#144569=CARTESIAN_POINT('Ctrl Pts',(20.9269263843814,-17.6311389654154,
2.09768604057411));
#144570=CARTESIAN_POINT('Ctrl Pts',(20.970316080766,-17.7031756199314,2.10185560446557));
#144571=CARTESIAN_POINT('Ctrl Pts',(21.010153279513,-17.7773538054376,2.10602516835703));
#144572=CARTESIAN_POINT('Ctrl Pts',(21.0462340501421,-17.8532854340807,
2.1101947322485));
#144573=CARTESIAN_POINT('Ctrl Pts',(21.0835834150717,-17.9318868070124,
2.11451089735982));
#144574=CARTESIAN_POINT('Ctrl Pts',(21.1169070502971,-18.0123667468948,
2.11882706247114));
#144575=CARTESIAN_POINT('Ctrl Pts',(21.1460326532687,-18.094271325205,2.12314322758247));
#144576=CARTESIAN_POINT('Ctrl Pts',(21.1742094633,-18.1735077875708,2.12731878969955));
#144577=CARTESIAN_POINT('Ctrl Pts',(21.1984574604608,-18.2540770310568,
2.13149435181663));
#144578=CARTESIAN_POINT('Ctrl Pts',(21.2186717693381,-18.3355535719509,
2.13566991393371));
#144579=CARTESIAN_POINT('Ctrl Pts',(21.2399070877016,-18.4211454314377,
2.14005638054216));
#144580=CARTESIAN_POINT('Ctrl Pts',(21.2566904008667,-18.507738082136,2.1444428471506));
#144581=CARTESIAN_POINT('Ctrl Pts',(21.268961401442,-18.5948296020113,2.14882931375904));
#144582=CARTESIAN_POINT('Ctrl Pts',(21.2812324020172,-18.6819211218865,
2.15321578036749));
#144583=CARTESIAN_POINT('Ctrl Pts',(21.2889911145759,-18.769510926268,2.15760224697593));
#144584=CARTESIAN_POINT('Ctrl Pts',(21.2922402934534,-18.8570968865022,
2.16198871358438));
#144585=CARTESIAN_POINT('Ctrl Pts',(21.295340067666,-18.9406554442682,2.16617348044096));
#144586=CARTESIAN_POINT('Ctrl Pts',(21.2943474565442,-19.0245215346741,
2.17035824729755));
#144587=CARTESIAN_POINT('Ctrl Pts',(21.2892265251078,-19.1082606968682,
2.17454301415413));
#144588=CARTESIAN_POINT('Ctrl Pts',(21.2841129263152,-19.1918799532477,
2.17872178885763));
#144589=CARTESIAN_POINT('Ctrl Pts',(21.2748827772586,-19.2753721871246,
2.18290056356113));
#144590=CARTESIAN_POINT('Ctrl Pts',(21.2615521105126,-19.3583007859252,
2.18707933826462));
#144591=CARTESIAN_POINT('Ctrl Pts',(21.2482373459004,-19.4411304593154,
2.19125312811358));
#144592=CARTESIAN_POINT('Ctrl Pts',(21.2308318605286,-19.5233973824746,
2.19542691796253));
#144593=CARTESIAN_POINT('Ctrl Pts',(21.2094035420871,-19.6046693679211,
2.19960070781149));
#144594=CARTESIAN_POINT('Ctrl Pts',(21.1879892258981,-19.6858882465004,
2.20377177031347));
#144595=CARTESIAN_POINT('Ctrl Pts',(21.1625574130303,-19.766113034728,2.20794283281545));
#144596=CARTESIAN_POINT('Ctrl Pts',(21.1332269868316,-19.8449220938352,
2.21211389531743));
#144597=CARTESIAN_POINT('Ctrl Pts',(21.1039069279009,-19.9237032967282,
2.21628348349639));
#144598=CARTESIAN_POINT('Ctrl Pts',(21.0706911534139,-20.0010693338703,
2.22045307167534));
#144599=CARTESIAN_POINT('Ctrl Pts',(21.0337478603941,-20.0766153914174,
2.2246226598543));
#144600=CARTESIAN_POINT('Ctrl Pts',(20.9968065435593,-20.1521574078251,
2.22879202499201));
#144601=CARTESIAN_POINT('Ctrl Pts',(20.9561383080146,-20.2258792256777,
2.23296139012972));
#144602=CARTESIAN_POINT('Ctrl Pts',(20.9119581930118,-20.297398866319,2.23713075526742));
#144603=CARTESIAN_POINT('Ctrl Pts',(20.8677415456929,-20.3689776461936,
2.24130356803231));
#144604=CARTESIAN_POINT('Ctrl Pts',(20.8200074609641,-20.4383502197373,
2.2454763807972));
#144605=CARTESIAN_POINT('Ctrl Pts',(20.7690150631306,-20.5051624811435,
2.24964919356209));
#144606=CARTESIAN_POINT('Ctrl Pts',(20.7180006959783,-20.5720035276221,
2.2538238041215));
#144607=CARTESIAN_POINT('Ctrl Pts',(20.6637255152003,-20.636281711919,2.25799841468091));
#144608=CARTESIAN_POINT('Ctrl Pts',(20.606488337404,-20.6976767817342,2.26217302524032));
#144609=CARTESIAN_POINT('Ctrl Pts',(20.5491647021454,-20.7591645895589,
2.26635394160043));
#144610=CARTESIAN_POINT('Ctrl Pts',(20.4888704630452,-20.8177602628929,
2.27053485796053));
#144611=CARTESIAN_POINT('Ctrl Pts',(20.425940338613,-20.8731813788849,2.27471577432064));
#144612=CARTESIAN_POINT('Ctrl Pts',(20.3829942629984,-20.911003001828,2.2775690016384));
#144613=CARTESIAN_POINT('Ctrl Pts',(20.3388213089917,-20.9473469766555,
2.28042222895615));
#144614=CARTESIAN_POINT('Ctrl Pts',(20.2935357468249,-20.9821350335323,
2.28327545627391));
#144615=CARTESIAN_POINT('Origin',(18.734,-18.952,-1.76670989022851));
#144616=CARTESIAN_POINT('',(20.2935357468249,-20.9821350335323,3.1498113676566));
#144617=CARTESIAN_POINT('',(20.2933493665352,-20.9818838108336,3.08342410800429));
#144618=CARTESIAN_POINT('',(20.2935357468249,-20.9821350335323,-1.76670989022851));
#144619=CARTESIAN_POINT('',(16.1740010149448,-18.9497204131756,2.63329010980609));
#144620=CARTESIAN_POINT('Ctrl Pts',(16.1740010149447,-18.9497204131756,
2.63329010980609));
#144621=CARTESIAN_POINT('Ctrl Pts',(16.1740928743929,-18.8465613267996,
2.63841342883191));
#144622=CARTESIAN_POINT('Ctrl Pts',(16.1804238944876,-18.7436786900648,
2.64353674785773));
#144623=CARTESIAN_POINT('Ctrl Pts',(16.1928719236877,-18.6417289897893,
2.64866006688355));
#144624=CARTESIAN_POINT('Ctrl Pts',(16.2055250386107,-18.5380996318225,
2.6538677944185));
#144625=CARTESIAN_POINT('Ctrl Pts',(16.2244983314994,-18.4354341185118,
2.65907552195346));
#144626=CARTESIAN_POINT('Ctrl Pts',(16.249614957165,-18.3343990293583,2.66428324948841));
#144627=CARTESIAN_POINT('Ctrl Pts',(16.2576437833537,-18.3021019692125,
2.66594796113293));
#144628=CARTESIAN_POINT('Ctrl Pts',(16.2662999939976,-18.2699713447297,
2.66761267277746));
#144629=CARTESIAN_POINT('Ctrl Pts',(16.2755767948953,-18.2380284707337,
2.66927738442199));
#144630=CARTESIAN_POINT('Ctrl Pts',(16.2988961609904,-18.1577327328976,
2.67346201883521));
#144631=CARTESIAN_POINT('Ctrl Pts',(16.3261969265522,-18.0784312369419,
2.67764665324844));
#144632=CARTESIAN_POINT('Ctrl Pts',(16.3573766633345,-18.0005476808496,
2.68183128766167));
#144633=CARTESIAN_POINT('Ctrl Pts',(16.3885120196228,-17.9227749823538,
2.68600996576607));
#144634=CARTESIAN_POINT('Ctrl Pts',(16.4235152107072,-17.8464166382457,
2.69018864387046));
#144635=CARTESIAN_POINT('Ctrl Pts',(16.4622338002163,-17.7718820679608,
2.69436732197485));
#144636=CARTESIAN_POINT('Ctrl Pts',(16.5016463923759,-17.6960115195325,
2.6986208998552));
#144637=CARTESIAN_POINT('Ctrl Pts',(16.5449087556002,-17.6220312333017,
2.70287447773556));
#144638=CARTESIAN_POINT('Ctrl Pts',(16.5918084260802,-17.55035266182,2.70712805561592));
#144639=CARTESIAN_POINT('Ctrl Pts',(16.6377988552168,-17.4800637188786,
2.71129916961483));
#144640=CARTESIAN_POINT('Ctrl Pts',(16.6872865541291,-17.4119884433509,
2.71547028361374));
#144641=CARTESIAN_POINT('Ctrl Pts',(16.7400252973106,-17.346489213666,2.71964139761265));
#144642=CARTESIAN_POINT('Ctrl Pts',(16.7927463434996,-17.2810119628777,
2.72381111195413));
#144643=CARTESIAN_POINT('Ctrl Pts',(16.8487159791043,-17.2181093992062,
2.72798082629561));
#144644=CARTESIAN_POINT('Ctrl Pts',(16.9076465125813,-17.1581123393608,
2.73215054063709));
#144645=CARTESIAN_POINT('Ctrl Pts',(16.9665749490587,-17.0981174144666,
2.73632010660236));
#144646=CARTESIAN_POINT('Ctrl Pts',(17.0284637509528,-17.0410281154315,
2.74048967256763));
#144647=CARTESIAN_POINT('Ctrl Pts',(17.0929880053965,-16.987138774985,2.74465923853289));
#144648=CARTESIAN_POINT('Ctrl Pts',(17.1597808523047,-16.9313547524115,
2.7489754012471));
#144649=CARTESIAN_POINT('Ctrl Pts',(17.2293975200618,-16.8790002342604,
2.75329156396131));
#144650=CARTESIAN_POINT('Ctrl Pts',(17.3014414464082,-16.8303553571508,
2.75760772667552));
#144651=CARTESIAN_POINT('Ctrl Pts',(17.3711385501861,-16.7832950812869,
2.76178329088851));
#144652=CARTESIAN_POINT('Ctrl Pts',(17.4431067778018,-16.7397066785438,
2.76595885510149));
#144653=CARTESIAN_POINT('Ctrl Pts',(17.5169602827153,-16.6997978939377,
2.77013441931447));
#144654=CARTESIAN_POINT('Ctrl Pts',(17.5945439513522,-16.6578734121651,
2.77452088127929));
#144655=CARTESIAN_POINT('Ctrl Pts',(17.6742078257199,-16.6200102829155,
2.77890734324412));
#144656=CARTESIAN_POINT('Ctrl Pts',(17.7554809190364,-16.5863921694013,
2.78329380520894));
#144657=CARTESIAN_POINT('Ctrl Pts',(17.8367540123529,-16.5527740558871,
2.78768026717377));
#144658=CARTESIAN_POINT('Ctrl Pts',(17.9196357523207,-16.523401080228,2.79206672913859));
#144659=CARTESIAN_POINT('Ctrl Pts',(18.0036392138267,-16.4983958913426,
2.79645319110342));
#144660=CARTESIAN_POINT('Ctrl Pts',(18.0837775523632,-16.4745412280212,
2.80063782549362));
#144661=CARTESIAN_POINT('Ctrl Pts',(18.1652349468392,-16.4545724558021,
2.80482245988383));
#144662=CARTESIAN_POINT('Ctrl Pts',(18.247599691841,-16.4386327884245,2.80900709427403));
#144663=CARTESIAN_POINT('Ctrl Pts',(18.3298472008232,-16.4227158091904,
2.81318577235514));
#144664=CARTESIAN_POINT('Ctrl Pts',(18.4129990472135,-16.4108166300769,
2.81736445043625));
#144665=CARTESIAN_POINT('Ctrl Pts',(18.4966284631471,-16.4030286871971,
2.82154312851736));
#144666=CARTESIAN_POINT('Ctrl Pts',(18.5817568763298,-16.3951011510316,
2.82579670640351));
#144667=CARTESIAN_POINT('Ctrl Pts',(18.6673796862237,-16.3914338261788,
2.83005028428965));
#144668=CARTESIAN_POINT('Ctrl Pts',(18.7530359237116,-16.3920707756642,
2.8343038621758));
#144669=CARTESIAN_POINT('Ctrl Pts',(18.8370315478211,-16.3926953766405,
2.83847497615095));
#144670=CARTESIAN_POINT('Ctrl Pts',(18.921058833767,-16.3974588441841,2.84264609012611));
#144671=CARTESIAN_POINT('Ctrl Pts',(19.0046798014456,-16.4063502901834,
2.84681720410127));
#144672=CARTESIAN_POINT('Ctrl Pts',(19.0882727093013,-16.4152387525721,
2.85098691841886));
#144673=CARTESIAN_POINT('Ctrl Pts',(19.1714591125976,-16.4282523938203,
2.85515663273646));
#144674=CARTESIAN_POINT('Ctrl Pts',(19.2538051248627,-16.4453283756809,
2.85932634705406));
#144675=CARTESIAN_POINT('Ctrl Pts',(19.3361482069038,-16.4624037499049,
2.86349591299535));
#144676=CARTESIAN_POINT('Ctrl Pts',(19.4176505070951,-16.4835410830843,
2.86766547893664));
#144677=CARTESIAN_POINT('Ctrl Pts',(19.4978886690212,-16.508626491643,2.87183504487793));
#144678=CARTESIAN_POINT('Ctrl Pts',(19.580947905855,-16.5345938722575,2.87615120762017));
#144679=CARTESIAN_POINT('Ctrl Pts',(19.66265195286,-16.5647919650882,2.88046737036242));
#144680=CARTESIAN_POINT('Ctrl Pts',(19.7425506078301,-16.5990389566664,
2.88478353310466));
#144681=CARTESIAN_POINT('Ctrl Pts',(19.8198465724095,-16.6321703560494,
2.88895909729368));
#144682=CARTESIAN_POINT('Ctrl Pts',(19.8954525574107,-16.6690906702005,
2.89313466148269));
#144683=CARTESIAN_POINT('Ctrl Pts',(19.9689850307411,-16.7095879116796,
2.89731022567171));
#144684=CARTESIAN_POINT('Ctrl Pts',(20.046231454653,-16.7521305726411,2.90169668769057));
#144685=CARTESIAN_POINT('Ctrl Pts',(20.1211888996699,-16.7986206906169,
2.90608314970943));
#144686=CARTESIAN_POINT('Ctrl Pts',(20.1934479978659,-16.8487616536576,
2.91046961172828));
#144687=CARTESIAN_POINT('Ctrl Pts',(20.2657070960619,-16.8989026166982,
2.91485607374714));
#144688=CARTESIAN_POINT('Ctrl Pts',(20.3352674349797,-16.9526940096932,
2.919242535766));
#144689=CARTESIAN_POINT('Ctrl Pts',(20.401762322946,-17.0097927931959,2.92362899778485));
#144690=CARTESIAN_POINT('Ctrl Pts',(20.4651976823984,-17.0642643769006,
2.92781363217406));
#144691=CARTESIAN_POINT('Ctrl Pts',(20.5260796023552,-17.1219484370562,
2.93199826656327));
#144692=CARTESIAN_POINT('Ctrl Pts',(20.5840648143939,-17.1825763134451,
2.93618290095248));
#144693=CARTESIAN_POINT('Ctrl Pts',(20.6419674916593,-17.243117893555,2.94036157903251));
#144694=CARTESIAN_POINT('Ctrl Pts',(20.6969813355446,-17.3065946373119,
2.94454025711253));
#144695=CARTESIAN_POINT('Ctrl Pts',(20.7487967797138,-17.3726982756753,
2.94871893519256));
#144696=CARTESIAN_POINT('Ctrl Pts',(20.8015409785421,-17.439986774327,2.95297251307897));
#144697=CARTESIAN_POINT('Ctrl Pts',(20.8509706214137,-17.5099969539569,
2.95722609096537));
#144698=CARTESIAN_POINT('Ctrl Pts',(20.8967991444563,-17.5823650629678,
2.96147966885178));
#144699=CARTESIAN_POINT('Ctrl Pts',(20.9417391920986,-17.6533301748853,
2.96565078282566));
#144700=CARTESIAN_POINT('Ctrl Pts',(20.9832162459024,-17.7265621993701,
2.96982189679953));
#144701=CARTESIAN_POINT('Ctrl Pts',(21.0210023907229,-17.801686970939,2.97399301077341));
#144702=CARTESIAN_POINT('Ctrl Pts',(21.0587758560372,-17.8767865336643,
2.97816272508966));
#144703=CARTESIAN_POINT('Ctrl Pts',(21.0928606655495,-17.953777171463,2.9823324394059));
#144704=CARTESIAN_POINT('Ctrl Pts',(21.1230748017627,-18.0322600413256,
2.98650215372215));
#144705=CARTESIAN_POINT('Ctrl Pts',(21.153287862827,-18.11074011843,2.99067171966202));
#144706=CARTESIAN_POINT('Ctrl Pts',(21.1796303599629,-18.190711892398,2.99484128560189));
#144707=CARTESIAN_POINT('Ctrl Pts',(21.2019688964371,-18.2717577444622,
2.99901085154177));
#144708=CARTESIAN_POINT('Ctrl Pts',(21.2250928283449,-18.3556530688812,
3.00332701428548));
#144709=CARTESIAN_POINT('Ctrl Pts',(21.2439258622492,-18.4406988974017,
3.00764317702919));
#144710=CARTESIAN_POINT('Ctrl Pts',(21.2583771885884,-18.5264182690313,
3.0119593397729));
#144711=CARTESIAN_POINT('Ctrl Pts',(21.2723577644625,-18.6093453409698,
3.01613490396033));
#144712=CARTESIAN_POINT('Ctrl Pts',(21.2822377087348,-18.6929022752308,
3.02031046814777));
#144713=CARTESIAN_POINT('Ctrl Pts',(21.2879876706469,-18.7766518372396,
3.02448603233521));
#144714=CARTESIAN_POINT('Ctrl Pts',(21.2940280494849,-18.8646313908058,
3.02887249435706));
#144715=CARTESIAN_POINT('Ctrl Pts',(21.295510260803,-18.9528229589747,3.0332589563789));
#144716=CARTESIAN_POINT('Ctrl Pts',(21.2924621252161,-19.0407217776804,
3.03764541840075));
#144717=CARTESIAN_POINT('Ctrl Pts',(21.2894139896292,-19.128620596386,3.0420318804226));
#144718=CARTESIAN_POINT('Ctrl Pts',(21.2818356329245,-19.2162260941259,
3.04641834244445));
#144719=CARTESIAN_POINT('Ctrl Pts',(21.2698170137414,-19.303044260485,3.05080480446629));
#144720=CARTESIAN_POINT('Ctrl Pts',(21.2583547009867,-19.3858438700274,
3.05498823010072));
#144721=CARTESIAN_POINT('Ctrl Pts',(21.2428114366919,-19.4682355295024,
3.05917165573515));
#144722=CARTESIAN_POINT('Ctrl Pts',(21.2232272746467,-19.549785559507,3.06335508136958));
#144723=CARTESIAN_POINT('Ctrl Pts',(21.2036685685069,-19.6312295890686,
3.06753306929945));
#144724=CARTESIAN_POINT('Ctrl Pts',(21.1800794975091,-19.711833717846,3.07171105722931));
#144725=CARTESIAN_POINT('Ctrl Pts',(21.1525516402421,-19.7911709977603,
3.07588904515917));
#144726=CARTESIAN_POINT('Ctrl Pts',(21.1250513038486,-19.8704289605227,
3.08006285616107));
#144727=CARTESIAN_POINT('Ctrl Pts',(21.0936201503625,-19.9484221572867,
3.08423666716296));
#144728=CARTESIAN_POINT('Ctrl Pts',(21.0584001058537,-20.024736756109,3.08841047816485));
#144729=CARTESIAN_POINT('Ctrl Pts',(21.0232047055544,-20.1009979559936,
3.09258136866297));
#144730=CARTESIAN_POINT('Ctrl Pts',(20.9842258731267,-20.175582474819,3.09675225916109));
#144731=CARTESIAN_POINT('Ctrl Pts',(20.941653896439,-20.2480957810045,3.10092314965921));
#144732=CARTESIAN_POINT('Ctrl Pts',(20.8990871157836,-20.3206002367323,
3.10509353108814));
#144733=CARTESIAN_POINT('Ctrl Pts',(20.8529282822877,-20.3910335782582,
3.10926391251707));
#144734=CARTESIAN_POINT('Ctrl Pts',(20.8034134872385,-20.4590261506807,
3.11343429394599));
#144735=CARTESIAN_POINT('Ctrl Pts',(20.7539049126767,-20.5270101812736,
3.11760415145464));
#144736=CARTESIAN_POINT('Ctrl Pts',(20.7010414902595,-20.5925536836385,
3.12177400896329));
#144737=CARTESIAN_POINT('Ctrl Pts',(20.6451014452025,-20.6553177231934,
3.12594386647194));
#144738=CARTESIAN_POINT('Ctrl Pts',(20.5891189590868,-20.718129381092,3.13011688760277));
#144739=CARTESIAN_POINT('Ctrl Pts',(20.5300554962292,-20.7781570214064,
3.13428990873359));
#144740=CARTESIAN_POINT('Ctrl Pts',(20.4682278066355,-20.8350968946638,
3.13846292986442));
#144741=CARTESIAN_POINT('Ctrl Pts',(20.4121814661711,-20.8867124659967,
3.14224574246181));
#144742=CARTESIAN_POINT('Ctrl Pts',(20.3538643415153,-20.9357910227048,
3.14602855505921));
#144743=CARTESIAN_POINT('Ctrl Pts',(20.2935357468249,-20.9821350335323,
3.1498113676566));
#144744=CARTESIAN_POINT('Ctrl Pts',(20.2935357468249,-20.9821350335323,
2.34989189284213));
#144745=CARTESIAN_POINT('Ctrl Pts',(20.2268473385658,-21.0333646093295,
2.354061433181));
#144746=CARTESIAN_POINT('Ctrl Pts',(20.1576293985627,-21.0813067494096,
2.35823097351988));
#144747=CARTESIAN_POINT('Ctrl Pts',(20.086244279078,-21.1257146569181,2.36240051385875));
#144748=CARTESIAN_POINT('Ctrl Pts',(20.0113055277115,-21.172333240224,2.36677761862545));
#144749=CARTESIAN_POINT('Ctrl Pts',(19.9339786873142,-21.2150562657093,
2.37115472339215));
#144750=CARTESIAN_POINT('Ctrl Pts',(19.8547138950657,-21.2536516603097,
2.37553182815884));
#144751=CARTESIAN_POINT('Ctrl Pts',(19.7791007054641,-21.2904690265942,
2.37970728668516));
#144752=CARTESIAN_POINT('Ctrl Pts',(19.7017246343737,-21.3235305286003,
2.38388274521148));
#144753=CARTESIAN_POINT('Ctrl Pts',(19.6229967617461,-21.3526842269663,
2.38805820373779));
#144754=CARTESIAN_POINT('Ctrl Pts',(19.5442131942302,-21.3818585496922,
2.39223661613151));
#144755=CARTESIAN_POINT('Ctrl Pts',(19.4640763602644,-21.4071194301684,
2.39641502852523));
#144756=CARTESIAN_POINT('Ctrl Pts',(19.3830113934786,-21.4283651207233,
2.40059344091895));
#144757=CARTESIAN_POINT('Ctrl Pts',(19.3018201752775,-21.4496438995358,
2.40477836081522));
#144758=CARTESIAN_POINT('Ctrl Pts',(19.2196983897446,-21.4668949224409,
2.4089632807115));
#144759=CARTESIAN_POINT('Ctrl Pts',(19.1370795562275,-21.4800678138356,
2.41314820060778));
#144760=CARTESIAN_POINT('Ctrl Pts',(19.1253819370915,-21.4819329027009,
2.41374072409156));
#144761=CARTESIAN_POINT('Ctrl Pts',(19.1136743577112,-21.4837163248914,
2.41433324757534));
#144762=CARTESIAN_POINT('Ctrl Pts',(19.1019580505853,-21.4854180217661,
2.41492577105912));
#144763=CARTESIAN_POINT('Ctrl Pts',(19.0192128717128,-21.4974360758147,
2.41911040544304));
#144764=CARTESIAN_POINT('Ctrl Pts',(18.93572429724,-21.5054183621376,2.42329503982696));
#144765=CARTESIAN_POINT('Ctrl Pts',(18.8519204122536,-21.5092826938714,
2.42747967421088));
#144766=CARTESIAN_POINT('Ctrl Pts',(18.7682358117201,-21.5131415252074,
2.43165835228593));
#144767=CARTESIAN_POINT('Ctrl Pts',(18.6842372477561,-21.5128940235269,
2.43583703036098));
#144768=CARTESIAN_POINT('Ctrl Pts',(18.6003605130579,-21.5085094342736,
2.44001570843604));
#144769=CARTESIAN_POINT('Ctrl Pts',(18.5149803479444,-21.5040462543972,
2.44426928632372));
#144770=CARTESIAN_POINT('Ctrl Pts',(18.4297268997688,-21.4952961442208,
2.44852286421141));
#144771=CARTESIAN_POINT('Ctrl Pts',(18.3450626650517,-21.4822821481968,
2.4527764420991));
#144772=CARTESIAN_POINT('Ctrl Pts',(18.2620398119422,-21.4695204539125,
2.45694755606877));
#144773=CARTESIAN_POINT('Ctrl Pts',(18.1795840056904,-21.4526587990534,
2.46111867003844));
#144774=CARTESIAN_POINT('Ctrl Pts',(18.0981270507739,-21.4317712782518,
2.46528978400811));
#144775=CARTESIAN_POINT('Ctrl Pts',(18.0166974295207,-21.4108907664583,
2.46945949832045));
#144776=CARTESIAN_POINT('Ctrl Pts',(17.9362664391865,-21.3859871858384,
2.47362921263278));
#144777=CARTESIAN_POINT('Ctrl Pts',(17.8572543229418,-21.3571854435281,
2.47779892694512));
#144778=CARTESIAN_POINT('Ctrl Pts',(17.7782450182821,-21.3283847261057,
2.48196849288139));
#144779=CARTESIAN_POINT('Ctrl Pts',(17.7006549192466,-21.2956862811423,
2.48613805881767));
#144780=CARTESIAN_POINT('Ctrl Pts',(17.6248864697077,-21.2592640024329,
2.49030762475394));
#144781=CARTESIAN_POINT('Ctrl Pts',(17.5464540946263,-21.2215611611785,
2.49462378750282));
#144782=CARTESIAN_POINT('Ctrl Pts',(17.4699743261966,-21.1798679825075,
2.49893995025171));
#144783=CARTESIAN_POINT('Ctrl Pts',(17.3958663510849,-21.1344294576552,
2.5032561130006));
#144784=CARTESIAN_POINT('Ctrl Pts',(17.3241724357537,-21.0904710881461,
2.50743167718525));
#144785=CARTESIAN_POINT('Ctrl Pts',(17.2546985266634,-21.0430079392875,
2.5116072413699));
#144786=CARTESIAN_POINT('Ctrl Pts',(17.1877934784105,-20.9923052204496,
2.51578280555455));
#144787=CARTESIAN_POINT('Ctrl Pts',(17.1175092148079,-20.9390416275037,
2.52016926758555));
#144788=CARTESIAN_POINT('Ctrl Pts',(17.0500605848376,-20.8822029788446,
2.52455572961655));
#144789=CARTESIAN_POINT('Ctrl Pts',(16.985809772922,-20.8221419544914,2.52894219164755));
#144790=CARTESIAN_POINT('Ctrl Pts',(16.9215589610063,-20.7620809301381,
2.53332865367855));
#144791=CARTESIAN_POINT('Ctrl Pts',(16.8605063152546,-20.6987980004711,
2.53771511570955));
#144792=CARTESIAN_POINT('Ctrl Pts',(16.802965079949,-20.6326856153201,2.54210157774055));
#144793=CARTESIAN_POINT('Ctrl Pts',(16.7485317522925,-20.5701440813406,
2.54625111891253));
#144794=CARTESIAN_POINT('Ctrl Pts',(16.6970294692199,-20.5048282635504,
2.5504006600845));
#144795=CARTESIAN_POINT('Ctrl Pts',(16.6487573722081,-20.4370465256145,
2.55455020125647));
#144796=CARTESIAN_POINT('Ctrl Pts',(16.6005493742832,-20.3693547930394,
2.55869423237572));
#144797=CARTESIAN_POINT('Ctrl Pts',(16.5555633203296,-20.2992040148308,
2.56283826349496));
#144798=CARTESIAN_POINT('Ctrl Pts',(16.514059720175,-20.2269373137572,2.5669822946142));
#144799=CARTESIAN_POINT('Ctrl Pts',(16.4725982721948,-20.154744008692,2.5711221169438));
#144800=CARTESIAN_POINT('Ctrl Pts',(16.4346124893252,-20.0804394498693,
2.57526193927339));
#144801=CARTESIAN_POINT('Ctrl Pts',(16.4003201033268,-20.0043963796323,
2.57940176160299));
#144802=CARTESIAN_POINT('Ctrl Pts',(16.3660518421397,-19.9284068059566,
2.58353867155335));
#144803=CARTESIAN_POINT('Ctrl Pts',(16.3354720095443,-19.8506815753093,
2.58767558150371));
#144804=CARTESIAN_POINT('Ctrl Pts',(16.3087521158423,-19.7716174109842,
2.59181249145407));
#144805=CARTESIAN_POINT('Ctrl Pts',(16.2820372325143,-19.6925680723558,
2.59594862567282));
#144806=CARTESIAN_POINT('Ctrl Pts',(16.2591810094483,-19.6121807387927,
2.60008475989157));
#144807=CARTESIAN_POINT('Ctrl Pts',(16.2403061251851,-19.5308703297896,
2.60422089411032));
#144808=CARTESIAN_POINT('Ctrl Pts',(16.2214331728165,-19.4495682431231,
2.60835660498473));
#144809=CARTESIAN_POINT('Ctrl Pts',(16.2065408484312,-19.3673437264668,
2.61249231585914));
#144810=CARTESIAN_POINT('Ctrl Pts',(16.1957010120584,-19.2846232821293,
2.61662802673355));
#144811=CARTESIAN_POINT('Ctrl Pts',(16.1848552750847,-19.2018578094073,
2.62076598885772));
#144812=CARTESIAN_POINT('Ctrl Pts',(16.1780664813587,-19.1185963356398,
2.62490395098188));
#144813=CARTESIAN_POINT('Ctrl Pts',(16.1753546619781,-19.0352708485527,
2.62904191310604));
#144814=CARTESIAN_POINT('Ctrl Pts',(16.1744266413966,-19.0067557610314,
2.63045797866119));
#144815=CARTESIAN_POINT('Ctrl Pts',(16.1739756253558,-18.9782331861948,
2.63187404421635));
#144816=CARTESIAN_POINT('Ctrl Pts',(16.1740010149441,-18.949720413872,2.6332901097715));
#144817=CARTESIAN_POINT('',(16.1740009418753,-18.9541959965583,2.56670989022851));
#144818=CARTESIAN_POINT('Ctrl Pts',(20.2935357468249,-20.9821350335323,
2.28327545627391));
#144819=CARTESIAN_POINT('Ctrl Pts',(20.262379265198,-21.006069228076,2.28523847760454));
#144820=CARTESIAN_POINT('Ctrl Pts',(20.2306962676017,-21.0292671335208,
2.28720149893518));
#144821=CARTESIAN_POINT('Ctrl Pts',(20.1985254700657,-21.0517059669222,
2.28916452026582));
#144822=CARTESIAN_POINT('Ctrl Pts',(20.1299459675163,-21.0995395349505,
2.29334915467529));
#144823=CARTESIAN_POINT('Ctrl Pts',(20.0588929044663,-21.1440987240594,
2.29753378908477));
#144824=CARTESIAN_POINT('Ctrl Pts',(19.9857121094434,-21.1851181775877,
2.30171842349424));
#144825=CARTESIAN_POINT('Ctrl Pts',(19.9126354781746,-21.226079245029,2.30589710159743));
#144826=CARTESIAN_POINT('Ctrl Pts',(19.8374375284691,-21.2635103616748,
2.31007577970061));
#144827=CARTESIAN_POINT('Ctrl Pts',(19.7604940332823,-21.2971886916911,
2.3142544578038));
#144828=CARTESIAN_POINT('Ctrl Pts',(19.6821713816853,-21.3314706813749,
2.31850803568478));
#144829=CARTESIAN_POINT('Ctrl Pts',(19.6020403867589,-21.3618637479467,
2.32276161356576));
#144830=CARTESIAN_POINT('Ctrl Pts',(19.5205248076212,-21.3881811769646,
2.32701519144673));
#144831=CARTESIAN_POINT('Ctrl Pts',(19.4405895664662,-21.413988391455,2.33118630545076));
#144832=CARTESIAN_POINT('Ctrl Pts',(19.3593234056757,-21.4358764386427,
2.33535741945479));
#144833=CARTESIAN_POINT('Ctrl Pts',(19.2771455317525,-21.4537179959654,
2.33952853345882));
#144834=CARTESIAN_POINT('Ctrl Pts',(19.194995233359,-21.4715535663921,2.34369824780777));
#144835=CARTESIAN_POINT('Ctrl Pts',(19.1119342786071,-21.485345246116,2.34786796215672));
#144836=CARTESIAN_POINT('Ctrl Pts',(19.0283943159569,-21.4950163166469,
2.35203767650567));
#144837=CARTESIAN_POINT('Ctrl Pts',(18.9448573259675,-21.5046870430453,
2.35620724248077));
#144838=CARTESIAN_POINT('Ctrl Pts',(18.8608418190481,-21.5102373997256,
2.36037680845588));
#144839=CARTESIAN_POINT('Ctrl Pts',(18.7767854909901,-21.5116424363103,
2.36454637443098));
#144840=CARTESIAN_POINT('Ctrl Pts',(18.6897738473697,-21.5130968722274,
2.36886253714067));
#144841=CARTESIAN_POINT('Ctrl Pts',(18.6027189860106,-21.5101090568378,
2.37317869985036));
#144842=CARTESIAN_POINT('Ctrl Pts',(18.5161054386262,-21.5027100893915,
2.37749486256005));
#144843=CARTESIAN_POINT('Ctrl Pts',(18.4323133171285,-21.4955521424197,
2.3816704267887));
#144844=CARTESIAN_POINT('Ctrl Pts',(18.3489346599974,-21.4842661264524,
2.38584599101735));
#144845=CARTESIAN_POINT('Ctrl Pts',(18.266400191337,-21.4689327402492,2.390021555246));
#144846=CARTESIAN_POINT('Ctrl Pts',(18.1796971048713,-21.452824901532,2.39440801719621));
#144847=CARTESIAN_POINT('Ctrl Pts',(18.0939262957253,-21.4322502184638,
2.39879447914641));
#144848=CARTESIAN_POINT('Ctrl Pts',(18.0095696123222,-21.4073616054278,
2.40318094109662));
#144849=CARTESIAN_POINT('Ctrl Pts',(17.9252129289191,-21.3824729923918,
2.40756740304683));
#144850=CARTESIAN_POINT('Ctrl Pts',(17.8422708932844,-21.3532707138249,
2.41195386499704));
#144851=CARTESIAN_POINT('Ctrl Pts',(17.7611994326681,-21.3199651720832,
2.41634032694725));
#144852=CARTESIAN_POINT('Ctrl Pts',(17.6838581936353,-21.288192069127,2.42052496109126));
#144853=CARTESIAN_POINT('Ctrl Pts',(17.6079312972239,-21.2525667345156,
2.42470959523527));
#144854=CARTESIAN_POINT('Ctrl Pts',(17.5338290567893,-21.2132363226944,
2.42889422937928));
#144855=CARTESIAN_POINT('Ctrl Pts',(17.4598322918057,-21.1739618928909,
2.4330729072098));
#144856=CARTESIAN_POINT('Ctrl Pts',(17.3876554268637,-21.1309930749775,
2.43725158504032));
#144857=CARTESIAN_POINT('Ctrl Pts',(17.3176892303927,-21.0845252176456,
2.44143026287085));
#144858=CARTESIAN_POINT('Ctrl Pts',(17.246468934763,-21.0372244537998,2.44568384081909));
#144859=CARTESIAN_POINT('Ctrl Pts',(17.1775397859107,-20.9862981588104,
2.44993741876734));
#144860=CARTESIAN_POINT('Ctrl Pts',(17.1112881539936,-20.9320015820273,
2.45419099671558));
#144861=CARTESIAN_POINT('Ctrl Pts',(17.046320944286,-20.8787576544711,2.4583621104312));
#144862=CARTESIAN_POINT('Ctrl Pts',(16.983928731977,-20.8222732634782,2.46253322414681));
#144863=CARTESIAN_POINT('Ctrl Pts',(16.9244454837175,-20.762831978015,2.46670433786243));
#144864=CARTESIAN_POINT('Ctrl Pts',(16.8649821956771,-20.7034106386898,
2.4708740519177));
#144865=CARTESIAN_POINT('Ctrl Pts',(16.8084262582069,-20.641034700359,2.47504376597298));
#144866=CARTESIAN_POINT('Ctrl Pts',(16.7550758225426,-20.5760255847352,
2.47921348002825));
#144867=CARTESIAN_POINT('Ctrl Pts',(16.7017272853469,-20.5110187824527,
2.48338304570478));
#144868=CARTESIAN_POINT('Ctrl Pts',(16.651584314341,-20.4433793453335,2.4875526113813));
#144869=CARTESIAN_POINT('Ctrl Pts',(16.6049048052798,-20.3734618010412,
2.49172217705783));
#144870=CARTESIAN_POINT('Ctrl Pts',(16.5565840957098,-20.3010860323251,
2.4960383401054));
#144871=CARTESIAN_POINT('Ctrl Pts',(16.5119752240842,-20.2262694173157,
2.50035450315297));
#144872=CARTESIAN_POINT('Ctrl Pts',(16.4713143087945,-20.1494362040685,
2.50467066620054));
#144873=CARTESIAN_POINT('Ctrl Pts',(16.4319779239082,-20.0751058347982,
2.50884623012138));
#144874=CARTESIAN_POINT('Ctrl Pts',(16.3963363916713,-19.9988886782757,
2.51302179404221));
#144875=CARTESIAN_POINT('Ctrl Pts',(16.3645549999889,-19.9211905859647,
2.51719735796305));
#144876=CARTESIAN_POINT('Ctrl Pts',(16.3311683990456,-19.8395681312915,
2.52158382057399));
#144877=CARTESIAN_POINT('Ctrl Pts',(16.3020423326888,-19.7563117555003,
2.52597028318493));
#144878=CARTESIAN_POINT('Ctrl Pts',(16.2773090396202,-19.6719093867897,
2.53035674579587));
#144879=CARTESIAN_POINT('Ctrl Pts',(16.2525757465516,-19.5875070180792,
2.53474320840681));
#144880=CARTESIAN_POINT('Ctrl Pts',(16.2322352869843,-19.5019592385255,
2.53912967101775));
#144881=CARTESIAN_POINT('Ctrl Pts',(16.2163575306375,-19.4157632978817,
2.54351613362869));
#144882=CARTESIAN_POINT('Ctrl Pts',(16.193544110504,-19.2919155599045,2.54981867488562));
#144883=CARTESIAN_POINT('Ctrl Pts',(16.1798641823048,-19.1663368454762,
2.55612121614255));
#144884=CARTESIAN_POINT('Ctrl Pts',(16.1755170133934,-19.040118143674,2.56242375739948));
#144885=CARTESIAN_POINT('Ctrl Pts',(16.1745315620426,-19.0115058691761,
2.56385246834249));
#144886=CARTESIAN_POINT('Ctrl Pts',(16.1740255308992,-18.9828608310217,
2.5652811792855));
#144887=CARTESIAN_POINT('Ctrl Pts',(16.1740009418753,-18.9541959965583,
2.56670989022851));
#144888=CARTESIAN_POINT('Ctrl Pts',(16.172685086933,-18.9541844540912,2.56671052146184));
#144889=CARTESIAN_POINT('Ctrl Pts',(16.1790130664392,-18.2584131946872,
2.60137099441126));
#144890=CARTESIAN_POINT('Ctrl Pts',(16.8320815170599,-16.7012241087188,
2.67842340292117));
#144891=CARTESIAN_POINT('Ctrl Pts',(19.4673983706617,-16.0150936874702,
2.79786774699155));
#144892=CARTESIAN_POINT('Ctrl Pts',(21.600448060805,-17.9789802882804,2.92504355367299));
#144893=CARTESIAN_POINT('Ctrl Pts',(21.2286613153073,-20.1169976411095,
3.0202290073439));
#144894=CARTESIAN_POINT('Ctrl Pts',(20.4604812917091,-20.8561430802638,
3.07302252545434));
#144895=CARTESIAN_POINT('Ctrl Pts',(20.293349366535,-20.9818838108338,3.08342410800431));
#144896=CARTESIAN_POINT('Origin',(18.734,-18.952,-1.76670989022851));
#144897=CARTESIAN_POINT('',(20.2935357468249,-20.9821350335323,3.94993168858525));
#144898=CARTESIAN_POINT('',(20.2935357468249,-20.9821350335323,3.88329345209041));
#144899=CARTESIAN_POINT('',(20.2935357468249,-20.9821350335323,-1.76670989022851));
#144900=CARTESIAN_POINT('',(16.1740000028035,-18.9521198080497,3.43329010980363));
#144901=CARTESIAN_POINT('Ctrl Pts',(16.1740000028035,-18.9521198080497,
3.43329010980363));
#144902=CARTESIAN_POINT('Ctrl Pts',(16.173996094898,-18.8686175883754,3.43746913841141));
#144903=CARTESIAN_POINT('Ctrl Pts',(16.1780820066338,-18.7849577973269,
3.4416481670192));
#144904=CARTESIAN_POINT('Ctrl Pts',(16.1862780259001,-18.7015748760835,
3.44582719562698));
#144905=CARTESIAN_POINT('Ctrl Pts',(16.1944623792895,-18.6183106386623,
3.45000027597724));
#144906=CARTESIAN_POINT('Ctrl Pts',(16.2067451760218,-18.5353229435673,
3.45417335632751));
#144907=CARTESIAN_POINT('Ctrl Pts',(16.2230946976723,-18.4530465324877,
3.45834643667777));
#144908=CARTESIAN_POINT('Ctrl Pts',(16.2396087147061,-18.369942324114,3.46256150311587));
#144909=CARTESIAN_POINT('Ctrl Pts',(16.2602717621694,-18.2875642714266,
3.46677656955396));
#144910=CARTESIAN_POINT('Ctrl Pts',(16.2849973159137,-18.2063554108437,
3.47099163599205));
#144911=CARTESIAN_POINT('Ctrl Pts',(16.3094325809408,-18.1260999774803,
3.47515721572334));
#144912=CARTESIAN_POINT('Ctrl Pts',(16.3378353258575,-18.0469868800097,
3.47932279545462));
#144913=CARTESIAN_POINT('Ctrl Pts',(16.3700710228284,-17.9694320426107,
3.4834883751859));
#144914=CARTESIAN_POINT('Ctrl Pts',(16.4022960455082,-17.8919028861488,
3.48765257555781));
#144915=CARTESIAN_POINT('Ctrl Pts',(16.4383513227395,-17.8159313907882,
3.49181677592972));
#144916=CARTESIAN_POINT('Ctrl Pts',(16.4780536821042,-17.7419147919373,
3.49598097630164));
#144917=CARTESIAN_POINT('Ctrl Pts',(16.5177548909312,-17.667900338019,3.50014505599887));
#144918=CARTESIAN_POINT('Ctrl Pts',(16.561102752779,-17.5958410741347,3.50430913569611));
#144919=CARTESIAN_POINT('Ctrl Pts',(16.6078681568274,-17.5261096166088,
3.50847321539335));
#144920=CARTESIAN_POINT('Ctrl Pts',(16.6556310871524,-17.4548907569615,
3.51272611670991));
#144921=CARTESIAN_POINT('Ctrl Pts',(16.7069587733462,-17.3861005826234,
3.51697901802647));
#144922=CARTESIAN_POINT('Ctrl Pts',(16.7615616490752,-17.320103265583,3.52123191934302));
#144923=CARTESIAN_POINT('Ctrl Pts',(16.815101261178,-17.255391092332,3.52540200532769));
#144924=CARTESIAN_POINT('Ctrl Pts',(16.8717892886061,-17.1933642853471,
3.52957209131236));
#144925=CARTESIAN_POINT('Ctrl Pts',(16.9313144499797,-17.134329840772,3.53374217729703));
#144926=CARTESIAN_POINT('Ctrl Pts',(16.9926128107595,-17.0735368147895,
3.53803648627953));
#144927=CARTESIAN_POINT('Ctrl Pts',(17.0569196193486,-17.0159176096088,
3.54233079526203));
#144928=CARTESIAN_POINT('Ctrl Pts',(17.1238587796064,-16.9617625140729,
3.54662510424453));
#144929=CARTESIAN_POINT('Ctrl Pts',(17.1907979398642,-16.9076074185369,
3.55091941322703));
#144930=CARTESIAN_POINT('Ctrl Pts',(17.2603689845986,-16.8569166856669,
3.55521372220953));
#144931=CARTESIAN_POINT('Ctrl Pts',(17.3321657913458,-16.809930708066,3.55950803119203));
#144932=CARTESIAN_POINT('Ctrl Pts',(17.4021289421208,-16.7641447297734,
3.56369266558497));
#144933=CARTESIAN_POINT('Ctrl Pts',(17.4744678068902,-16.7217048000894,
3.5678772999779));
#144934=CARTESIAN_POINT('Ctrl Pts',(17.5488288662328,-16.6828659396842,
3.57206193437084));
#144935=CARTESIAN_POINT('Ctrl Pts',(17.6230840818116,-16.6440823615896,
3.57624061245467));
#144936=CARTESIAN_POINT('Ctrl Pts',(17.6993553703909,-16.6088898827214,
3.5804192905385));
#144937=CARTESIAN_POINT('Ctrl Pts',(17.7772605377961,-16.5775001365631,
3.58459796862233));
#144938=CARTESIAN_POINT('Ctrl Pts',(17.8565620993404,-16.5455477517632,
3.58885154650779));
#144939=CARTESIAN_POINT('Ctrl Pts',(17.9375562869753,-16.5175360325719,
3.59310512439325));
#144940=CARTESIAN_POINT('Ctrl Pts',(18.0198140087904,-16.4936390887504,
3.59735870227872));
#144941=CARTESIAN_POINT('Ctrl Pts',(18.1004770041527,-16.4702054338167,
3.60152981625656));
#144942=CARTESIAN_POINT('Ctrl Pts',(18.1823545166279,-16.4507285663625,
3.60570093023439));
#144943=CARTESIAN_POINT('Ctrl Pts',(18.2650237601176,-16.4353233647475,
3.60987204421223));
#144944=CARTESIAN_POINT('Ctrl Pts',(18.3476652631442,-16.4199233324967,
3.61404175853249));
#144945=CARTESIAN_POINT('Ctrl Pts',(18.4310975176832,-16.408592336823,3.61821147285275));
#144946=CARTESIAN_POINT('Ctrl Pts',(18.5148867965883,-16.4013943064263,
3.622381187173));
#144947=CARTESIAN_POINT('Ctrl Pts',(18.5986730939112,-16.3941965321664,
3.62655075311693));
#144948=CARTESIAN_POINT('Ctrl Pts',(18.6828159319226,-16.3911314692988,
3.63072031906086));
#144949=CARTESIAN_POINT('Ctrl Pts',(18.766877068662,-16.3922111223079,3.63488988500479));
#144950=CARTESIAN_POINT('Ctrl Pts',(18.8538936912736,-16.3933287345849,
3.63920604774384));
#144951=CARTESIAN_POINT('Ctrl Pts',(18.9408222331035,-16.398887935209,3.6435222104829));
#144952=CARTESIAN_POINT('Ctrl Pts',(19.027179293109,-16.4088433193977,3.64783837322195));
#144953=CARTESIAN_POINT('Ctrl Pts',(19.110723280963,-16.418474407993,3.65201393741352));
#144954=CARTESIAN_POINT('Ctrl Pts',(19.1937319902678,-16.4322195436239,
3.65618950160508));
#144955=CARTESIAN_POINT('Ctrl Pts',(19.2757772698982,-16.4499853338116,
3.66036506579664));
#144956=CARTESIAN_POINT('Ctrl Pts',(19.3619664615662,-16.4686484318293,
3.66475152780944));
#144957=CARTESIAN_POINT('Ctrl Pts',(19.4470917766262,-16.4917488722623,
3.66913798982225));
#144958=CARTESIAN_POINT('Ctrl Pts',(19.5306760960807,-16.5191195676866,
3.67352445183505));
#144959=CARTESIAN_POINT('Ctrl Pts',(19.6142604155353,-16.5464902631109,
3.67791091384785));
#144960=CARTESIAN_POINT('Ctrl Pts',(19.6963032254015,-16.578130933778,3.68229737586066));
#144961=CARTESIAN_POINT('Ctrl Pts',(19.7763550154477,-16.6138177954293,
3.68668383787346));
#144962=CARTESIAN_POINT('Ctrl Pts',(19.8527235039631,-16.647862651673,3.69086847226646));
#144963=CARTESIAN_POINT('Ctrl Pts',(19.9275644240484,-16.6857162600702,
3.69505310665946));
#144964=CARTESIAN_POINT('Ctrl Pts',(20.0004719903204,-16.7272194045853,
3.69923774105246));
#144965=CARTESIAN_POINT('Ctrl Pts',(20.0732757816959,-16.7686634745112,
3.70341641913635));
#144966=CARTESIAN_POINT('Ctrl Pts',(20.1441512890029,-16.813746536681,3.70759509722024));
#144967=CARTESIAN_POINT('Ctrl Pts',(20.2127136875159,-16.8622617794678,
3.71177377530413));
#144968=CARTESIAN_POINT('Ctrl Pts',(20.2825050177484,-16.9116466231151,
3.71602735318958));
#144969=CARTESIAN_POINT('Ctrl Pts',(20.3498990582277,-16.964587704994,3.72028093107503));
#144970=CARTESIAN_POINT('Ctrl Pts',(20.4145171508852,-17.0208184690245,
3.72453450896048));
#144971=CARTESIAN_POINT('Ctrl Pts',(20.4778824957237,-17.0759590899682,
3.72870562293838));
#144972=CARTESIAN_POINT('Ctrl Pts',(20.5385782035453,-17.1342626616187,
3.73287673691628));
#144973=CARTESIAN_POINT('Ctrl Pts',(20.5962788337327,-17.1954358692518,
3.73704785089418));
#144974=CARTESIAN_POINT('Ctrl Pts',(20.6539601019164,-17.2565885496243,
3.7412175652145));
#144975=CARTESIAN_POINT('Ctrl Pts',(20.7086479730736,-17.3206086192034,
3.74538727953482));
#144976=CARTESIAN_POINT('Ctrl Pts',(20.7600539250065,-17.3871659854905,
3.74955699385514));
#144977=CARTESIAN_POINT('Ctrl Pts',(20.811458047695,-17.4537209833809,3.75372655979912));
#144978=CARTESIAN_POINT('Ctrl Pts',(20.8595802028305,-17.5228127338603,
3.75789612574311));
#144979=CARTESIAN_POINT('Ctrl Pts',(20.9041730844802,-17.5940792425927,
3.76206569168709));
#144980=CARTESIAN_POINT('Ctrl Pts',(20.9503337968388,-17.6678513938574,
3.76638185442608));
#144981=CARTESIAN_POINT('Ctrl Pts',(20.9927121598376,-17.7439536306547,
3.77069801716506));
#144982=CARTESIAN_POINT('Ctrl Pts',(21.0310846958974,-17.8219549124597,
3.77501417990405));
#144983=CARTESIAN_POINT('Ctrl Pts',(21.06820725063,-17.8974153107121,3.77918974409567));
#144984=CARTESIAN_POINT('Ctrl Pts',(21.1015808067413,-17.9746524800457,
3.78336530828729));
#144985=CARTESIAN_POINT('Ctrl Pts',(21.1310521424428,-18.0532558615431,
3.78754087247891));
#144986=CARTESIAN_POINT('Ctrl Pts',(21.1620120052503,-18.1358293129816,
3.79192733449158));
#144987=CARTESIAN_POINT('Ctrl Pts',(21.1886649090815,-18.2199100618434,
3.79631379650424));
#144988=CARTESIAN_POINT('Ctrl Pts',(21.2108930925539,-18.3050064853038,
3.80070025851691));
#144989=CARTESIAN_POINT('Ctrl Pts',(21.2331212760262,-18.3901029087642,
3.80508672052957));
#144990=CARTESIAN_POINT('Ctrl Pts',(21.2509246961549,-18.4762144232225,
3.80947318254223));
#144991=CARTESIAN_POINT('Ctrl Pts',(21.2642482087236,-18.5628419315355,
3.8138596445549));
#144992=CARTESIAN_POINT('Ctrl Pts',(21.2769586867287,-18.645483579777,3.818044278948));
#144993=CARTESIAN_POINT('Ctrl Pts',(21.285639763102,-18.7289023900137,3.82222891334111));
#144994=CARTESIAN_POINT('Ctrl Pts',(21.2902056694013,-18.8126709803349,
3.82641354773422));
#144995=CARTESIAN_POINT('Ctrl Pts',(21.2947650766981,-18.8963203364363,
3.83059222581822));
#144996=CARTESIAN_POINT('Ctrl Pts',(21.2952209238071,-18.9803180282762,
3.83477090390223));
#144997=CARTESIAN_POINT('Ctrl Pts',(21.2915388082527,-19.0642285359493,
3.83894958198623));
#144998=CARTESIAN_POINT('Ctrl Pts',(21.2877906934233,-19.1496430791655,
3.84320315987165));
#144999=CARTESIAN_POINT('Ctrl Pts',(21.2797547375529,-19.2349668053837,
3.84745673775707));
#145000=CARTESIAN_POINT('Ctrl Pts',(21.2674501116906,-19.319737041342,3.85171031564249));
#145001=CARTESIAN_POINT('Ctrl Pts',(21.2553840350109,-19.4028638408623,
3.85588142962051));
#145002=CARTESIAN_POINT('Ctrl Pts',(21.2392133934507,-19.4854579433579,
3.86005254359852));
#145003=CARTESIAN_POINT('Ctrl Pts',(21.2190086634415,-19.5670869390749,
3.86422365757654));
#145004=CARTESIAN_POINT('Ctrl Pts',(21.1988107133246,-19.648688543394,3.86839337189697));
#145005=CARTESIAN_POINT('Ctrl Pts',(21.1745814736228,-19.7293252379223,
3.87256308621741));
#145006=CARTESIAN_POINT('Ctrl Pts',(21.1464423282955,-19.8085757483422,
3.87673280053784));
#145007=CARTESIAN_POINT('Ctrl Pts',(21.1183041842799,-19.8878234386887,
3.88090236648194));
#145008=CARTESIAN_POINT('Ctrl Pts',(21.0862565659976,-19.9656846097689,
3.88507193242604));
#145009=CARTESIAN_POINT('Ctrl Pts',(21.0504699913875,-20.0417553757616,
3.88924149837014));
#145010=CARTESIAN_POINT('Ctrl Pts',(21.0134252049627,-20.1205006960409,
3.89355766110899));
#145011=CARTESIAN_POINT('Ctrl Pts',(20.9723738713789,-20.1973268901837,
3.89787382384784));
#145012=CARTESIAN_POINT('Ctrl Pts',(20.9275574633286,-20.2718127348512,
3.90218998658669));
#145013=CARTESIAN_POINT('Ctrl Pts',(20.8842009450553,-20.3438722109655,
3.90636555077843));
#145014=CARTESIAN_POINT('Ctrl Pts',(20.8373211816344,-20.413741105018,3.91054111497017));
#145015=CARTESIAN_POINT('Ctrl Pts',(20.7871804520949,-20.4810683539775,
3.91471667916191));
#145016=CARTESIAN_POINT('Ctrl Pts',(20.734507233507,-20.5517961422233,3.91910314117432));
#145017=CARTESIAN_POINT('Ctrl Pts',(20.6782353411158,-20.6197183310684,
3.92348960318672));
#145018=CARTESIAN_POINT('Ctrl Pts',(20.6187144099127,-20.6844697957158,
3.92787606519912));
#145019=CARTESIAN_POINT('Ctrl Pts',(20.5591934787095,-20.7492212603632,
3.93226252721153));
#145020=CARTESIAN_POINT('Ctrl Pts',(20.4964239761435,-20.8108016487773,
3.93664898922393));
#145021=CARTESIAN_POINT('Ctrl Pts',(20.4307957154099,-20.8688944415817,
3.94103545123633));
#145022=CARTESIAN_POINT('Ctrl Pts',(20.3864285555263,-20.9081673431888,
3.94400086368597));
#145023=CARTESIAN_POINT('Ctrl Pts',(20.3406387761084,-20.9459508109373,
3.94696627613561));
#145024=CARTESIAN_POINT('Ctrl Pts',(20.2935357468249,-20.9821350335323,
3.94993168858525));
#145025=CARTESIAN_POINT('Ctrl Pts',(20.2935357468249,-20.9821350335323,
3.1498113676566));
#145026=CARTESIAN_POINT('Ctrl Pts',(20.2269038271573,-21.0333212151827,
3.15398942064128));
#145027=CARTESIAN_POINT('Ctrl Pts',(20.1578180813607,-21.0811707044176,
3.15816747362595));
#145028=CARTESIAN_POINT('Ctrl Pts',(20.0866541319508,-21.1254596382994,
3.16234552661063));
#145029=CARTESIAN_POINT('Ctrl Pts',(20.0153772946765,-21.1698188280228,
3.16653020726961));
#145030=CARTESIAN_POINT('Ctrl Pts',(19.9420160778716,-21.2106059717294,
3.17071488792859));
#145031=CARTESIAN_POINT('Ctrl Pts',(19.8669695219043,-21.247643714176,3.17489956858757));
#145032=CARTESIAN_POINT('Ctrl Pts',(19.8485514193241,-21.2567336041907,
3.17592658277429));
#145033=CARTESIAN_POINT('Ctrl Pts',(19.8300318898626,-21.2655978908399,
3.176953596961));
#145034=CARTESIAN_POINT('Ctrl Pts',(19.8114169849418,-21.2742344068933,
3.17798061114772));
#145035=CARTESIAN_POINT('Ctrl Pts',(19.7355693750926,-21.3094244389056,
3.18216524554016));
#145036=CARTESIAN_POINT('Ctrl Pts',(19.6578547653244,-21.3409601078314,
3.1863498799326));
#145037=CARTESIAN_POINT('Ctrl Pts',(19.578659830513,-21.3686401823022,3.19053451432504));
#145038=CARTESIAN_POINT('Ctrl Pts',(19.4995776198891,-21.3962808576131,
3.19471319240837));
#145039=CARTESIAN_POINT('Ctrl Pts',(19.4190197000617,-21.4200766888,3.1988918704917));
#145040=CARTESIAN_POINT('Ctrl Pts',(19.337394846703,-21.4398735214983,3.20307054857503));
#145041=CARTESIAN_POINT('Ctrl Pts',(19.2543069264955,-21.4600251981986,
3.20732412646062));
#145042=CARTESIAN_POINT('Ctrl Pts',(19.1701138843276,-21.4760328992744,
3.21157770434621));
#145043=CARTESIAN_POINT('Ctrl Pts',(19.0852654759068,-21.4877863800873,
3.2158312822318));
#145044=CARTESIAN_POINT('Ctrl Pts',(19.0020620194665,-21.4993119967374,
3.22000239620914));
#145045=CARTESIAN_POINT('Ctrl Pts',(18.9182288577838,-21.5067468078097,
3.22417351018648));
#145046=CARTESIAN_POINT('Ctrl Pts',(18.8342009436325,-21.5100382661124,
3.22834462416382));
#145047=CARTESIAN_POINT('Ctrl Pts',(18.7502012258592,-21.5133286199344,
3.23251433848358));
#145048=CARTESIAN_POINT('Ctrl Pts',(18.6660073447033,-21.5124783642369,
3.23668405280334));
#145049=CARTESIAN_POINT('Ctrl Pts',(18.582057712998,-21.5074869480044,3.2408537671231));
#145050=CARTESIAN_POINT('Ctrl Pts',(18.4981110685809,-21.5024957093878,
3.24502333306653));
#145051=CARTESIAN_POINT('Ctrl Pts',(18.414409115505,-21.4933636313811,3.24919289900997));
#145052=CARTESIAN_POINT('Ctrl Pts',(18.3313872270487,-21.4801421943903,
3.2533624649534));
#145053=CARTESIAN_POINT('Ctrl Pts',(18.2454463913859,-21.4664559079809,
3.25767862769305));
#145054=CARTESIAN_POINT('Ctrl Pts',(18.1602348531239,-21.4483874314135,
3.2619947904327));
#145055=CARTESIAN_POINT('Ctrl Pts',(18.0762243702397,-21.4260515800794,
3.26631095317234));
#145056=CARTESIAN_POINT('Ctrl Pts',(17.9949505200244,-21.4044433167599,
3.27048651736342));
#145057=CARTESIAN_POINT('Ctrl Pts',(17.9148011124187,-21.378841616957,3.2746620815545));
#145058=CARTESIAN_POINT('Ctrl Pts',(17.8361862981299,-21.349400791844,3.27883764574558));
#145059=CARTESIAN_POINT('Ctrl Pts',(17.7536008364223,-21.3184729806292,
3.28322410775951));
#145060=CARTESIAN_POINT('Ctrl Pts',(17.6727096022459,-21.2833082561226,
3.28761056977344));
#145061=CARTESIAN_POINT('Ctrl Pts',(17.5939605452813,-21.2441409297172,
3.29199703178737));
#145062=CARTESIAN_POINT('Ctrl Pts',(17.5152114883168,-21.2049736033118,
3.2963834938013));
#145063=CARTESIAN_POINT('Ctrl Pts',(17.4386050767024,-21.161804026126,3.30076995581523));
#145064=CARTESIAN_POINT('Ctrl Pts',(17.364553744478,-21.1149186191895,3.30515641782916));
#145065=CARTESIAN_POINT('Ctrl Pts',(17.2939096238495,-21.070190479346,3.30934105222176));
#145066=CARTESIAN_POINT('Ctrl Pts',(17.2253276726157,-21.0219144506012,
3.31352568661436));
#145067=CARTESIAN_POINT('Ctrl Pts',(17.1591863942882,-20.97030674261,3.31771032100696));
#145068=CARTESIAN_POINT('Ctrl Pts',(17.093139259884,-20.9187724918035,3.32188899909045));
#145069=CARTESIAN_POINT('Ctrl Pts',(17.0295262575255,-20.8639162618917,
3.32606767717394));
#145070=CARTESIAN_POINT('Ctrl Pts',(16.9686982691563,-20.8059983276908,
3.33024635525743));
#145071=CARTESIAN_POINT('Ctrl Pts',(16.9067799828036,-20.7470422561362,
3.33449993314298));
#145072=CARTESIAN_POINT('Ctrl Pts',(16.8477479425957,-20.6849138964936,
3.33875351102853));
#145073=CARTESIAN_POINT('Ctrl Pts',(16.7919382910611,-20.6199317488055,
3.34300708891408));
#145074=CARTESIAN_POINT('Ctrl Pts',(16.7372106185328,-20.5562094068615,
3.34717820289155));
#145075=CARTESIAN_POINT('Ctrl Pts',(16.6855818186072,-20.4897433069906,
3.35134931686903));
#145076=CARTESIAN_POINT('Ctrl Pts',(16.6373315068437,-20.420870732844,3.35552043084651));
#145077=CARTESIAN_POINT('Ctrl Pts',(16.5890973859384,-20.352021269555,3.3596901451664));
#145078=CARTESIAN_POINT('Ctrl Pts',(16.544239765417,-20.2807673121879,3.36385985948629));
#145079=CARTESIAN_POINT('Ctrl Pts',(16.5029964131481,-20.207477198301,3.36802957380618));
#145080=CARTESIAN_POINT('Ctrl Pts',(16.4617545284946,-20.1341896923911,
3.37219913974973));
#145081=CARTESIAN_POINT('Ctrl Pts',(16.4241268812486,-20.0588665753509,
3.37636870569329));
#145082=CARTESIAN_POINT('Ctrl Pts',(16.3903058438335,-19.9819017925758,
3.38053827163684));
#145083=CARTESIAN_POINT('Ctrl Pts',(16.3552957004569,-19.9022310229649,
3.38485443437632));
#145084=CARTESIAN_POINT('Ctrl Pts',(16.3243650403573,-19.8208014806367,
3.3891705971158));
#145085=CARTESIAN_POINT('Ctrl Pts',(16.2976726756056,-19.7380719867858,
3.39348675985528));
#145086=CARTESIAN_POINT('Ctrl Pts',(16.2718498118347,-19.6580373975154,
3.39766232404646));
#145087=CARTESIAN_POINT('Ctrl Pts',(16.2499934356292,-19.5767867151056,
3.40183788823764));
#145088=CARTESIAN_POINT('Ctrl Pts',(16.2321958025117,-19.4947483371048,
3.40601345242882));
#145089=CARTESIAN_POINT('Ctrl Pts',(16.2134992532485,-19.4085663956273,
3.41039991444245));
#145090=CARTESIAN_POINT('Ctrl Pts',(16.1992823307861,-19.3215156705806,
3.41478637645608));
#145091=CARTESIAN_POINT('Ctrl Pts',(16.1895904829899,-19.2340996450696,
3.41917283846971));
#145092=CARTESIAN_POINT('Ctrl Pts',(16.1798986351937,-19.1466836195585,
3.42355930048334));
#145093=CARTESIAN_POINT('Ctrl Pts',(16.174731820223,-19.0589028772671,3.42794576249697));
#145094=CARTESIAN_POINT('Ctrl Pts',(16.1740724460423,-18.9712592442245,
3.43233222451059));
#145095=CARTESIAN_POINT('Ctrl Pts',(16.1740244495167,-18.9648795739235,
3.43265151959756));
#145096=CARTESIAN_POINT('Ctrl Pts',(16.1740003013853,-18.958499723977,3.43297081468453));
#145097=CARTESIAN_POINT('Ctrl Pts',(16.1740000028035,-18.9521198086917,
3.4332901097715));
#145098=CARTESIAN_POINT('',(16.1743944592445,-18.9523823947444,3.36670986511428));
#145099=CARTESIAN_POINT('Ctrl Pts',(20.293349366535,-20.9818838108338,3.08342410800431));
#145100=CARTESIAN_POINT('Ctrl Pts',(19.779330537192,-21.3686028835722,3.11541446101482));
#145101=CARTESIAN_POINT('Ctrl Pts',(18.2370602754448,-21.8303674869899,
3.18979674958582));
#145102=CARTESIAN_POINT('Ctrl Pts',(16.4590845454477,-20.6164716802603,
3.28422525531007));
#145103=CARTESIAN_POINT('Ctrl Pts',(16.1776267599649,-19.3569817996596,
3.34666340802382));
#145104=CARTESIAN_POINT('Ctrl Pts',(16.1781627867106,-18.9523866751972,
3.36670962517707));
#145105=CARTESIAN_POINT('Ctrl Pts',(16.1740000284928,-18.9523819467095,
3.3667098902285));
#145106=CARTESIAN_POINT('Ctrl Pts',(16.1739869935966,-18.8650154810558,
3.37103154303558));
#145107=CARTESIAN_POINT('Ctrl Pts',(16.1784506871914,-18.7777135371325,
3.37535319584266));
#145108=CARTESIAN_POINT('Ctrl Pts',(16.1873453738309,-18.6909440385447,
3.37967484864975));
#145109=CARTESIAN_POINT('Ctrl Pts',(16.1966194662204,-18.6004733587883,
3.38418084296216));
#145110=CARTESIAN_POINT('Ctrl Pts',(16.2107109130556,-18.5105820575904,
3.38868683727458));
#145111=CARTESIAN_POINT('Ctrl Pts',(16.2295088315793,-18.4217887333309,
3.39319283158699));
#145112=CARTESIAN_POINT('Ctrl Pts',(16.2475982064586,-18.3363422660913,
3.39752898296558));
#145113=CARTESIAN_POINT('Ctrl Pts',(16.2700454505065,-18.2519128648082,
3.40186513434417));
#145114=CARTESIAN_POINT('Ctrl Pts',(16.296700996459,-18.1689459997304,3.40620128572276));
#145115=CARTESIAN_POINT('Ctrl Pts',(16.3233900671469,-18.0858747870546,
3.41054289068792));
#145116=CARTESIAN_POINT('Ctrl Pts',(16.3542978445813,-18.0042701592832,
3.41488449565309));
#145117=CARTESIAN_POINT('Ctrl Pts',(16.3892268388776,-17.9245571437398,
3.41922610061825));
#145118=CARTESIAN_POINT('Ctrl Pts',(16.4242296046626,-17.8446757709924,
3.42357687523365));
#145119=CARTESIAN_POINT('Ctrl Pts',(16.4632703651625,-17.7666943545301,
3.42792764984905));
#145120=CARTESIAN_POINT('Ctrl Pts',(16.5061059491331,-17.6910130460184,
3.43227842446446));
#145121=CARTESIAN_POINT('Ctrl Pts',(16.5109248522389,-17.6824990756499,
3.43276787644255));
#145122=CARTESIAN_POINT('Ctrl Pts',(16.515791737601,-17.6740141830169,3.43325732842064));
#145123=CARTESIAN_POINT('Ctrl Pts',(16.5207062260025,-17.6655589131312,
3.43374678039873));
#145124=CARTESIAN_POINT('Ctrl Pts',(16.5627232942887,-17.5932694654538,
3.43793141479117));
#145125=CARTESIAN_POINT('Ctrl Pts',(16.608363899273,-17.5229061642045,3.44211604918361));
#145126=CARTESIAN_POINT('Ctrl Pts',(16.6574263400684,-17.4548554395523,
3.44630068357605));
#145127=CARTESIAN_POINT('Ctrl Pts',(16.7064189465521,-17.3869015766835,
3.4504793616594));
#145128=CARTESIAN_POINT('Ctrl Pts',(16.7588234476463,-17.3212541220954,
3.45465803974274));
#145129=CARTESIAN_POINT('Ctrl Pts',(16.8143930615577,-17.2582735752536,
3.45883671782609));
#145130=CARTESIAN_POINT('Ctrl Pts',(16.8709587208714,-17.1941641473616,
3.46309029571167));
#145131=CARTESIAN_POINT('Ctrl Pts',(16.930803836094,-17.1328185931037,3.46734387359726));
#145132=CARTESIAN_POINT('Ctrl Pts',(16.9936228831504,-17.0745848910946,
3.47159745148285));
#145133=CARTESIAN_POINT('Ctrl Pts',(17.0552240603871,-17.0174801630432,
3.47576856546019));
#145134=CARTESIAN_POINT('Ctrl Pts',(17.1196845346186,-16.9633680324694,
3.47993967943753));
#145135=CARTESIAN_POINT('Ctrl Pts',(17.1866778681086,-16.912540703971,3.48411079341487));
#145136=CARTESIAN_POINT('Ctrl Pts',(17.2536487213386,-16.8617304310735,
3.48828050773463));
#145137=CARTESIAN_POINT('Ctrl Pts',(17.3231503796754,-16.8142030489943,
3.49245022205439));
#145138=CARTESIAN_POINT('Ctrl Pts',(17.3948237869026,-16.7702101223367,
3.49661993637416));
#145139=CARTESIAN_POINT('Ctrl Pts',(17.4664946436824,-16.7262187611362,
3.50078950231759));
#145140=CARTESIAN_POINT('Ctrl Pts',(17.5403367031857,-16.6857618452163,
3.50495906826103));
#145141=CARTESIAN_POINT('Ctrl Pts',(17.6159635983346,-16.6490465474632,
3.50912863420446));
#145142=CARTESIAN_POINT('Ctrl Pts',(17.6942494418455,-16.6110403851225,
3.5134447969441));
#145143=CARTESIAN_POINT('Ctrl Pts',(17.7744474914057,-16.5770440773059,
3.51776095968374));
#145144=CARTESIAN_POINT('Ctrl Pts',(17.8561052781559,-16.5472337208456,
3.52207712242339));
#145145=CARTESIAN_POINT('Ctrl Pts',(17.9351030710671,-16.5183944336203,
3.52625268661447));
#145146=CARTESIAN_POINT('Ctrl Pts',(18.0154664958606,-16.4934726654686,
3.53042825080555));
#145147=CARTESIAN_POINT('Ctrl Pts',(18.0967709615458,-16.472576850848,3.53460381499663));
#145148=CARTESIAN_POINT('Ctrl Pts',(18.1821819225488,-16.450625638296,3.53899027701055));
#145149=CARTESIAN_POINT('Ctrl Pts',(18.2686309144569,-16.4331178853207,
3.54337673902447));
#145150=CARTESIAN_POINT('Ctrl Pts',(18.3556165397332,-16.4201180997139,
3.54776320103839));
#145151=CARTESIAN_POINT('Ctrl Pts',(18.4426021650095,-16.407118314107,3.55214966305232));
#145152=CARTESIAN_POINT('Ctrl Pts',(18.530123838803,-16.3986264761921,3.55653612506624));
#145153=CARTESIAN_POINT('Ctrl Pts',(18.6176794289204,-16.3946440363642,
3.56092258708016));
#145154=CARTESIAN_POINT('Ctrl Pts',(18.7012064565128,-16.3908448344978,
3.56510722147276));
#145155=CARTESIAN_POINT('Ctrl Pts',(18.7850752514674,-16.391135040087,3.56929185586537));
#145156=CARTESIAN_POINT('Ctrl Pts',(18.8688517103014,-16.3955542219267,
3.57347649025797));
#145157=CARTESIAN_POINT('Ctrl Pts',(18.9525089237155,-16.3999671136081,
3.57765516834146));
#145158=CARTESIAN_POINT('Ctrl Pts',(19.0360736066035,-16.4084972837709,
3.58183384642495));
#145159=CARTESIAN_POINT('Ctrl Pts',(19.1191090576612,-16.4211323595045,
3.58601252450843));
#145160=CARTESIAN_POINT('Ctrl Pts',(19.2036328595139,-16.4339939098916,
3.59026610239398));
#145161=CARTESIAN_POINT('Ctrl Pts',(19.2876077883166,-16.4511089960901,
3.59451968027953));
#145162=CARTESIAN_POINT('Ctrl Pts',(19.370575874736,-16.4724090749271,3.59877325816508));
#145163=CARTESIAN_POINT('Ctrl Pts',(19.4519354628899,-16.4932962101692,
3.60294437214256));
#145164=CARTESIAN_POINT('Ctrl Pts',(19.5323264333864,-16.5182073979463,
3.60711548612004));
#145165=CARTESIAN_POINT('Ctrl Pts',(19.6113263938458,-16.5470263205886,
3.61128660009752));
#145166=CARTESIAN_POINT('Ctrl Pts',(19.6902998451053,-16.575835572763,3.61545631441741));
#145167=CARTESIAN_POINT('Ctrl Pts',(19.7678827815192,-16.6085497980588,
3.6196260287373));
#145168=CARTESIAN_POINT('Ctrl Pts',(19.8436693267471,-16.6450032541686,
3.62379574305719));
#145169=CARTESIAN_POINT('Ctrl Pts',(19.9194531751644,-16.6814554131079,
3.62796530900075));
#145170=CARTESIAN_POINT('Ctrl Pts',(19.993440345293,-16.7216463381321,3.6321348749443));
#145171=CARTESIAN_POINT('Ctrl Pts',(20.06524750435,-16.7653632944264,3.63630444088786));
#145172=CARTESIAN_POINT('Ctrl Pts',(20.139579314554,-16.8106172849844,3.64062060362734));
#145173=CARTESIAN_POINT('Ctrl Pts',(20.2115745125432,-16.8596495964176,
3.64493676636682));
#145174=CARTESIAN_POINT('Ctrl Pts',(20.2808401159382,-16.9121750918953,
3.6492529291063));
#145175=CARTESIAN_POINT('Ctrl Pts',(20.3478493995713,-16.9629895748699,
3.65342849329748));
#145176=CARTESIAN_POINT('Ctrl Pts',(20.4123038602611,-17.0170728169147,
3.65760405748865));
#145177=CARTESIAN_POINT('Ctrl Pts',(20.4738824987383,-17.074126497715,3.66177962167983));
#145178=CARTESIAN_POINT('Ctrl Pts',(20.5385713278796,-17.1340618243223,
3.66616608369346));
#145179=CARTESIAN_POINT('Ctrl Pts',(20.6000857771511,-17.1972751310407,
3.67055254570709));
#145180=CARTESIAN_POINT('Ctrl Pts',(20.6581002087316,-17.2633797387337,
3.67493900772071));
#145181=CARTESIAN_POINT('Ctrl Pts',(20.716114640312,-17.3294843464266,3.67932546973434));
#145182=CARTESIAN_POINT('Ctrl Pts',(20.7706287541777,-17.3984797526766,
3.68371193174797));
#145183=CARTESIAN_POINT('Ctrl Pts',(20.8213695361432,-17.4699445288447,
3.6880983937616));
#145184=CARTESIAN_POINT('Ctrl Pts',(20.8697756595073,-17.5381211047148,
3.69228302815506));
#145185=CARTESIAN_POINT('Ctrl Pts',(20.914928230553,-17.6087985715452,3.69646766254852));
#145186=CARTESIAN_POINT('Ctrl Pts',(20.956559006204,-17.6816333348432,3.70065229694198));
#145187=CARTESIAN_POINT('Ctrl Pts',(20.9981305255987,-17.7543644268708,
3.70483097502633));
#145188=CARTESIAN_POINT('Ctrl Pts',(21.0361899803433,-17.8292463201213,
3.70900965311069));
#145189=CARTESIAN_POINT('Ctrl Pts',(21.0705113959643,-17.905905120685,3.71318833119505));
#145190=CARTESIAN_POINT('Ctrl Pts',(21.1054479982896,-17.9839379751455,
3.71744190908038));
#145191=CARTESIAN_POINT('Ctrl Pts',(21.1365109555626,-18.0638116724909,
3.72169548696571));
#145192=CARTESIAN_POINT('Ctrl Pts',(21.1635100116305,-18.1451040318682,
3.72594906485105));
#145193=CARTESIAN_POINT('Ctrl Pts',(21.1899856383155,-18.22482038024,3.73012017882942));
#145194=CARTESIAN_POINT('Ctrl Pts',(21.2125533792703,-18.3059004177639,
3.7342912928078));
#145195=CARTESIAN_POINT('Ctrl Pts',(21.2310824062636,-18.3879260187451,
3.73846240678618));
#145196=CARTESIAN_POINT('Ctrl Pts',(21.249605215663,-18.4699240952438,3.74263212110699));
#145197=CARTESIAN_POINT('Ctrl Pts',(21.2640919013283,-18.5528666566977,
3.74680183542779));
#145198=CARTESIAN_POINT('Ctrl Pts',(21.2744621331457,-18.6363227121685,
3.75097154974859));
#145199=CARTESIAN_POINT('Ctrl Pts',(21.2848319959458,-18.7197757979147,
3.75514111569307));
#145200=CARTESIAN_POINT('Ctrl Pts',(21.2910856402585,-18.8037418847205,
3.75931068163754));
#145201=CARTESIAN_POINT('Ctrl Pts',(21.293194451632,-18.887783501059,3.76348024758202));
#145202=CARTESIAN_POINT('Ctrl Pts',(21.2953774062114,-18.9747799169322,
3.76779641032044));
#145203=CARTESIAN_POINT('Ctrl Pts',(21.293118626995,-19.0618567451373,3.77211257305885));
#145204=CARTESIAN_POINT('Ctrl Pts',(21.2864451550249,-19.148529210526,3.77642873579727));
#145205=CARTESIAN_POINT('Ctrl Pts',(21.2799890707009,-19.2323783294898,
3.7806042999894));
#145206=CARTESIAN_POINT('Ctrl Pts',(21.2694016000863,-19.315848563955,3.78477986418152));
#145207=CARTESIAN_POINT('Ctrl Pts',(21.2547598325396,-19.3985085292071,
3.78895542837364));
#145208=CARTESIAN_POINT('Ctrl Pts',(21.2393785441267,-19.4853434527702,
3.79334189038521));
#145209=CARTESIAN_POINT('Ctrl Pts',(21.21952276158,-19.5712835336821,3.79772835239677));
#145210=CARTESIAN_POINT('Ctrl Pts',(21.1953413592831,-19.6558456599869,
3.80211481440834));
#145211=CARTESIAN_POINT('Ctrl Pts',(21.1711599569862,-19.7404077862916,
3.8065012764199));
#145212=CARTESIAN_POINT('Ctrl Pts',(21.1426531949957,-19.8235914337676,
3.81088773843147));
#145213=CARTESIAN_POINT('Ctrl Pts',(21.1100276507034,-19.9049389293616,
3.81527420044303));
#145214=CARTESIAN_POINT('Ctrl Pts',(21.0789046619559,-19.982540000698,3.81945864581518));
#145215=CARTESIAN_POINT('Ctrl Pts',(21.0439180829632,-20.0587591592275,
3.82364309118733));
#145216=CARTESIAN_POINT('Ctrl Pts',(21.0052116068261,-20.1331849292209,
3.82782753655948));
#145217=CARTESIAN_POINT('Ctrl Pts',(20.966557925707,-20.2075091836474,3.83200627441467));
#145218=CARTESIAN_POINT('Ctrl Pts',(20.9241946333094,-20.2800445023936,
3.83618501226986));
#145219=CARTESIAN_POINT('Ctrl Pts',(20.8783138059628,-20.3503984773867,
3.84036375012505));
#145220=CARTESIAN_POINT('Ctrl Pts',(20.8324875829267,-20.4206687217558,
3.84453751472425));
#145221=CARTESIAN_POINT('Ctrl Pts',(20.7831523972177,-20.4887624000407,
3.84871127932344));
#145222=CARTESIAN_POINT('Ctrl Pts',(20.7305459075014,-20.5543122165294,
3.85288504392264));
#145223=CARTESIAN_POINT('Ctrl Pts',(20.6779756656207,-20.6198168667471,
3.85705593264219));
#145224=CARTESIAN_POINT('Ctrl Pts',(20.622138884113,-20.6827807791786,3.86122682136175));
#145225=CARTESIAN_POINT('Ctrl Pts',(20.5633154981063,-20.7428670549173,
3.8653977100813));
#145226=CARTESIAN_POINT('Ctrl Pts',(20.5045103316162,-20.8029347199814,
3.86956730694091));
#145227=CARTESIAN_POINT('Ctrl Pts',(20.4427207177839,-20.8601261886896,
3.87373690380052));
#145228=CARTESIAN_POINT('Ctrl Pts',(20.3782648488349,-20.914139930506,3.87790650066013));
#145229=CARTESIAN_POINT('Ctrl Pts',(20.3505067188033,-20.9374011244559,
3.87970215113689));
#145230=CARTESIAN_POINT('Ctrl Pts',(20.3222545566491,-20.960073441674,3.88149780161365));
#145231=CARTESIAN_POINT('Ctrl Pts',(20.2935357468249,-20.9821350335323,
3.88329345209042));
#145232=CARTESIAN_POINT('Origin',(18.734,-18.952,-1.76670989022851));
#145233=CARTESIAN_POINT('',(20.2917778074115,-20.9798105030549,4.74997346711436));
#145234=CARTESIAN_POINT('',(20.2944552458115,-20.9833106134465,4.68319930664559));
#145235=CARTESIAN_POINT('',(20.2935357468249,-20.9821350335323,-1.76670989022851));
#145236=CARTESIAN_POINT('',(16.1740009581142,-18.9542148462772,4.23329008724971));
#145237=CARTESIAN_POINT('Ctrl Pts',(16.1756127776244,-18.9542129983521,
4.2332901097715));
#145238=CARTESIAN_POINT('Ctrl Pts',(16.1805387770827,-18.3551144017957,
4.26304769694121));
#145239=CARTESIAN_POINT('Ctrl Pts',(16.6895187238437,-16.8950156783259,
4.3351972196714));
#145240=CARTESIAN_POINT('Ctrl Pts',(19.1239734419868,-15.950132033759,4.44973867796206));
#145241=CARTESIAN_POINT('Ctrl Pts',(21.4691811314196,-17.6550517548787,
4.5769144846435));
#145242=CARTESIAN_POINT('Ctrl Pts',(21.3400058517746,-19.9330438229453,
4.67699274769427));
#145243=CARTESIAN_POINT('Ctrl Pts',(20.5375803711221,-20.7936897955478,
4.73467907518456));
#145244=CARTESIAN_POINT('Ctrl Pts',(20.2917778074114,-20.979810503055,4.74997346711437));
#145245=CARTESIAN_POINT('Ctrl Pts',(20.2935357468249,-20.9821350335323,
3.94993168858525));
#145246=CARTESIAN_POINT('Ctrl Pts',(20.2271357439777,-21.033143058279,3.95411195890108));
#145247=CARTESIAN_POINT('Ctrl Pts',(20.1581247303567,-21.080971361085,3.95829222921691));
#145248=CARTESIAN_POINT('Ctrl Pts',(20.0868406859495,-21.1253435251795,
3.96247249953274));
#145249=CARTESIAN_POINT('Ctrl Pts',(20.0156413709827,-21.1696629477571,
3.96664780110743));
#145250=CARTESIAN_POINT('Ctrl Pts',(19.9421747810589,-21.210534151495,3.97082310268211));
#145251=CARTESIAN_POINT('Ctrl Pts',(19.8668100196579,-21.2477224264625,
3.9749984042568));
#145252=CARTESIAN_POINT('Ctrl Pts',(19.7915083980674,-21.2848795454813,
3.97917020780741));
#145253=CARTESIAN_POINT('Ctrl Pts',(19.7143121762206,-21.3183596641629,
3.98334201135802));
#145254=CARTESIAN_POINT('Ctrl Pts',(19.6356162179364,-21.3479733294747,
3.98751381490862));
#145255=CARTESIAN_POINT('Ctrl Pts',(19.5569539985136,-21.3775742986917,
3.99168382990611));
#145256=CARTESIAN_POINT('Ctrl Pts',(19.4767937494083,-21.4033119443507,
3.9958538449036));
#145257=CARTESIAN_POINT('Ctrl Pts',(19.395550402454,-21.4250448974924,4.00002385990109));
#145258=CARTESIAN_POINT('Ctrl Pts',(19.3143175153553,-21.4467750525765,
4.0041933380207));
#145259=CARTESIAN_POINT('Ctrl Pts',(19.232002251929,-21.4645014211188,4.00836281614032));
#145260=CARTESIAN_POINT('Ctrl Pts',(19.1490334747512,-21.4781328577167,
4.01253229425994));
#145261=CARTESIAN_POINT('Ctrl Pts',(19.0660504912852,-21.4917666283507,
4.01670248629641));
#145262=CARTESIAN_POINT('Ctrl Pts',(18.9824142259904,-21.5013040015176,
4.02087267833288));
#145263=CARTESIAN_POINT('Ctrl Pts',(18.8985611115136,-21.5067053921299,
4.02504287036935));
#145264=CARTESIAN_POINT('Ctrl Pts',(18.814615568438,-21.5121127365218,4.02921765907475));
#145265=CARTESIAN_POINT('Ctrl Pts',(18.7304531589254,-21.5133749701138,
4.03339244778016));
#145266=CARTESIAN_POINT('Ctrl Pts',(18.6465122350704,-21.5105046200833,
4.03756723648557));
#145267=CARTESIAN_POINT('Ctrl Pts',(18.5625187387461,-21.5076324723434,
4.04174463987451));
#145268=CARTESIAN_POINT('Ctrl Pts',(18.4787474622756,-21.5006226277578,
4.04592204326345));
#145269=CARTESIAN_POINT('Ctrl Pts',(18.395631157065,-21.4895394629701,4.05009944665238));
#145270=CARTESIAN_POINT('Ctrl Pts',(18.3123782833495,-21.4784380874206,
4.05428371393804));
#145271=CARTESIAN_POINT('Ctrl Pts',(18.229782980652,-21.4632501162163,4.0584679812237));
#145272=CARTESIAN_POINT('Ctrl Pts',(18.1482669036117,-21.4440908369872,
4.06265224850936));
#145273=CARTESIAN_POINT('Ctrl Pts',(18.1121675017119,-21.4356061484924,
4.0645052516455));
#145274=CARTESIAN_POINT('Ctrl Pts',(18.076279539388,-21.4263432749685,4.06635825478164));
#145275=CARTESIAN_POINT('Ctrl Pts',(18.0406384682269,-21.4163152773655,
4.06821125791777));
#145276=CARTESIAN_POINT('Ctrl Pts',(17.9601502870268,-21.3936690643915,
4.07239589231081));
#145277=CARTESIAN_POINT('Ctrl Pts',(17.8806229756134,-21.3670332665356,
4.07658052670385));
#145278=CARTESIAN_POINT('Ctrl Pts',(17.8024810747699,-21.3365067607239,
4.08076516109689));
#145279=CARTESIAN_POINT('Ctrl Pts',(17.7244503992504,-21.306023705615,4.08494383918082));
#145280=CARTESIAN_POINT('Ctrl Pts',(17.6478016421986,-21.2716611086066,
4.08912251726475));
#145281=CARTESIAN_POINT('Ctrl Pts',(17.5729454850813,-21.2335679725546,
4.09330119534867));
#145282=CARTESIAN_POINT('Ctrl Pts',(17.4967475851455,-21.1947920444157,
4.09755477323411));
#145283=CARTESIAN_POINT('Ctrl Pts',(17.422407646075,-21.1521506525344,4.10180835111955));
#145284=CARTESIAN_POINT('Ctrl Pts',(17.3503388850133,-21.1058528080799,
4.10606192900499));
#145285=CARTESIAN_POINT('Ctrl Pts',(17.2796673175155,-21.0604525376831,
4.11023304298293));
#145286=CARTESIAN_POINT('Ctrl Pts',(17.2111800563182,-21.0115365845697,
4.11440415696087));
#145287=CARTESIAN_POINT('Ctrl Pts',(17.1452415288503,-20.959348131329,4.11857527093882));
#145288=CARTESIAN_POINT('Ctrl Pts',(17.0793251276922,-20.9071771904278,
4.12274498525918));
#145289=CARTESIAN_POINT('Ctrl Pts',(17.01595612214,-20.8517362155439,4.12691469957954));
#145290=CARTESIAN_POINT('Ctrl Pts',(16.9554677262149,-20.7933101181237,
4.1310844138999));
#145291=CARTESIAN_POINT('Ctrl Pts',(16.8949814827263,-20.7348860997546,
4.13525397984395));
#145292=CARTESIAN_POINT('Ctrl Pts',(16.8373759753517,-20.6734774902646,
4.139423545788));
#145293=CARTESIAN_POINT('Ctrl Pts',(16.7829482470746,-20.6094067266084,
4.14359311173204));
#145294=CARTESIAN_POINT('Ctrl Pts',(16.7266069070151,-20.5430833139417,
4.14790927447097));
#145295=CARTESIAN_POINT('Ctrl Pts',(16.6736713066581,-20.47390746331,4.1522254372099));
#145296=CARTESIAN_POINT('Ctrl Pts',(16.6244248933205,-20.4022733774286,
4.15654159994883));
#145297=CARTESIAN_POINT('Ctrl Pts',(16.5767826767178,-20.3329727643605,
4.1607171641405));
#145298=CARTESIAN_POINT('Ctrl Pts',(16.5325931948253,-20.2613720362608,
4.16489272833218));
#145299=CARTESIAN_POINT('Ctrl Pts',(16.4920674161606,-20.1878552866412,
4.16906829252386));
#145300=CARTESIAN_POINT('Ctrl Pts',(16.4494947767562,-20.1106253807675,
4.17345475453641));
#145301=CARTESIAN_POINT('Ctrl Pts',(16.4109659295264,-20.0312813353545,
4.17784121654897));
#145302=CARTESIAN_POINT('Ctrl Pts',(16.3766684749372,-19.9502925828358,
4.18222767856152));
#145303=CARTESIAN_POINT('Ctrl Pts',(16.342371020348,-19.8693038303171,4.18661414057408));
#145304=CARTESIAN_POINT('Ctrl Pts',(16.3123050853067,-19.7866709419478,
4.19100060258663));
#145305=CARTESIAN_POINT('Ctrl Pts',(16.2865973915759,-19.702879798822,4.19538706459919));
#145306=CARTESIAN_POINT('Ctrl Pts',(16.2566341527394,-19.6052182170345,
4.2004996433589));
#145307=CARTESIAN_POINT('Ctrl Pts',(16.2324986213406,-19.5056900725379,
4.20561222211862));
#145308=CARTESIAN_POINT('Ctrl Pts',(16.2143850329185,-19.404924295726,4.21072480087833));
#145309=CARTESIAN_POINT('Ctrl Pts',(16.1965183144937,-19.3055318551339,
4.21576770033015));
#145310=CARTESIAN_POINT('Ctrl Pts',(16.1845105456257,-19.2049352741343,
4.22081059978196));
#145311=CARTESIAN_POINT('Ctrl Pts',(16.1785021632643,-19.1037590407164,
4.22585349923378));
#145312=CARTESIAN_POINT('Ctrl Pts',(16.1755487125963,-19.0540253526453,
4.22833236190576));
#145313=CARTESIAN_POINT('Ctrl Pts',(16.174044162412,-19.0041519285503,4.23081122457773));
#145314=CARTESIAN_POINT('Ctrl Pts',(16.1740009581142,-18.9542148462772,
4.23329008724971));
#145315=CARTESIAN_POINT('',(16.1740010840393,-18.9496440968074,4.16670989022851));
#145316=CARTESIAN_POINT('Ctrl Pts',(20.2935357468249,-20.9821350335323,
3.88329345209042));
#145317=CARTESIAN_POINT('Ctrl Pts',(20.2268447907951,-21.0333665665094,
3.88746332012199));
#145318=CARTESIAN_POINT('Ctrl Pts',(20.1576354539796,-21.081301703658,3.89163318815356));
#145319=CARTESIAN_POINT('Ctrl Pts',(20.0862723557994,-21.1256971904432,
3.89580305618514));
#145320=CARTESIAN_POINT('Ctrl Pts',(20.0148340605621,-21.1701394578481,
3.89997731810953));
#145321=CARTESIAN_POINT('Ctrl Pts',(19.9412378639014,-21.2110343840631,
3.90415158003392));
#145322=CARTESIAN_POINT('Ctrl Pts',(19.8658750790502,-21.2481835304316,
3.90832584195832));
#145323=CARTESIAN_POINT('Ctrl Pts',(19.7904707301851,-21.2853531652631,
3.91250240606781));
#145324=CARTESIAN_POINT('Ctrl Pts',(19.7132982754322,-21.318772723907,3.9166789701773));
#145325=CARTESIAN_POINT('Ctrl Pts',(19.6347689672755,-21.348291982959,3.92085553428679));
#145326=CARTESIAN_POINT('Ctrl Pts',(19.5561040322652,-21.3778622243043,
3.92503931168088));
#145327=CARTESIAN_POINT('Ctrl Pts',(19.4760780019455,-21.4035185719984,
3.92922308907496));
#145328=CARTESIAN_POINT('Ctrl Pts',(19.3951169987244,-21.425160794206,3.93340686646905));
#145329=CARTESIAN_POINT('Ctrl Pts',(19.3367852034137,-21.440753852909,3.93642124668752));
#145330=CARTESIAN_POINT('Ctrl Pts',(19.2779683413532,-21.4542642055276,
3.939435626906));
#145331=CARTESIAN_POINT('Ctrl Pts',(19.2188278686569,-21.4656710082613,
3.94245000712447));
#145332=CARTESIAN_POINT('Ctrl Pts',(19.1367276562992,-21.4815062034173,
3.94663464151748));
#145333=CARTESIAN_POINT('Ctrl Pts',(19.0536980417282,-21.4933443659488,
3.95081927591048));
#145334=CARTESIAN_POINT('Ctrl Pts',(18.9701628470243,-21.5010835823263,
3.95500391030349));
#145335=CARTESIAN_POINT('Ctrl Pts',(18.8867465543307,-21.5088117828872,
3.95918258838737));
#145336=CARTESIAN_POINT('Ctrl Pts',(18.8028265650705,-21.5124525840587,
3.96336126647126));
#145337=CARTESIAN_POINT('Ctrl Pts',(18.7188367813175,-21.511955092731,3.96753994455515));
#145338=CARTESIAN_POINT('Ctrl Pts',(18.6333415410516,-21.5114486842287,
3.97179352244059));
#145339=CARTESIAN_POINT('Ctrl Pts',(18.5477744529633,-21.5066540748902,
3.97604710032604));
#145340=CARTESIAN_POINT('Ctrl Pts',(18.4625985845178,-21.4975728769128,
3.98030067821149));
#145341=CARTESIAN_POINT('Ctrl Pts',(18.3790740164904,-21.4886677356789,
3.98447179218939));
#145342=CARTESIAN_POINT('Ctrl Pts',(18.2959261128669,-21.4756407813848,
3.98864290616729));
#145343=CARTESIAN_POINT('Ctrl Pts',(18.2135896449266,-21.4585460423324,
3.99281402014519));
#145344=CARTESIAN_POINT('Ctrl Pts',(18.1312808057834,-21.4414570395849,
3.99698373446551));
#145345=CARTESIAN_POINT('Ctrl Pts',(18.0497833116132,-21.4203030564001,
4.00115344878582));
#145346=CARTESIAN_POINT('Ctrl Pts',(17.9695227367358,-21.39518941426,4.00532316310613));
#145347=CARTESIAN_POINT('Ctrl Pts',(17.8892650178741,-21.370076665771,4.00949272905012));
#145348=CARTESIAN_POINT('Ctrl Pts',(17.8102445695797,-21.3410046766655,
4.0136622949941));
#145349=CARTESIAN_POINT('Ctrl Pts',(17.7328714533957,-21.3081285264548,
4.01783186093808));
#145350=CARTESIAN_POINT('Ctrl Pts',(17.6527779938943,-21.2740964913587,
4.02214802367707));
#145351=CARTESIAN_POINT('Ctrl Pts',(17.574450347639,-21.2359880155545,4.02646418641605));
#145352=CARTESIAN_POINT('Ctrl Pts',(17.4983185919004,-21.1940284248147,
4.03078034915504));
#145353=CARTESIAN_POINT('Ctrl Pts',(17.4246668200994,-21.153435663331,4.03495591334666));
#145354=CARTESIAN_POINT('Ctrl Pts',(17.3530704495486,-21.1092391216323,
4.03913147753829));
#145355=CARTESIAN_POINT('Ctrl Pts',(17.283890236673,-21.0616875774161,4.04330704172991));
#145356=CARTESIAN_POINT('Ctrl Pts',(17.2112158957024,-21.0117343177425,
4.04769350374258));
#145357=CARTESIAN_POINT('Ctrl Pts',(17.1412086706277,-20.9580785813379,
4.05207996575524));
#145358=CARTESIAN_POINT('Ctrl Pts',(17.0742466821567,-20.9010559057934,
4.05646642776791));
#145359=CARTESIAN_POINT('Ctrl Pts',(17.0072846936857,-20.8440332302489,
4.06085288978057));
#145360=CARTESIAN_POINT('Ctrl Pts',(16.943368311327,-20.7836440693278,4.06523935179323));
#145361=CARTESIAN_POINT('Ctrl Pts',(16.8828286089282,-20.7202659530956,
4.0696258138059));
#145362=CARTESIAN_POINT('Ctrl Pts',(16.8258191500137,-20.66058359639,4.07375648865202));
#145363=CARTESIAN_POINT('Ctrl Pts',(16.7715797255597,-20.5980163329693,
4.07788716349815));
#145364=CARTESIAN_POINT('Ctrl Pts',(16.720421868205,-20.5328551822216,4.08201783834428));
#145365=CARTESIAN_POINT('Ctrl Pts',(16.6693300782615,-20.467778183328,4.08614317866297));
#145366=CARTESIAN_POINT('Ctrl Pts',(16.6213122506322,-20.4001143092104,
4.09026851898165));
#145367=CARTESIAN_POINT('Ctrl Pts',(16.5766430483355,-20.3301911997632,
4.09439385930034));
#145368=CARTESIAN_POINT('Ctrl Pts',(16.5320173182039,-20.2603361396388,
4.09851518482882));
#145369=CARTESIAN_POINT('Ctrl Pts',(16.4907340001793,-20.1882266026471,
4.1026365103573));
#145370=CARTESIAN_POINT('Ctrl Pts',(16.4530264539488,-20.1142218730582,
4.10675783588578));
#145371=CARTESIAN_POINT('Ctrl Pts',(16.4153436115611,-20.0402656271648,
4.11087646135585));
#145372=CARTESIAN_POINT('Ctrl Pts',(16.3812321043791,-19.9644170734852,
4.11499508682592));
#145373=CARTESIAN_POINT('Ctrl Pts',(16.3508802454214,-19.8870616211443,
4.11911371229599));
#145374=CARTESIAN_POINT('Ctrl Pts',(16.3205285952527,-19.8097067009281,
4.12323230943423));
#145375=CARTESIAN_POINT('Ctrl Pts',(16.2939367323083,-19.7308453355426,
4.12735090657246));
#145376=CARTESIAN_POINT('Ctrl Pts',(16.2712450678812,-19.6508834983921,
4.13146950371069));
#145377=CARTESIAN_POINT('Ctrl Pts',(16.2485547151173,-19.570926283335,4.1355878627786));
#145378=CARTESIAN_POINT('Ctrl Pts',(16.2297642345971,-19.4898691801182,
4.1397062218465));
#145379=CARTESIAN_POINT('Ctrl Pts',(16.2149637529308,-19.4081319830394,
4.14382458091441));
#145380=CARTESIAN_POINT('Ctrl Pts',(16.2001500672816,-19.3263218655941,
4.14794661410208));
#145381=CARTESIAN_POINT('Ctrl Pts',(16.1893335672674,-19.2438309098088,
4.15206864728976));
#145382=CARTESIAN_POINT('Ctrl Pts',(16.1825528364004,-19.1610869947166,
4.15619068047744));
#145383=CARTESIAN_POINT('Ctrl Pts',(16.1767848147302,-19.0907009692733,
4.1596970837278));
#145384=CARTESIAN_POINT('Ctrl Pts',(16.1739362156169,-19.020132176051,4.16320348697815));
#145385=CARTESIAN_POINT('Ctrl Pts',(16.1740010840393,-18.9496440968074,
4.16670989022851));
#145386=CARTESIAN_POINT('Ctrl Pts',(16.174088184599,-18.9496434116999,4.16670992829755));
#145387=CARTESIAN_POINT('Ctrl Pts',(16.1722334877636,-18.748007243103,4.17674049236081));
#145388=CARTESIAN_POINT('Ctrl Pts',(16.2862273000593,-17.6962739531831,
4.22916299198455));
#145389=CARTESIAN_POINT('Ctrl Pts',(17.7370129389085,-16.0937997547996,
4.32397742716877));
#145390=CARTESIAN_POINT('Ctrl Pts',(20.5976438994044,-16.5666020755754,
4.4511532338502));
#145391=CARTESIAN_POINT('Ctrl Pts',(21.6812139993619,-19.0722717640235,
4.57089386034247));
#145392=CARTESIAN_POINT('Ctrl Pts',(20.8466207859578,-20.5504284027622,
4.64824255127427));
#145393=CARTESIAN_POINT('Ctrl Pts',(20.2944552458116,-20.9833106134464,
4.68319930664559));
#145394=CARTESIAN_POINT('Origin',(18.734,-18.952,-1.76670989022851));
#145395=CARTESIAN_POINT('',(20.2935357468249,-20.9821350335323,5.54983331705304));
#145396=CARTESIAN_POINT('',(20.2935357468249,-20.9821350335323,5.4833696516309));
#145397=CARTESIAN_POINT('',(20.2935357468249,-20.9821350335323,-1.76670989022851));
#145398=CARTESIAN_POINT('',(16.1741505039397,-18.9508032548666,5.03329016024815));
#145399=CARTESIAN_POINT('Ctrl Pts',(16.1740002797795,-18.9508031412289,
5.03329016239971));
#145400=CARTESIAN_POINT('Ctrl Pts',(16.1740435234788,-18.8583078019676,
5.03786858507912));
#145401=CARTESIAN_POINT('Ctrl Pts',(16.1791038614083,-18.7659792628304,
5.04244700775854));
#145402=CARTESIAN_POINT('Ctrl Pts',(16.1891023385012,-18.6743385289637,
5.04702543043795));
#145403=CARTESIAN_POINT('Ctrl Pts',(16.1991318881351,-18.5824130006799,
5.05161808160685));
#145404=CARTESIAN_POINT('Ctrl Pts',(16.2141301908472,-18.4911798450087,
5.05621073277575));
#145405=CARTESIAN_POINT('Ctrl Pts',(16.2339673694791,-18.401148979913,5.06080338394464));
#145406=CARTESIAN_POINT('Ctrl Pts',(16.253896242195,-18.3107019620039,5.06541726388551));
#145407=CARTESIAN_POINT('Ctrl Pts',(16.2787086950666,-18.2214686541854,
5.07003114382637));
#145408=CARTESIAN_POINT('Ctrl Pts',(16.3082244096464,-18.1339457320907,
5.07464502376723));
#145409=CARTESIAN_POINT('Ctrl Pts',(16.3316224115872,-18.064563657823,5.07830258630123));
#145410=CARTESIAN_POINT('Ctrl Pts',(16.3579750606108,-17.996256071474,5.08196014883524));
#145411=CARTESIAN_POINT('Ctrl Pts',(16.3871718743356,-17.9292596866308,
5.08561771136924));
#145412=CARTESIAN_POINT('Ctrl Pts',(16.4205760854036,-17.8526088095457,
5.08980234576229));
#145413=CARTESIAN_POINT('Ctrl Pts',(16.4578017058021,-17.7774535557437,
5.09398698015534));
#145414=CARTESIAN_POINT('Ctrl Pts',(16.4986929228155,-17.7042010295369,
5.09817161454839));
#145415=CARTESIAN_POINT('Ctrl Pts',(16.5395259362428,-17.6310527692343,
5.10235029263233));
#145416=CARTESIAN_POINT('Ctrl Pts',(16.5840139603303,-17.559802255246,5.10652897071626));
#145417=CARTESIAN_POINT('Ctrl Pts',(16.6319534129312,-17.4908360304906,
5.1107076488002));
#145418=CARTESIAN_POINT('Ctrl Pts',(16.6807521457665,-17.4206336357216,
5.11496122668564));
#145419=CARTESIAN_POINT('Ctrl Pts',(16.7331270652481,-17.3527986694292,
5.11921480457108));
#145420=CARTESIAN_POINT('Ctrl Pts',(16.7888147952352,-17.2877120083459,
5.12346838245651));
#145421=CARTESIAN_POINT('Ctrl Pts',(16.8434229099109,-17.2238871791938,
5.12763949643446));
#145422=CARTESIAN_POINT('Ctrl Pts',(16.9012162179242,-17.1627054093257,
5.13181061041241));
#145423=CARTESIAN_POINT('Ctrl Pts',(16.961904139826,-17.1044945839446,5.13598172439036));
#145424=CARTESIAN_POINT('Ctrl Pts',(17.0225716973095,-17.0463032917681,
5.14015143871074));
#145425=CARTESIAN_POINT('Ctrl Pts',(17.086131607912,-16.9910812823427,5.14432115303111));
#145426=CARTESIAN_POINT('Ctrl Pts',(17.1522562065725,-16.9391198316955,
5.14849086735148));
#145427=CARTESIAN_POINT('Ctrl Pts',(17.218378452236,-16.8871602300597,5.15266043329552));
#145428=CARTESIAN_POINT('Ctrl Pts',(17.2870648422621,-16.8384612400851,
5.15682999923956));
#145429=CARTESIAN_POINT('Ctrl Pts',(17.3579554657567,-16.7932731901004,
5.1609995651836));
#145430=CARTESIAN_POINT('Ctrl Pts',(17.4313385161205,-16.7464963840237,
5.16531572792253));
#145431=CARTESIAN_POINT('Ctrl Pts',(17.5070832408523,-16.7034822843462,
5.16963189066145));
#145432=CARTESIAN_POINT('Ctrl Pts',(17.5847604857694,-16.6644579700187,
5.17394805340037));
#145433=CARTESIAN_POINT('Ctrl Pts',(17.6599074026034,-16.6267048686259,
5.17812361759205));
#145434=CARTESIAN_POINT('Ctrl Pts',(17.7368624194976,-16.5926857570979,
5.18229918178373));
#145435=CARTESIAN_POINT('Ctrl Pts',(17.81521627489,-16.5625572895604,5.1864747459754));
#145436=CARTESIAN_POINT('Ctrl Pts',(17.8975275972497,-16.5309071047512,
5.19086120798795));
#145437=CARTESIAN_POINT('Ctrl Pts',(17.9813822273942,-16.5035511069692,
5.19524767000049));
#145438=CARTESIAN_POINT('Ctrl Pts',(18.0662895457778,-16.4806111699446,
5.19963413201304));
#145439=CARTESIAN_POINT('Ctrl Pts',(18.1511968641614,-16.4576712329201,
5.20402059402558));
#145440=CARTESIAN_POINT('Ctrl Pts',(18.2371562875636,-16.439147404523,5.20840705603812));
#145441=CARTESIAN_POINT('Ctrl Pts',(18.3236691980734,-16.4250990060965,
5.21279351805067));
#145442=CARTESIAN_POINT('Ctrl Pts',(18.4062015213278,-16.4116969953064,
5.21697815244372));
#145443=CARTESIAN_POINT('Ctrl Pts',(18.4895447184805,-16.4023177375285,
5.22116278683677));
#145444=CARTESIAN_POINT('Ctrl Pts',(18.573272140763,-16.3970505767697,5.22534742122982));
#145445=CARTESIAN_POINT('Ctrl Pts',(18.6568803874232,-16.3917909131622,
5.22952609931376));
#145446=CARTESIAN_POINT('Ctrl Pts',(18.7408713177055,-16.3906317491884,
5.2337047773977));
#145447=CARTESIAN_POINT('Ctrl Pts',(18.8248097150325,-16.3936111328307,
5.23788345548165));
#145448=CARTESIAN_POINT('Ctrl Pts',(18.910252647806,-16.3966439197836,5.24213703336708));
#145449=CARTESIAN_POINT('Ctrl Pts',(18.9956406698882,-16.4039651578947,
5.24639061125252));
#145450=CARTESIAN_POINT('Ctrl Pts',(19.0805109637125,-16.4155595508613,
5.25064418913795));
#145451=CARTESIAN_POINT('Ctrl Pts',(19.1637358812804,-16.4269291638956,
5.25481530311591));
#145452=CARTESIAN_POINT('Ctrl Pts',(19.2464624890054,-16.44240765832,5.25898641709386));
#145453=CARTESIAN_POINT('Ctrl Pts',(19.3282578021761,-16.4619281808444,
5.26315753107181));
#145454=CARTESIAN_POINT('Ctrl Pts',(19.4100256681395,-16.4814421530689,
5.26732724539218));
#145455=CARTESIAN_POINT('Ctrl Pts',(19.4908624130939,-16.504995352978,5.27149695971256));
#145456=CARTESIAN_POINT('Ctrl Pts',(19.570345761113,-16.5324699282984,5.27566667403293));
#145457=CARTESIAN_POINT('Ctrl Pts',(19.6498262807736,-16.5599435259555,
5.27983623997698));
#145458=CARTESIAN_POINT('Ctrl Pts',(19.7279530647408,-16.5913380704867,
5.28400580592102));
#145459=CARTESIAN_POINT('Ctrl Pts',(19.8043208135647,-16.6264864317639,
5.28817537186507));
#145460=CARTESIAN_POINT('Ctrl Pts',(19.8833735582274,-16.6628705660633,
5.29249153460399));
#145461=CARTESIAN_POINT('Ctrl Pts',(19.9605407918123,-16.7032771763716,
5.29680769734291));
#145462=CARTESIAN_POINT('Ctrl Pts',(20.0353992838381,-16.7474683254656,
5.30112386008183));
#145463=CARTESIAN_POINT('Ctrl Pts',(20.10781926836,-16.7902199525259,5.30529942427351));
#145464=CARTESIAN_POINT('Ctrl Pts',(20.1780782485914,-16.8365130434918,
5.30947498846519));
#145465=CARTESIAN_POINT('Ctrl Pts',(20.2458229776825,-16.8860882680639,
5.31365055265687));
#145466=CARTESIAN_POINT('Ctrl Pts',(20.3169893319923,-16.9381674193753,
5.31803701466941));
#145467=CARTESIAN_POINT('Ctrl Pts',(20.3853803178148,-16.993868610292,5.32242347668195));
#145468=CARTESIAN_POINT('Ctrl Pts',(20.450627895575,-17.052845275357,5.32680993869449));
#145469=CARTESIAN_POINT('Ctrl Pts',(20.5158754733353,-17.1118219404221,
5.33119640070703));
#145470=CARTESIAN_POINT('Ctrl Pts',(20.5779792870959,-17.1740736151504,
5.33558286271957));
#145471=CARTESIAN_POINT('Ctrl Pts',(20.6366195645771,-17.239213150305,5.33996932473211));
#145472=CARTESIAN_POINT('Ctrl Pts',(20.6925617159657,-17.3013555188871,
5.34415395912515));
#145473=CARTESIAN_POINT('Ctrl Pts',(20.7455602793472,-17.3663571440021,
5.3483385935182));
#145474=CARTESIAN_POINT('Ctrl Pts',(20.7953091936645,-17.4339076417707,
5.35252322791125));
#145475=CARTESIAN_POINT('Ctrl Pts',(20.8449872965599,-17.5013619897667,
5.35670190599519));
#145476=CARTESIAN_POINT('Ctrl Pts',(20.891424667568,-17.5713576368075,5.36088058407914));
#145477=CARTESIAN_POINT('Ctrl Pts',(20.934353739878,-17.6435492292772,5.36505926216308));
#145478=CARTESIAN_POINT('Ctrl Pts',(20.9780522849565,-17.7170348041588,
5.36931284004852));
#145479=CARTESIAN_POINT('Ctrl Pts',(21.0181151991572,-17.7927954651137,
5.37356641793395));
#145480=CARTESIAN_POINT('Ctrl Pts',(21.0543048298795,-17.8704337762125,
5.37781999581939));
#145481=CARTESIAN_POINT('Ctrl Pts',(21.089792853992,-17.9465669171521,5.38199110979734));
#145482=CARTESIAN_POINT('Ctrl Pts',(21.1215562334332,-18.0245051179383,
5.38616222377529));
#145483=CARTESIAN_POINT('Ctrl Pts',(21.1494168148284,-18.1038481205324,
5.39033333775324));
#145484=CARTESIAN_POINT('Ctrl Pts',(21.1772680473364,-18.1831644988156,
5.39450305207362));
#145485=CARTESIAN_POINT('Ctrl Pts',(21.2012189304412,-18.2638843090191,
5.39867276639399));
#145486=CARTESIAN_POINT('Ctrl Pts',(21.2211399893044,-18.3455886927151,
5.40284248071436));
#145487=CARTESIAN_POINT('Ctrl Pts',(21.2410603392908,-18.4272901690185,
5.4070120466584));
#145488=CARTESIAN_POINT('Ctrl Pts',(21.2569510420042,-18.5099757020134,
5.41118161260245));
#145489=CARTESIAN_POINT('Ctrl Pts',(21.2687332465284,-18.5932140346339,
5.41535117854649));
#145490=CARTESIAN_POINT('Ctrl Pts',(21.2809296988287,-18.6793789243437,
5.41966734128541));
#145491=CARTESIAN_POINT('Ctrl Pts',(21.2887232939913,-18.766135687597,5.42398350402433));
#145492=CARTESIAN_POINT('Ctrl Pts',(21.2920850129342,-18.8529996636307,
5.42829966676325));
#145493=CARTESIAN_POINT('Ctrl Pts',(21.2953372242362,-18.9370340547816,
5.43247523095493));
#145494=CARTESIAN_POINT('Ctrl Pts',(21.2944419142066,-19.0211683105535,
5.43665079514661));
#145495=CARTESIAN_POINT('Ctrl Pts',(21.2894259327675,-19.1049650356757,
5.44082635933829));
#145496=CARTESIAN_POINT('Ctrl Pts',(21.2841566060303,-19.1929941341762,
5.44521282135083));
#145497=CARTESIAN_POINT('Ctrl Pts',(21.2743394628619,-19.2806501283313,
5.44959928336337));
#145498=CARTESIAN_POINT('Ctrl Pts',(21.2600666971253,-19.3674359657934,
5.45398574537591));
#145499=CARTESIAN_POINT('Ctrl Pts',(21.2457939313886,-19.4542218032555,
5.45837220738845));
#145500=CARTESIAN_POINT('Ctrl Pts',(21.2270657409798,-19.5401369333207,
5.46275866940099));
#145501=CARTESIAN_POINT('Ctrl Pts',(21.2040345704695,-19.6247029215675,
5.46714513141354));
#145502=CARTESIAN_POINT('Ctrl Pts',(21.1820669712701,-19.7053636823778,
5.4713290281613));
#145503=CARTESIAN_POINT('Ctrl Pts',(21.1561032921522,-19.7850973400373,
5.47551292490906));
#145504=CARTESIAN_POINT('Ctrl Pts',(21.1262387968713,-19.8634787648343,
5.47969682165682));
#145505=CARTESIAN_POINT('Ctrl Pts',(21.0964141293845,-19.9417556588425,
5.48387513868938));
#145506=CARTESIAN_POINT('Ctrl Pts',(21.0626991366584,-20.0186834745666,
5.48805345572194));
#145507=CARTESIAN_POINT('Ctrl Pts',(21.0252393289067,-20.0938504007405,
5.4922317727545));
#145508=CARTESIAN_POINT('Ctrl Pts',(20.9878182356716,-20.1689396422868,
5.49640577151812));
#145509=CARTESIAN_POINT('Ctrl Pts',(20.9466602184249,-20.2422711993806,
5.50057977028174));
#145510=CARTESIAN_POINT('Ctrl Pts',(20.9019590364997,-20.3134527593932,
5.50475376904535));
#145511=CARTESIAN_POINT('Ctrl Pts',(20.8572882174555,-20.3845859699629,
5.50892493265736));
#145512=CARTESIAN_POINT('Ctrl Pts',(20.809079257669,-20.4535716954205,5.51309609626937));
#145513=CARTESIAN_POINT('Ctrl Pts',(20.7575714330065,-20.5200429380346,
5.51726725988138));
#145514=CARTESIAN_POINT('Ctrl Pts',(20.7060846236983,-20.5864870601728,
5.52143672164553));
#145515=CARTESIAN_POINT('Ctrl Pts',(20.6513019074181,-20.65041837625,5.52560618340968));
#145516=CARTESIAN_POINT('Ctrl Pts',(20.5935045656375,-20.7115007162185,
5.52977564517383));
#145517=CARTESIAN_POINT('Ctrl Pts',(20.5356974931368,-20.7725933399669,
5.53394580890565));
#145518=CARTESIAN_POINT('Ctrl Pts',(20.4748750940648,-20.8308356918434,
5.53811597263746));
#145519=CARTESIAN_POINT('Ctrl Pts',(20.4113567585225,-20.885927171493,5.54228613636927));
#145520=CARTESIAN_POINT('Ctrl Pts',(20.3730381707404,-20.9191621056419,
5.54480186326386));
#145521=CARTESIAN_POINT('Ctrl Pts',(20.3337391579018,-20.951251050111,5.54731759015845));
#145522=CARTESIAN_POINT('Ctrl Pts',(20.2935357468249,-20.9821350335323,
5.54983331705304));
#145523=CARTESIAN_POINT('Ctrl Pts',(20.2917778074114,-20.979810503055,4.74997346711437));
#145524=CARTESIAN_POINT('Ctrl Pts',(19.8562818605801,-21.3095662733656,
4.77707101074504));
#145525=CARTESIAN_POINT('Ctrl Pts',(18.4733993847563,-21.8166034507402,
4.84656048993618));
#145526=CARTESIAN_POINT('Ctrl Pts',(16.5671405548292,-20.815635979695,4.94099937082189));
#145527=CARTESIAN_POINT('Ctrl Pts',(16.1797898378084,-19.4541224957223,
5.00834070807693));
#145528=CARTESIAN_POINT('Ctrl Pts',(16.1776748285763,-18.9508059208577,
5.0332901097715));
#145529=CARTESIAN_POINT('',(16.1737368696253,-18.9528355653615,4.96670989022851));
#145530=CARTESIAN_POINT('Ctrl Pts',(20.2944552458116,-20.9833106134464,
4.68319930664559));
#145531=CARTESIAN_POINT('Ctrl Pts',(20.1770115574137,-21.0753831528721,
4.69063448683475));
#145532=CARTESIAN_POINT('Ctrl Pts',(19.3369083430137,-21.6211180130261,
4.74046160258439));
#145533=CARTESIAN_POINT('Ctrl Pts',(17.2348043616254,-21.581772666889,4.8326806538945));
#145534=CARTESIAN_POINT('Ctrl Pts',(16.1917618388527,-19.8928505847622,
4.91974900156632));
#145535=CARTESIAN_POINT('Ctrl Pts',(16.1699049957539,-18.998574246681,4.96442541367765));
#145536=CARTESIAN_POINT('Ctrl Pts',(16.1700997034774,-18.952836752384,4.96670989022851));
#145537=CARTESIAN_POINT('Ctrl Pts',(16.1740001363332,-18.952835479442,4.96670989022851));
#145538=CARTESIAN_POINT('Ctrl Pts',(16.1739730621524,-18.8698772454868,
4.97085977152528));
#145539=CARTESIAN_POINT('Ctrl Pts',(16.1779827035226,-18.7867551328103,
4.97500965282205));
#145540=CARTESIAN_POINT('Ctrl Pts',(16.1860506816107,-18.7038986680416,
4.97915953411883));
#145541=CARTESIAN_POINT('Ctrl Pts',(16.194107496698,-18.6211568449803,4.98330367356457));
#145542=CARTESIAN_POINT('Ctrl Pts',(16.2062114544436,-18.5386804021303,
4.98744781301032));
#145543=CARTESIAN_POINT('Ctrl Pts',(16.2223321624274,-18.4568993297282,
4.99159195245607));
#145544=CARTESIAN_POINT('Ctrl Pts',(16.2384354396283,-18.3752066844675,
4.99573161098228));
#145545=CARTESIAN_POINT('Ctrl Pts',(16.258546748188,-18.2942083730103,4.99987126950849));
#145546=CARTESIAN_POINT('Ctrl Pts',(16.2825840079951,-18.2143282341429,
5.0040109280347));
#145547=CARTESIAN_POINT('Ctrl Pts',(16.3066073287289,-18.1344944173239,
5.00814818599595));
#145548=CARTESIAN_POINT('Ctrl Pts',(16.33455194816,-18.0557779336924,5.0122854439572));
#145549=CARTESIAN_POINT('Ctrl Pts',(16.3662852025775,-17.9785902003439,
5.01642270191845));
#145550=CARTESIAN_POINT('Ctrl Pts',(16.3980099615293,-17.9014231313034,
5.020558852274));
#145551=CARTESIAN_POINT('Ctrl Pts',(16.4335211635118,-17.8257844328042,
5.02469500262956));
#145552=CARTESIAN_POINT('Ctrl Pts',(16.4726375176037,-17.7520667838541,
5.02883115298511));
#145553=CARTESIAN_POINT('Ctrl Pts',(16.5117556109323,-17.6783458571842,
5.03296748724699));
#145554=CARTESIAN_POINT('Ctrl Pts',(16.5544789534253,-17.6065465624547,
5.03710382150887));
#145555=CARTESIAN_POINT('Ctrl Pts',(16.6005803897996,-17.5370368319944,
5.04124015577075));
#145556=CARTESIAN_POINT('Ctrl Pts',(16.646728500548,-17.4674567279532,5.04538067777228));
#145557=CARTESIAN_POINT('Ctrl Pts',(16.6962612737695,-17.4001712070013,
5.04952119977381));
#145558=CARTESIAN_POINT('Ctrl Pts',(16.7489086678727,-17.3355185113609,
5.05366172177533));
#145559=CARTESIAN_POINT('Ctrl Pts',(16.8015842228024,-17.2708312333184,
5.05780445852127));
#145560=CARTESIAN_POINT('Ctrl Pts',(16.8573774008556,-17.2087799314012,
5.06194719526721));
#145561=CARTESIAN_POINT('Ctrl Pts',(16.9159800655235,-17.1496672011401,
5.06608993201314));
#145562=CARTESIAN_POINT('Ctrl Pts',(16.9746826938398,-17.0904536371675,
5.07023973538449));
#145563=CARTESIAN_POINT('Ctrl Pts',(17.0362040315237,-17.0341889688223,
5.07438953875584));
#145564=CARTESIAN_POINT('Ctrl Pts',(17.1002018437186,-16.9811363353769,
5.07853934212719));
#145565=CARTESIAN_POINT('Ctrl Pts',(17.1438608301676,-16.9449440949669,
5.08137031717058));
#145566=CARTESIAN_POINT('Ctrl Pts',(17.1886716656529,-16.910245843732,5.08420129221397));
#145567=CARTESIAN_POINT('Ctrl Pts',(17.2345184376715,-16.8771132454428,
5.08703226725736));
#145568=CARTESIAN_POINT('Ctrl Pts',(17.302287307428,-16.8281379601765,5.09121690165041));
#145569=CARTESIAN_POINT('Ctrl Pts',(17.3725842232475,-16.78239517261,5.09540153604346));
#145570=CARTESIAN_POINT('Ctrl Pts',(17.4450678487465,-16.7401559934152,
5.09958617043651));
#145571=CARTESIAN_POINT('Ctrl Pts',(17.5174483027761,-16.6979769364639,
5.10376484852044));
#145572=CARTESIAN_POINT('Ctrl Pts',(17.5920088899902,-16.6592918118672,
5.10794352660438));
#145573=CARTESIAN_POINT('Ctrl Pts',(17.668377621725,-16.6243297168801,5.11212220468832));
#145574=CARTESIAN_POINT('Ctrl Pts',(17.7461152080912,-16.588740951467,5.11637578257375));
#145575=CARTESIAN_POINT('Ctrl Pts',(17.8257260077699,-16.5570102814917,
5.12062936045919));
#145576=CARTESIAN_POINT('Ctrl Pts',(17.9067894477687,-16.5293314914588,
5.12488293834462));
#145577=CARTESIAN_POINT('Ctrl Pts',(17.9862813148007,-16.5021893087815,
5.12905405232258));
#145578=CARTESIAN_POINT('Ctrl Pts',(18.0671695448446,-16.4789434563412,
5.13322516630053));
#145579=CARTESIAN_POINT('Ctrl Pts',(18.1490371223199,-16.4597282588497,
5.13739628027848));
#145580=CARTESIAN_POINT('Ctrl Pts',(18.230877228339,-16.4405195092033,5.14156599459885));
#145581=CARTESIAN_POINT('Ctrl Pts',(18.3136955816366,-16.4253388333998,
5.14573570891923));
#145582=CARTESIAN_POINT('Ctrl Pts',(18.3970618790066,-16.4142701675274,
5.1499054232396));
#145583=CARTESIAN_POINT('Ctrl Pts',(18.4804252098459,-16.4032018955257,
5.15407498918364));
#145584=CARTESIAN_POINT('Ctrl Pts',(18.5643359898469,-16.3962454022306,
5.15824455512768));
#145585=CARTESIAN_POINT('Ctrl Pts',(18.6483570024146,-16.3934329641449,
5.16241412107172));
#145586=CARTESIAN_POINT('Ctrl Pts',(18.7353320901331,-16.3905216442056,
5.16673028381064));
#145587=CARTESIAN_POINT('Ctrl Pts',(18.8224247790685,-16.3920512290412,
5.17104644654956));
#145588=CARTESIAN_POINT('Ctrl Pts',(18.9091500846456,-16.3979987376964,
5.17536260928849));
#145589=CARTESIAN_POINT('Ctrl Pts',(18.9930503225153,-16.4037525068826,
5.17953817348017));
#145590=CARTESIAN_POINT('Ctrl Pts',(19.0766062822584,-16.4136406900188,
5.18371373767185));
#145591=CARTESIAN_POINT('Ctrl Pts',(19.1593859487955,-16.4275898125369,
5.18788930186352));
#145592=CARTESIAN_POINT('Ctrl Pts',(19.2463466194995,-16.4422434720725,
5.19227576387607));
#145593=CARTESIAN_POINT('Ctrl Pts',(19.3324499449359,-16.4613789616178,
5.19666222588862));
#145594=CARTESIAN_POINT('Ctrl Pts',(19.4172115835231,-16.4848514572203,
5.20104868790117));
#145595=CARTESIAN_POINT('Ctrl Pts',(19.5019732221102,-16.5083239528228,
5.20543514991371));
#145596=CARTESIAN_POINT('Ctrl Pts',(19.5853926474676,-16.5361331988246,
5.20982161192626));
#145597=CARTESIAN_POINT('Ctrl Pts',(19.6670104728637,-16.5680764572817,
5.21420807393881));
#145598=CARTESIAN_POINT('Ctrl Pts',(19.7448729411266,-16.5985499590658,
5.21839270833186));
#145599=CARTESIAN_POINT('Ctrl Pts',(19.8213857737637,-16.6328988372128,
5.22257734272491));
#145600=CARTESIAN_POINT('Ctrl Pts',(19.8961362506934,-16.6709828289063,
5.22676197711796));
#145601=CARTESIAN_POINT('Ctrl Pts',(19.9707803295716,-16.7090126127515,
5.23094065520191));
#145602=CARTESIAN_POINT('Ctrl Pts',(20.0436666290096,-16.7507667429072,
5.23511933328585));
#145603=CARTESIAN_POINT('Ctrl Pts',(20.1144011640629,-16.7960564417746,
5.2392980113698));
#145604=CARTESIAN_POINT('Ctrl Pts',(20.186403564821,-16.842157925945,5.24355158925524));
#145605=CARTESIAN_POINT('Ctrl Pts',(20.2561758527108,-16.8919227999547,
5.24780516714067));
#145606=CARTESIAN_POINT('Ctrl Pts',(20.3233274374464,-16.9451023203511,
5.25205874502611));
#145607=CARTESIAN_POINT('Ctrl Pts',(20.3891771576765,-16.9972508519734,
5.25622985900406));
#145608=CARTESIAN_POINT('Ctrl Pts',(20.4525065055991,-17.052682513567,5.26040097298202));
#145609=CARTESIAN_POINT('Ctrl Pts',(20.5129768127645,-17.1111193684417,
5.26457208695997));
#145610=CARTESIAN_POINT('Ctrl Pts',(20.5734268285343,-17.1695366142654,
5.26874180128035));
#145611=CARTESIAN_POINT('Ctrl Pts',(20.6310193783568,-17.2309567312121,
5.27291151560072));
#145612=CARTESIAN_POINT('Ctrl Pts',(20.6854509703006,-17.2950633353948,
5.2770812299211));
#145613=CARTESIAN_POINT('Ctrl Pts',(20.7398806253347,-17.3591676583894,
5.28125079586514));
#145614=CARTESIAN_POINT('Ctrl Pts',(20.7911492490277,-17.4259579273212,
5.28542036180918));
#145615=CARTESIAN_POINT('Ctrl Pts',(20.838993044898,-17.4950839828834,5.28958992775322));
#145616=CARTESIAN_POINT('Ctrl Pts',(20.8885189696096,-17.566640425283,5.29390609049214));
#145617=CARTESIAN_POINT('Ctrl Pts',(20.934374451502,-17.6406995292214,5.29822225323106));
#145618=CARTESIAN_POINT('Ctrl Pts',(20.9763163009699,-17.7168410602662,
5.30253841596997));
#145619=CARTESIAN_POINT('Ctrl Pts',(21.016891899103,-17.7905022889458,5.30671398016165));
#145620=CARTESIAN_POINT('Ctrl Pts',(21.0538047581692,-17.8661119140599,
5.31088954435333));
#145621=CARTESIAN_POINT('Ctrl Pts',(21.0868828170839,-17.9432669089043,
5.31506510854501));
#145622=CARTESIAN_POINT('Ctrl Pts',(21.1216315701187,-18.0243188191198,
5.31945157055755));
#145623=CARTESIAN_POINT('Ctrl Pts',(21.1521477486479,-18.1070757672225,
5.32383803257009));
#145624=CARTESIAN_POINT('Ctrl Pts',(21.1782909617847,-18.1910521081326,
5.32822449458263));
#145625=CARTESIAN_POINT('Ctrl Pts',(21.2044341749215,-18.2750284490427,
5.33261095659517));
#145626=CARTESIAN_POINT('Ctrl Pts',(21.226204352714,-18.3602236017744,5.3369974186077));
#145627=CARTESIAN_POINT('Ctrl Pts',(21.2435233083642,-18.4461415565825,
5.34138388062024));
#145628=CARTESIAN_POINT('Ctrl Pts',(21.2600453931922,-18.528106298929,5.34556851501329));
#145629=CARTESIAN_POINT('Ctrl Pts',(21.2725783676242,-18.6110338790214,
5.34975314940634));
#145630=CARTESIAN_POINT('Ctrl Pts',(21.2810167729394,-18.6945013429835,
5.35393778379939));
#145631=CARTESIAN_POINT('Ctrl Pts',(21.2894431672291,-18.7778500013417,
5.35811646188332));
#145632=CARTESIAN_POINT('Ctrl Pts',(21.2937865229904,-18.8617365633854,
5.36229513996726));
#145633=CARTESIAN_POINT('Ctrl Pts',(21.293992315731,-18.945727568392,5.36647381805119));
#145634=CARTESIAN_POINT('Ctrl Pts',(21.2942017971586,-19.0312240518003,
5.37072739593663));
#145635=CARTESIAN_POINT('Ctrl Pts',(21.2901238296771,-19.1168282866476,
5.37498097382207));
#145636=CARTESIAN_POINT('Ctrl Pts',(21.2817561480521,-19.2020772082028,
5.37923455170751));
#145637=CARTESIAN_POINT('Ctrl Pts',(21.2735506902637,-19.2856734130641,
5.38340566568545));
#145638=CARTESIAN_POINT('Ctrl Pts',(21.2612204100085,-19.3689274796563,
5.3875767796634));
#145639=CARTESIAN_POINT('Ctrl Pts',(21.2448156932503,-19.4514041995498,
5.39174789364135));
#145640=CARTESIAN_POINT('Ctrl Pts',(21.2284164812532,-19.5338532435835,
5.39591760796173));
#145641=CARTESIAN_POINT('Ctrl Pts',(21.2079456377351,-19.6155250081441,
5.4000873222821));
#145642=CARTESIAN_POINT('Ctrl Pts',(21.1835049170499,-19.6959930519489,
5.40425703660247));
#145643=CARTESIAN_POINT('Ctrl Pts',(21.1590650660705,-19.7764582323552,
5.40842660254651));
#145644=CARTESIAN_POINT('Ctrl Pts',(21.1306557533067,-19.8557193372406,
5.41259616849056));
#145645=CARTESIAN_POINT('Ctrl Pts',(21.0984286192897,-19.9333650209193,
5.4167657344346));
#145646=CARTESIAN_POINT('Ctrl Pts',(21.065068418997,-20.0137406310499,5.42108189717352));
#145647=CARTESIAN_POINT('Ctrl Pts',(21.0276171353225,-20.092384622854,5.42539805991244));
#145648=CARTESIAN_POINT('Ctrl Pts',(20.9862964849993,-20.1688650474313,
5.42971422265136));
#145649=CARTESIAN_POINT('Ctrl Pts',(20.9463218505143,-20.2428541302222,
5.43388978684304));
#145650=CARTESIAN_POINT('Ctrl Pts',(20.9027263517807,-20.3148180591345,
5.43806535103473));
#145651=CARTESIAN_POINT('Ctrl Pts',(20.8557557370747,-20.3843940073146,
5.44224091522641));
#145652=CARTESIAN_POINT('Ctrl Pts',(20.8064127482818,-20.4574840712362,
5.44662737723895));
#145653=CARTESIAN_POINT('Ctrl Pts',(20.7533450801511,-20.5279381144878,
5.4510138392515));
#145654=CARTESIAN_POINT('Ctrl Pts',(20.6968850924154,-20.5953752200801,
5.45540030126404));
#145655=CARTESIAN_POINT('Ctrl Pts',(20.6404251046797,-20.6628123256725,
5.45978676327659));
#145656=CARTESIAN_POINT('Ctrl Pts',(20.5805732479924,-20.7272321203105,
5.46417322528913));
#145657=CARTESIAN_POINT('Ctrl Pts',(20.5177042670233,-20.788300380603,5.46855968730168));
#145658=CARTESIAN_POINT('Ctrl Pts',(20.4577251723804,-20.8465615279495,
5.47274451766067));
#145659=CARTESIAN_POINT('Ctrl Pts',(20.3947769753923,-20.9019893649409,
5.47692934801966));
#145660=CARTESIAN_POINT('Ctrl Pts',(20.3291582734039,-20.9542662367405,
5.48111417837865));
#145661=CARTESIAN_POINT('Ctrl Pts',(20.3173695655801,-20.9636580221449,
5.48186600279606));
#145662=CARTESIAN_POINT('Ctrl Pts',(20.3054947684578,-20.9729481955016,
5.48261782721348));
#145663=CARTESIAN_POINT('Ctrl Pts',(20.2935357468249,-20.9821350335323,
5.4833696516309));
#145664=CARTESIAN_POINT('Origin',(18.734,-18.952,-1.76670989022851));
#145665=CARTESIAN_POINT('',(20.2958869033725,-20.9851650055234,6.34984102531927));
#145666=CARTESIAN_POINT('',(20.2935357468249,-20.9821350335323,6.2833427999391));
#145667=CARTESIAN_POINT('',(20.2935357468249,-20.9821350335323,-1.76670989022851));
#145668=CARTESIAN_POINT('',(16.1740005630998,-18.9503020392334,5.8332901097715));
#145669=CARTESIAN_POINT('Ctrl Pts',(16.1712326851452,-18.9503002033939,
5.8332901097715));
#145670=CARTESIAN_POINT('Ctrl Pts',(16.1704460832798,-18.847523176255,5.83841759033362));
#145671=CARTESIAN_POINT('Ctrl Pts',(16.2227680109981,-17.8958349863275,
5.88593700645621));
#145672=CARTESIAN_POINT('Ctrl Pts',(17.4141948925089,-16.2277744127114,
5.97584835813928));
#145673=CARTESIAN_POINT('Ctrl Pts',(20.3102571282625,-16.3676811269119,
6.10302416482071));
#145674=CARTESIAN_POINT('Ctrl Pts',(21.731566457484,-18.8289532658523,6.22768838721405));
#145675=CARTESIAN_POINT('Ctrl Pts',(20.9266954653819,-20.4955799071986,
6.3099606740469));
#145676=CARTESIAN_POINT('Ctrl Pts',(20.2958869033725,-20.9851650055234,
6.34984102531927));
#145677=CARTESIAN_POINT('Ctrl Pts',(20.2935357468249,-20.9821350335323,
5.54983331705304));
#145678=CARTESIAN_POINT('Ctrl Pts',(20.2268225019857,-21.0333836886193,
5.55400789577091));
#145679=CARTESIAN_POINT('Ctrl Pts',(20.157617582879,-21.0813119452572,5.55818247448878));
#145680=CARTESIAN_POINT('Ctrl Pts',(20.0862916035558,-21.12568521616,5.56235705320665));
#145681=CARTESIAN_POINT('Ctrl Pts',(20.0149229753758,-21.1700850197413,
5.56653412808387));
#145682=CARTESIAN_POINT('Ctrl Pts',(19.9414311643003,-21.2109253827401,
5.57071120296108));
#145683=CARTESIAN_POINT('Ctrl Pts',(19.8662111471552,-21.2480178392725,
5.5748882778383));
#145684=CARTESIAN_POINT('Ctrl Pts',(19.7908651826575,-21.2851724028993,
5.57907234675171));
#145685=CARTESIAN_POINT('Ctrl Pts',(19.7137856568982,-21.3185663488317,
5.58325641566512));
#145686=CARTESIAN_POINT('Ctrl Pts',(19.6353869037669,-21.3480596089658,
5.58744048457852));
#145687=CARTESIAN_POINT('Ctrl Pts',(19.5924128683777,-21.3642262487927,
5.58973396908401));
#145688=CARTESIAN_POINT('Ctrl Pts',(19.5490427171948,-21.3792217476382,
5.5920274535895));
#145689=CARTESIAN_POINT('Ctrl Pts',(19.5053461655913,-21.393029514944,5.59432093809498));
#145690=CARTESIAN_POINT('Ctrl Pts',(19.4256185318269,-21.4182228213827,
5.59850557248803));
#145691=CARTESIAN_POINT('Ctrl Pts',(19.3445069543659,-21.4395528703719,
5.60269020688108));
#145692=CARTESIAN_POINT('Ctrl Pts',(19.2624206826503,-21.4568695738795,
5.60687484127413));
#145693=CARTESIAN_POINT('Ctrl Pts',(19.1804512505824,-21.4741616292031,
5.61105351935807));
#145694=CARTESIAN_POINT('Ctrl Pts',(19.0975103262626,-21.4874515917235,
5.61523219744201));
#145695=CARTESIAN_POINT('Ctrl Pts',(19.0140230530431,-21.4966388918203,
5.61941087552596));
#145696=CARTESIAN_POINT('Ctrl Pts',(18.9290393304524,-21.5059908676686,
5.62366445341139));
#145697=CARTESIAN_POINT('Ctrl Pts',(18.8434899394336,-21.511091508697,5.62791803129683));
#145698=CARTESIAN_POINT('Ctrl Pts',(18.7578350465905,-21.5118890387191,
5.63217160918226));
#145699=CARTESIAN_POINT('Ctrl Pts',(18.6738407409869,-21.5126711070654,
5.63634272316022));
#145700=CARTESIAN_POINT('Ctrl Pts',(18.5897454689696,-21.5093154194064,
5.64051383713817));
#145701=CARTESIAN_POINT('Ctrl Pts',(18.5059873315595,-21.5018255279589,
5.64468495111612));
#145702=CARTESIAN_POINT('Ctrl Pts',(18.4222573000012,-21.4943381498168,
5.64885466543649));
#145703=CARTESIAN_POINT('Ctrl Pts',(18.3388646361978,-21.4827193639703,
5.65302437975686));
#145704=CARTESIAN_POINT('Ctrl Pts',(18.2562442180635,-21.4670247340387,
5.65719409407724));
#145705=CARTESIAN_POINT('Ctrl Pts',(18.1736267399183,-21.4513306625893,
5.66136366002128));
#145706=CARTESIAN_POINT('Ctrl Pts',(18.091781904597,-21.4315611221137,5.66553322596532));
#145707=CARTESIAN_POINT('Ctrl Pts',(18.0111349162339,-21.4078228907378,
5.66970279190937));
#145708=CARTESIAN_POINT('Ctrl Pts',(17.9276524792488,-21.383250052431,5.67401895464829));
#145709=CARTESIAN_POINT('Ctrl Pts',(17.8454541950082,-21.3544244012909,
5.67833511738721));
#145710=CARTESIAN_POINT('Ctrl Pts',(17.7649932472175,-21.3215201862533,
5.68265128012613));
#145711=CARTESIAN_POINT('Ctrl Pts',(17.687153306338,-21.2896878225596,5.68682684431781));
#145712=CARTESIAN_POINT('Ctrl Pts',(17.6109396593039,-21.2540387751657,
5.69100240850949));
#145713=CARTESIAN_POINT('Ctrl Pts',(17.5367393343474,-21.2147785791988,
5.69517797270117));
#145714=CARTESIAN_POINT('Ctrl Pts',(17.4587913273718,-21.1735354440659,
5.69956443471371));
#145715=CARTESIAN_POINT('Ctrl Pts',(17.3830658746253,-21.1283070744552,
5.70395089672625));
#145716=CARTESIAN_POINT('Ctrl Pts',(17.3099772536614,-21.0793831854911,
5.70833735873879));
#145717=CARTESIAN_POINT('Ctrl Pts',(17.2368886326976,-21.030459296527,5.71272382075133));
#145718=CARTESIAN_POINT('Ctrl Pts',(17.166437262867,-20.9778402963549,5.71711028276386));
#145719=CARTESIAN_POINT('Ctrl Pts',(17.0989955289256,-20.9218630357379,
5.72149674477641));
#145720=CARTESIAN_POINT('Ctrl Pts',(17.0355419517776,-20.8691959820086,
5.72562381401755));
#145721=CARTESIAN_POINT('Ctrl Pts',(16.9745020021859,-20.8133485129554,
5.72975088325869));
#145722=CARTESIAN_POINT('Ctrl Pts',(16.9162185170907,-20.7545732940416,
5.73387795249984));
#145723=CARTESIAN_POINT('Ctrl Pts',(16.8577217299027,-20.6955829734197,
5.73802012571949));
#145724=CARTESIAN_POINT('Ctrl Pts',(16.8020020379165,-20.6336436795684,
5.74216229893914));
#145725=CARTESIAN_POINT('Ctrl Pts',(16.7493744028763,-20.5690532580101,
5.7463044721588));
#145726=CARTESIAN_POINT('Ctrl Pts',(16.6970742796337,-20.5048647949489,
5.75042086784547));
#145727=CARTESIAN_POINT('Ctrl Pts',(16.6478281605157,-20.4380584608901,
5.75453726353214));
#145728=CARTESIAN_POINT('Ctrl Pts',(16.6019085746493,-20.3689637094668,
5.75865365921882));
#145729=CARTESIAN_POINT('Ctrl Pts',(16.5560170315913,-20.2999111537828,
5.76276754104799));
#145730=CARTESIAN_POINT('Ctrl Pts',(16.5134482524877,-20.2285733472958,
5.76688142287716));
#145731=CARTESIAN_POINT('Ctrl Pts',(16.4744330306069,-20.1553108953332,
5.77099530470634));
#145732=CARTESIAN_POINT('Ctrl Pts',(16.4354291736147,-20.0820697842618,
5.77510798818763));
#145733=CARTESIAN_POINT('Ctrl Pts',(16.3999770407453,-20.0069055590536,
5.77922067166892));
#145734=CARTESIAN_POINT('Ctrl Pts',(16.3682620211175,-19.9302043831803,
5.78333335515021));
#145735=CARTESIAN_POINT('Ctrl Pts',(16.3361584999705,-19.852563635971,5.78749641803532));
#145736=CARTESIAN_POINT('Ctrl Pts',(16.3078844956127,-19.7733484709671,
5.79165948092042));
#145737=CARTESIAN_POINT('Ctrl Pts',(16.2835818660734,-19.6929797358388,
5.79582254380553));
#145738=CARTESIAN_POINT('Ctrl Pts',(16.2595524301165,-19.6135144512041,
5.79993880837768));
#145739=CARTESIAN_POINT('Ctrl Pts',(16.2394055983612,-19.5329218806178,
5.80405507294983));
#145740=CARTESIAN_POINT('Ctrl Pts',(16.2232275631065,-19.4516216269696,
5.80817133752197));
#145741=CARTESIAN_POINT('Ctrl Pts',(16.2067736327737,-19.3689349046017,
5.81235779956356));
#145742=CARTESIAN_POINT('Ctrl Pts',(16.1944252132089,-19.2855166404035,
5.81654426160515));
#145743=CARTESIAN_POINT('Ctrl Pts',(16.186218055036,-19.2018142528269,5.82073072364674));
#145744=CARTESIAN_POINT('Ctrl Pts',(16.1780108968631,-19.1181118652502,
5.82491718568833));
#145745=CARTESIAN_POINT('Ctrl Pts',(16.1739449655996,-19.0341258661345,
5.82910364772991));
#145746=CARTESIAN_POINT('Ctrl Pts',(16.1740005630998,-18.9503020392334,
5.8332901097715));
#145747=CARTESIAN_POINT('',(16.1740007055014,-18.9539005700932,5.76670989019962));
#145748=CARTESIAN_POINT('Ctrl Pts',(20.2935357468249,-20.9821350335323,
5.4833696516309));
#145749=CARTESIAN_POINT('Ctrl Pts',(20.2270815882697,-21.0331846603208,
5.48754740634818));
#145750=CARTESIAN_POINT('Ctrl Pts',(20.1580239132524,-21.0810403461138,
5.49172516106546));
#145751=CARTESIAN_POINT('Ctrl Pts',(20.0867037291457,-21.1254287706652,
5.49590291578274));
#145752=CARTESIAN_POINT('Ctrl Pts',(20.015460353698,-21.1697693908621,5.50007617124442));
#145753=CARTESIAN_POINT('Ctrl Pts',(19.9419597007997,-21.2106499296345,
5.5042494267061));
#145754=CARTESIAN_POINT('Ctrl Pts',(19.8665733495297,-21.2478391947031,
5.50842268216778));
#145755=CARTESIAN_POINT('Ctrl Pts',(19.7912312733654,-21.2850066181702,
5.51259348663769));
#145756=CARTESIAN_POINT('Ctrl Pts',(19.7140061091704,-21.3184868690186,
5.51676429110759));
#145757=CARTESIAN_POINT('Ctrl Pts',(19.635294757175,-21.3480942720788,5.5209350955775));
#145758=CARTESIAN_POINT('Ctrl Pts',(19.556606021274,-21.3776931680583,5.52510470165219));
#145759=CARTESIAN_POINT('Ctrl Pts',(19.4764323760497,-21.4034212646175,
5.52927430772688));
#145760=CARTESIAN_POINT('Ctrl Pts',(19.3951901898219,-21.4251412278484,
5.53344391380158));
#145761=CARTESIAN_POINT('Ctrl Pts',(19.3139469762852,-21.4468614657285,
5.53761357260102));
#145762=CARTESIAN_POINT('Ctrl Pts',(19.2316356396825,-21.4645733520643,
5.54178323140045));
#145763=CARTESIAN_POINT('Ctrl Pts',(19.1486858492173,-21.4781899466309,
5.54595289019989));
#145764=CARTESIAN_POINT('Ctrl Pts',(19.0656524537254,-21.4918202653521,
5.55012675159506));
#145765=CARTESIAN_POINT('Ctrl Pts',(18.9819797739384,-21.5013469721866,
5.55430061299022));
#145766=CARTESIAN_POINT('Ctrl Pts',(18.8981053133176,-21.5067347114996,
5.55847447438539));
#145767=CARTESIAN_POINT('Ctrl Pts',(18.8141902491749,-21.5121250590105,
5.56265035634165));
#145768=CARTESIAN_POINT('Ctrl Pts',(18.7300736701582,-21.5133724406709,
5.56682623829792));
#145769=CARTESIAN_POINT('Ctrl Pts',(18.6461933463466,-21.5104936958246,
5.57100212025418));
#145770=CARTESIAN_POINT('Ctrl Pts',(18.562161458039,-21.5076097493351,5.57518554766825));
#145771=CARTESIAN_POINT('Ctrl Pts',(18.4783671375726,-21.5005848165362,
5.57936897508233));
#145772=CARTESIAN_POINT('Ctrl Pts',(18.3952432446133,-21.4894877065081,
5.5835524024964));
#145773=CARTESIAN_POINT('Ctrl Pts',(18.3145513547331,-21.4787152709484,
5.58761343299197));
#145774=CARTESIAN_POINT('Ctrl Pts',(18.2344915683268,-21.4641058135859,
5.59167446348754));
#145775=CARTESIAN_POINT('Ctrl Pts',(18.1554472698611,-21.4457675790757,
5.59573549398311));
#145776=CARTESIAN_POINT('Ctrl Pts',(18.073997132933,-21.4268711913427,5.59992012837615));
#145777=CARTESIAN_POINT('Ctrl Pts',(17.9933221701874,-21.4039450190917,
5.60410476276919));
#145778=CARTESIAN_POINT('Ctrl Pts',(17.9138510440901,-21.3770681825714,
5.60828939716224));
#145779=CARTESIAN_POINT('Ctrl Pts',(17.8344930353044,-21.3502296019012,
5.61246807524617));
#145780=CARTESIAN_POINT('Ctrl Pts',(17.7563358916503,-21.3194516726889,
5.6166467533301));
#145781=CARTESIAN_POINT('Ctrl Pts',(17.6797967513082,-21.2848642288928,
5.62082543141404));
#145782=CARTESIAN_POINT('Ctrl Pts',(17.6018857018828,-21.2496568300241,
5.62507900929947));
#145783=CARTESIAN_POINT('Ctrl Pts',(17.5256517013921,-21.2105021111289,
5.62933258718491));
#145784=CARTESIAN_POINT('Ctrl Pts',(17.4515171985772,-21.1675897327923,
5.63358616507035));
#145785=CARTESIAN_POINT('Ctrl Pts',(17.378819937761,-21.1255092946465,5.6377572790483));
#145786=CARTESIAN_POINT('Ctrl Pts',(17.3081419118304,-21.0798158370634,
5.64192839302626));
#145787=CARTESIAN_POINT('Ctrl Pts',(17.2398584137968,-21.03073541375,5.64609950700422));
#145788=CARTESIAN_POINT('Ctrl Pts',(17.1715978289504,-20.9816714598466,
5.65026922132459));
#145789=CARTESIAN_POINT('Ctrl Pts',(17.105730549462,-20.929223065652,5.65443893564497));
#145790=CARTESIAN_POINT('Ctrl Pts',(17.0426026198917,-20.8736594137783,
5.65860864996535));
#145791=CARTESIAN_POINT('Ctrl Pts',(16.979476936684,-20.8180977390978,5.66277821590939));
#145792=CARTESIAN_POINT('Ctrl Pts',(16.9190907543433,-20.7594213317294,
5.66694778185343));
#145793=CARTESIAN_POINT('Ctrl Pts',(16.8617557221019,-20.6979385338201,
5.67111734779747));
#145794=CARTESIAN_POINT('Ctrl Pts',(16.8024048608573,-20.6342940765834,
5.67543351053639));
#145795=CARTESIAN_POINT('Ctrl Pts',(16.7463240583281,-20.5676425973542,
5.67974967327531));
#145796=CARTESIAN_POINT('Ctrl Pts',(16.6938147044707,-20.4983647564227,
5.68406583601423));
#145797=CARTESIAN_POINT('Ctrl Pts',(16.6430158372923,-20.4313436338728,
5.68824140020591));
#145798=CARTESIAN_POINT('Ctrl Pts',(16.595559538813,-20.36186504502,5.6924169643976));
#145799=CARTESIAN_POINT('Ctrl Pts',(16.5516743299492,-20.2903029066087,
5.69659252858928));
#145800=CARTESIAN_POINT('Ctrl Pts',(16.5055725835129,-20.215126334709,5.70097899060182));
#145801=CARTESIAN_POINT('Ctrl Pts',(16.4634124379743,-20.1376507144179,
5.70536545261436));
#145802=CARTESIAN_POINT('Ctrl Pts',(16.4254030213235,-20.0583362915703,
5.70975191462691));
#145803=CARTESIAN_POINT('Ctrl Pts',(16.3873936046727,-19.9790218687227,
5.71413837663945));
#145804=CARTESIAN_POINT('Ctrl Pts',(16.3535350701226,-19.897869208087,5.718524838652));
#145805=CARTESIAN_POINT('Ctrl Pts',(16.323976493569,-19.8153578044185,5.72291130066454));
#145806=CARTESIAN_POINT('Ctrl Pts',(16.2911969765866,-19.7238552940422,
5.72777574688618));
#145807=CARTESIAN_POINT('Ctrl Pts',(16.2636032939182,-19.630402505787,5.73264019310782));
#145808=CARTESIAN_POINT('Ctrl Pts',(16.2413973788046,-19.5355513454785,
5.73750463932946));
#145809=CARTESIAN_POINT('Ctrl Pts',(16.2191773325018,-19.4406398246901,
5.74237218114115));
#145810=CARTESIAN_POINT('Ctrl Pts',(16.2023520711407,-19.3443282665182,
5.74723972295285));
#145811=CARTESIAN_POINT('Ctrl Pts',(16.1910760934491,-19.2471914725933,
5.75210726476454));
#145812=CARTESIAN_POINT('Ctrl Pts',(16.1798001157575,-19.1500546786684,
5.75697480657623));
#145813=CARTESIAN_POINT('Ctrl Pts',(16.1740736044194,-19.0520927805192,
5.76184234838793));
#145814=CARTESIAN_POINT('Ctrl Pts',(16.1740007055014,-18.9539005700933,
5.76670989019962));
#145815=CARTESIAN_POINT('Ctrl Pts',(16.174000705501,-18.9539005695105,5.76670989022851));
#145816=CARTESIAN_POINT('Ctrl Pts',(16.1739381768052,-18.8696766480678,
5.77088500205647));
#145817=CARTESIAN_POINT('Ctrl Pts',(16.1780364138872,-18.7854119279347,
5.77506011388444));
#145818=CARTESIAN_POINT('Ctrl Pts',(16.1862808495761,-18.7015461508315,
5.7792352257124));
#145819=CARTESIAN_POINT('Ctrl Pts',(16.1945245019764,-18.617688341661,5.78340994087069));
#145820=CARTESIAN_POINT('Ctrl Pts',(16.2069135252697,-18.5342298557721,
5.78758465602899));
#145821=CARTESIAN_POINT('Ctrl Pts',(16.2233814427541,-18.4516056954636,
5.79175937118728));
#145822=CARTESIAN_POINT('Ctrl Pts',(16.2398526754154,-18.3689649019825,
5.79593492676267));
#145823=CARTESIAN_POINT('Ctrl Pts',(16.2604043427349,-18.2871592164315,
5.80011048233807));
#145824=CARTESIAN_POINT('Ctrl Pts',(16.2849190524512,-18.2066125085881,
5.80428603791346));
#145825=CARTESIAN_POINT('Ctrl Pts',(16.3094630809747,-18.1259694694634,
5.80846658731951));
#145826=CARTESIAN_POINT('Ctrl Pts',(16.3379794801119,-18.0465888526479,
5.81264713672555));
#145827=CARTESIAN_POINT('Ctrl Pts',(16.370301376024,-17.9688780263803,5.8168276861316));
#145828=CARTESIAN_POINT('Ctrl Pts',(16.4026440716432,-17.8911171918327,
5.82101092579452));
#145829=CARTESIAN_POINT('Ctrl Pts',(16.4387969424267,-17.815028700182,5.82519416545745));
#145830=CARTESIAN_POINT('Ctrl Pts',(16.4785465454209,-17.7409964020585,
5.82937740512037));
#145831=CARTESIAN_POINT('Ctrl Pts',(16.5183679957913,-17.6668302906143,
5.8335682059857));
#145832=CARTESIAN_POINT('Ctrl Pts',(16.5617989238527,-17.5947281861652,
5.83775900685103));
#145833=CARTESIAN_POINT('Ctrl Pts',(16.6085819963934,-17.5250457926251,
5.84194980771636));
#145834=CARTESIAN_POINT('Ctrl Pts',(16.6388616407137,-17.4799449051204,
5.84466224092623));
#145835=CARTESIAN_POINT('Ctrl Pts',(16.67054468148,-17.4358570345709,5.8473746741361));
#145836=CARTESIAN_POINT('Ctrl Pts',(16.7035527014987,-17.392870830236,5.85008710734598));
#145837=CARTESIAN_POINT('Ctrl Pts',(16.754476165831,-17.3265534188316,5.85427174173903));
#145838=CARTESIAN_POINT('Ctrl Pts',(16.8087468503132,-17.262610070515,5.85845637613208));
#145839=CARTESIAN_POINT('Ctrl Pts',(16.8661152556942,-17.2013982228989,
5.86264101052513));
#145840=CARTESIAN_POINT('Ctrl Pts',(16.9234020042509,-17.1402735027714,
5.86681968860908));
#145841=CARTESIAN_POINT('Ctrl Pts',(16.9837774037106,-17.0818728934346,
5.87099836669302));
#145842=CARTESIAN_POINT('Ctrl Pts',(17.0469505633859,-17.0265223453854,
5.87517704477697));
#145843=CARTESIAN_POINT('Ctrl Pts',(17.1112560565466,-16.9701796785422,
5.87943062266241));
#145844=CARTESIAN_POINT('Ctrl Pts',(17.1784603025304,-16.9169978755986,
5.88368420054784));
#145845=CARTESIAN_POINT('Ctrl Pts',(17.2482157539324,-16.8672829510609,
5.88793777843328));
#145846=CARTESIAN_POINT('Ctrl Pts',(17.3166188597925,-16.818531847346,5.89210889241123));
#145847=CARTESIAN_POINT('Ctrl Pts',(17.3874747417498,-16.773114676503,5.89628000638918));
#145848=CARTESIAN_POINT('Ctrl Pts',(17.4604222489457,-16.7312794610714,
5.90045112036713));
#145849=CARTESIAN_POINT('Ctrl Pts',(17.5333452779011,-16.6894582838502,
5.9046208346875));
#145850=CARTESIAN_POINT('Ctrl Pts',(17.6083581394479,-16.6512169036012,
5.90879054900788));
#145851=CARTESIAN_POINT('Ctrl Pts',(17.6850725337916,-16.6167588624226,
5.91296026332825));
#145852=CARTESIAN_POINT('Ctrl Pts',(17.7617841983079,-16.582302047409,5.9171298292723));
#145853=CARTESIAN_POINT('Ctrl Pts',(17.8401968552436,-16.5516284915071,
5.92129939521634));
#145854=CARTESIAN_POINT('Ctrl Pts',(17.9199008000001,-16.5248942147983,
5.92546896116039));
#145855=CARTESIAN_POINT('Ctrl Pts',(18.0024070371288,-16.4972199939007,
5.92978512389931));
#145856=CARTESIAN_POINT('Ctrl Pts',(18.0862965548759,-16.4737673840696,
5.93410128663823));
#145857=CARTESIAN_POINT('Ctrl Pts',(18.1710980677306,-16.4546531248848,
5.93841744937714));
#145858=CARTESIAN_POINT('Ctrl Pts',(18.2531371802236,-16.4361615106825,
5.94259301356882));
#145859=CARTESIAN_POINT('Ctrl Pts',(18.3360293116304,-16.4217299783601,
5.9467685777605));
#145860=CARTESIAN_POINT('Ctrl Pts',(18.4193394847883,-16.411411729507,5.95094414195217));
#145861=CARTESIAN_POINT('Ctrl Pts',(18.5068574567414,-16.4005723304336,
5.95533060396471));
#145862=CARTESIAN_POINT('Ctrl Pts',(18.5948362284719,-16.3942727005953,
5.95971706597725));
#145863=CARTESIAN_POINT('Ctrl Pts',(18.682770269855,-16.3925126461048,5.96410352798979));
#145864=CARTESIAN_POINT('Ctrl Pts',(18.7707043112381,-16.3907525916143,
5.96848999000233));
#145865=CARTESIAN_POINT('Ctrl Pts',(18.8585930447509,-16.3935320181048,
5.97287645201487));
#145866=CARTESIAN_POINT('Ctrl Pts',(18.9459382820312,-16.4007880988421,
5.97726291402741));
#145867=CARTESIAN_POINT('Ctrl Pts',(19.0292646354676,-16.4077103165486,
5.98144754842046));
#145868=CARTESIAN_POINT('Ctrl Pts',(19.1124065643328,-16.4187320520138,
5.9856321828135));
#145869=CARTESIAN_POINT('Ctrl Pts',(19.1949284709478,-16.4338369900521,
5.98981681720655));
#145870=CARTESIAN_POINT('Ctrl Pts',(19.2773329178427,-16.4489204280808,
5.99399549529048));
#145871=CARTESIAN_POINT('Ctrl Pts',(19.3591186468153,-16.4680754422333,
5.99817417337441));
#145872=CARTESIAN_POINT('Ctrl Pts',(19.4398541314688,-16.491233870298,6.00235285145835));
#145873=CARTESIAN_POINT('Ctrl Pts',(19.5220367416614,-16.5148073965422,
6.00660642934378));
#145874=CARTESIAN_POINT('Ctrl Pts',(19.6031306054559,-16.5425292308513,
6.01086000722922));
#145875=CARTESIAN_POINT('Ctrl Pts',(19.682690292262,-16.5742727807068,6.01511358511466));
#145876=CARTESIAN_POINT('Ctrl Pts',(19.7607075592913,-16.6054009199058,
6.01928469909261));
#145877=CARTESIAN_POINT('Ctrl Pts',(19.8372491575625,-16.6403960502729,
6.02345581307056));
#145878=CARTESIAN_POINT('Ctrl Pts',(19.9119110552604,-16.6790887509858,
6.02762692704851));
#145879=CARTESIAN_POINT('Ctrl Pts',(19.9865478994375,-16.7177684679893,
6.03179664136888));
#145880=CARTESIAN_POINT('Ctrl Pts',(20.059305887621,-16.7601430796837,6.03596635568925));
#145881=CARTESIAN_POINT('Ctrl Pts',(20.1298036938035,-16.805996260869,6.04013607000962));
#145882=CARTESIAN_POINT('Ctrl Pts',(20.2002989913718,-16.8518478104014,
6.04430563595367));
#145883=CARTESIAN_POINT('Ctrl Pts',(20.2685338816756,-16.9011774317726,
6.04847520189772));
#145884=CARTESIAN_POINT('Ctrl Pts',(20.3341554111886,-16.9537250789634,
6.05264476784177));
#145885=CARTESIAN_POINT('Ctrl Pts',(20.4020841127263,-17.0081202366048,
6.0569609305807));
#145886=CARTESIAN_POINT('Ctrl Pts',(20.4672118510044,-17.0659635923385,
6.06127709331962));
#145887=CARTESIAN_POINT('Ctrl Pts',(20.5291853686021,-17.1269220585529,
6.06559325605854));
#145888=CARTESIAN_POINT('Ctrl Pts',(20.5891401053826,-17.185894809142,6.06976882025022));
#145889=CARTESIAN_POINT('Ctrl Pts',(20.6461426787832,-17.2477824589604,
6.07394438444191));
#145890=CARTESIAN_POINT('Ctrl Pts',(20.6999129097985,-17.3122480580625,
6.07811994863359));
#145891=CARTESIAN_POINT('Ctrl Pts',(20.7563989473557,-17.3799696613228,
6.08250641064613));
#145892=CARTESIAN_POINT('Ctrl Pts',(20.8093171796,-17.4505360152562,6.08689287265867));
#145893=CARTESIAN_POINT('Ctrl Pts',(20.8583941356916,-17.523521944082,6.09127933467122));
#145894=CARTESIAN_POINT('Ctrl Pts',(20.9074710917831,-17.5965078729078,
6.09566579668376));
#145895=CARTESIAN_POINT('Ctrl Pts',(20.9527065384673,-17.6719128399418,
6.1000522586963));
#145896=CARTESIAN_POINT('Ctrl Pts',(20.9938836431733,-17.7492839406918,
6.10443872070884));
#145897=CARTESIAN_POINT('Ctrl Pts',(21.0331661282526,-17.8230950824048,
6.10862335510189));
#145898=CARTESIAN_POINT('Ctrl Pts',(21.0689017421373,-17.8989701434485,
6.11280798949494));
#145899=CARTESIAN_POINT('Ctrl Pts',(21.1008684225542,-17.9765340240092,
6.11699262388799));
#145900=CARTESIAN_POINT('Ctrl Pts',(21.1327896023583,-18.0539875019864,
6.12117130197193));
#145901=CARTESIAN_POINT('Ctrl Pts',(21.1609523307066,-18.1331246030375,
6.12534998005586));
#145902=CARTESIAN_POINT('Ctrl Pts',(21.1851803441782,-18.2135455868408,
6.1295286581398));
#145903=CARTESIAN_POINT('Ctrl Pts',(21.209842627379,-18.2954080589815,6.13378223602524));
#145904=CARTESIAN_POINT('Ctrl Pts',(21.2304275222057,-18.3786004681758,
6.13803581391068));
#145905=CARTESIAN_POINT('Ctrl Pts',(21.2468003698022,-18.462679755659,6.14228939179611));
#145906=CARTESIAN_POINT('Ctrl Pts',(21.2628557977991,-18.5451290020871,
6.14646050577407));
#145907=CARTESIAN_POINT('Ctrl Pts',(21.2748609466778,-18.6284305735953,
6.15063161975202));
#145908=CARTESIAN_POINT('Ctrl Pts',(21.2827395777799,-18.7121530390886,
6.15480273372997));
#145909=CARTESIAN_POINT('Ctrl Pts',(21.2906155651312,-18.7958474107,6.15897244805034));
#145910=CARTESIAN_POINT('Ctrl Pts',(21.2943677416632,-18.8799619381733,
6.16314216237071));
#145911=CARTESIAN_POINT('Ctrl Pts',(21.2939715980996,-18.9640588939544,
6.16731187669109));
#145912=CARTESIAN_POINT('Ctrl Pts',(21.2935754686325,-19.0481528572048,
6.17148144263512));
#145913=CARTESIAN_POINT('Ctrl Pts',(21.2890313155855,-19.1322287899825,
6.17565100857916));
#145914=CARTESIAN_POINT('Ctrl Pts',(21.2803667494582,-19.2158491562499,
6.1798205745232));
#145915=CARTESIAN_POINT('Ctrl Pts',(21.2713975478748,-19.3024095114386,
6.18413673726212));
#145916=CARTESIAN_POINT('Ctrl Pts',(21.2580128490968,-19.3884811440151,
6.18845290000104));
#145917=CARTESIAN_POINT('Ctrl Pts',(21.2403015155519,-19.4735867263861,
6.19276906273997));
#145918=CARTESIAN_POINT('Ctrl Pts',(21.2231671268343,-19.5559200033628,
6.19694462693165));
#145919=CARTESIAN_POINT('Ctrl Pts',(21.2019838191124,-19.6373487577945,
6.20112019112333));
#145920=CARTESIAN_POINT('Ctrl Pts',(21.1768832583853,-19.7174550188619,
6.20529575531501));
#145921=CARTESIAN_POINT('Ctrl Pts',(21.1505149280068,-19.8016072567413,
6.20968221732755));
#145922=CARTESIAN_POINT('Ctrl Pts',(21.1198234271566,-19.8842993445544,
6.2140686793401));
#145923=CARTESIAN_POINT('Ctrl Pts',(21.085018236802,-19.9650711970166,6.21845514135264));
#145924=CARTESIAN_POINT('Ctrl Pts',(21.0502130464473,-20.0458430494787,
6.22284160336519));
#145925=CARTESIAN_POINT('Ctrl Pts',(21.0112944915985,-20.1246941799627,
6.22722806537773));
#145926=CARTESIAN_POINT('Ctrl Pts',(20.9685260259017,-20.2011971179794,
6.23161452739028));
#145927=CARTESIAN_POINT('Ctrl Pts',(20.926496351346,-20.2763785287457,6.23592521676934));
#145928=CARTESIAN_POINT('Ctrl Pts',(20.8805876001805,-20.3495805638946,
6.24023590614841));
#145929=CARTESIAN_POINT('Ctrl Pts',(20.8310139355987,-20.420377524312,6.24454659552748));
#145930=CARTESIAN_POINT('Ctrl Pts',(20.7829663020667,-20.4889951348523,
6.24872458852646));
#145931=CARTESIAN_POINT('Ctrl Pts',(20.7314763645207,-20.555353152089,6.25290258152543));
#145932=CARTESIAN_POINT('Ctrl Pts',(20.6767860610052,-20.6190879764319,
6.25708057452441));
#145933=CARTESIAN_POINT('Ctrl Pts',(20.6194902461936,-20.6858592038318,
6.26145761209352));
#145934=CARTESIAN_POINT('Ctrl Pts',(20.5586817759822,-20.7497506182763,
6.26583464966264));
#145935=CARTESIAN_POINT('Ctrl Pts',(20.4946892619671,-20.8103792193182,
6.27021168723176));
#145936=CARTESIAN_POINT('Ctrl Pts',(20.430696747952,-20.8710078203602,6.27458872480087));
#145937=CARTESIAN_POINT('Ctrl Pts',(20.363520576587,-20.9283731694461,6.27896576236998));
#145938=CARTESIAN_POINT('Ctrl Pts',(20.2935357468249,-20.9821350335323,
6.2833427999391));
#145939=CARTESIAN_POINT('Origin',(18.734,-18.952,-1.76670989022851));
#145940=CARTESIAN_POINT('',(20.2935357468249,-20.9821350335323,7.14996297925329));
#145941=CARTESIAN_POINT('',(20.2935357468249,-20.9821350335323,7.08324142646255));
#145942=CARTESIAN_POINT('',(20.2935357468249,-20.9821350335323,-1.76670989022851));
#145943=CARTESIAN_POINT('',(16.1740008768645,-18.954118854712,6.6332901097715));
#145944=CARTESIAN_POINT('Ctrl Pts',(16.1740008768645,-18.954118854712,6.6332901097715));
#145945=CARTESIAN_POINT('Ctrl Pts',(16.1739325519701,-18.8715687540989,
6.63740642252224));
#145946=CARTESIAN_POINT('Ctrl Pts',(16.1778613169669,-18.7888758591841,
6.64152273527298));
#145947=CARTESIAN_POINT('Ctrl Pts',(16.1858020059738,-18.7064659224448,
6.64563904802372));
#145948=CARTESIAN_POINT('Ctrl Pts',(16.1937337220434,-18.624149108506,6.64975070936243));
#145949=CARTESIAN_POINT('Ctrl Pts',(16.2056683130375,-18.5421150878493,
6.65386237070115));
#145950=CARTESIAN_POINT('Ctrl Pts',(16.2215685692311,-18.4607889397778,
6.65797403203986));
#145951=CARTESIAN_POINT('Ctrl Pts',(16.2374592000152,-18.3795120234588,
6.6620832043354));
#145952=CARTESIAN_POINT('Ctrl Pts',(16.2573106430753,-18.2989425946372,
6.66619237663094));
#145953=CARTESIAN_POINT('Ctrl Pts',(16.2810340922893,-18.219498630985,6.67030154892649));
#145954=CARTESIAN_POINT('Ctrl Pts',(16.3047507902538,-18.1400772755974,
6.67440955182854));
#145955=CARTESIAN_POINT('Ctrl Pts',(16.3323371713263,-18.0617812045222,
6.67851755473059));
#145956=CARTESIAN_POINT('Ctrl Pts',(16.3636541468014,-17.9850147176797,
6.68262555763264));
#145957=CARTESIAN_POINT('Ctrl Pts',(16.3949722554067,-17.9082454532245,
6.686733709173));
#145958=CARTESIAN_POINT('Ctrl Pts',(16.4300210447237,-17.8330063217983,
6.69084186071336));
#145959=CARTESIAN_POINT('Ctrl Pts',(16.4686133150906,-17.7596815996408,
6.69495001225373));
#145960=CARTESIAN_POINT('Ctrl Pts',(16.5072438266208,-17.6862842198592,
6.69906223457025));
#145961=CARTESIAN_POINT('Ctrl Pts',(16.5494246053548,-17.6148054564872,
6.70317445688677));
#145962=CARTESIAN_POINT('Ctrl Pts',(16.5949228757402,-17.5456042319217,
6.70728667920329));
#145963=CARTESIAN_POINT('Ctrl Pts',(16.6404458510681,-17.4763654320318,
6.71140113440064));
#145964=CARTESIAN_POINT('Ctrl Pts',(16.6892896206455,-17.4094070139063,
6.71551558959799));
#145965=CARTESIAN_POINT('Ctrl Pts',(16.7411800554791,-17.3450561090319,
6.71963004479534));
#145966=CARTESIAN_POINT('Ctrl Pts',(16.7931561866084,-17.2805989295773,
6.72375129495539));
#145967=CARTESIAN_POINT('Ctrl Pts',(16.8481887081044,-17.2187582108671,
6.72787254511545));
#145968=CARTESIAN_POINT('Ctrl Pts',(16.9059658904507,-17.1598249822285,
6.73199379527551));
#145969=CARTESIAN_POINT('Ctrl Pts',(16.9382542996129,-17.1268905239829,
6.73429692959297));
#145970=CARTESIAN_POINT('Ctrl Pts',(16.9713992632832,-17.0948633881751,
6.73660006391043));
#145971=CARTESIAN_POINT('Ctrl Pts',(17.0053421035808,-17.0637887096123,
6.73890319822789));
#145972=CARTESIAN_POINT('Ctrl Pts',(17.067013876621,-17.0073281863675,6.74308783262094));
#145973=CARTESIAN_POINT('Ctrl Pts',(17.1315694533285,-16.9537872066973,
6.74727246701399));
#145974=CARTESIAN_POINT('Ctrl Pts',(17.1987010234279,-16.9034744198481,
6.75145710140704));
#145975=CARTESIAN_POINT('Ctrl Pts',(17.2657370400464,-16.8532332470236,
6.75563577949098));
#145976=CARTESIAN_POINT('Ctrl Pts',(17.3353414020478,-16.8062114135714,
6.75981445757493));
#145977=CARTESIAN_POINT('Ctrl Pts',(17.4071710083241,-16.7626793686515,
6.76399313565888));
#145978=CARTESIAN_POINT('Ctrl Pts',(17.4802881086697,-16.7183670431123,
6.76824671354431));
#145979=CARTESIAN_POINT('Ctrl Pts',(17.5557106573433,-16.6776711711576,
6.77250029142975));
#145980=CARTESIAN_POINT('Ctrl Pts',(17.6330432222703,-16.6408327248832,
6.77675386931518));
#145981=CARTESIAN_POINT('Ctrl Pts',(17.7088765445241,-16.6047084637741,
6.78092498329313));
#145982=CARTESIAN_POINT('Ctrl Pts',(17.7865460506903,-16.5722936025649,
6.78509609727108));
#145983=CARTESIAN_POINT('Ctrl Pts',(17.8656529884826,-16.5437696398416,
6.78926721124903));
#145984=CARTESIAN_POINT('Ctrl Pts',(17.9447333811778,-16.5152552486095,
6.7934369255694));
#145985=CARTESIAN_POINT('Ctrl Pts',(18.0252498151565,-16.4906293187767,
6.79760663988977));
#145986=CARTESIAN_POINT('Ctrl Pts',(18.1067845307984,-16.4700248278449,
6.80177635421014));
#145987=CARTESIAN_POINT('Ctrl Pts',(18.1883163450853,-16.4494210701093,
6.80594592015419));
#145988=CARTESIAN_POINT('Ctrl Pts',(18.2708659227707,-16.4328385786397,
6.81011548609823));
#145989=CARTESIAN_POINT('Ctrl Pts',(18.3540026821446,-16.4203598126071,
6.81428505204228));
#145990=CARTESIAN_POINT('Ctrl Pts',(18.4400624274178,-16.407442308555,6.8186012147812));
#145991=CARTESIAN_POINT('Ctrl Pts',(18.5267508916658,-16.3989225513938,
6.82291737752012));
#145992=CARTESIAN_POINT('Ctrl Pts',(18.6135836740995,-16.3948336173693,
6.82723354025904));
#145993=CARTESIAN_POINT('Ctrl Pts',(18.6975878877786,-16.3908778799405,
6.83140910445072));
#145994=CARTESIAN_POINT('Ctrl Pts',(18.7817266907699,-16.3910686822566,
6.8355846686424));
#145995=CARTESIAN_POINT('Ctrl Pts',(18.8655624783154,-16.3953828377523,
6.83976023283408));
#145996=CARTESIAN_POINT('Ctrl Pts',(18.9536326121891,-16.3999148909862,
6.84414669484662));
#145997=CARTESIAN_POINT('Ctrl Pts',(19.0413677347563,-16.4089977253143,
6.84853315685916));
#145998=CARTESIAN_POINT('Ctrl Pts',(19.1282700391326,-16.4225433120446,
6.8529196188717));
#145999=CARTESIAN_POINT('Ctrl Pts',(19.2151723435089,-16.4360888987749,
6.85730608088424));
#146000=CARTESIAN_POINT('Ctrl Pts',(19.3012412773527,-16.4540970446291,
6.86169254289678));
#146001=CARTESIAN_POINT('Ctrl Pts',(19.3859971465594,-16.4764193164273,
6.86607900490932));
#146002=CARTESIAN_POINT('Ctrl Pts',(19.4668532725857,-16.4977145074105,
6.87026363930238));
#146003=CARTESIAN_POINT('Ctrl Pts',(19.5468154727232,-16.5230148144696,
6.87444827369543));
#146004=CARTESIAN_POINT('Ctrl Pts',(19.6254576099361,-16.5522284838579,
6.87863290808848));
#146005=CARTESIAN_POINT('Ctrl Pts',(19.7039878098006,-16.5814005712038,
6.88281158617243));
#146006=CARTESIAN_POINT('Ctrl Pts',(19.7812012513676,-16.6144747979098,
6.88699026425638));
#146007=CARTESIAN_POINT('Ctrl Pts',(19.8566848155709,-16.6513090592419,
6.89116894234032));
#146008=CARTESIAN_POINT('Ctrl Pts',(19.9335213684134,-16.688803548236,6.89542252022576));
#146009=CARTESIAN_POINT('Ctrl Pts',(20.0085649515612,-16.7301940721625,
6.89967609811119));
#146010=CARTESIAN_POINT('Ctrl Pts',(20.0813989057343,-16.7752785688504,
6.90392967599663));
#146011=CARTESIAN_POINT('Ctrl Pts',(20.1528208315821,-16.8194890145949,
6.90810078997458));
#146012=CARTESIAN_POINT('Ctrl Pts',(20.2221176306652,-16.8672512282388,
6.91227190395253));
#146013=CARTESIAN_POINT('Ctrl Pts',(20.2889208543458,-16.9183281639555,
6.91644301793049));
#146014=CARTESIAN_POINT('Ctrl Pts',(20.3557016615595,-16.9693879603131,
6.92061273225086));
#146015=CARTESIAN_POINT('Ctrl Pts',(20.4199901900087,-17.0237599905365,
6.92478244657124));
#146016=CARTESIAN_POINT('Ctrl Pts',(20.4814485012998,-17.0811649630966,
6.92895216089161));
#146017=CARTESIAN_POINT('Ctrl Pts',(20.5429046256404,-17.1385678929415,
6.93312172683566));
#146018=CARTESIAN_POINT('Ctrl Pts',(20.6015303974547,-17.1990032359004,
6.9372912927797));
#146019=CARTESIAN_POINT('Ctrl Pts',(20.6570234159163,-17.2621535744815,
6.94146085872375));
#146020=CARTESIAN_POINT('Ctrl Pts',(20.7144675004489,-17.3275242010627,
6.94577702146266));
#146021=CARTESIAN_POINT('Ctrl Pts',(20.7685540894613,-17.395803897787,6.95009318420158));
#146022=CARTESIAN_POINT('Ctrl Pts',(20.8189931741054,-17.4666032637932,
6.9544093469405));
#146023=CARTESIAN_POINT('Ctrl Pts',(20.8677892108726,-17.5350963478986,
6.95858491113218));
#146024=CARTESIAN_POINT('Ctrl Pts',(20.9131715145605,-17.6059470436349,
6.96276047532386));
#146025=CARTESIAN_POINT('Ctrl Pts',(20.9549227142454,-17.6787748442051,
6.96693603951554));
#146026=CARTESIAN_POINT('Ctrl Pts',(20.9987826677722,-17.7552810038503,
6.97132250152808));
#146027=CARTESIAN_POINT('Ctrl Pts',(21.0386347993093,-17.8339687234974,
6.97570896354062));
#146028=CARTESIAN_POINT('Ctrl Pts',(21.074283673631,-17.9143717780746,6.98009542555315));
#146029=CARTESIAN_POINT('Ctrl Pts',(21.1099325479527,-17.9947748326519,
6.98448188756569));
#146030=CARTESIAN_POINT('Ctrl Pts',(21.1413780286033,-18.0768926531098,
6.98886834957823));
#146031=CARTESIAN_POINT('Ctrl Pts',(21.1684852750765,-18.1602415485544,
6.99325481159076));
#146032=CARTESIAN_POINT('Ctrl Pts',(21.194345276957,-18.2397554377671,6.99743944598381));
#146033=CARTESIAN_POINT('Ctrl Pts',(21.216353744912,-18.320685570143,7.00162408037686));
#146034=CARTESIAN_POINT('Ctrl Pts',(21.2343571694271,-18.4026239673098,
7.00580871476991));
#146035=CARTESIAN_POINT('Ctrl Pts',(21.2523349682957,-18.48444573531,7.00998739285385));
#146036=CARTESIAN_POINT('Ctrl Pts',(21.2663189491972,-18.5672724719892,
7.01416607093779));
#146037=CARTESIAN_POINT('Ctrl Pts',(21.2762049862094,-18.650679890993,7.01834474902173));
#146038=CARTESIAN_POINT('Ctrl Pts',(21.2862682233301,-18.7355823280387,
7.02259832690716));
#146039=CARTESIAN_POINT('Ctrl Pts',(21.2920850111441,-18.8210860111296,
7.0268519047926));
#146040=CARTESIAN_POINT('Ctrl Pts',(21.2935997221946,-18.9067312233282,
7.03110548267803));
#146041=CARTESIAN_POINT('Ctrl Pts',(21.2950850676157,-18.9907160359654,
7.03527659665599));
#146042=CARTESIAN_POINT('Ctrl Pts',(21.2924336475012,-19.0748364579016,
7.03944771063394));
#146043=CARTESIAN_POINT('Ctrl Pts',(21.2856453456188,-19.1586543737303,
7.0436188246119));
#146044=CARTESIAN_POINT('Ctrl Pts',(21.2788593216166,-19.2424441636478,
7.04778853893227));
#146045=CARTESIAN_POINT('Ctrl Pts',(21.2679392098803,-19.3259311909062,
7.05195825325264));
#146046=CARTESIAN_POINT('Ctrl Pts',(21.2529369307439,-19.4086801275887,
7.05612796757301));
#146047=CARTESIAN_POINT('Ctrl Pts',(21.237935185453,-19.491426119709,7.06029753351705));
#146048=CARTESIAN_POINT('Ctrl Pts',(21.2188516444823,-19.573433620972,7.0644670994611));
#146049=CARTESIAN_POINT('Ctrl Pts',(21.1957895218783,-19.6542765480707,
7.06863666540515));
#146050=CARTESIAN_POINT('Ctrl Pts',(21.1719165634938,-19.7379618127557,
7.07295282814407));
#146051=CARTESIAN_POINT('Ctrl Pts',(21.143780188844,-19.8203985795368,7.07726899088298));
#146052=CARTESIAN_POINT('Ctrl Pts',(21.1115508461403,-19.9011322215674,
7.0815851536219));
#146053=CARTESIAN_POINT('Ctrl Pts',(21.0803713708853,-19.9792359737004,
7.08576071781358));
#146054=CARTESIAN_POINT('Ctrl Pts',(21.0453617283796,-20.0557454470089,
7.08993628200526));
#146055=CARTESIAN_POINT('Ctrl Pts',(21.0067242058648,-20.1302719058334,
7.09411184619694));
#146056=CARTESIAN_POINT('Ctrl Pts',(20.9661351939396,-20.2085625189234,
7.09849830820948));
#146057=CARTESIAN_POINT('Ctrl Pts',(20.9215424772636,-20.284664025024,7.10288477022202));
#146058=CARTESIAN_POINT('Ctrl Pts',(20.8732322919593,-20.3581597352501,
7.10727123223456));
#146059=CARTESIAN_POINT('Ctrl Pts',(20.824922106655,-20.4316554454762,7.11165769424711));
#146060=CARTESIAN_POINT('Ctrl Pts',(20.7728948573421,-20.5025449370744,
7.11604415625965));
#146061=CARTESIAN_POINT('Ctrl Pts',(20.7174842649082,-20.5704530178111,
7.12043061827219));
#146062=CARTESIAN_POINT('Ctrl Pts',(20.6646206180301,-20.6352397064664,
7.1246154567424));
#146063=CARTESIAN_POINT('Ctrl Pts',(20.6084810526635,-20.6975542088253,
7.12880029521261));
#146064=CARTESIAN_POINT('Ctrl Pts',(20.5493255613569,-20.7570465662371,
7.13298513368282));
#146065=CARTESIAN_POINT('Ctrl Pts',(20.4902614757663,-20.816446997415,7.13716350583606));
#146066=CARTESIAN_POINT('Ctrl Pts',(20.4281910470698,-20.8730336263624,
7.14134187798931));
#146067=CARTESIAN_POINT('Ctrl Pts',(20.3634146060857,-20.9264893115626,
7.14552025014255));
#146068=CARTESIAN_POINT('Ctrl Pts',(20.3404563686433,-20.9454352168149,
7.14700115984613));
#146069=CARTESIAN_POINT('Ctrl Pts',(20.3171585752192,-20.9639881395014,
7.14848206954971));
#146070=CARTESIAN_POINT('Ctrl Pts',(20.2935357468249,-20.9821350335323,
7.14996297925329));
#146071=CARTESIAN_POINT('Ctrl Pts',(20.2958869033725,-20.9851650055234,
6.34984102531927));
#146072=CARTESIAN_POINT('Ctrl Pts',(20.256159849257,-21.0159980900227,6.35235260960738));
#146073=CARTESIAN_POINT('Ctrl Pts',(19.5288319784645,-21.5446793381704,
6.39725612945596));
#146074=CARTESIAN_POINT('Ctrl Pts',(17.5479307767974,-21.7370548235123,
6.48455158486502));
#146075=CARTESIAN_POINT('Ctrl Pts',(16.247850859816,-20.0919179750469,6.57652302872766));
#146076=CARTESIAN_POINT('Ctrl Pts',(16.1710772471096,-19.0983559299756,
6.62610253702982));
#146077=CARTESIAN_POINT('Ctrl Pts',(16.1723626618067,-18.9541202106264,
6.6332901097715));
#146078=CARTESIAN_POINT('',(16.174000571626,-18.9502892327451,6.56670989025839));
#146079=CARTESIAN_POINT('Ctrl Pts',(20.2935357468249,-20.9821350335323,
6.2833427999391));
#146080=CARTESIAN_POINT('Ctrl Pts',(20.2268670566194,-21.0333494620566,
6.28751243731202));
#146081=CARTESIAN_POINT('Ctrl Pts',(20.1576502309574,-21.081293830517,6.29168207468495));
#146082=CARTESIAN_POINT('Ctrl Pts',(20.0862433854993,-21.1257152128035,
6.29585171205787));
#146083=CARTESIAN_POINT('Ctrl Pts',(20.0148367451412,-21.1701364674997,
6.30002133745445));
#146084=CARTESIAN_POINT('Ctrl Pts',(19.9412404887745,-21.2110345141912,
6.30419096285104));
#146085=CARTESIAN_POINT('Ctrl Pts',(19.8658401818764,-21.2482007322292,
6.30836058824763));
#146086=CARTESIAN_POINT('Ctrl Pts',(19.7898457788971,-21.2856597913099,
6.3125630670663));
#146087=CARTESIAN_POINT('Ctrl Pts',(19.7120191890284,-21.3193277301869,
6.31676554588497));
#146088=CARTESIAN_POINT('Ctrl Pts',(19.6327770921237,-21.3490397866272,
6.32096802470365));
#146089=CARTESIAN_POINT('Ctrl Pts',(19.5540386680255,-21.3785629894727,
6.32514379203458));
#146090=CARTESIAN_POINT('Ctrl Pts',(19.4739031398565,-21.4041803691427,
6.32931955936551));
#146091=CARTESIAN_POINT('Ctrl Pts',(19.3927942500441,-21.4257805351544,
6.33349532669644));
#146092=CARTESIAN_POINT('Ctrl Pts',(19.3109071059811,-21.447587958608,6.33771116125899));
#146093=CARTESIAN_POINT('Ctrl Pts',(19.2280282903973,-21.4653005647945,
6.34192699582153));
#146094=CARTESIAN_POINT('Ctrl Pts',(19.1446022367281,-21.4788569020018,
6.34614283038408));
#146095=CARTESIAN_POINT('Ctrl Pts',(19.0611761830589,-21.492413239209,6.35035866494663));
#146096=CARTESIAN_POINT('Ctrl Pts',(18.9772033709819,-21.5018133183543,
6.35457449950917));
#146097=CARTESIAN_POINT('Ctrl Pts',(18.8931294701917,-21.5070494734381,
6.35879033407172));
#146098=CARTESIAN_POINT('Ctrl Pts',(18.8096777759696,-21.512246877256,6.36297496846477));
#146099=CARTESIAN_POINT('Ctrl Pts',(18.7258158815286,-21.5133611702432,
6.36715960285782));
#146100=CARTESIAN_POINT('Ctrl Pts',(18.6419771668657,-21.5103455197025,
6.37134423725086));
#146101=CARTESIAN_POINT('Ctrl Pts',(18.5582577862359,-21.5073341615672,
6.3755229153348));
#146102=CARTESIAN_POINT('Ctrl Pts',(18.4745619756521,-21.5002045527773,
6.37970159341874));
#146103=CARTESIAN_POINT('Ctrl Pts',(18.3913265823787,-21.4889617515555,
6.38388027150268));
#146104=CARTESIAN_POINT('Ctrl Pts',(18.306599254501,-21.4775174312019,6.38813384938812));
#146105=CARTESIAN_POINT('Ctrl Pts',(18.2223494934531,-21.4618109801083,
6.39238742727355));
#146106=CARTESIAN_POINT('Ctrl Pts',(18.1390363521672,-21.4419032627308,
6.39664100515899));
#146107=CARTESIAN_POINT('Ctrl Pts',(18.0573383986974,-21.4223814953014,
6.40081211913694));
#146108=CARTESIAN_POINT('Ctrl Pts',(17.9765415407097,-21.3988200192303,
6.4049832331149));
#146109=CARTESIAN_POINT('Ctrl Pts',(17.8970700591984,-21.3713280625392,
6.40915434709285));
#146110=CARTESIAN_POINT('Ctrl Pts',(17.8176252451101,-21.3438453310398,
6.41332406141322));
#146111=CARTESIAN_POINT('Ctrl Pts',(17.7395053586241,-21.3124348885695,
6.41749377573359));
#146112=CARTESIAN_POINT('Ctrl Pts',(17.6631189946706,-21.2772556574331,
6.42166349005396));
#146113=CARTESIAN_POINT('Ctrl Pts',(17.586735348872,-21.2420776781249,6.425833055998));
#146114=CARTESIAN_POINT('Ctrl Pts',(17.5120855204508,-21.2031313700068,
6.43000262194203));
#146115=CARTESIAN_POINT('Ctrl Pts',(17.4395563508726,-21.1606230188137,
6.43417218788607));
#146116=CARTESIAN_POINT('Ctrl Pts',(17.3644771451662,-21.1166201264322,
6.43848835062499));
#146117=CARTESIAN_POINT('Ctrl Pts',(17.2916709526712,-21.0688003143231,
6.44280451336392));
#146118=CARTESIAN_POINT('Ctrl Pts',(17.2215354755328,-21.0174420984933,
6.44712067610284));
#146119=CARTESIAN_POINT('Ctrl Pts',(17.1536846541854,-20.9677568711423,
6.45129624029452));
#146120=CARTESIAN_POINT('Ctrl Pts',(17.0883335592485,-20.9147605602812,
6.4554718044862));
#146121=CARTESIAN_POINT('Ctrl Pts',(17.0258081406203,-20.8587460689743,
6.45964736867787));
#146122=CARTESIAN_POINT('Ctrl Pts',(16.9601247117371,-20.7999024188732,
6.46403383069042));
#146123=CARTESIAN_POINT('Ctrl Pts',(16.8975603248983,-20.7377280904825,
6.46842029270297));
#146124=CARTESIAN_POINT('Ctrl Pts',(16.838447047551,-20.6726042556212,6.47280675471551));
#146125=CARTESIAN_POINT('Ctrl Pts',(16.7793337702036,-20.6074804207598,
6.47719321672806));
#146126=CARTESIAN_POINT('Ctrl Pts',(16.7236719107426,-20.5394075767508,
6.48157967874061));
#146127=CARTESIAN_POINT('Ctrl Pts',(16.6717415022696,-20.4688025212726,
6.48596614075316));
#146128=CARTESIAN_POINT('Ctrl Pts',(16.6219091295864,-20.4010499743281,
6.49017538570612));
#146129=CARTESIAN_POINT('Ctrl Pts',(16.5753265021952,-20.3307132360493,
6.49438463065908));
#146130=CARTESIAN_POINT('Ctrl Pts',(16.532270626113,-20.2581346654013,6.49859387561204));
#146131=CARTESIAN_POINT('Ctrl Pts',(16.489277141859,-20.1856612676153,6.50279702099133));
#146132=CARTESIAN_POINT('Ctrl Pts',(16.4498004872776,-20.110952875341,6.50700016637061));
#146133=CARTESIAN_POINT('Ctrl Pts',(16.4140760664827,-20.0343829926109,
6.5112033117499));
#146134=CARTESIAN_POINT('Ctrl Pts',(16.3783931208862,-19.9579020056842,
6.51540157737789));
#146135=CARTESIAN_POINT('Ctrl Pts',(16.3464539443372,-19.8795642299173,
6.51959984300589));
#146136=CARTESIAN_POINT('Ctrl Pts',(16.3184487740251,-19.7997689984254,
6.52379810863388));
#146137=CARTESIAN_POINT('Ctrl Pts',(16.2904693914727,-19.7200472440891,
6.52799250840909));
#146138=CARTESIAN_POINT('Ctrl Pts',(16.2664169618497,-19.6388711282231,
6.5321869081843));
#146139=CARTESIAN_POINT('Ctrl Pts',(16.2464336691667,-19.5566600282013,
6.53638130795952));
#146140=CARTESIAN_POINT('Ctrl Pts',(16.2264610773219,-19.4744929513394,
6.54057346167876));
#146141=CARTESIAN_POINT('Ctrl Pts',(16.210553397436,-19.3912924312907,6.54476561539801));
#146142=CARTESIAN_POINT('Ctrl Pts',(16.1988026788696,-19.3074919730929,
6.54895776911726));
#146143=CARTESIAN_POINT('Ctrl Pts',(16.1870533030452,-19.2237010906829,
6.55314944380363));
#146144=CARTESIAN_POINT('Ctrl Pts',(16.1794600117858,-19.1393108539568,
6.55734111849));
#146145=CARTESIAN_POINT('Ctrl Pts',(16.1760633700115,-19.0547628189716,
6.56153279317637));
#146146=CARTESIAN_POINT('Ctrl Pts',(16.1746649834927,-19.0199546642812,
6.56325849219375));
#146147=CARTESIAN_POINT('Ctrl Pts',(16.173977295445,-18.9851198216844,6.56498419121113));
#146148=CARTESIAN_POINT('Ctrl Pts',(16.1740005716256,-18.9502892333483,
6.5667098902285));
#146149=CARTESIAN_POINT('Ctrl Pts',(16.174000571626,-18.9502892327451,6.56670989025839));
#146150=CARTESIAN_POINT('Ctrl Pts',(16.1740643617891,-18.8548333601137,
6.57143929947809));
#146151=CARTESIAN_POINT('Ctrl Pts',(16.1794711562484,-18.7595846663132,
6.57616870869779));
#146152=CARTESIAN_POINT('Ctrl Pts',(16.1901275024526,-18.6650980721186,
6.58089811791749));
#146153=CARTESIAN_POINT('Ctrl Pts',(16.2008364140088,-18.5701453968694,
6.585650856246));
#146154=CARTESIAN_POINT('Ctrl Pts',(16.2168466650978,-18.4759625571763,
6.59040359457451));
#146155=CARTESIAN_POINT('Ctrl Pts',(16.2380139506878,-18.3830943473309,
6.59515633290303));
#146156=CARTESIAN_POINT('Ctrl Pts',(16.2593038089219,-18.2896883688619,
6.59993659274351));
#146157=CARTESIAN_POINT('Ctrl Pts',(16.2858104835345,-18.19761248234,6.604716852584));
#146158=CARTESIAN_POINT('Ctrl Pts',(16.3173390825673,-18.1073994967126,
6.60949711242449));
#146159=CARTESIAN_POINT('Ctrl Pts',(16.3253523527945,-18.0844710744544,
6.61071205742785));
#146160=CARTESIAN_POINT('Ctrl Pts',(16.333689786842,-18.0616628735359,6.61192700243122));
#146161=CARTESIAN_POINT('Ctrl Pts',(16.3423477078173,-18.0389833992214,
6.61314194743458));
#146162=CARTESIAN_POINT('Ctrl Pts',(16.3721681801721,-17.9608684985717,
6.61732658182763));
#146163=CARTESIAN_POINT('Ctrl Pts',(16.405875193857,-17.8840707367779,6.62151121622068));
#146164=CARTESIAN_POINT('Ctrl Pts',(16.4433319467771,-17.8090039939072,
6.62569585061373));
#146165=CARTESIAN_POINT('Ctrl Pts',(16.4807353846456,-17.7340440992537,
6.62987452869767));
#146166=CARTESIAN_POINT('Ctrl Pts',(16.5218777565726,-17.6608107375732,
6.63405320678161));
#146167=CARTESIAN_POINT('Ctrl Pts',(16.5665735905076,-17.5896994606788,
6.63823188486555));
#146168=CARTESIAN_POINT('Ctrl Pts',(16.6120705651436,-17.5173135652528,
6.64248546275099));
#146169=CARTESIAN_POINT('Ctrl Pts',(16.661249474465,-17.4471270300731,6.64673904063642));
#146170=CARTESIAN_POINT('Ctrl Pts',(16.7138648542455,-17.3795325145214,
6.65099261852186));
#146171=CARTESIAN_POINT('Ctrl Pts',(16.7654601822184,-17.3132484505536,
6.65516373249981));
#146172=CARTESIAN_POINT('Ctrl Pts',(16.8203596287512,-17.2494571801029,
6.65933484647777));
#146173=CARTESIAN_POINT('Ctrl Pts',(16.8782881026493,-17.1884996869773,
6.66350596045572));
#146174=CARTESIAN_POINT('Ctrl Pts',(16.9361971380885,-17.1275626487273,
6.66767567477609));
#146175=CARTESIAN_POINT('Ctrl Pts',(16.99713286563,-17.0694578324917,6.67184538909646));
#146176=CARTESIAN_POINT('Ctrl Pts',(17.060781453689,-17.0144913687209,6.67601510341684));
#146177=CARTESIAN_POINT('Ctrl Pts',(17.1244277768581,-16.9595268608928,
6.68018466936088));
#146178=CARTESIAN_POINT('Ctrl Pts',(17.1907864198799,-16.9077007835217,
6.68435423530492));
#146179=CARTESIAN_POINT('Ctrl Pts',(17.2595094445541,-16.8592798558094,
6.68852380124896));
#146180=CARTESIAN_POINT('Ctrl Pts',(17.3306486859969,-16.8091565080125,
6.69283996398789));
#146181=CARTESIAN_POINT('Ctrl Pts',(17.4043212347438,-16.7626825189769,
6.69715612672681));
#146182=CARTESIAN_POINT('Ctrl Pts',(17.4801089073792,-16.7201045885064,
6.70147228946573));
#146183=CARTESIAN_POINT('Ctrl Pts',(17.5534278045499,-16.6789136296426,
6.70564785365741));
#146184=CARTESIAN_POINT('Ctrl Pts',(17.6287256988455,-16.6413689670528,
6.70982341784909));
#146185=CARTESIAN_POINT('Ctrl Pts',(17.7056010183993,-16.6076460304292,
6.71399898204077));
#146186=CARTESIAN_POINT('Ctrl Pts',(17.78635912759,-16.5722198284453,6.71838544405331));
#146187=CARTESIAN_POINT('Ctrl Pts',(17.8688576552586,-16.5410117758975,
6.72277190606585));
#146188=CARTESIAN_POINT('Ctrl Pts',(17.9526121488767,-16.5141663251738,
6.72715836807839));
#146189=CARTESIAN_POINT('Ctrl Pts',(18.0363666424947,-16.48732087445,6.73154483009094));
#146190=CARTESIAN_POINT('Ctrl Pts',(18.1213765216826,-16.4648381003647,
6.73593129210348));
#146191=CARTESIAN_POINT('Ctrl Pts',(18.20714644876,-16.4468003401833,6.74031775411602));
#146192=CARTESIAN_POINT('Ctrl Pts',(18.2889699743511,-16.4295925240862,
6.74450238850907));
#146193=CARTESIAN_POINT('Ctrl Pts',(18.3717897057139,-16.4163656164704,
6.74868702290212));
#146194=CARTESIAN_POINT('Ctrl Pts',(18.4551835868307,-16.407228613854,6.75287165729516));
#146195=CARTESIAN_POINT('Ctrl Pts',(18.5384587670798,-16.3981046166299,
6.75705033537911));
#146196=CARTESIAN_POINT('Ctrl Pts',(18.6223060204197,-16.3930590108019,
6.76122901346306));
#146197=CARTESIAN_POINT('Ctrl Pts',(18.7062923578699,-16.3921499484213,
6.76540769154701));
#146198=CARTESIAN_POINT('Ctrl Pts',(18.7917840900589,-16.3912245917508,
6.76966126943244));
#146199=CARTESIAN_POINT('Ctrl Pts',(18.877419469749,-16.3945856314592,6.77391484731788));
#146200=CARTESIAN_POINT('Ctrl Pts',(18.9627354674095,-16.4022392100534,
6.77816842520332));
#146201=CARTESIAN_POINT('Ctrl Pts',(19.0463974479748,-16.4097444090919,
6.78233953918127));
#146202=CARTESIAN_POINT('Ctrl Pts',(19.1297518403943,-16.4213771508024,
6.78651065315922));
#146203=CARTESIAN_POINT('Ctrl Pts',(19.2123630296012,-16.4370906950924,
6.79068176713717));
#146204=CARTESIAN_POINT('Ctrl Pts',(19.2949464978256,-16.4527989665508,
6.79485148145754));
#146205=CARTESIAN_POINT('Ctrl Pts',(19.3767868065739,-16.472585235142,6.79902119577791));
#146206=CARTESIAN_POINT('Ctrl Pts',(19.457456677499,-16.4963513207745,6.80319091009829));
#146207=CARTESIAN_POINT('Ctrl Pts',(19.5381236778441,-16.5201165607077,
6.80736047604233));
#146208=CARTESIAN_POINT('Ctrl Pts',(19.6176198821352,-16.5478612052844,
6.81153004198638));
#146209=CARTESIAN_POINT('Ctrl Pts',(19.6955326893842,-16.579437063586,6.81569960793043));
#146210=CARTESIAN_POINT('Ctrl Pts',(19.7761848148201,-16.6121230901123,
6.82001577066935));
#146211=CARTESIAN_POINT('Ctrl Pts',(19.8551396382572,-16.6489145558588,
6.82433193340827));
#146212=CARTESIAN_POINT('Ctrl Pts',(19.9319633694499,-16.6895933686765,
6.82864809614719));
#146213=CARTESIAN_POINT('Ctrl Pts',(20.0062845756794,-16.7289470734454,
6.83282366033887));
#146214=CARTESIAN_POINT('Ctrl Pts',(20.0786110173904,-16.771938472629,6.83699922453055));
#146215=CARTESIAN_POINT('Ctrl Pts',(20.1485778227392,-16.8183248646023,
6.84117478872223));
#146216=CARTESIAN_POINT('Ctrl Pts',(20.2220784850958,-16.867054122961,6.84556125073476));
#146217=CARTESIAN_POINT('Ctrl Pts',(20.2929744068258,-16.9195300021186,
6.8499477127473));
#146218=CARTESIAN_POINT('Ctrl Pts',(20.3608819013655,-16.9754233435029,
6.85433417475984));
#146219=CARTESIAN_POINT('Ctrl Pts',(20.4287893959053,-17.0313166848872,
6.85872063677238));
#146220=CARTESIAN_POINT('Ctrl Pts',(20.4937080861994,-17.0906270409862,
6.86310709878492));
#146221=CARTESIAN_POINT('Ctrl Pts',(20.5553006227462,-17.1529824788,6.86749356079746));
#146222=CARTESIAN_POINT('Ctrl Pts',(20.6140591953844,-17.2124688504871,
6.87167819519051));
#146223=CARTESIAN_POINT('Ctrl Pts',(20.6700096812721,-17.2749476638323,
6.87586282958355));
#146224=CARTESIAN_POINT('Ctrl Pts',(20.7228319806688,-17.3401230342644,
6.8800474639766));
#146225=CARTESIAN_POINT('Ctrl Pts',(20.7755790940605,-17.4052056356238,
6.88422614206054));
#146226=CARTESIAN_POINT('Ctrl Pts',(20.8252065780214,-17.4729768158299,
6.88840482014449));
#146227=CARTESIAN_POINT('Ctrl Pts',(20.8714311671561,-17.5431039762745,
6.89258349822843));
#146228=CARTESIAN_POINT('Ctrl Pts',(20.9184842988301,-17.6144881156706,
6.89683707611387));
#146229=CARTESIAN_POINT('Ctrl Pts',(20.9620110031542,-17.6883131849442,
6.90109065399931));
#146230=CARTESIAN_POINT('Ctrl Pts',(21.0017554861493,-17.7641931743588,
6.90534423188474));
#146231=CARTESIAN_POINT('Ctrl Pts',(21.0407294447865,-17.838602082111,6.90951534586269));
#146232=CARTESIAN_POINT('Ctrl Pts',(21.0760663016048,-17.9149865174727,
6.91368645984064));
#146233=CARTESIAN_POINT('Ctrl Pts',(21.1075695674518,-17.9929548975847,
6.9178575738186));
#146234=CARTESIAN_POINT('Ctrl Pts',(21.1390622620736,-18.0708971146537,
6.92202728813897));
#146235=CARTESIAN_POINT('Ctrl Pts',(21.1667237483346,-18.1504217947136,
6.92619700245934));
#146236=CARTESIAN_POINT('Ctrl Pts',(21.1904053024889,-18.2311165212712,
6.93036671677971));
#146237=CARTESIAN_POINT('Ctrl Pts',(21.214086013952,-18.3118083763641,6.93453628272375));
#146238=CARTESIAN_POINT('Ctrl Pts',(21.2337869461661,-18.3936697535163,
6.9387058486678));
#146239=CARTESIAN_POINT('Ctrl Pts',(21.2494093711531,-18.4762735076587,
6.94287541461184));
#146240=CARTESIAN_POINT('Ctrl Pts',(21.2655810613302,-18.561781507894,6.94719157735076));
#146241=CARTESIAN_POINT('Ctrl Pts',(21.2773820094429,-18.6480845421362,
6.95150774008968));
#146242=CARTESIAN_POINT('Ctrl Pts',(21.2847607940422,-18.7346998122938,
6.9558239028286));
#146243=CARTESIAN_POINT('Ctrl Pts',(21.2918992155093,-18.8184935991363,
6.95999946702028));
#146244=CARTESIAN_POINT('Ctrl Pts',(21.2948991834511,-18.9025791196893,
6.96417503121196));
#146245=CARTESIAN_POINT('Ctrl Pts',(21.2937672733171,-18.9865182046883,
6.96835059540364));
#146246=CARTESIAN_POINT('Ctrl Pts',(21.2925781930931,-19.0746968533244,
6.97273705741618));
#146247=CARTESIAN_POINT('Ctrl Pts',(21.2868289009943,-19.1627133020808,
6.97712351942873));
#146248=CARTESIAN_POINT('Ctrl Pts',(21.2765884850301,-19.250066763985,6.98150998144127));
#146249=CARTESIAN_POINT('Ctrl Pts',(21.2663480690658,-19.3374202258893,
6.98589644345381));
#146250=CARTESIAN_POINT('Ctrl Pts',(21.2516167014297,-19.4241101416678,
6.99028290546635));
#146251=CARTESIAN_POINT('Ctrl Pts',(21.2325245180281,-19.5096515334976,
6.9946693674789));
#146252=CARTESIAN_POINT('Ctrl Pts',(21.2143148178506,-19.5912390117464,
6.99885307745113));
#146253=CARTESIAN_POINT('Ctrl Pts',(21.1920707686421,-19.6720854131111,
7.00303678742336));
#146254=CARTESIAN_POINT('Ctrl Pts',(21.1658678428317,-19.7517617113874,
7.00722049739559));
#146255=CARTESIAN_POINT('Ctrl Pts',(21.1396995424223,-19.8313327228036,
7.01139867887696));
#146256=CARTESIAN_POINT('Ctrl Pts',(21.1095828937122,-19.9097362679935,
7.01557686035833));
#146257=CARTESIAN_POINT('Ctrl Pts',(21.0756441740988,-19.9865542817607,
7.0197550418397));
#146258=CARTESIAN_POINT('Ctrl Pts',(21.0417401170689,-20.0632938390966,
7.02392895602501));
#146259=CARTESIAN_POINT('Ctrl Pts',(21.0040219265316,-20.1384506626217,
7.02810287021032));
#146260=CARTESIAN_POINT('Ctrl Pts',(20.9626649802985,-20.2116239143455,
7.03227678439562));
#146261=CARTESIAN_POINT('Ctrl Pts',(20.9205833380602,-20.2860793778389,
7.0365238379012));
#146262=CARTESIAN_POINT('Ctrl Pts',(20.8747343561323,-20.3584806290068,
7.04077089140678));
#146263=CARTESIAN_POINT('Ctrl Pts',(20.8253528363596,-20.4284292444444,
7.04501794491235));
#146264=CARTESIAN_POINT('Ctrl Pts',(20.7768706609689,-20.4971039441618,
7.04918765037907));
#146265=CARTESIAN_POINT('Ctrl Pts',(20.7249838359412,-20.5634142202303,
7.05335735584579));
#146266=CARTESIAN_POINT('Ctrl Pts',(20.6699585837801,-20.6270117497762,
7.0575270613125));
#146267=CARTESIAN_POINT('Ctrl Pts',(20.613402253929,-20.6923788806378,7.06181278883751));
#146268=CARTESIAN_POINT('Ctrl Pts',(20.5535305486344,-20.754879647566,7.06609851636252));
#146269=CARTESIAN_POINT('Ctrl Pts',(20.4906759641957,-20.8141733423119,
7.07038424388752));
#146270=CARTESIAN_POINT('Ctrl Pts',(20.427821379757,-20.8734670370578,7.07466997141253));
#146271=CARTESIAN_POINT('Ctrl Pts',(20.3619843152027,-20.9295533148579,
7.07895569893754));
#146272=CARTESIAN_POINT('Ctrl Pts',(20.2935357468249,-20.9821350335323,
7.08324142646255));
#146273=CARTESIAN_POINT('Origin',(18.734,-18.952,-1.76670989022851));
#146274=CARTESIAN_POINT('',(20.290984793813,-20.9788230549133,7.94987222229573));
#146275=CARTESIAN_POINT('',(20.2961055615655,-20.9854720348211,7.88329696296241));
#146276=CARTESIAN_POINT('',(20.2935357468249,-20.9821350335323,-1.76670989022851));
#146277=CARTESIAN_POINT('',(16.1743644997381,-18.9525601738959,7.4332900849458));
#146278=CARTESIAN_POINT('Ctrl Pts',(16.1781030393919,-18.952558854618,7.43329010977151));
#146279=CARTESIAN_POINT('Ctrl Pts',(16.1790025482941,-18.4906083143692,
7.4561794192865));
#146280=CARTESIAN_POINT('Ctrl Pts',(16.5197425194489,-17.1718695770502,
7.52146066436197));
#146281=CARTESIAN_POINT('Ctrl Pts',(18.6352034714368,-15.9265199028681,
7.62913384499793));
#146282=CARTESIAN_POINT('Ctrl Pts',(21.2244732819954,-17.231292760559,7.75630965167936));
#146283=CARTESIAN_POINT('Ctrl Pts',(21.4803857440547,-19.6552910993149,
7.86322244411196));
#146284=CARTESIAN_POINT('Ctrl Pts',(20.6448527398538,-20.7063099546061,
7.92774330098409));
#146285=CARTESIAN_POINT('Ctrl Pts',(20.290984793813,-20.9788230549133,7.94987222229573));
#146286=CARTESIAN_POINT('Ctrl Pts',(20.2935357468249,-20.9821350335323,
7.14996297925329));
#146287=CARTESIAN_POINT('Ctrl Pts',(20.2269740650341,-21.0332672589297,
7.15413571584543));
#146288=CARTESIAN_POINT('Ctrl Pts',(20.1578294177455,-21.0811729380824,
7.15830845243758));
#146289=CARTESIAN_POINT('Ctrl Pts',(20.0864499467968,-21.1255866997683,
7.16248118902972));
#146290=CARTESIAN_POINT('Ctrl Pts',(20.015108654789,-21.1699767057388,7.16665169373835));
#146291=CARTESIAN_POINT('Ctrl Pts',(19.9415353022569,-21.210878260028,7.17082219844698));
#146292=CARTESIAN_POINT('Ctrl Pts',(19.8661075037954,-21.2480689449252,
7.17499270315561));
#146293=CARTESIAN_POINT('Ctrl Pts',(19.7906974228729,-21.2852508939529,
7.17916222823762));
#146294=CARTESIAN_POINT('Ctrl Pts',(19.7134341737692,-21.3187235017973,
7.18333175331963));
#146295=CARTESIAN_POINT('Ctrl Pts',(19.634719278428,-21.3483106604671,7.18750127840164));
#146296=CARTESIAN_POINT('Ctrl Pts',(19.5559992603542,-21.3778997446568,
7.1916710748346));
#146297=CARTESIAN_POINT('Ctrl Pts',(19.4758278395417,-21.4036027169435,
7.19584087126757));
#146298=CARTESIAN_POINT('Ctrl Pts',(19.3946244955917,-21.4252923959419,
7.20001066770053));
#146299=CARTESIAN_POINT('Ctrl Pts',(19.3133366948555,-21.4470046336245,
7.20418480099438));
#146300=CARTESIAN_POINT('Ctrl Pts',(19.2310152730944,-21.4646951235253,
7.20835893428822));
#146301=CARTESIAN_POINT('Ctrl Pts',(19.1480923087683,-21.4782873074571,
7.21253306758207));
#146302=CARTESIAN_POINT('Ctrl Pts',(19.0651253024502,-21.4918867104611,
7.21670941783893));
#146303=CARTESIAN_POINT('Ctrl Pts',(18.9815565747079,-21.5013834208329,
7.22088576809579));
#146304=CARTESIAN_POINT('Ctrl Pts',(18.8978233448839,-21.5067528083302,
7.22506211835265));
#146305=CARTESIAN_POINT('Ctrl Pts',(18.8139435125698,-21.5121315967019,
7.22924578068082));
#146306=CARTESIAN_POINT('Ctrl Pts',(18.7298990634063,-21.5133686206996,
7.233429443009));
#146307=CARTESIAN_POINT('Ctrl Pts',(18.6461270483911,-21.5104914196408,
7.23761310533717));
#146308=CARTESIAN_POINT('Ctrl Pts',(18.5794262764124,-21.5082005408583,
7.24094421187599));
#146309=CARTESIAN_POINT('Ctrl Pts',(18.5128982522666,-21.5033024356435,
7.24427531841481));
#146310=CARTESIAN_POINT('Ctrl Pts',(18.4467595506041,-21.4958342957494,
7.24760642495362));
#146311=CARTESIAN_POINT('Ctrl Pts',(18.3636741606704,-21.4864525978996,
7.25179105934667));
#146312=CARTESIAN_POINT('Ctrl Pts',(18.2808942658294,-21.4729786230522,
7.25597569373971));
#146313=CARTESIAN_POINT('Ctrl Pts',(18.1988547913486,-21.4554415522751,
7.26016032813276));
#146314=CARTESIAN_POINT('Ctrl Pts',(18.1169320899054,-21.4379294433476,
7.2643390062167));
#146315=CARTESIAN_POINT('Ctrl Pts',(18.0357481614735,-21.4163658213153,
7.26851768430064));
#146316=CARTESIAN_POINT('Ctrl Pts',(17.9557323296064,-21.3908315713104,
7.27269636238458));
#146317=CARTESIAN_POINT('Ctrl Pts',(17.8742822714594,-21.3648396382252,
7.27694994027001));
#146318=CARTESIAN_POINT('Ctrl Pts',(17.7940430771268,-21.3347333841336,
7.28120351815545));
#146319=CARTESIAN_POINT('Ctrl Pts',(17.7154562415199,-21.3006525098578,
7.28545709604089));
#146320=CARTESIAN_POINT('Ctrl Pts',(17.638392965071,-21.2672323598332,7.28962821001883));
#146321=CARTESIAN_POINT('Ctrl Pts',(17.5629189921772,-21.229990517358,7.29379932399678));
#146322=CARTESIAN_POINT('Ctrl Pts',(17.4894331713725,-21.1891082694139,
7.29797043797473));
#146323=CARTESIAN_POINT('Ctrl Pts',(17.4159720094446,-21.1482397399029,
7.30214015229511));
#146324=CARTESIAN_POINT('Ctrl Pts',(17.3444980763224,-21.1037334544496,
7.30630986661548));
#146325=CARTESIAN_POINT('Ctrl Pts',(17.275386138507,-21.0558169129134,7.31047958093586));
#146326=CARTESIAN_POINT('Ctrl Pts',(17.2062766599911,-21.0079020764535,
7.3146491468799));
#146327=CARTESIAN_POINT('Ctrl Pts',(17.1395293872401,-20.9565774880024,
7.31881871282395));
#146328=CARTESIAN_POINT('Ctrl Pts',(17.0754894346058,-20.9021135106644,
7.32298827876799));
#146329=CARTESIAN_POINT('Ctrl Pts',(17.0091979162386,-20.8457346470717,
7.32730444150691));
#146330=CARTESIAN_POINT('Ctrl Pts',(16.9458080406879,-20.7859918669771,
7.33162060424583));
#146331=CARTESIAN_POINT('Ctrl Pts',(16.8856630675041,-20.7232285521558,
7.33593676698475));
#146332=CARTESIAN_POINT('Ctrl Pts',(16.8274773104958,-20.6625097457132,
7.34011233117643));
#146333=CARTESIAN_POINT('Ctrl Pts',(16.77232857006,-20.5989645570467,7.34428789536811));
#146334=CARTESIAN_POINT('Ctrl Pts',(16.7204869451087,-20.532938068927,7.34846345955978));
#146335=CARTESIAN_POINT('Ctrl Pts',(16.6660269229229,-20.4635767398552,
7.35284992157233));
#146336=CARTESIAN_POINT('Ctrl Pts',(16.6152172172817,-20.3914773402462,
7.35723638358488));
#146337=CARTESIAN_POINT('Ctrl Pts',(16.5683186145659,-20.317072941928,7.36162284559742));
#146338=CARTESIAN_POINT('Ctrl Pts',(16.52142001185,-20.2426685436099,7.36600930760997));
#146339=CARTESIAN_POINT('Ctrl Pts',(16.4784327293519,-20.1659596899256,
7.37039576962251));
#146340=CARTESIAN_POINT('Ctrl Pts',(16.4395601204679,-20.0874054955004,
7.37478223163505));
#146341=CARTESIAN_POINT('Ctrl Pts',(16.3997963941391,-20.0070505211682,
7.37926924910123));
#146342=CARTESIAN_POINT('Ctrl Pts',(16.3642056179145,-19.9244993534859,
7.38375626656741));
#146343=CARTESIAN_POINT('Ctrl Pts',(16.333017909016,-19.8401919830611,7.38824328403359));
#146344=CARTESIAN_POINT('Ctrl Pts',(16.3019356806124,-19.7561697500662,
7.39271512587963));
#146345=CARTESIAN_POINT('Ctrl Pts',(16.2752269677052,-19.6704034844248,
7.39718696772568));
#146346=CARTESIAN_POINT('Ctrl Pts',(16.2530742870064,-19.5833537887801,
7.40165880957172));
#146347=CARTESIAN_POINT('Ctrl Pts',(16.2309688572623,-19.4964897673338,
7.40612111312307));
#146348=CARTESIAN_POINT('Ctrl Pts',(16.2134002030054,-19.408348109083,7.41058341667443));
#146349=CARTESIAN_POINT('Ctrl Pts',(16.2005019648758,-19.3194067310513,
7.41504572022578));
#146350=CARTESIAN_POINT('Ctrl Pts',(16.1876417930136,-19.2307278436206,
7.41949485428542));
#146351=CARTESIAN_POINT('Ctrl Pts',(16.1794246278367,-19.1412542906273,
7.42394398834506));
#146352=CARTESIAN_POINT('Ctrl Pts',(16.175933399183,-19.0514749505386,7.4283931224047));
#146353=CARTESIAN_POINT('Ctrl Pts',(16.1746525201579,-19.0185362676236,
7.43002544244505));
#146354=CARTESIAN_POINT('Ctrl Pts',(16.1740072831437,-18.9855565464226,
7.4316577624854));
#146355=CARTESIAN_POINT('Ctrl Pts',(16.1740000613162,-18.952560302501,7.43329008252576));
#146356=CARTESIAN_POINT('',(16.1738764939443,-18.9508698166505,7.36670989022851));
#146357=CARTESIAN_POINT('Ctrl Pts',(20.2935357468249,-20.9821350335323,
7.08324142646255));
#146358=CARTESIAN_POINT('Ctrl Pts',(20.226845872581,-21.033365735489,7.08741703796854));
#146359=CARTESIAN_POINT('Ctrl Pts',(20.1576775032969,-21.0812695904658,
7.09159264947453));
#146360=CARTESIAN_POINT('Ctrl Pts',(20.0864031447847,-21.1256158202351,
7.09576826098051));
#146361=CARTESIAN_POINT('Ctrl Pts',(20.012217792683,-21.1717732426027,7.10011441317715));
#146362=CARTESIAN_POINT('Ctrl Pts',(19.9357512244538,-21.2140759358748,
7.10446056537378));
#146363=CARTESIAN_POINT('Ctrl Pts',(19.8574497188556,-21.2523175279085,
7.10880671757042));
#146364=CARTESIAN_POINT('Ctrl Pts',(19.7791482132574,-21.2905591199422,
7.11315286976705));
#146365=CARTESIAN_POINT('Ctrl Pts',(19.6990123085245,-21.3247394606782,
7.11749902196369));
#146366=CARTESIAN_POINT('Ctrl Pts',(19.6175072439402,-21.3547099179687,
7.12184517416032));
#146367=CARTESIAN_POINT('Ctrl Pts',(19.5390311848803,-21.3835665710906,
7.12602980855337));
#146368=CARTESIAN_POINT('Ctrl Pts',(19.4589938470389,-21.4086281659991,
7.13021444294642));
#146369=CARTESIAN_POINT('Ctrl Pts',(19.3777970941006,-21.429725832619,7.13439907733946));
#146370=CARTESIAN_POINT('Ctrl Pts',(19.29671591469,-21.4507934693218,7.13857775542341));
#146371=CARTESIAN_POINT('Ctrl Pts',(19.2144790396055,-21.4679082701427,
7.14275643350735));
#146372=CARTESIAN_POINT('Ctrl Pts',(19.1315065014625,-21.4809500946628,
7.1469351115913));
#146373=CARTESIAN_POINT('Ctrl Pts',(19.0470467402046,-21.4942256845144,
7.15118868947673));
#146374=CARTESIAN_POINT('Ctrl Pts',(18.9618251354748,-21.5032806792605,
7.15544226736217));
#146375=CARTESIAN_POINT('Ctrl Pts',(18.8762989641011,-21.508042058499,7.1596958452476));
#146376=CARTESIAN_POINT('Ctrl Pts',(18.79243088445,-21.5127111291099,7.16386695922556));
#146377=CARTESIAN_POINT('Ctrl Pts',(18.7082704224838,-21.5132515520536,
7.16803807320351));
#146378=CARTESIAN_POINT('Ctrl Pts',(18.6242553740811,-21.5096465973785,
7.17220918718146));
#146379=CARTESIAN_POINT('Ctrl Pts',(18.5402685177393,-21.5060428523808,
7.17637890150183));
#146380=CARTESIAN_POINT('Ctrl Pts',(18.456427437281,-21.4982965120596,7.18054861582221));
#146381=CARTESIAN_POINT('Ctrl Pts',(18.3731691163824,-21.4864429513066,
7.18471833014258));
#146382=CARTESIAN_POINT('Ctrl Pts',(18.2899137581722,-21.4745898123542,
7.18888789608662));
#146383=CARTESIAN_POINT('Ctrl Pts',(18.2072415736112,-21.4586298092437,
7.19305746203067));
#146384=CARTESIAN_POINT('Ctrl Pts',(18.1255822535273,-21.4386499242509,
7.19722702797471));
#146385=CARTESIAN_POINT('Ctrl Pts',(18.0410518924869,-21.4179675711496,
7.20154319071364));
#146386=CARTESIAN_POINT('Ctrl Pts',(17.9576074580675,-21.3929775239273,
7.20585935345255));
#146387=CARTESIAN_POINT('Ctrl Pts',(17.8757097136974,-21.363832868264,7.21017551619147));
#146388=CARTESIAN_POINT('Ctrl Pts',(17.7964797797361,-21.3356375966935,
7.21435108038315));
#146389=CARTESIAN_POINT('Ctrl Pts',(17.7186977338733,-21.303554456016,7.21852664457484));
#146390=CARTESIAN_POINT('Ctrl Pts',(17.6427597031132,-21.2677708467054,
7.22270220876652));
#146391=CARTESIAN_POINT('Ctrl Pts',(17.562986222945,-21.2301798923558,7.22708867077906));
#146392=CARTESIAN_POINT('Ctrl Pts',(17.4852484504759,-21.1885050997006,
7.2314751327916));
#146393=CARTESIAN_POINT('Ctrl Pts',(17.4099736292609,-21.1430166976971,
7.23586159480414));
#146394=CARTESIAN_POINT('Ctrl Pts',(17.334698808046,-21.0975282956936,7.24024805681668));
#146395=CARTESIAN_POINT('Ctrl Pts',(17.2618873758782,-21.0482266726393,
7.24463451882922));
#146396=CARTESIAN_POINT('Ctrl Pts',(17.1919269101811,-20.9954310816997,
7.24902098084176));
#146397=CARTESIAN_POINT('Ctrl Pts',(17.1258771580207,-20.9455867065661,
7.25316224442402));
#146398=CARTESIAN_POINT('Ctrl Pts',(17.0621112325388,-20.892434299838,7.25730350800628));
#146399=CARTESIAN_POINT('Ctrl Pts',(17.0009846311415,-20.8362127616859,
7.26144477158854));
#146400=CARTESIAN_POINT('Ctrl Pts',(16.9399453026366,-20.7800714932715,
7.26558012252322));
#146401=CARTESIAN_POINT('Ctrl Pts',(16.8815381604268,-20.7208701082194,
7.26971547345791));
#146402=CARTESIAN_POINT('Ctrl Pts',(16.8260879518442,-20.6588894564388,
7.27385082439259));
#146403=CARTESIAN_POINT('Ctrl Pts',(16.770701311821,-20.5969798597695,7.27798143452813));
#146404=CARTESIAN_POINT('Ctrl Pts',(16.7182651826551,-20.5322976752766,
7.28211204466367));
#146405=CARTESIAN_POINT('Ctrl Pts',(16.6690684130046,-20.4651614391824,
7.2862426547992));
#146406=CARTESIAN_POINT('Ctrl Pts',(16.6199019406792,-20.3980665482496,
7.29037072114092));
#146407=CARTESIAN_POINT('Ctrl Pts',(16.5739711466917,-20.3285209831314,
7.29449878748264));
#146408=CARTESIAN_POINT('Ctrl Pts',(16.5315246255303,-20.2568763255016,
7.29862685382436));
#146409=CARTESIAN_POINT('Ctrl Pts',(16.4890908665707,-20.185253208944,7.30275367899921));
#146410=CARTESIAN_POINT('Ctrl Pts',(16.4501395400175,-20.1115326575802,
7.30688050417406));
#146411=CARTESIAN_POINT('Ctrl Pts',(16.4148750854128,-20.0360939214575,
7.31100732934891));
#146412=CARTESIAN_POINT('Ctrl Pts',(16.3796101195077,-19.9606540915462,
7.31513421435872));
#146413=CARTESIAN_POINT('Ctrl Pts',(16.3480323287909,-19.8834964546655,
7.31926109936854));
#146414=CARTESIAN_POINT('Ctrl Pts',(16.320298833946,-19.8050220870468,7.32338798437836));
#146415=CARTESIAN_POINT('Ctrl Pts',(16.2925397363851,-19.7264752742868,
7.32751867920247));
#146416=CARTESIAN_POINT('Ctrl Pts',(16.2686321752694,-19.646609748954,7.33164937402659));
#146417=CARTESIAN_POINT('Ctrl Pts',(16.2486837569799,-19.5658429540043,
7.3357800688507));
#146418=CARTESIAN_POINT('Ctrl Pts',(16.2287250388403,-19.4850344572077,
7.33991289645232));
#146419=CARTESIAN_POINT('Ctrl Pts',(16.2127296214478,-19.4033242264923,
7.34404572405394));
#146420=CARTESIAN_POINT('Ctrl Pts',(16.2007537416511,-19.3211387199432,
7.34817855165555));
#146421=CARTESIAN_POINT('Ctrl Pts',(16.1887593096482,-19.2388258972814,
7.35231778154836));
#146422=CARTESIAN_POINT('Ctrl Pts',(16.180796886798,-19.1560367972438,7.35645701144116));
#146423=CARTESIAN_POINT('Ctrl Pts',(16.176870697397,-19.0732011954116,7.36059624133396));
#146424=CARTESIAN_POINT('Ctrl Pts',(16.1749377014765,-19.0324184251309,
7.36263412429881));
#146425=CARTESIAN_POINT('Ctrl Pts',(16.1739822581149,-18.9916243590029,
7.36467200726366));
#146426=CARTESIAN_POINT('Ctrl Pts',(16.1740002494514,-18.9508698712832,
7.36670989022851));
#146427=CARTESIAN_POINT('Ctrl Pts',(16.170378839146,-18.9508682725878,7.36670989022851));
#146428=CARTESIAN_POINT('Ctrl Pts',(16.1700290602903,-18.8875375837258,
7.36987218932674));
#146429=CARTESIAN_POINT('Ctrl Pts',(16.2008981559486,-17.9755793377669,
7.41542642398544));
#146430=CARTESIAN_POINT('Ctrl Pts',(17.2895132774888,-16.291783852743,7.50337259420463));
#146431=CARTESIAN_POINT('Ctrl Pts',(20.1889475254729,-16.2974907158275,
7.63054840088606));
#146432=CARTESIAN_POINT('Ctrl Pts',(21.746983751553,-18.7282885913632,7.75718985713872));
#146433=CARTESIAN_POINT('Ctrl Pts',(20.9598514166904,-20.4743156438175,
7.8414393778309));
#146434=CARTESIAN_POINT('Ctrl Pts',(20.2961055615625,-20.9854720348234,
7.8832969629626));
#146435=CARTESIAN_POINT('Origin',(18.734,-18.952,-1.76670989022851));
#146436=CARTESIAN_POINT('',(20.2935357468249,-20.9821350335323,8.74981199600226));
#146437=CARTESIAN_POINT('',(20.2935357468249,-20.9821350335323,8.68337763131693));
#146438=CARTESIAN_POINT('',(20.2935357468249,-20.9821350335323,-1.76670989022851));
#146439=CARTESIAN_POINT('',(16.1740010826189,-18.9496456407634,8.23329012251336));
#146440=CARTESIAN_POINT('Ctrl Pts',(16.1740010826189,-18.9496456407634,
8.23329012251336));
#146441=CARTESIAN_POINT('Ctrl Pts',(16.1741014808467,-18.8404782076363,
8.23871812867226));
#146442=CARTESIAN_POINT('Ctrl Pts',(16.1811885397045,-18.7316228555833,
8.24414613483116));
#146443=CARTESIAN_POINT('Ctrl Pts',(16.1951208364064,-18.6238345041446,
8.24957414099005));
#146444=CARTESIAN_POINT('Ctrl Pts',(16.2083299266979,-18.5216412981712,
8.25472038679507));
#146445=CARTESIAN_POINT('Ctrl Pts',(16.2276915596983,-18.4204066645004,
8.25986663260008));
#146446=CARTESIAN_POINT('Ctrl Pts',(16.253046772176,-18.32075434152,8.2650128784051));
#146447=CARTESIAN_POINT('Ctrl Pts',(16.2736641888711,-18.2397227402536,
8.26919751279815));
#146448=CARTESIAN_POINT('Ctrl Pts',(16.2982940662941,-18.1595514977397,
8.27338214719119));
#146449=CARTESIAN_POINT('Ctrl Pts',(16.3268482220626,-18.0806675043515,
8.27756678158424));
#146450=CARTESIAN_POINT('Ctrl Pts',(16.3553617345247,-18.0018957925641,
8.28174545966818));
#146451=CARTESIAN_POINT('Ctrl Pts',(16.3877882750862,-17.9244081193637,
8.28592413775211));
#146452=CARTESIAN_POINT('Ctrl Pts',(16.4239892031398,-17.8486187792113,
8.29010281583605));
#146453=CARTESIAN_POINT('Ctrl Pts',(16.4608390068116,-17.7714709696053,
8.29435639372149));
#146454=CARTESIAN_POINT('Ctrl Pts',(16.5015997218016,-17.6960834444033,
8.29860997160693));
#146455=CARTESIAN_POINT('Ctrl Pts',(16.5460727818104,-17.6228745401938,
8.30286354949236));
#146456=CARTESIAN_POINT('Ctrl Pts',(16.5896836447689,-17.5510849334478,
8.30703466347031));
#146457=CARTESIAN_POINT('Ctrl Pts',(16.636863945312,-17.4813906391621,8.31120577744826));
#146458=CARTESIAN_POINT('Ctrl Pts',(16.6873797310321,-17.4141620778998,
8.31537689142621));
#146459=CARTESIAN_POINT('Ctrl Pts',(16.7378785656923,-17.3469560758304,
8.31954660574659));
#146460=CARTESIAN_POINT('Ctrl Pts',(16.7917103865527,-17.2822145310262,
8.32371632006696));
#146461=CARTESIAN_POINT('Ctrl Pts',(16.8485987415143,-17.220277708609,8.32788603438733));
#146462=CARTESIAN_POINT('Ctrl Pts',(16.9054850721441,-17.1583430901697,
8.33205560033138));
#146463=CARTESIAN_POINT('Ctrl Pts',(16.9654274088045,-17.0992133339122,
8.33622516627543));
#146464=CARTESIAN_POINT('Ctrl Pts',(17.0281108772058,-17.0431934878746,
8.34039473221947));
#146465=CARTESIAN_POINT('Ctrl Pts',(17.0929982190277,-16.9852040531583,
8.34471089495839));
#146466=CARTESIAN_POINT('Ctrl Pts',(17.160822642128,-16.9305476379184,8.34902705769731));
#146467=CARTESIAN_POINT('Ctrl Pts',(17.2311971876102,-16.8795175013831,
8.35334322043624));
#146468=CARTESIAN_POINT('Ctrl Pts',(17.2992792896754,-16.8301496661781,
8.35751878462792));
#146469=CARTESIAN_POINT('Ctrl Pts',(17.3697475047294,-16.7841757035315,
8.36169434881959));
#146470=CARTESIAN_POINT('Ctrl Pts',(17.4422231594134,-16.7418161628217,
8.36586991301127));
#146471=CARTESIAN_POINT('Ctrl Pts',(17.518359387121,-16.6973171424109,8.37025637502381));
#146472=CARTESIAN_POINT('Ctrl Pts',(17.5967106568091,-16.6568075367651,
8.37464283703635));
#146473=CARTESIAN_POINT('Ctrl Pts',(17.6768123961764,-16.6204866780733,
8.3790292990489));
#146474=CARTESIAN_POINT('Ctrl Pts',(17.7569141355437,-16.5841658193815,
8.38341576106144));
#146475=CARTESIAN_POINT('Ctrl Pts',(17.8387657767031,-16.5520338488593,
8.38780222307398));
#146476=CARTESIAN_POINT('Ctrl Pts',(17.921884774769,-16.524229652346,8.39218868508653));
#146477=CARTESIAN_POINT('Ctrl Pts',(18.001179344522,-16.49770476813,8.39637331947957));
#146478=CARTESIAN_POINT('Ctrl Pts',(18.0819223576085,-16.4750194242753,
8.40055795387262));
#146479=CARTESIAN_POINT('Ctrl Pts',(18.1637071353304,-16.4563305410157,
8.40474258826567));
#146480=CARTESIAN_POINT('Ctrl Pts',(18.2453755025443,-16.4376682590682,
8.40892126634961));
#146481=CARTESIAN_POINT('Ctrl Pts',(18.3280822444037,-16.4229912402357,
8.41309994443356));
#146482=CARTESIAN_POINT('Ctrl Pts',(18.4114039612995,-16.4124071594418,
8.4172786225175));
#146483=CARTESIAN_POINT('Ctrl Pts',(18.4962191600883,-16.4016333666062,
8.42153220040294));
#146484=CARTESIAN_POINT('Ctrl Pts',(18.5816711403846,-16.3951008398354,
8.42578577828838));
#146485=CARTESIAN_POINT('Ctrl Pts',(18.667300667149,-16.3928690539566,8.43003935617381));
#146486=CARTESIAN_POINT('Ctrl Pts',(18.7512700984448,-16.3906805356019,
8.43421047015176));
#146487=CARTESIAN_POINT('Ctrl Pts',(18.8354097724167,-16.3926275022743,
8.43838158412972));
#146488=CARTESIAN_POINT('Ctrl Pts',(18.9192815899905,-16.3987137386477,
8.44255269810767));
#146489=CARTESIAN_POINT('Ctrl Pts',(19.0031252635658,-16.4047979327256,
8.44672241242804));
#146490=CARTESIAN_POINT('Ctrl Pts',(19.086700800805,-16.4150186047168,8.45089212674841));
#146491=CARTESIAN_POINT('Ctrl Pts',(19.1695724543109,-16.4293274812125,
8.45506184106879));
#146492=CARTESIAN_POINT('Ctrl Pts',(19.2524411588877,-16.443635848537,8.45923140701283));
#146493=CARTESIAN_POINT('Ctrl Pts',(19.3346055763513,-16.4620320520102,
8.46340097295687));
#146494=CARTESIAN_POINT('Ctrl Pts',(19.4156387740957,-16.484416448902,8.46757053890091));
#146495=CARTESIAN_POINT('Ctrl Pts',(19.4995209991075,-16.5075878535744,
8.47188670163983));
#146496=CARTESIAN_POINT('Ctrl Pts',(19.5821904685913,-16.5350329790257,
8.47620286437876));
#146497=CARTESIAN_POINT('Ctrl Pts',(19.6631911444339,-16.5665851897195,
8.48051902711768));
#146498=CARTESIAN_POINT('Ctrl Pts',(19.7415532317808,-16.5971095904687,
8.48469459130936));
#146499=CARTESIAN_POINT('Ctrl Pts',(19.8183531671026,-16.6314773734769,
8.48887015550104));
#146500=CARTESIAN_POINT('Ctrl Pts',(19.8932005345678,-16.6694895135711,
8.49304571969272));
#146501=CARTESIAN_POINT('Ctrl Pts',(19.971828264631,-16.7094215564963,8.49743218170526));
#146502=CARTESIAN_POINT('Ctrl Pts',(20.0483004884278,-16.7533754937361,
8.5018186437178));
#146503=CARTESIAN_POINT('Ctrl Pts',(20.122198134957,-16.8010685882386,8.50620510573035));
#146504=CARTESIAN_POINT('Ctrl Pts',(20.1960957814862,-16.8487616827411,
8.51059156774289));
#146505=CARTESIAN_POINT('Ctrl Pts',(20.2674184246211,-16.9001935334404,
8.51497802975543));
#146506=CARTESIAN_POINT('Ctrl Pts',(20.3357880909559,-16.9550335727229,
8.51936449176797));
#146507=CARTESIAN_POINT('Ctrl Pts',(20.4010119675945,-17.0073503405056,
8.52354912616102));
#146508=CARTESIAN_POINT('Ctrl Pts',(20.4637914133142,-17.0629632902855,
8.52773376055407));
#146509=CARTESIAN_POINT('Ctrl Pts',(20.5237743555655,-17.1216154075823,
8.53191839494712));
#146510=CARTESIAN_POINT('Ctrl Pts',(20.5836719195229,-17.1801840408498,
8.53609707303107));
#146511=CARTESIAN_POINT('Ctrl Pts',(20.6407805603835,-17.2417829302056,
8.54027575111501));
#146512=CARTESIAN_POINT('Ctrl Pts',(20.6947805623984,-17.3061143459765,
8.54445442919895));
#146513=CARTESIAN_POINT('Ctrl Pts',(20.7497484756404,-17.3715988561409,
8.54870800708439));
#146514=CARTESIAN_POINT('Ctrl Pts',(20.8014948330692,-17.4399145156592,
8.55296158496982));
#146515=CARTESIAN_POINT('Ctrl Pts',(20.8497210505507,-17.5107073731346,
8.55721516285526));
#146516=CARTESIAN_POINT('Ctrl Pts',(20.8970123087006,-17.5801277729269,
8.56138627683321));
#146517=CARTESIAN_POINT('Ctrl Pts',(20.9409184275291,-17.6519297794778,
8.56555739081116));
#146518=CARTESIAN_POINT('Ctrl Pts',(20.9811990900048,-17.7257470693688,
8.56972850478911));
#146519=CARTESIAN_POINT('Ctrl Pts',(21.0214662359151,-17.7995395891551,
8.57389821910949));
#146520=CARTESIAN_POINT('Ctrl Pts',(21.058110121399,-17.8753456457563,8.57806793342986));
#146521=CARTESIAN_POINT('Ctrl Pts',(21.0909354749525,-17.9527727150891,
8.58223764775023));
#146522=CARTESIAN_POINT('Ctrl Pts',(21.123759660439,-18.0301970292345,8.58640721369427));
#146523=CARTESIAN_POINT('Ctrl Pts',(21.152765405382,-18.1092418175489,8.59057677963832));
#146524=CARTESIAN_POINT('Ctrl Pts',(21.1778054030264,-18.1894941625543,
8.59474634558237));
#146525=CARTESIAN_POINT('Ctrl Pts',(21.2037257760979,-18.272568081008,8.59906250832129));
#146526=CARTESIAN_POINT('Ctrl Pts',(21.2253961847597,-18.3569355479854,
8.6033786710602));
#146527=CARTESIAN_POINT('Ctrl Pts',(21.2427098983461,-18.4421229109477,
8.60769483379912));
#146528=CARTESIAN_POINT('Ctrl Pts',(21.2594596195335,-18.5245353045217,
8.6118703979908));
#146529=CARTESIAN_POINT('Ctrl Pts',(21.2721321012068,-18.6077145253799,
8.61604596218248));
#146530=CARTESIAN_POINT('Ctrl Pts',(21.2806833673555,-18.6912245670412,
8.62022152637416));
#146531=CARTESIAN_POINT('Ctrl Pts',(21.2896665376286,-18.7789525023805,
8.6246079883867));
#146532=CARTESIAN_POINT('Ctrl Pts',(21.2941011966021,-18.8670449731774,
8.62899445039924));
#146533=CARTESIAN_POINT('Ctrl Pts',(21.2939982462078,-18.9549965668354,
8.63338091241178));
#146534=CARTESIAN_POINT('Ctrl Pts',(21.2938952958136,-19.0429481604934,
8.63776737442432));
#146535=CARTESIAN_POINT('Ctrl Pts',(21.2892548426303,-19.1307583016182,
8.64215383643686));
#146536=CARTESIAN_POINT('Ctrl Pts',(21.2801502518719,-19.2179302444115,
8.6465402984494));
#146537=CARTESIAN_POINT('Ctrl Pts',(21.2712189219787,-19.303443300316,8.65084328584743));
#146538=CARTESIAN_POINT('Ctrl Pts',(21.2579577432873,-19.3886695757442,
8.65514627324547));
#146539=CARTESIAN_POINT('Ctrl Pts',(21.2403952844639,-19.4731359496497,
8.65944926064351));
#146540=CARTESIAN_POINT('Ctrl Pts',(21.2233438132473,-19.555144736568,8.66362705069559));
#146541=CARTESIAN_POINT('Ctrl Pts',(21.2022379883831,-19.6364367360942,
8.66780484074767));
#146542=CARTESIAN_POINT('Ctrl Pts',(21.1771565050491,-19.7165824297198,
8.67198263079975));
#146543=CARTESIAN_POINT('Ctrl Pts',(21.1520996601068,-19.7966493935124,
8.67615631686697));
#146544=CARTESIAN_POINT('Ctrl Pts',(21.1230750478627,-19.8755718507968,
8.68033000293419));
#146545=CARTESIAN_POINT('Ctrl Pts',(21.0902120830425,-19.9529318756661,
8.68450368900141));
#146546=CARTESIAN_POINT('Ctrl Pts',(21.0573715411633,-20.030239116519,8.68867452729403));
#146547=CARTESIAN_POINT('Ctrl Pts',(21.020698028392,-20.1059856204581,8.69284536558666));
#146548=CARTESIAN_POINT('Ctrl Pts',(20.9803698817383,-20.1797712956488,
8.69701620387929));
#146549=CARTESIAN_POINT('Ctrl Pts',(20.9400571536068,-20.253528760615,8.70118544754959));
#146550=CARTESIAN_POINT('Ctrl Pts',(20.8960927897238,-20.3253264840432,
8.70535469121989));
#146551=CARTESIAN_POINT('Ctrl Pts',(20.8487014677721,-20.3947881695532,
8.70952393489019));
#146552=CARTESIAN_POINT('Ctrl Pts',(20.801299148321,-20.4642659741502,8.71369414606367));
#146553=CARTESIAN_POINT('Ctrl Pts',(20.7504685369908,-20.5314062746653,
8.71786435723714));
#146554=CARTESIAN_POINT('Ctrl Pts',(20.6964775883006,-20.5958618297831,
8.72203456841062));
#146555=CARTESIAN_POINT('Ctrl Pts',(20.6424782982004,-20.6603273430554,
8.72620542386693));
#146556=CARTESIAN_POINT('Ctrl Pts',(20.5853180035682,-20.7221069405515,
8.73037627932324));
#146557=CARTESIAN_POINT('Ctrl Pts',(20.5253036567636,-20.7808879706711,
8.73454713477954));
#146558=CARTESIAN_POINT('Ctrl Pts',(20.465239521452,-20.8397177661257,8.73872145041956));
#146559=CARTESIAN_POINT('Ctrl Pts',(20.4023169479903,-20.8955437192182,
8.74289576605959));
#146560=CARTESIAN_POINT('Ctrl Pts',(20.3368776276693,-20.948092009582,8.74707008169962));
#146561=CARTESIAN_POINT('Ctrl Pts',(20.3225496097124,-20.9595975210122,
8.74798405313383));
#146562=CARTESIAN_POINT('Ctrl Pts',(20.308101057154,-20.9709460624804,8.74889802456805));
#146563=CARTESIAN_POINT('Ctrl Pts',(20.2935357468249,-20.9821350335323,
8.74981199600226));
#146564=CARTESIAN_POINT('Ctrl Pts',(20.290984793813,-20.9788230549133,7.94987222229573));
#146565=CARTESIAN_POINT('Ctrl Pts',(19.966954935699,-21.2283578947164,7.97013523654456));
#146566=CARTESIAN_POINT('Ctrl Pts',(18.7905372718575,-21.7718985897377,
8.03279018635388));
#146567=CARTESIAN_POINT('Ctrl Pts',(16.7471750902531,-21.0909114965219,
8.12726281551246));
#146568=CARTESIAN_POINT('Ctrl Pts',(16.1802303010149,-19.5894613347174,
8.20147243042223));
#146569=CARTESIAN_POINT('Ctrl Pts',(16.1744184492745,-18.9496462808249,
8.23329010977151));
#146570=CARTESIAN_POINT('',(16.1740010575059,-18.9543268925436,8.16670989022852));
#146571=CARTESIAN_POINT('Ctrl Pts',(20.2961055615625,-20.9854720348234,
7.8832969629626));
#146572=CARTESIAN_POINT('Ctrl Pts',(20.2876322375241,-20.9919974145329,
7.88383131339138));
#146573=CARTESIAN_POINT('Ctrl Pts',(19.6033699017491,-21.511539674794,7.92675759938063));
#146574=CARTESIAN_POINT('Ctrl Pts',(17.6781136533722,-21.788969486026,8.01207582093036));
#146575=CARTESIAN_POINT('Ctrl Pts',(16.2739022033865,-20.1719439048314,
8.1060124462569));
#146576=CARTESIAN_POINT('Ctrl Pts',(16.1718447244466,-19.1382186602577,
8.15755713602294));
#146577=CARTESIAN_POINT('Ctrl Pts',(16.1735502429248,-18.9543273023083,
8.16670989022852));
#146578=CARTESIAN_POINT('Ctrl Pts',(16.1740010575059,-18.9543268925436,
8.16670989022852));
#146579=CARTESIAN_POINT('Ctrl Pts',(16.173925195224,-18.8708647825268,8.17086478789788));
#146580=CARTESIAN_POINT('Ctrl Pts',(16.1779353066412,-18.7872780169979,
8.17501968556725));
#146581=CARTESIAN_POINT('Ctrl Pts',(16.1860403077383,-18.7040052286649,
8.17917458323661));
#146582=CARTESIAN_POINT('Ctrl Pts',(16.1940671586084,-18.621535375116,8.18328941845664));
#146583=CARTESIAN_POINT('Ctrl Pts',(16.2061102365111,-18.539373952273,8.18740425367668));
#146584=CARTESIAN_POINT('Ctrl Pts',(16.2221259449782,-18.4579466307084,
8.19151908889671));
#146585=CARTESIAN_POINT('Ctrl Pts',(16.238134689091,-18.3765547174256,8.1956321348003));
#146586=CARTESIAN_POINT('Ctrl Pts',(16.2581125446655,-18.2958967363639,
8.19974518070389));
#146587=CARTESIAN_POINT('Ctrl Pts',(16.2819644394348,-18.216390314281,8.20385822660748));
#146588=CARTESIAN_POINT('Ctrl Pts',(16.3058135810414,-18.136893069419,8.2079707977528));
#146589=CARTESIAN_POINT('Ctrl Pts',(16.3335357367832,-18.0585475732033,
8.21208336889813));
#146590=CARTESIAN_POINT('Ctrl Pts',(16.3649858005362,-17.9817568744182,
8.21619594004345));
#146591=CARTESIAN_POINT('Ctrl Pts',(16.3969970744395,-17.9035958852594,
8.2203818978976));
#146592=CARTESIAN_POINT('Ctrl Pts',(16.4328704281987,-17.8270462022341,
8.22456785575175));
#146593=CARTESIAN_POINT('Ctrl Pts',(16.4724022025116,-17.7525103575288,
8.2287538136059));
#146594=CARTESIAN_POINT('Ctrl Pts',(16.5112918107485,-17.6791852955861,
8.23287177349699));
#146595=CARTESIAN_POINT('Ctrl Pts',(16.553721559467,-17.6078095092637,8.23698973338808));
#146596=CARTESIAN_POINT('Ctrl Pts',(16.5994527799561,-17.5387384653211,
8.24110769327917));
#146597=CARTESIAN_POINT('Ctrl Pts',(16.6463167081173,-17.467956614176,8.24532765011484));
#146598=CARTESIAN_POINT('Ctrl Pts',(16.6966475137941,-17.3995956231065,
8.24954760695052));
#146599=CARTESIAN_POINT('Ctrl Pts',(16.7501447185243,-17.3340017854889,
8.25376756378619));
#146600=CARTESIAN_POINT('Ctrl Pts',(16.8036419232545,-17.2684079478714,
8.25798752062187));
#146601=CARTESIAN_POINT('Ctrl Pts',(16.8603051182412,-17.2055816046286,
8.26220747745754));
#146602=CARTESIAN_POINT('Ctrl Pts',(16.9197953580223,-17.1458268308308,
8.26642743429322));
#146603=CARTESIAN_POINT('Ctrl Pts',(16.9787876447051,-17.0865722243692,
8.27061206868627));
#146604=CARTESIAN_POINT('Ctrl Pts',(17.040795780927,-17.0301005497847,8.27479670307932));
#146605=CARTESIAN_POINT('Ctrl Pts',(17.1055265727615,-16.9767343731087,
8.27898133747237));
#146606=CARTESIAN_POINT('Ctrl Pts',(17.170165228326,-16.9234441565798,8.28316001555632));
#146607=CARTESIAN_POINT('Ctrl Pts',(17.2375184898922,-16.8732509480031,
8.28733869364027));
#146608=CARTESIAN_POINT('Ctrl Pts',(17.3072561423608,-16.8264407877716,
8.29151737172422));
#146609=CARTESIAN_POINT('Ctrl Pts',(17.3782437921302,-16.77879158906,8.29577094960966));
#146610=CARTESIAN_POINT('Ctrl Pts',(17.4517018138305,-16.7346482555831,
8.30002452749509));
#146611=CARTESIAN_POINT('Ctrl Pts',(17.5272463530815,-16.6942698045052,
8.30427810538053));
#146612=CARTESIAN_POINT('Ctrl Pts',(17.6013263140262,-16.6546741684935,
8.30844921935848));
#146613=CARTESIAN_POINT('Ctrl Pts',(17.6774121876528,-16.6186989652307,
8.31262033333643));
#146614=CARTESIAN_POINT('Ctrl Pts',(17.7551140500804,-16.5865439557984,
8.31679144731439));
#146615=CARTESIAN_POINT('Ctrl Pts',(17.8327898388978,-16.55439973629,8.32096116163476));
#146616=CARTESIAN_POINT('Ctrl Pts',(17.9120801148583,-16.5260733404923,
8.32513087595514));
#146617=CARTESIAN_POINT('Ctrl Pts',(17.9925737212266,-16.5017169401997,
8.32930059027551));
#146618=CARTESIAN_POINT('Ctrl Pts',(18.0730644632869,-16.4773614066124,
8.33347015621955));
#146619=CARTESIAN_POINT('Ctrl Pts',(18.1547580100548,-16.456975720069,8.3376397221636));
#146620=CARTESIAN_POINT('Ctrl Pts',(18.2372280581084,-16.440662181675,8.34180928810765));
#146621=CARTESIAN_POINT('Ctrl Pts',(18.3225976513137,-16.4237750793961,
8.34612545084656));
#146622=CARTESIAN_POINT('Ctrl Pts',(18.4087988479278,-16.4112519089493,
8.35044161358548));
#146623=CARTESIAN_POINT('Ctrl Pts',(18.4953492973486,-16.4031481325656,
8.3547577763244));
#146624=CARTESIAN_POINT('Ctrl Pts',(18.5790803749831,-16.3953083358451,
8.35893334051608));
#146625=CARTESIAN_POINT('Ctrl Pts',(18.6631378283663,-16.3916044048151,
8.36310890470776));
#146626=CARTESIAN_POINT('Ctrl Pts',(18.7470834485361,-16.392033433153,8.36728446889944));
#146627=CARTESIAN_POINT('Ctrl Pts',(18.8352689624189,-16.3924841306924,
8.37167093091198));
#146628=CARTESIAN_POINT('Ctrl Pts',(18.9233304658572,-16.3974962383813,
8.37605739292452));
#146629=CARTESIAN_POINT('Ctrl Pts',(19.0107666109438,-16.4070048638422,
8.38044385493706));
#146630=CARTESIAN_POINT('Ctrl Pts',(19.0982027560304,-16.4165134893032,
8.38483031694959));
#146631=CARTESIAN_POINT('Ctrl Pts',(19.1850129820695,-16.4305184650313,
8.38921677896213));
#146632=CARTESIAN_POINT('Ctrl Pts',(19.2707112385804,-16.4488937205181,
8.39360324097467));
#146633=CARTESIAN_POINT('Ctrl Pts',(19.3524663912739,-16.4664235032614,
8.39778787536771));
#146634=CARTESIAN_POINT('Ctrl Pts',(19.4335139608228,-16.4879954864411,
8.40197250976076));
#146635=CARTESIAN_POINT('Ctrl Pts',(19.5134240199301,-16.5135377392389,
8.40615714415381));
#146636=CARTESIAN_POINT('Ctrl Pts',(19.5932203369592,-16.5390436358014,
8.41033582223775));
#146637=CARTESIAN_POINT('Ctrl Pts',(19.6718819251547,-16.5685084380806,
8.41451450032169));
#146638=CARTESIAN_POINT('Ctrl Pts',(19.7489895306428,-16.6018093156755,
8.41869317840564));
#146639=CARTESIAN_POINT('Ctrl Pts',(19.827479234543,-16.6357070875684,8.42294675629107));
#146640=CARTESIAN_POINT('Ctrl Pts',(19.904358226068,-16.6735797096679,8.42720033417651));
#146641=CARTESIAN_POINT('Ctrl Pts',(19.9792009396772,-16.7152446222649,
8.43145391206194));
#146642=CARTESIAN_POINT('Ctrl Pts',(20.0525926812396,-16.7561017792288,
8.4356250260399));
#146643=CARTESIAN_POINT('Ctrl Pts',(20.1240259742956,-16.8006052628958,
8.43979614001785));
#146644=CARTESIAN_POINT('Ctrl Pts',(20.1931217929874,-16.8485353358734,
8.44396725399581));
#146645=CARTESIAN_POINT('Ctrl Pts',(20.2621944259099,-16.8964493254521,
8.44813696831618));
#146646=CARTESIAN_POINT('Ctrl Pts',(20.3289307645448,-16.9477873587841,
8.45230668263656));
#146647=CARTESIAN_POINT('Ctrl Pts',(20.3929803051522,-17.0022860858277,
8.45647639695693));
#146648=CARTESIAN_POINT('Ctrl Pts',(20.457027566602,-17.0567828735727,8.46064596290098));
#146649=CARTESIAN_POINT('Ctrl Pts',(20.518387870305,-17.1144398326397,8.46481552884503));
#146650=CARTESIAN_POINT('Ctrl Pts',(20.5767444472642,-17.1749538829628,
8.46898509478907));
#146651=CARTESIAN_POINT('Ctrl Pts',(20.6371527694786,-17.2375955326431,
8.47330125752799));
#146652=CARTESIAN_POINT('Ctrl Pts',(20.6943418467819,-17.3032985427184,
8.47761742026691));
#146653=CARTESIAN_POINT('Ctrl Pts',(20.7480039569826,-17.3716873533195,
8.48193358300583));
#146654=CARTESIAN_POINT('Ctrl Pts',(20.7999180295879,-17.4378484056085,
8.48610914719751));
#146655=CARTESIAN_POINT('Ctrl Pts',(20.848531154665,-17.5065225539075,8.4902847113892));
#146656=CARTESIAN_POINT('Ctrl Pts',(20.8936085817713,-17.5773397606901,
8.49446027558088));
#146657=CARTESIAN_POINT('Ctrl Pts',(20.9409627625594,-17.6517337762353,
8.49884673759342));
#146658=CARTESIAN_POINT('Ctrl Pts',(20.9844143947689,-17.7284925234218,
8.50323319960595));
#146659=CARTESIAN_POINT('Ctrl Pts',(21.0237466725066,-17.8071593229863,
8.50761966161849));
#146660=CARTESIAN_POINT('Ctrl Pts',(21.0630789502442,-17.8858261225508,
8.51200612363103));
#146661=CARTESIAN_POINT('Ctrl Pts',(21.0982917108611,-17.9664004123699,
8.51639258564357));
#146662=CARTESIAN_POINT('Ctrl Pts',(21.1292278697973,-18.0484052613331,
8.5207790476561));
#146663=CARTESIAN_POINT('Ctrl Pts',(21.1587406102024,-18.1266369456354,
8.52496368204915));
#146664=CARTESIAN_POINT('Ctrl Pts',(21.1844714983967,-18.2064616309202,
8.5291483164422));
#146665=CARTESIAN_POINT('Ctrl Pts',(21.2062483053235,-18.2874788815808,
8.53333295083525));
#146666=CARTESIAN_POINT('Ctrl Pts',(21.2279941156611,-18.3683808142131,
8.5375116289192));
#146667=CARTESIAN_POINT('Ctrl Pts',(21.2457969056056,-18.4504715000491,
8.54169030700315));
#146668=CARTESIAN_POINT('Ctrl Pts',(21.2595330219157,-18.5333319271626,
8.5458689850871));
#146669=CARTESIAN_POINT('Ctrl Pts',(21.2735153482387,-18.6176775678812,
8.55012256297253));
#146670=CARTESIAN_POINT('Ctrl Pts',(21.2832836065124,-18.7028203654208,
8.55437614085796));
#146671=CARTESIAN_POINT('Ctrl Pts',(21.2887609500061,-18.7883036704011,
8.5586297187434));
#146672=CARTESIAN_POINT('Ctrl Pts',(21.2941321045079,-18.8721297147074,
8.56280083272135));
#146673=CARTESIAN_POINT('Ctrl Pts',(21.2953772042646,-18.9562827012374,
8.5669719466993));
#146674=CARTESIAN_POINT('Ctrl Pts',(21.2924758541409,-19.0403249895437,
8.57114306067725));
#146675=CARTESIAN_POINT('Ctrl Pts',(21.2895754775933,-19.1243390766486,
8.57531277499763));
#146676=CARTESIAN_POINT('Ctrl Pts',(21.2825314303294,-19.2082420799258,
8.57948248931799));
#146677=CARTESIAN_POINT('Ctrl Pts',(21.2713754270314,-19.2915967348155,
8.58365220363837));
#146678=CARTESIAN_POINT('Ctrl Pts',(21.2602198207118,-19.3749484235889,
8.58782176958241));
#146679=CARTESIAN_POINT('Ctrl Pts',(21.2449526111524,-19.4577513469167,
8.59199133552645));
#146680=CARTESIAN_POINT('Ctrl Pts',(21.2256571796747,-19.5395751007108,
8.59616090147049));
#146681=CARTESIAN_POINT('Ctrl Pts',(21.2056833446298,-19.624275676748,8.60047706420941));
#146682=CARTESIAN_POINT('Ctrl Pts',(21.1813928737509,-19.7079264335899,
8.60479322694833));
#146683=CARTESIAN_POINT('Ctrl Pts',(21.1529349892686,-19.7900653421377,
8.60910938968725));
#146684=CARTESIAN_POINT('Ctrl Pts',(21.12540411738,-19.869528584379,8.61328495387892));
#146685=CARTESIAN_POINT('Ctrl Pts',(21.0939733891636,-19.9475765433409,
8.6174605180706));
#146686=CARTESIAN_POINT('Ctrl Pts',(21.0588268816571,-20.0238115367567,
8.62163608226228));
#146687=CARTESIAN_POINT('Ctrl Pts',(21.0219052076092,-20.1038969784584,
8.62602254427482));
#146688=CARTESIAN_POINT('Ctrl Pts',(20.9808827929501,-20.181980978784,8.63040900628737));
#146689=CARTESIAN_POINT('Ctrl Pts',(20.936026279751,-20.257634046464,8.63479546829991));
#146690=CARTESIAN_POINT('Ctrl Pts',(20.8911697665519,-20.333287114144,8.63918193031245));
#146691=CARTESIAN_POINT('Ctrl Pts',(20.842479539431,-20.4065088081494,8.64356839232499));
#146692=CARTESIAN_POINT('Ctrl Pts',(20.790271595083,-20.4769088914603,8.64795485433753));
#146693=CARTESIAN_POINT('Ctrl Pts',(20.7404694331031,-20.5440648845997,
8.6521391847952));
#146694=CARTESIAN_POINT('Ctrl Pts',(20.6872812569759,-20.6089035367256,
8.65632351525286));
#146695=CARTESIAN_POINT('Ctrl Pts',(20.6309504906871,-20.6710633600545,
8.66050784571053));
#146696=CARTESIAN_POINT('Ctrl Pts',(20.5747060923804,-20.7331278781203,
8.66468576063008));
#146697=CARTESIAN_POINT('Ctrl Pts',(20.5153289851622,-20.7925213917038,
8.66886367554964));
#146698=CARTESIAN_POINT('Ctrl Pts',(20.4531043975684,-20.8489133006706,
8.67304159046919));
#146699=CARTESIAN_POINT('Ctrl Pts',(20.4017904533731,-20.8954172853764,
8.67648693741844));
#146700=CARTESIAN_POINT('Ctrl Pts',(20.34854091394,-20.9398804430942,8.67993228436769));
#146701=CARTESIAN_POINT('Ctrl Pts',(20.2935357468249,-20.9821350335323,
8.68337763131693));
#146702=CARTESIAN_POINT('Origin',(18.734,-18.952,-1.76670989022851));
#146703=CARTESIAN_POINT('',(20.2954164701606,-20.9846205560609,9.5499633223245));
#146704=CARTESIAN_POINT('',(20.2935357468249,-20.9821350335323,9.48328065736197));
#146705=CARTESIAN_POINT('',(20.2935357468249,-20.9821350335323,-1.76670989022851));
#146706=CARTESIAN_POINT('',(16.1736699172806,-18.9526425113319,9.03329016588271));
#146707=CARTESIAN_POINT('Ctrl Pts',(16.1699656690245,-18.9526308403706,
9.03329079541859));
#146708=CARTESIAN_POINT('Ctrl Pts',(16.1727141322405,-18.1388729144851,
9.07394170533744));
#146709=CARTESIAN_POINT('Ctrl Pts',(17.0319371704071,-16.4715241260563,
9.15698455081677));
#146710=CARTESIAN_POINT('Ctrl Pts',(19.8732646791955,-16.1474739147344,
9.28241933185658));
#146711=CARTESIAN_POINT('Ctrl Pts',(21.7088249748179,-18.3919045247491,
9.40959513853799));
#146712=CARTESIAN_POINT('Ctrl Pts',(21.0821529663045,-20.3261355156988,
9.49877646869399));
#146713=CARTESIAN_POINT('Ctrl Pts',(20.3656977374887,-20.9314719539678,
9.54556586328949));
#146714=CARTESIAN_POINT('Ctrl Pts',(20.2954164701606,-20.9846205560609,
9.5499633223245));
#146715=CARTESIAN_POINT('Ctrl Pts',(20.2935357468249,-20.9821350335323,
8.74981199600226));
#146716=CARTESIAN_POINT('Ctrl Pts',(20.226866111391,-21.0333501881746,8.75399550743729));
#146717=CARTESIAN_POINT('Ctrl Pts',(20.1577482566508,-21.081218427346,8.75817901887232));
#146718=CARTESIAN_POINT('Ctrl Pts',(20.0865601504742,-21.1255181249185,
8.76236253030735));
#146719=CARTESIAN_POINT('Ctrl Pts',(20.0221613392068,-21.1655929072999,
8.76614705524851));
#146720=CARTESIAN_POINT('Ctrl Pts',(19.9560688974245,-21.2027478334321,
8.76993158018967));
#146721=CARTESIAN_POINT('Ctrl Pts',(19.8885775886028,-21.2368524223451,
8.77371610513083));
#146722=CARTESIAN_POINT('Ctrl Pts',(19.8139509296381,-21.2745626337838,
8.77790073952388));
#146723=CARTESIAN_POINT('Ctrl Pts',(19.7373359438749,-21.3086830520783,
8.78208537391693));
#146724=CARTESIAN_POINT('Ctrl Pts',(19.6591123506694,-21.3389996101045,
8.78627000830997));
#146725=CARTESIAN_POINT('Ctrl Pts',(19.5810000990667,-21.3692730162627,
8.79044868639392));
#146726=CARTESIAN_POINT('Ctrl Pts',(19.5012842132702,-21.3957531518832,
8.79462736447786));
#146727=CARTESIAN_POINT('Ctrl Pts',(19.4203680775091,-21.4182722603509,
8.79880604256181));
#146728=CARTESIAN_POINT('Ctrl Pts',(19.3380015781678,-21.4411950076538,
8.80305962044724));
#146729=CARTESIAN_POINT('Ctrl Pts',(19.2543918069889,-21.4600131107993,
8.80731319833268));
#146730=CARTESIAN_POINT('Ctrl Pts',(19.1699845756622,-21.4746013259698,
8.81156677621811));
#146731=CARTESIAN_POINT('Ctrl Pts',(19.0872137432219,-21.4889067201227,
8.81573789019606));
#146732=CARTESIAN_POINT('Ctrl Pts',(19.0036765695344,-21.4991446900207,
8.81990900417402));
#146733=CARTESIAN_POINT('Ctrl Pts',(18.9198060037776,-21.5052481526401,
8.82408011815197));
#146734=CARTESIAN_POINT('Ctrl Pts',(18.8359635815991,-21.5113495671838,
8.82824983247234));
#146735=CARTESIAN_POINT('Ctrl Pts',(18.7517884479705,-21.5133191964338,
8.83241954679272));
#146736=CARTESIAN_POINT('Ctrl Pts',(18.6677187513895,-21.5111418085137,
8.83658926111309));
#146737=CARTESIAN_POINT('Ctrl Pts',(18.5836520463691,-21.5089644980744,
8.84075882705713));
#146738=CARTESIAN_POINT('Ctrl Pts',(18.4996912307932,-21.502640476632,8.84492839300118));
#146739=CARTESIAN_POINT('Ctrl Pts',(18.4162731576902,-21.4922066163357,
8.84909795894522));
#146740=CARTESIAN_POINT('Ctrl Pts',(18.3299222080443,-21.481405914383,8.85341412168414));
#146741=CARTESIAN_POINT('Ctrl Pts',(18.2441533999762,-21.4662010579768,
8.85773028442306));
#146742=CARTESIAN_POINT('Ctrl Pts',(18.1594420717104,-21.4466910003124,
8.86204644716198));
#146743=CARTESIAN_POINT('Ctrl Pts',(18.0774902060527,-21.4278164807242,
8.86622201135366));
#146744=CARTESIAN_POINT('Ctrl Pts',(17.996528423794,-21.404913110059,8.87039757554534));
#146745=CARTESIAN_POINT('Ctrl Pts',(17.9169718130409,-21.3781213781908,
8.87457313973702));
#146746=CARTESIAN_POINT('Ctrl Pts',(17.8333969870066,-21.3499764596372,
8.87895960174956));
#146747=CARTESIAN_POINT('Ctrl Pts',(17.7513735563979,-21.3175402693169,
8.88334606376211));
#146748=CARTESIAN_POINT('Ctrl Pts',(17.6713570660693,-21.2810319866776,
8.88773252577465));
#146749=CARTESIAN_POINT('Ctrl Pts',(17.5913405757408,-21.2445237040383,
8.89211898778719));
#146750=CARTESIAN_POINT('Ctrl Pts',(17.513331505326,-21.203943664325,8.89650544979973));
#146751=CARTESIAN_POINT('Ctrl Pts',(17.4377516489576,-21.159564316712,8.90089191181227));
#146752=CARTESIAN_POINT('Ctrl Pts',(17.3656493338169,-21.1172269286685,
8.90507654620532));
#146753=CARTESIAN_POINT('Ctrl Pts',(17.295489223029,-21.0712745855039,8.90926118059836));
#146754=CARTESIAN_POINT('Ctrl Pts',(17.227656848054,-21.0219107006307,8.91344581499141));
#146755=CARTESIAN_POINT('Ctrl Pts',(17.1599210240689,-20.9726170791376,
8.91762449307535));
#146756=CARTESIAN_POINT('Ctrl Pts',(17.0945067235341,-20.919921829671,8.9218031711593));
#146757=CARTESIAN_POINT('Ctrl Pts',(17.0317733474473,-20.8640733310569,
8.92598184924324));
#146758=CARTESIAN_POINT('Ctrl Pts',(16.9679155206798,-20.8072237882428,
8.93023542712867));
#146759=CARTESIAN_POINT('Ctrl Pts',(16.9068360906094,-20.7471070845336,
8.93448900501411));
#146760=CARTESIAN_POINT('Ctrl Pts',(16.8488816768787,-20.6840302849062,
8.93874258289955));
#146761=CARTESIAN_POINT('Ctrl Pts',(16.7920508225469,-20.6221763521239,
8.9429136968775));
#146762=CARTESIAN_POINT('Ctrl Pts',(16.7382252223473,-20.5574764280243,
8.94708481085545));
#146763=CARTESIAN_POINT('Ctrl Pts',(16.6876956296652,-20.4902582435822,
8.9512559248334));
#146764=CARTESIAN_POINT('Ctrl Pts',(16.6371829926759,-20.423062614851,8.95542563915378));
#146765=CARTESIAN_POINT('Ctrl Pts',(16.5899644428517,-20.3533507714291,
8.95959535347415));
#146766=CARTESIAN_POINT('Ctrl Pts',(16.546289949262,-20.2814828821387,8.96376506779452));
#146767=CARTESIAN_POINT('Ctrl Pts',(16.5026170097982,-20.2096175502162,
8.96793463373857));
#146768=CARTESIAN_POINT('Ctrl Pts',(16.4624881140047,-20.1355967185418,
8.97210419968261));
#146769=CARTESIAN_POINT('Ctrl Pts',(16.426108718498,-20.0598076695739,8.97627376562665));
#146770=CARTESIAN_POINT('Ctrl Pts',(16.388450268324,-19.9813539711403,8.98058992836557));
#146771=CARTESIAN_POINT('Ctrl Pts',(16.3548101172678,-19.9010058763734,
8.98490609110449));
#146772=CARTESIAN_POINT('Ctrl Pts',(16.3253623529171,-19.8192166309839,
8.98922225384341));
#146773=CARTESIAN_POINT('Ctrl Pts',(16.2968738463928,-19.7400916616603,
8.99339781803509));
#146774=CARTESIAN_POINT('Ctrl Pts',(16.2723088794103,-19.6596184551162,
8.99757338222677));
#146775=CARTESIAN_POINT('Ctrl Pts',(16.2517740015378,-19.5782220792646,
9.00174894641845));
#146776=CARTESIAN_POINT('Ctrl Pts',(16.230201955801,-19.4927145659702,9.00613540843099));
#146777=CARTESIAN_POINT('Ctrl Pts',(16.213077931431,-19.4061887466983,9.01052187044353));
#146778=CARTESIAN_POINT('Ctrl Pts',(16.2004642109875,-19.3191463002578,
9.01490833245608));
#146779=CARTESIAN_POINT('Ctrl Pts',(16.1878504905441,-19.2321038538173,
9.01929479446862));
#146780=CARTESIAN_POINT('Ctrl Pts',(16.179747051756,-19.144545364966,9.02368125648116));
#146781=CARTESIAN_POINT('Ctrl Pts',(16.1761531171477,-19.0569729673897,
9.0280677184937));
#146782=CARTESIAN_POINT('Ctrl Pts',(16.1747268399112,-19.022219269613,9.0298085155863));
#146783=CARTESIAN_POINT('Ctrl Pts',(16.1740088273484,-18.9874363059254,
9.0315493126789));
#146784=CARTESIAN_POINT('Ctrl Pts',(16.1740000808904,-18.9526435515772,
9.0332901097715));
#146785=CARTESIAN_POINT('',(16.174000001606,-18.9519093211995,8.96670989026365));
#146786=CARTESIAN_POINT('Ctrl Pts',(20.2935357468249,-20.9821350335323,
8.68337763131693));
#146787=CARTESIAN_POINT('Ctrl Pts',(20.2269370171092,-21.0332957188903,
8.68754916178006));
#146788=CARTESIAN_POINT('Ctrl Pts',(20.1577639337492,-21.0812174419311,
8.69172069224319));
#146789=CARTESIAN_POINT('Ctrl Pts',(20.0863674114257,-21.1256380527848,
8.69589222270632));
#146790=CARTESIAN_POINT('Ctrl Pts',(20.0149990010201,-21.1700411733108,
8.70006211065636));
#146791=CARTESIAN_POINT('Ctrl Pts',(19.941409280332,-21.2109456764381,8.7042319986064));
#146792=CARTESIAN_POINT('Ctrl Pts',(19.865978108956,-21.2481327402492,8.70840188655645));
#146793=CARTESIAN_POINT('Ctrl Pts',(19.7905540105462,-21.2853163171353,
8.71257138350797));
#146794=CARTESIAN_POINT('Ctrl Pts',(19.7132892174036,-21.3187829444825,
8.71674088045949));
#146795=CARTESIAN_POINT('Ctrl Pts',(19.6345869215609,-21.3483604062648,
8.72091037741101));
#146796=CARTESIAN_POINT('Ctrl Pts',(19.5558683969919,-21.3779439670372,
8.72508073412939));
#146797=CARTESIAN_POINT('Ctrl Pts',(19.4757122121442,-21.4036366092316,
8.72925109084776));
#146798=CARTESIAN_POINT('Ctrl Pts',(19.3945389058334,-21.42531525566,8.73342144756614));
#146799=CARTESIAN_POINT('Ctrl Pts',(19.3132745301638,-21.4470182236359,
8.73759648306045));
#146800=CARTESIAN_POINT('Ctrl Pts',(19.230991201076,-21.464698091023,8.74177151855476));
#146801=CARTESIAN_POINT('Ctrl Pts',(19.1481213446228,-21.4782825479205,
8.74594655404907));
#146802=CARTESIAN_POINT('Ctrl Pts',(19.0651969871444,-21.4918759389089,
8.75012433533931));
#146803=CARTESIAN_POINT('Ctrl Pts',(18.9816857911789,-21.5013685073529,
8.75430211662955));
#146804=CARTESIAN_POINT('Ctrl Pts',(18.8980246552272,-21.5067398913544,
8.75847989791979));
#146805=CARTESIAN_POINT('Ctrl Pts',(18.8142288831572,-21.5121199195404,
8.76266440252606));
#146806=CARTESIAN_POINT('Ctrl Pts',(18.730283148478,-21.5133655227373,8.76684890713234));
#146807=CARTESIAN_POINT('Ctrl Pts',(18.6466231642283,-21.5105084108852,
8.77103341173861));
#146808=CARTESIAN_POINT('Ctrl Pts',(18.6193179957145,-21.5095758991081,
8.77239916149873));
#146809=CARTESIAN_POINT('Ctrl Pts',(18.5920432114748,-21.5082067533533,
8.77376491125885));
#146810=CARTESIAN_POINT('Ctrl Pts',(18.5648137584889,-21.5064032601928,
8.77513066101898));
#146811=CARTESIAN_POINT('Ctrl Pts',(18.481383170547,-21.5008773873516,8.77931529541203));
#146812=CARTESIAN_POINT('Ctrl Pts',(18.3980683312292,-21.4912494832413,
8.78349992980508));
#146813=CARTESIAN_POINT('Ctrl Pts',(18.3153050503464,-21.4775285662876,
8.78768456419813));
#146814=CARTESIAN_POINT('Ctrl Pts',(18.2326595727498,-21.4638271793608,
8.79186324228208));
#146815=CARTESIAN_POINT('Ctrl Pts',(18.1505645441386,-21.4460444262516,
8.79604192036603));
#146816=CARTESIAN_POINT('Ctrl Pts',(18.0694525718369,-21.4242412333188,
8.80022059844998));
#146817=CARTESIAN_POINT('Ctrl Pts',(17.9868867257261,-21.4020472338225,
8.80447417633541));
#146818=CARTESIAN_POINT('Ctrl Pts',(17.905340006223,-21.3756872759157,8.80872775422084));
#146819=CARTESIAN_POINT('Ctrl Pts',(17.8252599013634,-21.3452804752327,
8.81298133210628));
#146820=CARTESIAN_POINT('Ctrl Pts',(17.7467323056,-21.3154631697149,8.81715244608422));
#146821=CARTESIAN_POINT('Ctrl Pts',(17.669615415452,-21.2817547038761,8.82132356006217));
#146822=CARTESIAN_POINT('Ctrl Pts',(17.5943160431832,-21.2443177089082,
8.82549467404012));
#146823=CARTESIAN_POINT('Ctrl Pts',(17.5190419383459,-21.2068932762856,
8.82966438836049));
#146824=CARTESIAN_POINT('Ctrl Pts',(17.4455845517327,-21.1657430039568,
8.83383410268086));
#146825=CARTESIAN_POINT('Ctrl Pts',(17.3743287784394,-21.1210768011437,
8.83800381700123));
#146826=CARTESIAN_POINT('Ctrl Pts',(17.3030755407324,-21.0764121877459,
8.84217338294526));
#146827=CARTESIAN_POINT('Ctrl Pts',(17.2340241499108,-21.0282321376739,
8.8463429488893));
#146828=CARTESIAN_POINT('Ctrl Pts',(17.1675318647118,-20.9767907499607,
8.85051251483333));
#146829=CARTESIAN_POINT('Ctrl Pts',(17.098701792792,-20.9235407465152,8.85482867757225));
#146830=CARTESIAN_POINT('Ctrl Pts',(17.0326145482173,-20.8667961238599,
8.85914484031117));
#146831=CARTESIAN_POINT('Ctrl Pts',(16.9696289167235,-20.8068840072893,
8.86346100305009));
#146832=CARTESIAN_POINT('Ctrl Pts',(16.9086950355507,-20.7489235216145,
8.86763656724177));
#146833=CARTESIAN_POINT('Ctrl Pts',(16.8506640912075,-20.6879991088315,
8.87181213143345));
#146834=CARTESIAN_POINT('Ctrl Pts',(16.7958218659397,-20.6244429797905,
8.87598769562512));
#146835=CARTESIAN_POINT('Ctrl Pts',(16.7382096902485,-20.5576767817618,
8.88037415763767));
#146836=CARTESIAN_POINT('Ctrl Pts',(16.6841171816934,-20.4880064858708,
8.88476061965022));
#146837=CARTESIAN_POINT('Ctrl Pts',(16.6338248927157,-20.4158526287654,
8.88914708166276));
#146838=CARTESIAN_POINT('Ctrl Pts',(16.583532603738,-20.34369877166,8.89353354367531));
#146839=CARTESIAN_POINT('Ctrl Pts',(16.537040776547,-20.2690618860433,8.89792000568785));
#146840=CARTESIAN_POINT('Ctrl Pts',(16.4945737975988,-20.192391181845,8.9023064677004));
#146841=CARTESIAN_POINT('Ctrl Pts',(16.4520961746315,-20.115701260729,8.90669402914565));
#146842=CARTESIAN_POINT('Ctrl Pts',(16.4134992022811,-20.0367143701648,
8.91108159059091));
#146843=CARTESIAN_POINT('Ctrl Pts',(16.3790251742675,-19.955839414531,8.91546915203616));
#146844=CARTESIAN_POINT('Ctrl Pts',(16.3446454932948,-19.8751857940064,
8.91984470579147));
#146845=CARTESIAN_POINT('Ctrl Pts',(16.3143664333075,-19.7926547636182,
8.92422025954678));
#146846=CARTESIAN_POINT('Ctrl Pts',(16.288384114166,-19.7086788876112,8.9285958133021));
#146847=CARTESIAN_POINT('Ctrl Pts',(16.262443998658,-19.624839415405,8.93296425975242));
#146848=CARTESIAN_POINT('Ctrl Pts',(16.2407868563188,-19.5395601416143,
8.93733270620274));
#146849=CARTESIAN_POINT('Ctrl Pts',(16.2235607960526,-19.4532933305799,
8.94170115265305));
#146850=CARTESIAN_POINT('Ctrl Pts',(16.2063704951608,-19.3672055997965,
8.94606053069714));
#146851=CARTESIAN_POINT('Ctrl Pts',(16.193593030381,-19.2801348014828,8.95041990874123));
#146852=CARTESIAN_POINT('Ctrl Pts',(16.1853263642748,-19.1925466660734,
8.95477928678532));
#146853=CARTESIAN_POINT('Ctrl Pts',(16.1777850503447,-19.1126438833577,
8.95875615459972));
#146854=CARTESIAN_POINT('Ctrl Pts',(16.1739971536887,-19.0323109723967,
8.96273302241411));
#146855=CARTESIAN_POINT('Ctrl Pts',(16.174000001606,-18.95190932191,8.96670989022851));
#146856=CARTESIAN_POINT('Ctrl Pts',(16.174000001606,-18.9519093211995,8.96670989026365));
#146857=CARTESIAN_POINT('Ctrl Pts',(16.1740031377284,-18.8633718327363,
8.97108917708311));
#146858=CARTESIAN_POINT('Ctrl Pts',(16.1786036643305,-18.7749281972307,
8.97546846390257));
#146859=CARTESIAN_POINT('Ctrl Pts',(16.1877467776185,-18.6870575014995,
8.97984775072203));
#146860=CARTESIAN_POINT('Ctrl Pts',(16.1969159526897,-18.5989363367042,
8.9842395203819));
#146861=CARTESIAN_POINT('Ctrl Pts',(16.2106535575188,-18.5113917635125,
8.98863129004177));
#146862=CARTESIAN_POINT('Ctrl Pts',(16.2288531973792,-18.4248951742598,
8.99302305970163));
#146863=CARTESIAN_POINT('Ctrl Pts',(16.2470794228643,-18.3382722327341,
8.99742124475989));
#146864=CARTESIAN_POINT('Ctrl Pts',(16.2697805833342,-18.2527007028955,
9.00181942981814));
#146865=CARTESIAN_POINT('Ctrl Pts',(16.2968004138022,-18.1686366251622,
9.00621761487639));
#146866=CARTESIAN_POINT('Ctrl Pts',(16.323895396912,-18.0843387325822,9.01062803299535));
#146867=CARTESIAN_POINT('Ctrl Pts',(16.3553329301084,-18.0015570394279,
9.0150384511143));
#146868=CARTESIAN_POINT('Ctrl Pts',(16.3909082116846,-17.9207285170583,
9.01944886923326));
#146869=CARTESIAN_POINT('Ctrl Pts',(16.4178853374885,-17.8594353629383,
9.02279333761612));
#146870=CARTESIAN_POINT('Ctrl Pts',(16.4472408225495,-17.7992649146788,
9.02613780599898));
#146871=CARTESIAN_POINT('Ctrl Pts',(16.4788683829461,-17.7403971815138,
9.02948227438184));
#146872=CARTESIAN_POINT('Ctrl Pts',(16.5184411227219,-17.6667412480013,
9.03366690877489));
#146873=CARTESIAN_POINT('Ctrl Pts',(16.5616998679758,-17.5948890389389,
9.03785154316794));
#146874=CARTESIAN_POINT('Ctrl Pts',(16.6084559713663,-17.5252335221418,
9.04203617756098));
#146875=CARTESIAN_POINT('Ctrl Pts',(16.6551455232309,-17.4556771513513,
9.04621485564493));
#146876=CARTESIAN_POINT('Ctrl Pts',(16.7053222910481,-17.3883116408714,
9.05039353372887));
#146877=CARTESIAN_POINT('Ctrl Pts',(16.7587517035101,-17.3235055519856,
9.05457221181281));
#146878=CARTESIAN_POINT('Ctrl Pts',(16.8131387997914,-17.2575378605319,
9.05882578969825));
#146879=CARTESIAN_POINT('Ctrl Pts',(16.8708960667841,-17.1942226731586,
9.06307936758369));
#146880=CARTESIAN_POINT('Ctrl Pts',(16.9317298045576,-17.1339180044288,
9.06733294546913));
#146881=CARTESIAN_POINT('Ctrl Pts',(16.9913841616171,-17.0747824593773,
9.07150405944708));
#146882=CARTESIAN_POINT('Ctrl Pts',(17.053996425417,-17.0185420838703,9.07567517342503));
#146883=CARTESIAN_POINT('Ctrl Pts',(17.1192501263854,-16.9654998500726,
9.07984628740298));
#146884=CARTESIAN_POINT('Ctrl Pts',(17.1844819308442,-16.9124754151088,
9.08401600172335));
#146885=CARTESIAN_POINT('Ctrl Pts',(17.2523530554691,-16.8626472804565,
9.08818571604372));
#146886=CARTESIAN_POINT('Ctrl Pts',(17.3225130695872,-16.8162788933773,
9.0923554303641));
#146887=CARTESIAN_POINT('Ctrl Pts',(17.3926705871108,-16.7699121562842,
9.09652499630814));
#146888=CARTESIAN_POINT('Ctrl Pts',(17.4651164479273,-16.7270051749183,
9.10069456225218));
#146889=CARTESIAN_POINT('Ctrl Pts',(17.5394714392695,-16.6877779442821,
9.10486412819623));
#146890=CARTESIAN_POINT('Ctrl Pts',(17.6164406603806,-16.6471715326088,
9.10918029093515));
#146891=CARTESIAN_POINT('Ctrl Pts',(17.6954552934392,-16.6105086923157,
9.11349645367407));
#146892=CARTESIAN_POINT('Ctrl Pts',(17.7760690203242,-16.5779805733361,
9.11781261641299));
#146893=CARTESIAN_POINT('Ctrl Pts',(17.854056763535,-16.546512054411,9.12198818060467));
#146894=CARTESIAN_POINT('Ctrl Pts',(17.9335405590282,-16.5189131263824,
9.12616374479635));
#146895=CARTESIAN_POINT('Ctrl Pts',(18.0140996850994,-16.4953063812095,
9.13033930898803));
#146896=CARTESIAN_POINT('Ctrl Pts',(18.0987276611173,-16.4705073154576,
9.13472577100057));
#146897=CARTESIAN_POINT('Ctrl Pts',(18.1845418843914,-16.4501144565313,
9.13911223301311));
#146898=CARTESIAN_POINT('Ctrl Pts',(18.2710433987721,-16.4342090663879,
9.14349869502565));
#146899=CARTESIAN_POINT('Ctrl Pts',(18.3575449131528,-16.4183036762444,
9.14788515703819));
#146900=CARTESIAN_POINT('Ctrl Pts',(18.4447331334585,-16.406885754803,9.15227161905074));
#146901=CARTESIAN_POINT('Ctrl Pts',(18.5321062576864,-16.3999735665917,
9.15665808106328));
#146902=CARTESIAN_POINT('Ctrl Pts',(18.6154592149507,-16.3933794184063,
9.16084271545632));
#146903=CARTESIAN_POINT('Ctrl Pts',(18.6992906902525,-16.3908609393394,
9.16502734984937));
#146904=CARTESIAN_POINT('Ctrl Pts',(18.7831681486199,-16.3924722128562,
9.16921198424242));
#146905=CARTESIAN_POINT('Ctrl Pts',(18.8669262178074,-16.3940811929245,
9.17339066232636));
#146906=CARTESIAN_POINT('Ctrl Pts',(18.9507296840397,-16.3998082408783,
9.17756934041031));
#146907=CARTESIAN_POINT('Ctrl Pts',(19.0341416766035,-16.4096556146018,
9.18174801849426));
#146908=CARTESIAN_POINT('Ctrl Pts',(19.1190487691868,-16.4196794954222,
9.1860015963797));
#146909=CARTESIAN_POINT('Ctrl Pts',(19.203549735092,-16.4339729066197,9.19025517426513));
#146910=CARTESIAN_POINT('Ctrl Pts',(19.2871845665267,-16.4524826795246,
9.19450875215056));
#146911=CARTESIAN_POINT('Ctrl Pts',(19.3691979735541,-16.4706336043628,
9.19867986612851));
#146912=CARTESIAN_POINT('Ctrl Pts',(19.4503780599826,-16.4928387610342,
9.20285098010647));
#146913=CARTESIAN_POINT('Ctrl Pts',(19.5302987751908,-16.5189960417974,
9.20702209408442));
#146914=CARTESIAN_POINT('Ctrl Pts',(19.6101926722311,-16.5451445452324,
9.21119180840479));
#146915=CARTESIAN_POINT('Ctrl Pts',(19.6888276004822,-16.5752423959817,
9.21536152272516));
#146916=CARTESIAN_POINT('Ctrl Pts',(19.7657923610116,-16.609137536312,9.21953123704553));
#146917=CARTESIAN_POINT('Ctrl Pts',(19.8427543828047,-16.6430314705078,
9.22370080298958));
#146918=CARTESIAN_POINT('Ctrl Pts',(19.9180459343719,-16.6807222394304,
9.22787036893362));
#146919=CARTESIAN_POINT('Ctrl Pts',(19.9912767740527,-16.7220100642766,
9.23203993487766));
#146920=CARTESIAN_POINT('Ctrl Pts',(20.0670823197167,-16.7647495181104,
9.23635609761658));
#146921=CARTESIAN_POINT('Ctrl Pts',(20.1406790886265,-16.8113434200911,
9.2406722603555));
#146922=CARTESIAN_POINT('Ctrl Pts',(20.2116647704045,-16.8615199531434,
9.24498842309442));
#146923=CARTESIAN_POINT('Ctrl Pts',(20.2803381010649,-16.9100619909092,
9.2491639872861));
#146924=CARTESIAN_POINT('Ctrl Pts',(20.3465675028829,-16.9619565080489,
9.25333955147778));
#146925=CARTESIAN_POINT('Ctrl Pts',(20.4100221667426,-17.0169161008919,
9.25751511566946));
#146926=CARTESIAN_POINT('Ctrl Pts',(20.4766817748247,-17.0746515721154,
9.26190157768201));
#146927=CARTESIAN_POINT('Ctrl Pts',(20.5402785534046,-17.135769485738,9.26628803969454));
#146928=CARTESIAN_POINT('Ctrl Pts',(20.6004740985359,-17.1998942841557,
9.27067450170708));
#146929=CARTESIAN_POINT('Ctrl Pts',(20.6606696436673,-17.2640190825733,
9.27506096371962));
#146930=CARTESIAN_POINT('Ctrl Pts',(20.7174636386703,-17.3311502736972,
9.27944742573216));
#146931=CARTESIAN_POINT('Ctrl Pts',(20.7705691100608,-17.4008758076974,
9.2838338877447));
#146932=CARTESIAN_POINT('Ctrl Pts',(20.8212311199914,-17.4673931665203,
9.28801852213775));
#146933=CARTESIAN_POINT('Ctrl Pts',(20.8687251499199,-17.5365189656785,
9.2922031565308));
#146934=CARTESIAN_POINT('Ctrl Pts',(20.9127716012343,-17.6079187860643,
9.29638779092385));
#146935=CARTESIAN_POINT('Ctrl Pts',(20.9567553578772,-17.6792169776434,
9.3005664690078));
#146936=CARTESIAN_POINT('Ctrl Pts',(20.9973010436862,-17.752782372994,9.30474514709174));
#146937=CARTESIAN_POINT('Ctrl Pts',(21.0341702903065,-17.8282488551324,
9.30892382517569));
#146938=CARTESIAN_POINT('Ctrl Pts',(21.0717003916751,-17.9050680197264,
9.31317740306112));
#146939=CARTESIAN_POINT('Ctrl Pts',(21.1054206649962,-17.9838567118702,
9.31743098094655));
#146940=CARTESIAN_POINT('Ctrl Pts',(21.1351268232139,-18.0641993586155,
9.32168455883199));
#146941=CARTESIAN_POINT('Ctrl Pts',(21.1642570695877,-18.1429844063779,
9.32585567280994));
#146942=CARTESIAN_POINT('Ctrl Pts',(21.1895272879509,-18.2232632421891,
9.33002678678789));
#146943=CARTESIAN_POINT('Ctrl Pts',(21.2107927216345,-18.3046223559169,
9.33419790076584));
#146944=CARTESIAN_POINT('Ctrl Pts',(21.2320510194963,-18.3859541688083,
9.33836761508622));
#146945=CARTESIAN_POINT('Ctrl Pts',(21.2493070853372,-18.46836509498,9.34253732940659));
#146946=CARTESIAN_POINT('Ctrl Pts',(21.2624662014641,-18.5514270752366,
9.34670704372697));
#146947=CARTESIAN_POINT('Ctrl Pts',(21.2756248493332,-18.6344860997914,
9.35087660967101));
#146948=CARTESIAN_POINT('Ctrl Pts',(21.284686766209,-18.7181956778688,9.35504617561505));
#146949=CARTESIAN_POINT('Ctrl Pts',(21.2896087040397,-18.8021195415125,
9.3592157415591));
#146950=CARTESIAN_POINT('Ctrl Pts',(21.2947036911327,-18.8889940646706,
9.36353190429802));
#146951=CARTESIAN_POINT('Ctrl Pts',(21.2953621283496,-18.9760976958014,
9.36784806703694));
#146952=CARTESIAN_POINT('Ctrl Pts',(21.2915948078576,-19.062945026117,9.37216422977586));
#146953=CARTESIAN_POINT('Ctrl Pts',(21.2879502074343,-19.1469633137823,
9.37633979396754));
#146954=CARTESIAN_POINT('Ctrl Pts',(21.2801638500693,-19.2307412775515,
9.38051535815922));
#146955=CARTESIAN_POINT('Ctrl Pts',(21.2682983360669,-19.3138451931541,
9.3846909223509));
#146956=CARTESIAN_POINT('Ctrl Pts',(21.2558335231597,-19.4011464899729,
9.38907738436344));
#146957=CARTESIAN_POINT('Ctrl Pts',(21.2388667599596,-19.4877032838011,
9.39346384637598));
#146958=CARTESIAN_POINT('Ctrl Pts',(21.2175306593405,-19.5730277482655,
9.39785030838852));
#146959=CARTESIAN_POINT('Ctrl Pts',(21.1961945587214,-19.65835221273,9.40223677040106));
#146960=CARTESIAN_POINT('Ctrl Pts',(21.1704893630394,-19.7424438151945,
9.4066232324136));
#146961=CARTESIAN_POINT('Ctrl Pts',(21.1406062076889,-19.8248382216158,
9.41100969442614));
#146962=CARTESIAN_POINT('Ctrl Pts',(21.1121004746695,-19.9034347728897,
9.41519396859539));
#146963=CARTESIAN_POINT('Ctrl Pts',(21.079687362158,-19.9807796693134,9.41937824276465));
#146964=CARTESIAN_POINT('Ctrl Pts',(21.0434966865728,-20.0564569048673,
9.4235625169339));
#146965=CARTESIAN_POINT('Ctrl Pts',(21.0073550560038,-20.13203158386,9.42774112064272));
#146966=CARTESIAN_POINT('Ctrl Pts',(20.9674462242502,-20.2059426782205,
9.43191972435153));
#146967=CARTESIAN_POINT('Ctrl Pts',(20.9239489993266,-20.2777916051735,
9.43609832806035));
#146968=CARTESIAN_POINT('Ctrl Pts',(20.8805019784913,-20.34955760477,9.44027210886403));
#146969=CARTESIAN_POINT('Ctrl Pts',(20.8334750334865,-20.419265776318,9.4444458896677));
#146970=CARTESIAN_POINT('Ctrl Pts',(20.7830933893995,-20.4865410654391,
9.44861967047138));
#146971=CARTESIAN_POINT('Ctrl Pts',(20.7327462827068,-20.5537702363118,
9.45279059008393));
#146972=CARTESIAN_POINT('Ctrl Pts',(20.679049319678,-20.6185694703057,9.45696150969649));
#146973=CARTESIAN_POINT('Ctrl Pts',(20.622270999894,-20.6805926735235,9.46113242930904));
#146974=CARTESIAN_POINT('Ctrl Pts',(20.5655043373564,-20.7426031426597,
9.46530249258352));
#146975=CARTESIAN_POINT('Ctrl Pts',(20.5056578783584,-20.801838367992,9.46947255585799));
#146976=CARTESIAN_POINT('Ctrl Pts',(20.4430396423786,-20.8579862278564,
9.47364261913246));
#146977=CARTESIAN_POINT('Ctrl Pts',(20.3947976124209,-20.9012433828251,
9.47685529854229));
#146978=CARTESIAN_POINT('Ctrl Pts',(20.3449112722043,-20.9426687088704,
9.48006797795213));
#146979=CARTESIAN_POINT('Ctrl Pts',(20.2935357468249,-20.9821350335323,
9.48328065736197));
#146980=CARTESIAN_POINT('Origin',(18.734,-18.952,-1.76670989022851));
#146981=CARTESIAN_POINT('',(20.2935357468249,-20.9821350335323,10.3499274775013));
#146982=CARTESIAN_POINT('',(20.2935357468249,-20.9821350335323,10.2832382198804));
#146983=CARTESIAN_POINT('',(20.2935357468249,-20.9821350335323,-1.76670989022851));
#146984=CARTESIAN_POINT('',(16.1740007840082,-18.9540035272626,9.83329010977151));
#146985=CARTESIAN_POINT('Ctrl Pts',(16.1740007840082,-18.9540035272626,
9.83329010977151));
#146986=CARTESIAN_POINT('Ctrl Pts',(16.1739350379054,-18.8699966984849,
9.83745593779553));
#146987=CARTESIAN_POINT('Ctrl Pts',(16.1780086491546,-18.7859395799201,
9.84162176581955));
#146988=CARTESIAN_POINT('Ctrl Pts',(16.186209790272,-18.7022700514274,9.84578759384357));
#146989=CARTESIAN_POINT('Ctrl Pts',(16.1944094741073,-18.6186153903909,
9.84995268163077));
#146990=CARTESIAN_POINT('Ctrl Pts',(16.2067351859308,-18.5353486407625,
9.85411776941798));
#146991=CARTESIAN_POINT('Ctrl Pts',(16.2231231591269,-18.4529033260309,
9.85828285720518));
#146992=CARTESIAN_POINT('Ctrl Pts',(16.2395131466374,-18.3704478776005,
9.86244845694076));
#146993=CARTESIAN_POINT('Ctrl Pts',(16.2599662961797,-18.2888145159801,
9.86661405667633));
#146994=CARTESIAN_POINT('Ctrl Pts',(16.284367851052,-18.2084259721855,9.87077965641191));
#146995=CARTESIAN_POINT('Ctrl Pts',(16.308796991805,-18.127946549396,9.87494996534484));
#146996=CARTESIAN_POINT('Ctrl Pts',(16.3371833166001,-18.0487151959129,
9.87912027427777));
#146997=CARTESIAN_POINT('Ctrl Pts',(16.3693624790262,-17.971138442795,9.8832905832107));
#146998=CARTESIAN_POINT('Ctrl Pts',(16.4015603628991,-17.8935165564619,
9.88746331837885));
#146999=CARTESIAN_POINT('Ctrl Pts',(16.4375552801455,-17.8175516031283,
9.89163605354699));
#147000=CARTESIAN_POINT('Ctrl Pts',(16.4771361744291,-17.7436268486807,
9.89580878871514));
#147001=CARTESIAN_POINT('Ctrl Pts',(16.5167895617088,-17.6695666999467,
9.89998916630976));
#147002=CARTESIAN_POINT('Ctrl Pts',(16.5600418069661,-17.5975546086437,
9.90416954390437));
#147003=CARTESIAN_POINT('Ctrl Pts',(16.606637749578,-17.5279459787355,9.90834992149899));
#147004=CARTESIAN_POINT('Ctrl Pts',(16.6436006876738,-17.4727278774588,
9.91166606942058));
#147005=CARTESIAN_POINT('Ctrl Pts',(16.6826668124626,-17.4190216712155,
9.91498221734216));
#147006=CARTESIAN_POINT('Ctrl Pts',(16.7236914224215,-17.3669891410737,
9.91829836526375));
#147007=CARTESIAN_POINT('Ctrl Pts',(16.7754602209958,-17.3013294900759,
9.9224829996568));
#147008=CARTESIAN_POINT('Ctrl Pts',(16.8305455538228,-17.2380865845811,
9.92666763404985));
#147009=CARTESIAN_POINT('Ctrl Pts',(16.8886933634202,-17.1776146368405,
9.93085226844289));
#147010=CARTESIAN_POINT('Ctrl Pts',(16.9467584068079,-17.1172287634326,
9.93503094652683));
#147011=CARTESIAN_POINT('Ctrl Pts',(17.0078769523775,-17.0596063422905,
9.93920962461078));
#147012=CARTESIAN_POINT('Ctrl Pts',(17.0717539579497,-17.0050695709173,
9.94338830269472));
#147013=CARTESIAN_POINT('Ctrl Pts',(17.1367759129393,-16.949555267112,9.94764188058016));
#147014=CARTESIAN_POINT('Ctrl Pts',(17.2046558928939,-16.897238700291,9.95189545846559));
#147015=CARTESIAN_POINT('Ctrl Pts',(17.2750424589416,-16.8484214078412,
9.95614903635103));
#147016=CARTESIAN_POINT('Ctrl Pts',(17.3440644440583,-16.8005505338647,
9.96032015032898));
#147017=CARTESIAN_POINT('Ctrl Pts',(17.415496297028,-16.7560447387742,9.96449126430694));
#147018=CARTESIAN_POINT('Ctrl Pts',(17.4889737195062,-16.7151473984905,
9.96866237828489));
#147019=CARTESIAN_POINT('Ctrl Pts',(17.5624264859257,-16.6742637817044,
9.97283209260527));
#147020=CARTESIAN_POINT('Ctrl Pts',(17.6379230570027,-16.6369864384995,
9.97700180692564));
#147021=CARTESIAN_POINT('Ctrl Pts',(17.7150725574696,-16.6035139202332,
9.98117152124602));
#147022=CARTESIAN_POINT('Ctrl Pts',(17.792219312626,-16.5700425930628,9.98534108719005));
#147023=CARTESIAN_POINT('Ctrl Pts',(17.8710184578634,-16.5403760039566,
9.98951065313409));
#147024=CARTESIAN_POINT('Ctrl Pts',(17.9510583236138,-16.5146649119628,
9.99368021907812));
#147025=CARTESIAN_POINT('Ctrl Pts',(18.0339122923043,-16.4880498496924,
9.99799638181705));
#147026=CARTESIAN_POINT('Ctrl Pts',(18.1180953501443,-16.4656737716517,
10.002312544556));
#147027=CARTESIAN_POINT('Ctrl Pts',(18.2031347548808,-16.4476473707713,
10.0066287072949));
#147028=CARTESIAN_POINT('Ctrl Pts',(18.2854040099525,-16.4302081780036,
10.0108042714866));
#147029=CARTESIAN_POINT('Ctrl Pts',(18.3684742051319,-16.4168396609885,
10.0149798356782));
#147030=CARTESIAN_POINT('Ctrl Pts',(18.4519097174443,-16.4075894449819,
10.0191553998699));
#147031=CARTESIAN_POINT('Ctrl Pts',(18.5395593591347,-16.3978720225551,
10.0235418618825));
#147032=CARTESIAN_POINT('Ctrl Pts',(18.6276116092808,-16.3926998996316,
10.027928323895));
#147033=CARTESIAN_POINT('Ctrl Pts',(18.7155609817196,-16.3920664066025,
10.0323147859076));
#147034=CARTESIAN_POINT('Ctrl Pts',(18.8035103541583,-16.3914329135735,
10.0367012479201));
#147035=CARTESIAN_POINT('Ctrl Pts',(18.8913562726231,-16.395337948682,10.0410877099327));
#147036=CARTESIAN_POINT('Ctrl Pts',(18.9786013944251,-16.403712308658,10.0454741719452));
#147037=CARTESIAN_POINT('Ctrl Pts',(19.0618322388445,-16.4117013519176,
10.0496588063382));
#147038=CARTESIAN_POINT('Ctrl Pts',(19.1448261598422,-16.4237872141345,
10.0538434407313));
#147039=CARTESIAN_POINT('Ctrl Pts',(19.2271478044735,-16.4399480015448,
10.0580280751243));
#147040=CARTESIAN_POINT('Ctrl Pts',(19.3093522744331,-16.4560857860745,
10.0622067532083));
#147041=CARTESIAN_POINT('Ctrl Pts',(19.3908859211795,-16.4762868870104,
10.0663854312922));
#147042=CARTESIAN_POINT('Ctrl Pts',(19.4713181268663,-16.5004776199687,
10.0705641093762));
#147043=CARTESIAN_POINT('Ctrl Pts',(19.5531920220344,-16.5251019544297,
10.0748176872616));
#147044=CARTESIAN_POINT('Ctrl Pts',(19.6339241211585,-16.5538603099738,
10.079071265147));
#147045=CARTESIAN_POINT('Ctrl Pts',(19.7130706518195,-16.5866203985944,
10.0833248430325));
#147046=CARTESIAN_POINT('Ctrl Pts',(19.7906827725418,-16.6187453689711,
10.0874959570104));
#147047=CARTESIAN_POINT('Ctrl Pts',(19.8667698102185,-16.6547181102194,
10.0916670709884));
#147048=CARTESIAN_POINT('Ctrl Pts',(19.9409299364305,-16.6943640398532,
10.0958381849663));
#147049=CARTESIAN_POINT('Ctrl Pts',(20.0150651774959,-16.7339966659124,
10.1000078992867));
#147050=CARTESIAN_POINT('Ctrl Pts',(20.0872743858819,-16.7772998157407,
10.1041776136071));
#147051=CARTESIAN_POINT('Ctrl Pts',(20.1571790379496,-16.8240522971791,
10.1083473279274));
#147052=CARTESIAN_POINT('Ctrl Pts',(20.22708120251,-16.8708031149636,10.1125168938715));
#147053=CARTESIAN_POINT('Ctrl Pts',(20.2946785918819,-16.9210027638615,
10.1166864598155));
#147054=CARTESIAN_POINT('Ctrl Pts',(20.3596216126349,-16.9743866979275,
10.1208560257596));
#147055=CARTESIAN_POINT('Ctrl Pts',(20.4268479498818,-17.029647545259,10.1251721884985));
#147056=CARTESIAN_POINT('Ctrl Pts',(20.4912293829736,-17.0883204279971,
10.1294883512374));
#147057=CARTESIAN_POINT('Ctrl Pts',(20.5524169502582,-17.1500677607041,
10.1338045139763));
#147058=CARTESIAN_POINT('Ctrl Pts',(20.6116113389742,-17.2098036805429,
10.137980078168));
#147059=CARTESIAN_POINT('Ctrl Pts',(20.66781646727,-17.2724164438391,10.1421556423597));
#147060=CARTESIAN_POINT('Ctrl Pts',(20.7207564953883,-17.3375655392576,
10.1463312065514));
#147061=CARTESIAN_POINT('Ctrl Pts',(20.7763703984738,-17.4060051606085,
10.1507176685639));
#147062=CARTESIAN_POINT('Ctrl Pts',(20.8283803483073,-17.4772435963692,
10.1551041305764));
#147063=CARTESIAN_POINT('Ctrl Pts',(20.8765183429015,-17.5508522025388,
10.159490592589));
#147064=CARTESIAN_POINT('Ctrl Pts',(20.9246563374958,-17.6244608087083,
10.1638770546015));
#147065=CARTESIAN_POINT('Ctrl Pts',(20.9689221504901,-17.7004390456585,
10.1682635166141));
#147066=CARTESIAN_POINT('Ctrl Pts',(21.0091047687182,-17.7783312684767,
10.1726499786266));
#147067=CARTESIAN_POINT('Ctrl Pts',(21.0474385251168,-17.8526395546591,
10.1768346130197));
#147068=CARTESIAN_POINT('Ctrl Pts',(21.0821992629535,-17.9289661561369,
10.1810192474127));
#147069=CARTESIAN_POINT('Ctrl Pts',(21.1131697431269,-18.0069331593007,
10.1852038818058));
#147070=CARTESIAN_POINT('Ctrl Pts',(21.1440961406553,-18.0847891860861,
10.1893825598897));
#147071=CARTESIAN_POINT('Ctrl Pts',(21.1712428282378,-18.1642805528131,
10.1935612379737));
#147072=CARTESIAN_POINT('Ctrl Pts',(21.1944386775071,-18.2450052940602,
10.1977399160576));
#147073=CARTESIAN_POINT('Ctrl Pts',(21.2180502957041,-18.327176968278,10.2019934939431));
#147074=CARTESIAN_POINT('Ctrl Pts',(21.2375678238505,-18.4106262399203,
10.2062470718285));
#147075=CARTESIAN_POINT('Ctrl Pts',(21.252862289631,-18.4949083616223,10.2105006497139));
#147076=CARTESIAN_POINT('Ctrl Pts',(21.2678602423477,-18.5775565099321,
10.2146717636919));
#147077=CARTESIAN_POINT('Ctrl Pts',(21.2787973301571,-18.6610050301441,
10.2188428776698));
#147078=CARTESIAN_POINT('Ctrl Pts',(21.2856028472,-18.7448215499602,10.2230139916478));
#147079=CARTESIAN_POINT('Ctrl Pts',(21.2924060805859,-18.8286099443337,
10.2271837059682));
#147080=CARTESIAN_POINT('Ctrl Pts',(21.2950804593957,-18.9127656349242,
10.2313534202885));
#147081=CARTESIAN_POINT('Ctrl Pts',(21.2936070835643,-18.9968506161339,
10.2355231346089));
#147082=CARTESIAN_POINT('Ctrl Pts',(21.2921337601619,-19.0809326052393,
10.239692700553));
#147083=CARTESIAN_POINT('Ctrl Pts',(21.2865129844866,-19.1649434300193,
10.243862266497));
#147084=CARTESIAN_POINT('Ctrl Pts',(21.2767779695195,-19.2484459440205,
10.2480318324411));
#147085=CARTESIAN_POINT('Ctrl Pts',(21.2667006834357,-19.3348843034021,
10.25234799518));
#147086=CARTESIAN_POINT('Ctrl Pts',(21.2522145228801,-19.4207774186565,
10.2566641579189));
#147087=CARTESIAN_POINT('Ctrl Pts',(21.2334144574579,-19.5056491396638,
10.2609803206578));
#147088=CARTESIAN_POINT('Ctrl Pts',(21.2152268021894,-19.5877561732863,
10.2651558848495));
#147089=CARTESIAN_POINT('Ctrl Pts',(21.1930021468738,-19.6689068927559,
10.2693314490412));
#147090=CARTESIAN_POINT('Ctrl Pts',(21.166877500828,-19.748685048162,10.2735070132329));
#147091=CARTESIAN_POINT('Ctrl Pts',(21.1394333610159,-19.8324926085429,
10.2778934752454));
#147092=CARTESIAN_POINT('Ctrl Pts',(21.1076851096662,-19.9147847597333,
10.2822799372579));
#147093=CARTESIAN_POINT('Ctrl Pts',(21.0718481041567,-19.995104137606,10.2866663992705));
#147094=CARTESIAN_POINT('Ctrl Pts',(21.0360110986473,-20.0754235154787,
10.291052861283));
#147095=CARTESIAN_POINT('Ctrl Pts',(20.9960856701951,-20.15376963761,10.2954393232955));
#147096=CARTESIAN_POINT('Ctrl Pts',(20.9523407266399,-20.2297184433712,
10.2998257853081));
#147097=CARTESIAN_POINT('Ctrl Pts',(20.9106208944249,-20.3021513047666,
10.3040091821606));
#147098=CARTESIAN_POINT('Ctrl Pts',(20.8652721209666,-20.3726734304945,
10.308192579013));
#147099=CARTESIAN_POINT('Ctrl Pts',(20.8164943998492,-20.4408979396173,
10.3123759758655));
#147100=CARTESIAN_POINT('Ctrl Pts',(20.7677772522441,-20.509037725673,10.316554177661));
#147101=CARTESIAN_POINT('Ctrl Pts',(20.7156398718315,-20.5748851865346,
10.3207323794565));
#147102=CARTESIAN_POINT('Ctrl Pts',(20.6603275198092,-20.6380789680278,
10.324910581252));
#147103=CARTESIAN_POINT('Ctrl Pts',(20.6050732438228,-20.7012063982598,
10.3290843960816));
#147104=CARTESIAN_POINT('Ctrl Pts',(20.5466509193235,-20.7616853395333,
10.3332582109113));
#147105=CARTESIAN_POINT('Ctrl Pts',(20.4853475074052,-20.8191855580808,
10.337432025741));
#147106=CARTESIAN_POINT('Ctrl Pts',(20.4241713526063,-20.8765664143948,
10.3415971763278));
#147107=CARTESIAN_POINT('Ctrl Pts',(20.3601263754954,-20.9309805713415,
10.3457623269146));
#147108=CARTESIAN_POINT('Ctrl Pts',(20.2935357468249,-20.9821350335323,
10.3499274775013));
#147109=CARTESIAN_POINT('Ctrl Pts',(20.2954164701606,-20.9846205560609,
9.5499633223245));
#147110=CARTESIAN_POINT('Ctrl Pts',(19.6881794406823,-21.4438296808101,
9.58795779884996));
#147111=CARTESIAN_POINT('Ctrl Pts',(17.9381456550696,-21.8241543919292,
9.66834421093588));
#147112=CARTESIAN_POINT('Ctrl Pts',(16.3483940953146,-20.372000527443,9.7627861705977));
#147113=CARTESIAN_POINT('Ctrl Pts',(16.174290432163,-19.2372014285682,9.81923365373404));
#147114=CARTESIAN_POINT('Ctrl Pts',(16.1763511785197,-18.9540199907297,
9.8332892013099));
#147115=CARTESIAN_POINT('',(16.1740010233873,-18.9497109517325,9.7667098901893));
#147116=CARTESIAN_POINT('Ctrl Pts',(20.2935357468249,-20.9821350335323,
9.48328065736197));
#147117=CARTESIAN_POINT('Ctrl Pts',(20.2268468056927,-21.033365018679,9.48745093467704));
#147118=CARTESIAN_POINT('Ctrl Pts',(20.1576478466326,-21.0812925043171,
9.49162121199211));
#147119=CARTESIAN_POINT('Ctrl Pts',(20.0863050736588,-21.1256768360905,
9.49579148930719));
#147120=CARTESIAN_POINT('Ctrl Pts',(20.0148829142921,-21.1701105563565,
9.49996640708211));
#147121=CARTESIAN_POINT('Ctrl Pts',(19.9413125717026,-21.2109930116134,
9.50414132485704));
#147122=CARTESIAN_POINT('Ctrl Pts',(19.8659864837341,-21.2481286115205,
9.50831624263196));
#147123=CARTESIAN_POINT('Ctrl Pts',(19.7906119648809,-21.2852880877501,
9.51249384466897));
#147124=CARTESIAN_POINT('Ctrl Pts',(19.7134798757101,-21.318695731469,9.51667144670598));
#147125=CARTESIAN_POINT('Ctrl Pts',(19.6350021373819,-21.3482043210948,
9.520849048743));
#147126=CARTESIAN_POINT('Ctrl Pts',(19.5563968680676,-21.3777608639314,
9.52503343963145));
#147127=CARTESIAN_POINT('Ctrl Pts',(19.4764420228001,-21.4034055677312,
9.52921783051991));
#147128=CARTESIAN_POINT('Ctrl Pts',(19.3955636713297,-21.4250413479715,
9.53340222140836));
#147129=CARTESIAN_POINT('Ctrl Pts',(19.3647456632446,-21.4332854780539,
9.53499664797477));
#147130=CARTESIAN_POINT('Ctrl Pts',(19.333793658731,-21.4409480748349,9.53659107454117));
#147131=CARTESIAN_POINT('Ctrl Pts',(19.3027314805895,-21.4480257416514,
9.53818550110758));
#147132=CARTESIAN_POINT('Ctrl Pts',(19.2212075887321,-21.4666013528504,
9.54237013550063));
#147133=CARTESIAN_POINT('Ctrl Pts',(19.1386209669249,-21.4812132961356,
9.54655476989368));
#147134=CARTESIAN_POINT('Ctrl Pts',(19.0553917867601,-21.4917455225678,
9.55073940428673));
#147135=CARTESIAN_POINT('Ctrl Pts',(18.9722810730315,-21.5022627576793,
9.55491808237067));
#147136=CARTESIAN_POINT('Ctrl Pts',(18.8885300701227,-21.508711753151,9.55909676045462));
#147137=CARTESIAN_POINT('Ctrl Pts',(18.8045707324915,-21.5110271142986,
9.56327543853857));
#147138=CARTESIAN_POINT('Ctrl Pts',(18.7191064840738,-21.5133839766308,
9.567529016424));
#147139=CARTESIAN_POINT('Ctrl Pts',(18.6334268287618,-21.5114574491382,
9.57178259430944));
#147140=CARTESIAN_POINT('Ctrl Pts',(18.547994628297,-21.5052336363321,9.57603617219488));
#147141=CARTESIAN_POINT('Ctrl Pts',(18.4642186977454,-21.499130484282,9.58020728617283));
#147142=CARTESIAN_POINT('Ctrl Pts',(18.3806811928202,-21.4888952174951,
9.58437840015078));
#147143=CARTESIAN_POINT('Ctrl Pts',(18.2978184502098,-21.4745672747466,
9.58854951412873));
#147144=CARTESIAN_POINT('Ctrl Pts',(18.214983512993,-21.4602441398778,9.5927192284491));
#147145=CARTESIAN_POINT('Ctrl Pts',(18.1328233413403,-21.4418311348331,
9.59688894276948));
#147146=CARTESIAN_POINT('Ctrl Pts',(18.051766797798,-21.4194192707793,9.60105865708985));
#147147=CARTESIAN_POINT('Ctrl Pts',(17.9707131385955,-21.3970082042359,
9.6052282230339));
#147148=CARTESIAN_POINT('Ctrl Pts',(17.8907634725899,-21.3705986850245,
9.60939778897794));
#147149=CARTESIAN_POINT('Ctrl Pts',(17.812332824503,-21.3403319739122,9.61356735492198));
#147150=CARTESIAN_POINT('Ctrl Pts',(17.731144651584,-21.3090011225752,9.6178835176609));
#147151=CARTESIAN_POINT('Ctrl Pts',(17.6515847934176,-21.2735369848542,
9.62219968039982));
#147152=CARTESIAN_POINT('Ctrl Pts',(17.5740906315701,-21.2341503581115,
9.62651584313874));
#147153=CARTESIAN_POINT('Ctrl Pts',(17.4991208338937,-21.1960467465922,
9.63069140733042));
#147154=CARTESIAN_POINT('Ctrl Pts',(17.4260846045832,-21.1542725466306,
9.6348669715221));
#147155=CARTESIAN_POINT('Ctrl Pts',(17.3553508285745,-21.1090643157143,
9.63904253571378));
#147156=CARTESIAN_POINT('Ctrl Pts',(17.2810444576934,-21.0615727245268,
9.64342899772632));
#147157=CARTESIAN_POINT('Ctrl Pts',(17.2092797216844,-21.0102914191919,
9.64781545973885));
#147158=CARTESIAN_POINT('Ctrl Pts',(17.1404457653639,-20.9555430869521,
9.65220192175139));
#147159=CARTESIAN_POINT('Ctrl Pts',(17.0716118090435,-20.9007947547123,
9.65658838376393));
#147160=CARTESIAN_POINT('Ctrl Pts',(17.0057090169082,-20.8425798367027,
9.66097484577646));
#147161=CARTESIAN_POINT('Ctrl Pts',(16.9430809195061,-20.7812645645512,
9.665361307789));
#147162=CARTESIAN_POINT('Ctrl Pts',(16.8827886985014,-20.7222362035939,
9.66958416538901));
#147163=CARTESIAN_POINT('Ctrl Pts',(16.8252872091303,-20.6600954577447,
9.67380702298902));
#147164=CARTESIAN_POINT('Ctrl Pts',(16.7709203169311,-20.5951427685755,
9.67802988058904));
#147165=CARTESIAN_POINT('Ctrl Pts',(16.7179063153622,-20.5318063918538,
9.68214765466763));
#147166=CARTESIAN_POINT('Ctrl Pts',(16.6678730797622,-20.4657967543979,
9.68626542874624));
#147167=CARTESIAN_POINT('Ctrl Pts',(16.6211045875939,-20.3974317611818,
9.69038320282483));
#147168=CARTESIAN_POINT('Ctrl Pts',(16.57438033231,-20.329131432319,9.69449708202704));
#147169=CARTESIAN_POINT('Ctrl Pts',(16.530914960773,-20.2584805564846,9.69861096122925));
#147170=CARTESIAN_POINT('Ctrl Pts',(16.4909521572678,-20.1858299620347,
9.70272484043146));
#147171=CARTESIAN_POINT('Ctrl Pts',(16.4510143565681,-20.11322482157,9.70683614577718));
#147172=CARTESIAN_POINT('Ctrl Pts',(16.4145750025456,-20.0386228602468,
9.71094745112289));
#147173=CARTESIAN_POINT('Ctrl Pts',(16.3818335581792,-19.9624024099199,
9.71505875646861));
#147174=CARTESIAN_POINT('Ctrl Pts',(16.3475554603697,-19.8826047069797,
9.719363017612));
#147175=CARTESIAN_POINT('Ctrl Pts',(16.3173311789842,-19.8010333411257,
9.72366727875539));
#147176=CARTESIAN_POINT('Ctrl Pts',(16.2913340385439,-19.718148158481,9.72797153989879));
#147177=CARTESIAN_POINT('Ctrl Pts',(16.2665001036005,-19.6389715567965,
9.73208321292913));
#147178=CARTESIAN_POINT('Ctrl Pts',(16.245523244682,-19.5585966865051,9.73619488595948));
#147179=CARTESIAN_POINT('Ctrl Pts',(16.2285034541843,-19.4774398718271,
9.74030655898983));
#147180=CARTESIAN_POINT('Ctrl Pts',(16.2114791195104,-19.3962613887933,
9.74441932981084));
#147181=CARTESIAN_POINT('Ctrl Pts',(16.1984140354436,-19.3143010135803,
9.74853210063185));
#147182=CARTESIAN_POINT('Ctrl Pts',(16.1893567554131,-19.2319834955465,
9.75264487145287));
#147183=CARTESIAN_POINT('Ctrl Pts',(16.1802905487374,-19.1495848472745,
9.75676169572549));
#147184=CARTESIAN_POINT('Ctrl Pts',(16.1752400549859,-19.0668288268568,
9.76087851999812));
#147185=CARTESIAN_POINT('Ctrl Pts',(16.1742017924823,-18.9841424452887,
9.76499534427075));
#147186=CARTESIAN_POINT('Ctrl Pts',(16.1740576564023,-18.9726635650768,
9.76556685957694));
#147187=CARTESIAN_POINT('Ctrl Pts',(16.1739907628404,-18.9611860219109,
9.76613837488311));
#147188=CARTESIAN_POINT('Ctrl Pts',(16.1740010233873,-18.9497109517325,
9.7667098901893));
#147189=CARTESIAN_POINT('Ctrl Pts',(16.174001023388,-18.9497109509451,9.76670989022852));
#147190=CARTESIAN_POINT('Ctrl Pts',(16.1741079389015,-18.8301400729777,
9.7726651119283));
#147191=CARTESIAN_POINT('Ctrl Pts',(16.18259555166,-18.7109297707787,9.77862033362807));
#147192=CARTESIAN_POINT('Ctrl Pts',(16.1992930219765,-18.5930285031387,
9.78457555532785));
#147193=CARTESIAN_POINT('Ctrl Pts',(16.2067339930636,-18.5404876147875,
9.78722940837539));
#147194=CARTESIAN_POINT('Ctrl Pts',(16.2158047738385,-18.4882062515533,
9.78988326142292));
#147195=CARTESIAN_POINT('Ctrl Pts',(16.2264874578014,-18.4362666864388,
9.79253711447045));
#147196=CARTESIAN_POINT('Ctrl Pts',(16.2433320704913,-18.3543676186888,
9.7967217488635));
#147197=CARTESIAN_POINT('Ctrl Pts',(16.2642246666771,-18.2731422629635,
9.80090638325655));
#147198=CARTESIAN_POINT('Ctrl Pts',(16.2890969179466,-18.193021133782,9.80509101764959));
#147199=CARTESIAN_POINT('Ctrl Pts',(16.3139337666449,-18.1130140471109,
9.80926969573354));
#147200=CARTESIAN_POINT('Ctrl Pts',(16.3427388836329,-18.0341085006258,
9.81344837381748));
#147201=CARTESIAN_POINT('Ctrl Pts',(16.3753929533287,-17.9567247619916,
9.81762705190143));
#147202=CARTESIAN_POINT('Ctrl Pts',(16.4086323237558,-17.8779539754572,
9.82188062978686));
#147203=CARTESIAN_POINT('Ctrl Pts',(16.4458598919279,-17.8007605624573,
9.8261342076723));
#147204=CARTESIAN_POINT('Ctrl Pts',(16.4868966678982,-17.7255716022299,
9.83038778555773));
#147205=CARTESIAN_POINT('Ctrl Pts',(16.5271378658896,-17.6518403267158,
9.83455889953568));
#147206=CARTESIAN_POINT('Ctrl Pts',(16.5710416613175,-17.5800368994831,
9.83873001351364));
#147207=CARTESIAN_POINT('Ctrl Pts',(16.618391498167,-17.5105421730166,9.8429011274916));
#147208=CARTESIAN_POINT('Ctrl Pts',(16.6657254463214,-17.4410707661768,
9.84707084181197));
#147209=CARTESIAN_POINT('Ctrl Pts',(16.7165028805482,-17.3739069013823,
9.85124055613234));
#147210=CARTESIAN_POINT('Ctrl Pts',(16.7704633948898,-17.3094032751791,
9.85541027045272));
#147211=CARTESIAN_POINT('Ctrl Pts',(16.8244219890848,-17.2449019442917,
9.85957983639676));
#147212=CARTESIAN_POINT('Ctrl Pts',(16.8815631423607,-17.1830610160833,
9.86374940234081));
#147213=CARTESIAN_POINT('Ctrl Pts',(16.9415864376593,-17.1241997862083,
9.86791896828485));
#147214=CARTESIAN_POINT('Ctrl Pts',(17.0037200779738,-17.0632690681041,
9.87223513102377));
#147215=CARTESIAN_POINT('Ctrl Pts',(17.0689419268744,-17.0055318485509,
9.87655129376269));
#147216=CARTESIAN_POINT('Ctrl Pts',(17.1368790142893,-16.9512989836053,
9.88086745650161));
#147217=CARTESIAN_POINT('Ctrl Pts',(17.2026030582275,-16.8988327485311,
9.88504302069329));
#147218=CARTESIAN_POINT('Ctrl Pts',(17.2708677497022,-16.8496463025101,
9.88921858488496));
#147219=CARTESIAN_POINT('Ctrl Pts',(17.3413050297814,-16.8039774861683,
9.89339414907664));
#147220=CARTESIAN_POINT('Ctrl Pts',(17.4152999294287,-16.7560020464804,
9.89778061108918));
#147221=CARTESIAN_POINT('Ctrl Pts',(17.4916921547951,-16.7119092180967,
9.90216707310172));
#147222=CARTESIAN_POINT('Ctrl Pts',(17.5700268579948,-16.6719196231952,
9.90655353511426));
#147223=CARTESIAN_POINT('Ctrl Pts',(17.6483615611944,-16.6319300282936,
9.91093999712679));
#147224=CARTESIAN_POINT('Ctrl Pts',(17.7286381814853,-16.5960438342244,
9.91532645913933));
#147225=CARTESIAN_POINT('Ctrl Pts',(17.8103811197834,-16.5644221134993,
9.91971292115187));
#147226=CARTESIAN_POINT('Ctrl Pts',(17.8883629443183,-16.5342553550193,
9.92389755554492));
#147227=CARTESIAN_POINT('Ctrl Pts',(17.967969380348,-16.5078569775931,9.92808218993797));
#147228=CARTESIAN_POINT('Ctrl Pts',(18.0488014484187,-16.4854025571831,
9.93226682433102));
#147229=CARTESIAN_POINT('Ctrl Pts',(18.1295184620454,-16.4629800978612,
9.93644550241496));
#147230=CARTESIAN_POINT('Ctrl Pts',(18.2114572030593,-16.4444905669892,
9.9406241804989));
#147231=CARTESIAN_POINT('Ctrl Pts',(18.2941997096014,-16.4300611219609,
9.94480285858285));
#147232=CARTESIAN_POINT('Ctrl Pts',(18.3784253161073,-16.4153730395006,
9.94905643646828));
#147233=CARTESIAN_POINT('Ctrl Pts',(18.4634833368927,-16.404892202575,9.95331001435371));
#147234=CARTESIAN_POINT('Ctrl Pts',(18.5489177820416,-16.3986992788558,
9.95756359223915));
#147235=CARTESIAN_POINT('Ctrl Pts',(18.6326959137598,-16.3926264170474,
9.9617347062171));
#147236=CARTESIAN_POINT('Ctrl Pts',(18.7168355246874,-16.3906767277746,
9.96590582019505));
#147237=CARTESIAN_POINT('Ctrl Pts',(18.8008991604927,-16.3928742699263,
9.97007693417301));
#147238=CARTESIAN_POINT('Ctrl Pts',(18.8849345879332,-16.3950710746715,
9.97424664849338));
#147239=CARTESIAN_POINT('Ctrl Pts',(18.96889363139,-16.4014123350032,9.97841636281375));
#147240=CARTESIAN_POINT('Ctrl Pts',(19.0523387760777,-16.4118699986722,
9.98258607713412));
#147241=CARTESIAN_POINT('Ctrl Pts',(19.1357809514291,-16.4223272902127,
9.98675564307817));
#147242=CARTESIAN_POINT('Ctrl Pts',(19.2187088080138,-16.4369006358009,
9.99092520902221));
#147243=CARTESIAN_POINT('Ctrl Pts',(19.3006912586604,-16.4555102609148,
9.99509477496625));
#147244=CARTESIAN_POINT('Ctrl Pts',(19.3855561111354,-16.4747741774902,
9.99941093770517));
#147245=CARTESIAN_POINT('Ctrl Pts',(19.4694073254463,-16.498363368963,10.0037271004441));
#147246=CARTESIAN_POINT('Ctrl Pts',(19.5517816392175,-16.5261324870145,
10.008043263183));
#147247=CARTESIAN_POINT('Ctrl Pts',(19.6314726183819,-16.5529970289662,
10.0122188273747));
#147248=CARTESIAN_POINT('Ctrl Pts',(19.7097810183148,-16.5837731410383,
10.0163943915664));
#147249=CARTESIAN_POINT('Ctrl Pts',(19.7863076293696,-16.6182800825355,
10.0205699557581));
#147250=CARTESIAN_POINT('Ctrl Pts',(19.866699417624,-16.6545298876152,10.0249564177706));
#147251=CARTESIAN_POINT('Ctrl Pts',(19.945124171151,-16.6948970480992,10.0293428797831));
#147252=CARTESIAN_POINT('Ctrl Pts',(20.0211501810795,-16.739118527497,10.0337293417957));
#147253=CARTESIAN_POINT('Ctrl Pts',(20.097176191008,-16.7833400068949,10.0381158038082));
#147254=CARTESIAN_POINT('Ctrl Pts',(20.1708030131039,-16.8314154242948,
10.0425022658208));
#147255=CARTESIAN_POINT('Ctrl Pts',(20.2416377781113,-16.8830320616279,
10.0468887278333));
#147256=CARTESIAN_POINT('Ctrl Pts',(20.3092133305783,-16.9322737409631,
10.0510733622264));
#147257=CARTESIAN_POINT('Ctrl Pts',(20.3744996423274,-16.9849212146565,
10.0552579966194));
#147258=CARTESIAN_POINT('Ctrl Pts',(20.4371331217483,-17.0407340400657,
10.0594426310125));
#147259=CARTESIAN_POINT('Ctrl Pts',(20.4996774501638,-17.096467422826,10.0636213090964));
#147260=CARTESIAN_POINT('Ctrl Pts',(20.5595761060152,-17.1553569045525,
10.0677999871804));
#147261=CARTESIAN_POINT('Ctrl Pts',(20.6164959352303,-17.2171198733511,
10.0719786652643));
#147262=CARTESIAN_POINT('Ctrl Pts',(20.6744360114766,-17.2799898989772,
10.0762322431497));
#147263=CARTESIAN_POINT('Ctrl Pts',(20.7292890301008,-17.3458371554909,
10.0804858210352));
#147264=CARTESIAN_POINT('Ctrl Pts',(20.780740343664,-17.414321891416,10.0847393989206));
#147265=CARTESIAN_POINT('Ctrl Pts',(20.8311941731147,-17.4814789170983,
10.0889105128986));
#147266=CARTESIAN_POINT('Ctrl Pts',(20.8783767288093,-17.5511716846818,
10.0930816268765));
#147267=CARTESIAN_POINT('Ctrl Pts',(20.9220309952968,-17.6230453869223,
10.0972527408545));
#147268=CARTESIAN_POINT('Ctrl Pts',(20.9656706131735,-17.6948949712478,
10.1014224551748));
#147269=CARTESIAN_POINT('Ctrl Pts',(21.0057840545747,-17.7689236439344,
10.1055921694952));
#147270=CARTESIAN_POINT('Ctrl Pts',(21.0421580885473,-17.8447483401351,
10.1097618838156));
#147271=CARTESIAN_POINT('Ctrl Pts',(21.0785308281757,-17.9205703381677,
10.1139314497596));
#147272=CARTESIAN_POINT('Ctrl Pts',(21.1111642267361,-17.9981878174991,
10.1181010157037));
#147273=CARTESIAN_POINT('Ctrl Pts',(21.1398920226672,-18.0771951216034,
10.1222705816477));
#147274=CARTESIAN_POINT('Ctrl Pts',(21.1696298524636,-18.158980225054,10.1265867443866));
#147275=CARTESIAN_POINT('Ctrl Pts',(21.1951821474479,-18.242254208487,10.1309029071256));
#147276=CARTESIAN_POINT('Ctrl Pts',(21.2164203674168,-18.326548867269,10.1352190698645));
#147277=CARTESIAN_POINT('Ctrl Pts',(21.236966754604,-18.4080976364075,10.1393946340562));
#147278=CARTESIAN_POINT('Ctrl Pts',(21.2534757664241,-18.4906011339277,
10.1435701982478));
#147279=CARTESIAN_POINT('Ctrl Pts',(21.2658832925888,-18.5736258561825,
10.1477457624395));
#147280=CARTESIAN_POINT('Ctrl Pts',(21.278917493404,-18.6608439597858,10.1521322244521));
#147281=CARTESIAN_POINT('Ctrl Pts',(21.2874249313198,-18.748636744862,10.1565186864646));
#147282=CARTESIAN_POINT('Ctrl Pts',(21.291393102574,-18.8364988359062,10.1609051484772));
#147283=CARTESIAN_POINT('Ctrl Pts',(21.2953612738282,-18.9243609269505,
10.1652916104897));
#147284=CARTESIAN_POINT('Ctrl Pts',(21.294790258252,-19.012291744252,10.1696780725022));
#147285=CARTESIAN_POINT('Ctrl Pts',(21.2897303495757,-19.0997916785801,
10.1740645345148));
#147286=CARTESIAN_POINT('Ctrl Pts',(21.2849027735543,-19.1832739332733,
10.1782495861008));
#147287=CARTESIAN_POINT('Ctrl Pts',(21.2759715218877,-19.266674774493,10.1824346376867));
#147288=CARTESIAN_POINT('Ctrl Pts',(21.2629419677491,-19.3495582017232,
10.1866196892727));
#147289=CARTESIAN_POINT('Ctrl Pts',(21.2499348195042,-19.4322991008789,
10.1907975441565));
#147290=CARTESIAN_POINT('Ctrl Pts',(21.2328434536032,-19.5145239047262,
10.1949753990403));
#147291=CARTESIAN_POINT('Ctrl Pts',(21.2117251381579,-19.5957997668066,
10.1991532539241));
#147292=CARTESIAN_POINT('Ctrl Pts',(21.1906274886257,-19.6769960941389,
10.2033270204521));
#147293=CARTESIAN_POINT('Ctrl Pts',(21.1655108283406,-19.7572448807651,
10.2075007869801));
#147294=CARTESIAN_POINT('Ctrl Pts',(21.1364836587684,-19.8361223158311,
10.2116745535082));
#147295=CARTESIAN_POINT('Ctrl Pts',(21.1074761860977,-19.9149462272128,
10.2158454878528));
#147296=CARTESIAN_POINT('Ctrl Pts',(21.0745636328025,-19.9924002048068,
10.2200164221975));
#147297=CARTESIAN_POINT('Ctrl Pts',(21.0379042545248,-20.0680757975973,
10.2241873565421));
#147298=CARTESIAN_POINT('Ctrl Pts',(21.00125875479,-20.1437227410485,10.2283567118504));
#147299=CARTESIAN_POINT('Ctrl Pts',(20.9608694496218,-20.2175922243102,
10.2325260671587));
#147300=CARTESIAN_POINT('Ctrl Pts',(20.9169420720101,-20.2892972407989,
10.236695422467));
#147301=CARTESIAN_POINT('Ctrl Pts',(20.8729998723142,-20.3610264521712,
10.2408661846094));
#147302=CARTESIAN_POINT('Ctrl Pts',(20.8255174487911,-20.4305893408782,
10.2450369467519));
#147303=CARTESIAN_POINT('Ctrl Pts',(20.7747452964174,-20.4976256452162,
10.2492077088943));
#147304=CARTESIAN_POINT('Ctrl Pts',(20.7239654366853,-20.5646721258578,
10.2533791041704));
#147305=CARTESIAN_POINT('Ctrl Pts',(20.6698951413565,-20.6291908988708,
10.2575504994465));
#147306=CARTESIAN_POINT('Ctrl Pts',(20.6128256045793,-20.690854320401,10.2617218947226));
#147307=CARTESIAN_POINT('Ctrl Pts',(20.5556935666862,-20.7525852741537,
10.2658978584056));
#147308=CARTESIAN_POINT('Ctrl Pts',(20.49555604941,-20.8114543016472,10.2700738220885));
#147309=CARTESIAN_POINT('Ctrl Pts',(20.4327411706605,-20.8671706020882,
10.2742497857714));
#147310=CARTESIAN_POINT('Ctrl Pts',(20.3876731383385,-20.9071455901663,
10.2772459304744));
#147311=CARTESIAN_POINT('Ctrl Pts',(20.3412276536165,-20.9454984392925,
10.2802420751774));
#147312=CARTESIAN_POINT('Ctrl Pts',(20.2935357468249,-20.9821350335323,
10.2832382198805));
#147313=CARTESIAN_POINT('Origin',(18.734,-18.952,-1.76670989022851));
#147314=CARTESIAN_POINT('',(20.2922817658078,-20.9805345212666,11.1497835179515));
#147315=CARTESIAN_POINT('',(20.2948050232964,-20.9838171774959,11.0834063370138));
#147316=CARTESIAN_POINT('',(20.2935357468249,-20.9821350335323,-1.76670989022851));
#147317=CARTESIAN_POINT('',(16.1740004874608,-18.9504201902088,10.6332901097715));
#147318=CARTESIAN_POINT('Ctrl Pts',(16.1772048604514,-18.9504028912009,
10.6332910657491));
#147319=CARTESIAN_POINT('Ctrl Pts',(16.1753928930938,-18.6273578295265,
10.6493117789502));
#147320=CARTESIAN_POINT('Ctrl Pts',(16.3822354976306,-17.4517521542537,
10.7077244277117));
#147321=CARTESIAN_POINT('Ctrl Pts',(18.1490152356806,-15.9819691251248,
10.8085290120338));
#147322=CARTESIAN_POINT('Ctrl Pts',(20.9146847903814,-16.8524990075743,
10.9357048187152));
#147323=CARTESIAN_POINT('Ctrl Pts',(21.5989574361765,-19.3539801738065,
11.0494563206878));
#147324=CARTESIAN_POINT('Ctrl Pts',(20.7519189177889,-20.6211556360716,
11.1208158870999));
#147325=CARTESIAN_POINT('Ctrl Pts',(20.292281765808,-20.9805345212664,11.1497835179515));
#147326=CARTESIAN_POINT('Ctrl Pts',(20.2935357468249,-20.9821350335323,
10.3499274775013));
#147327=CARTESIAN_POINT('Ctrl Pts',(20.2268718913476,-21.0333457480517,
10.3540972083223));
#147328=CARTESIAN_POINT('Ctrl Pts',(20.1576571264186,-21.0812892905445,
10.3582669391434));
#147329=CARTESIAN_POINT('Ctrl Pts',(20.086248880528,-21.1257117943993,10.3624366699644));
#147330=CARTESIAN_POINT('Ctrl Pts',(20.0148436247903,-21.1701324381037,
10.3666062261818));
#147331=CARTESIAN_POINT('Ctrl Pts',(19.9412454617371,-21.2110320939803,
10.3707757823993));
#147332=CARTESIAN_POINT('Ctrl Pts',(19.8658394210623,-21.2482011072486,
10.3749453386168));
#147333=CARTESIAN_POINT('Ctrl Pts',(19.7873867082221,-21.2868718808152,
10.3792833597312));
#147334=CARTESIAN_POINT('Ctrl Pts',(19.7069774009645,-21.3215038936756,
10.3836213808456));
#147335=CARTESIAN_POINT('Ctrl Pts',(19.6250697922386,-21.351915545464,10.38795940196));
#147336=CARTESIAN_POINT('Ctrl Pts',(19.5462303075402,-21.3811880268991,
10.3921349279531));
#147337=CARTESIAN_POINT('Ctrl Pts',(19.4660032377296,-21.406550602145,10.3963104539462));
#147338=CARTESIAN_POINT('Ctrl Pts',(19.3848125515317,-21.4278923689791,
10.4004859799393));
#147339=CARTESIAN_POINT('Ctrl Pts',(19.3035638143394,-21.4492493950854,
10.4046644914157));
#147340=CARTESIAN_POINT('Ctrl Pts',(19.2213505391032,-21.4665797981134,
10.4088430028921));
#147341=CARTESIAN_POINT('Ctrl Pts',(19.138605750157,-21.4798240023664,10.4130215143685));
#147342=CARTESIAN_POINT('Ctrl Pts',(19.0557327305457,-21.4930887313334,
10.417206501338));
#147343=CARTESIAN_POINT('Ctrl Pts',(18.9723270098871,-21.5022545827837,
10.4213914883074));
#147344=CARTESIAN_POINT('Ctrl Pts',(18.8888248918782,-21.5073139245218,
10.4255764752769));
#147345=CARTESIAN_POINT('Ctrl Pts',(18.8793465458456,-21.5078882116517,
10.4260515141811));
#147346=CARTESIAN_POINT('Ctrl Pts',(18.8698669547576,-21.5084096433106,
10.4265265530853));
#147347=CARTESIAN_POINT('Ctrl Pts',(18.8603867536229,-21.5088782506229,
10.4270015919895));
#147348=CARTESIAN_POINT('Ctrl Pts',(18.7768753288336,-21.5130062288976,
10.4311862263825));
#147349=CARTESIAN_POINT('Ctrl Pts',(18.6930060412949,-21.5130461767751,
10.4353708607756));
#147350=CARTESIAN_POINT('Ctrl Pts',(18.6092128353627,-21.5089568169099,
10.4395554951686));
#147351=CARTESIAN_POINT('Ctrl Pts',(18.5255388986879,-21.5048732777423,
10.4437341732525));
#147352=CARTESIAN_POINT('Ctrl Pts',(18.4419412840721,-21.4966721277452,
10.4479128513365));
#147353=CARTESIAN_POINT('Ctrl Pts',(18.3588567381423,-21.48436402065,10.4520915294204));
#147354=CARTESIAN_POINT('Ctrl Pts',(18.274282961438,-21.4718352995808,10.4563451073058));
#147355=CARTESIAN_POINT('Ctrl Pts',(18.1902413094011,-21.4550509150076,
10.4605986851913));
#147356=CARTESIAN_POINT('Ctrl Pts',(18.1071900176379,-21.4340776067664,
10.4648522630767));
#147357=CARTESIAN_POINT('Ctrl Pts',(18.025748837227,-21.4135109070316,10.4690233770546));
#147358=CARTESIAN_POINT('Ctrl Pts',(17.9452604262043,-21.3889163729568,
10.4731944910326));
#147359=CARTESIAN_POINT('Ctrl Pts',(17.8661476315636,-21.3604086585543,
10.4773656050105));
#147360=CARTESIAN_POINT('Ctrl Pts',(17.7870613839853,-21.3319105101907,
10.4815353193309));
#147361=CARTESIAN_POINT('Ctrl Pts',(17.7093502684731,-21.2995019451713,
10.4857050336513));
#147362=CARTESIAN_POINT('Ctrl Pts',(17.6334208106706,-21.2633471067789,
10.4898747479716));
#147363=CARTESIAN_POINT('Ctrl Pts',(17.5574940547643,-21.2271935549308,
10.4940443139157));
#147364=CARTESIAN_POINT('Ctrl Pts',(17.4833492454977,-21.1872941933052,
10.4982138798597));
#147365=CARTESIAN_POINT('Ctrl Pts',(17.4113705501186,-21.143860246071,10.5023834458037));
#147366=CARTESIAN_POINT('Ctrl Pts',(17.3368611726046,-21.0988992148333,
10.5066996085427));
#147367=CARTESIAN_POINT('Ctrl Pts',(17.2646735157637,-21.0501506938751,
10.5110157712816));
#147368=CARTESIAN_POINT('Ctrl Pts',(17.195201681377,-20.9978982708344,10.5153319340205));
#147369=CARTESIAN_POINT('Ctrl Pts',(17.1279928846885,-20.9473479649783,
10.5195074982122));
#147370=CARTESIAN_POINT('Ctrl Pts',(17.0633260236122,-20.8935188682657,
10.5236830624039));
#147371=CARTESIAN_POINT('Ctrl Pts',(17.0015232692744,-20.8367080350798,
10.5278586265956));
#147372=CARTESIAN_POINT('Ctrl Pts',(16.9365990047368,-20.7770278217644,
10.5322450886081));
#147373=CARTESIAN_POINT('Ctrl Pts',(16.8748361916365,-20.714057157727,10.5366315506207));
#147374=CARTESIAN_POINT('Ctrl Pts',(16.8165619874416,-20.6481814372278,
10.5410180126332));
#147375=CARTESIAN_POINT('Ctrl Pts',(16.7582877832468,-20.5823057167286,
10.5454044746458));
#147376=CARTESIAN_POINT('Ctrl Pts',(16.7035024899566,-20.5135254410002,
10.5497909366583));
#147377=CARTESIAN_POINT('Ctrl Pts',(16.6524807786035,-20.4422609606901,
10.5541773986709));
#147378=CARTESIAN_POINT('Ctrl Pts',(16.6033728384837,-20.3736695367859,
10.5583993290636));
#147379=CARTESIAN_POINT('Ctrl Pts',(16.55756917535,-20.302523084569,10.5626212594563));
#147380=CARTESIAN_POINT('Ctrl Pts',(16.5153433201942,-20.2291697370175,
10.5668431898491));
#147381=CARTESIAN_POINT('Ctrl Pts',(16.4731798646836,-20.1559247880487,
10.5710588812454));
#147382=CARTESIAN_POINT('Ctrl Pts',(16.4345839361667,-20.0804798079436,
10.5752745726417));
#147383=CARTESIAN_POINT('Ctrl Pts',(16.3997870211452,-20.0032134746785,
10.579490264038));
#147384=CARTESIAN_POINT('Ctrl Pts',(16.3650317212897,-19.9260395476307,
10.583700913703));
#147385=CARTESIAN_POINT('Ctrl Pts',(16.3340665899187,-19.8470490030815,
10.587911563368));
#147386=CARTESIAN_POINT('Ctrl Pts',(16.3070776023617,-19.7666457364042,
10.5921222130329));
#147387=CARTESIAN_POINT('Ctrl Pts',(16.2801155537111,-19.686322723796,10.5963286598616));
#147388=CARTESIAN_POINT('Ctrl Pts',(16.2571218975387,-19.6045902181233,
10.6005351066902));
#147389=CARTESIAN_POINT('Ctrl Pts',(16.2382342921444,-19.5218715043693,
10.6047415535189));
#147390=CARTESIAN_POINT('Ctrl Pts',(16.2193575415102,-19.439200329293,10.6089455828907));
#147391=CARTESIAN_POINT('Ctrl Pts',(16.2045822501753,-19.3555445100533,
10.6131496122625));
#147392=CARTESIAN_POINT('Ctrl Pts',(16.1939957867901,-19.271340878805,10.6173536416343));
#147393=CARTESIAN_POINT('Ctrl Pts',(16.1834116610727,-19.1871558411241,
10.6215567426862));
#147394=CARTESIAN_POINT('Ctrl Pts',(16.1770145819502,-19.1024236771961,
10.6257598437382));
#147395=CARTESIAN_POINT('Ctrl Pts',(16.1748403468597,-19.0175886403178,
10.6299629447901));
#147396=CARTESIAN_POINT('Ctrl Pts',(16.1742666403856,-18.9952035679304,
10.6310719997839));
#147397=CARTESIAN_POINT('Ctrl Pts',(16.1739866695752,-18.9728113543428,
10.6321810547777));
#147398=CARTESIAN_POINT('Ctrl Pts',(16.1740004874608,-18.9504201902088,
10.6332901097715));
#147399=CARTESIAN_POINT('',(16.1739802850659,-18.9533010441961,10.5667098967402));
#147400=CARTESIAN_POINT('Ctrl Pts',(20.2935357468249,-20.9821350335323,
10.2832382198805));
#147401=CARTESIAN_POINT('Ctrl Pts',(20.2269313188769,-21.0333000962331,
10.2874225043308));
#147402=CARTESIAN_POINT('Ctrl Pts',(20.1578951114202,-21.081115850127,10.2916067887811));
#147403=CARTESIAN_POINT('Ctrl Pts',(20.0868063431064,-21.1253649021853,
10.2957910732315));
#147404=CARTESIAN_POINT('Ctrl Pts',(20.0559462878668,-21.1445736776812,
10.2976074958864));
#147405=CARTESIAN_POINT('Ctrl Pts',(20.0246997331957,-21.1631109097862,
10.2994239185413));
#147406=CARTESIAN_POINT('Ctrl Pts',(19.9930989518198,-21.1809616034213,
10.3012403411962));
#147407=CARTESIAN_POINT('Ctrl Pts',(19.9202977696528,-21.2220856371494,
10.3054249755893));
#147408=CARTESIAN_POINT('Ctrl Pts',(19.845344231219,-21.2597157589185,10.3096096099823));
#147409=CARTESIAN_POINT('Ctrl Pts',(19.7686077403709,-21.2936205549928,
10.3137942443753));
#147410=CARTESIAN_POINT('Ctrl Pts',(19.6919804744194,-21.3274770917864,
10.3179729224593));
#147411=CARTESIAN_POINT('Ctrl Pts',(19.6135757141378,-21.3576186510691,
10.3221516005432));
#147412=CARTESIAN_POINT('Ctrl Pts',(19.5337886464593,-21.3838589846031,
10.3263302786272));
#147413=CARTESIAN_POINT('Ctrl Pts',(19.4525714529346,-21.410569657257,10.3305838565126));
#147414=CARTESIAN_POINT('Ctrl Pts',(19.3699223286581,-21.43323763244,10.334837434398));
#147415=CARTESIAN_POINT('Ctrl Pts',(19.2862808103368,-21.4517171653077,
10.3390910122835));
#147416=CARTESIAN_POINT('Ctrl Pts',(19.2042608460611,-21.4698384363709,
10.3432621262614));
#147417=CARTESIAN_POINT('Ctrl Pts',(19.1212870932383,-21.4839321143086,
10.3474332402394));
#147418=CARTESIAN_POINT('Ctrl Pts',(19.0377889319357,-21.4939111480997,
10.3516043542173));
#147419=CARTESIAN_POINT('Ctrl Pts',(18.9543187892475,-21.5038868333295,
10.3557740685377));
#147420=CARTESIAN_POINT('Ctrl Pts',(18.8703250439617,-21.5097505619763,
10.3599437828581));
#147421=CARTESIAN_POINT('Ctrl Pts',(18.7862446699246,-21.5114668379302,
10.3641134971784));
#147422=CARTESIAN_POINT('Ctrl Pts',(18.702167287828,-21.5131830528116,10.3682830631225));
#147423=CARTESIAN_POINT('Ctrl Pts',(18.6180037430636,-21.510752099899,10.3724526290665));
#147424=CARTESIAN_POINT('Ctrl Pts',(18.5341921271334,-21.5041905912256,
10.3766221950106));
#147425=CARTESIAN_POINT('Ctrl Pts',(18.44743379818,-21.4973983880017,10.3809383577495));
#147426=CARTESIAN_POINT('Ctrl Pts',(18.3610531319647,-21.4861798052051,
10.3852545204884));
#147427=CARTESIAN_POINT('Ctrl Pts',(18.2755295374792,-21.470611688013,10.3895706832273));
#147428=CARTESIAN_POINT('Ctrl Pts',(18.1927918650885,-21.4555507006011,
10.393746247419));
#147429=CARTESIAN_POINT('Ctrl Pts',(18.1108567316686,-21.4364193523526,
10.3979218116107));
#147430=CARTESIAN_POINT('Ctrl Pts',(18.0301452832766,-21.4133387693989,
10.4020973758024));
#147431=CARTESIAN_POINT('Ctrl Pts',(17.9453572914996,-21.3890924410691,
10.4064838378149));
#147432=CARTESIAN_POINT('Ctrl Pts',(17.8619204024431,-21.3604876310562,
10.4108702998275));
#147433=CARTESIAN_POINT('Ctrl Pts',(17.7802998178502,-21.3277221981047,
10.41525676184));
#147434=CARTESIAN_POINT('Ctrl Pts',(17.6986792332574,-21.2949567651532,
10.4196432238525));
#147435=CARTESIAN_POINT('Ctrl Pts',(17.6188754477654,-21.258031021948,10.4240296858651));
#147436=CARTESIAN_POINT('Ctrl Pts',(17.5413224142635,-21.2171976020828,
10.4284161478776));
#147437=CARTESIAN_POINT('Ctrl Pts',(17.4673377107943,-21.1782429883953,
10.4326007822707));
#147438=CARTESIAN_POINT('Ctrl Pts',(17.3951258047344,-21.135587395429,10.4367854166637));
#147439=CARTESIAN_POINT('Ctrl Pts',(17.3250812297128,-21.0894161734984,
10.4409700510568));
#147440=CARTESIAN_POINT('Ctrl Pts',(17.255136354474,-21.0433106705873,10.4451487291407));
#147441=CARTESIAN_POINT('Ctrl Pts',(17.1873530634459,-20.9936997293727,
10.4493274072247));
#147442=CARTESIAN_POINT('Ctrl Pts',(17.1221018691138,-20.940814826887,10.4535060853086));
#147443=CARTESIAN_POINT('Ctrl Pts',(17.0556810940184,-20.8869820005319,
10.457759663194));
#147444=CARTESIAN_POINT('Ctrl Pts',(16.9918845107681,-20.8297569115571,
10.4620132410795));
#147445=CARTESIAN_POINT('Ctrl Pts',(16.9310725805954,-20.7694302518554,
10.4662668189649));
#147446=CARTESIAN_POINT('Ctrl Pts',(16.8714396083538,-20.7102731421697,
10.4704379329429));
#147447=CARTESIAN_POINT('Ctrl Pts',(16.8146769368997,-20.6481339874867,
10.4746090469208));
#147448=CARTESIAN_POINT('Ctrl Pts',(16.7610901776525,-20.5833267094255,
10.4787801608988));
#147449=CARTESIAN_POINT('Ctrl Pts',(16.70752139996,-20.5185411780723,10.4829498752191));
#147450=CARTESIAN_POINT('Ctrl Pts',(16.6571267108674,-20.4510896556874,
10.4871195895395));
#147451=CARTESIAN_POINT('Ctrl Pts',(16.6101724826409,-20.3813203547519,
10.4912893038599));
#147452=CARTESIAN_POINT('Ctrl Pts',(16.5632199252473,-20.3115535365076,
10.4954588698039));
#147453=CARTESIAN_POINT('Ctrl Pts',(16.5197078414471,-20.2394694858256,
10.499628435748));
#147454=CARTESIAN_POINT('Ctrl Pts',(16.4798593937702,-20.1654455601081,
10.503798001692));
#147455=CARTESIAN_POINT('Ctrl Pts',(16.4386099238314,-20.0888190444807,
10.5081141644309));
#147456=CARTESIAN_POINT('Ctrl Pts',(16.4012867603007,-20.0101141681399,
10.5124303271699));
#147457=CARTESIAN_POINT('Ctrl Pts',(16.3680847835395,-19.9297756330165,
10.5167464899088));
#147458=CARTESIAN_POINT('Ctrl Pts',(16.3359643576791,-19.8520541172246,
10.5209220541005));
#147459=CARTESIAN_POINT('Ctrl Pts',(16.307700860257,-19.7728042005823,10.5250976182921));
#147460=CARTESIAN_POINT('Ctrl Pts',(16.2834204017388,-19.6924455635533,
10.5292731824838));
#147461=CARTESIAN_POINT('Ctrl Pts',(16.257913594982,-19.6080282028025,10.5336596444963));
#147462=CARTESIAN_POINT('Ctrl Pts',(16.236802907853,-19.522387742153,10.5380461065089));
#147463=CARTESIAN_POINT('Ctrl Pts',(16.2201737773397,-19.4360224398369,
10.5424325685214));
#147464=CARTESIAN_POINT('Ctrl Pts',(16.2035446468265,-19.3496571375208,
10.546819030534));
#147465=CARTESIAN_POINT('Ctrl Pts',(16.1913970777482,-19.2625675787001,
10.5512054925465));
#147466=CARTESIAN_POINT('Ctrl Pts',(16.1837535357011,-19.1752553948527,
10.555591954559));
#147467=CARTESIAN_POINT('Ctrl Pts',(16.1772957565522,-19.1014881810632,
10.5592979331155));
#147468=CARTESIAN_POINT('Ctrl Pts',(16.174038011382,-19.0274367677245,10.563003911672));
#147469=CARTESIAN_POINT('Ctrl Pts',(16.1740003306697,-18.9533011644427,
10.5667098902285));
#147470=CARTESIAN_POINT('Ctrl Pts',(16.1705864007212,-18.9532806854788,
10.5667109992167));
#147471=CARTESIAN_POINT('Ctrl Pts',(16.1754042043383,-18.178366800346,10.6053965865579));
#147472=CARTESIAN_POINT('Ctrl Pts',(16.9631831042392,-16.5458334607307,
10.6864741094597));
#147473=CARTESIAN_POINT('Ctrl Pts',(19.7422306997689,-16.0977465603627,
10.8099435679219));
#147474=CARTESIAN_POINT('Ctrl Pts',(21.6797116025125,-18.2548092108606,
10.9371193746034));
#147475=CARTESIAN_POINT('Ctrl Pts',(21.1313727461762,-20.2593600726663,
11.0282736309673));
#147476=CARTESIAN_POINT('Ctrl Pts',(20.3968579082113,-20.906920109619,11.0770359517708));
#147477=CARTESIAN_POINT('Ctrl Pts',(20.2948050232963,-20.9838171774959,
11.0834063370138));
#147478=CARTESIAN_POINT('Origin',(18.734,-18.952,-1.76670989022851));
#147479=CARTESIAN_POINT('',(20.2935357468249,-20.9821350335323,11.9498687307687));
#147480=CARTESIAN_POINT('',(20.2935357468249,-20.9821350335323,11.8833305117342));
#147481=CARTESIAN_POINT('',(20.2935357468249,-20.9821350335323,-1.76670989022851));
#147482=CARTESIAN_POINT('',(16.1739804747524,-18.9506989546656,11.4332901033215));
#147483=CARTESIAN_POINT('Ctrl Pts',(16.1740003306697,-18.950698835557,11.4332901097715));
#147484=CARTESIAN_POINT('Ctrl Pts',(16.174038011382,-18.8765632322752,11.436996088328));
#147485=CARTESIAN_POINT('Ctrl Pts',(16.1772957565522,-18.8025118189363,
11.4407020668845));
#147486=CARTESIAN_POINT('Ctrl Pts',(16.1837535357011,-18.7287446051466,
11.444408045441));
#147487=CARTESIAN_POINT('Ctrl Pts',(16.1910453870482,-18.6454497843057,
11.448592679834));
#147488=CARTESIAN_POINT('Ctrl Pts',(16.2024358975503,-18.5623575749321,
11.4527773142271));
#147489=CARTESIAN_POINT('Ctrl Pts',(16.217906819526,-18.4799034980302,11.4569619486201));
#147490=CARTESIAN_POINT('Ctrl Pts',(16.2333557205591,-18.3975667843009,
11.4611406267041));
#147491=CARTESIAN_POINT('Ctrl Pts',(16.2528734125179,-18.3158668471442,
11.465319304788));
#147492=CARTESIAN_POINT('Ctrl Pts',(16.2763898192684,-18.2352349062878,
11.469497982872));
#147493=CARTESIAN_POINT('Ctrl Pts',(16.3003277407088,-18.1531576958409,
11.4737515607574));
#147494=CARTESIAN_POINT('Ctrl Pts',(16.3284090988417,-18.0721876262597,
11.4780051386428));
#147495=CARTESIAN_POINT('Ctrl Pts',(16.3605053261112,-17.9927695620856,
11.4822587165282));
#147496=CARTESIAN_POINT('Ctrl Pts',(16.3919793053844,-17.9148911720571,
11.4864298305062));
#147497=CARTESIAN_POINT('Ctrl Pts',(16.4273136905277,-17.8385055933013,
11.4906009444841));
#147498=CARTESIAN_POINT('Ctrl Pts',(16.4663372697809,-17.7640161019714,
11.4947720584621));
#147499=CARTESIAN_POINT('Ctrl Pts',(16.5053477542952,-17.6895516063097,
11.4989417727825));
#147500=CARTESIAN_POINT('Ctrl Pts',(16.5480447610381,-17.6169823416312,
11.5031114871028));
#147501=CARTESIAN_POINT('Ctrl Pts',(16.5942102750742,-17.5466886704001,
11.5072812014232));
#147502=CARTESIAN_POINT('Ctrl Pts',(16.6403741463431,-17.4763975005194,
11.5114507673673));
#147503=CARTESIAN_POINT('Ctrl Pts',(16.6900060262586,-17.4083821471394,
11.5156203333113));
#147504=CARTESIAN_POINT('Ctrl Pts',(16.7428443053793,-17.3429944065419,
11.5197898992553));
#147505=CARTESIAN_POINT('Ctrl Pts',(16.7975403132107,-17.2753077136495,
11.5241060619943));
#147506=CARTESIAN_POINT('Ctrl Pts',(16.8556720579014,-17.2104372553887,
11.5284222247332));
#147507=CARTESIAN_POINT('Ctrl Pts',(16.9169048877879,-17.1487348078625,
11.5327383874721));
#147508=CARTESIAN_POINT('Ctrl Pts',(16.9761430646814,-17.0890423110745,
11.5369139516638));
#147509=CARTESIAN_POINT('Ctrl Pts',(17.0382830139764,-17.0323148814136,
11.5410895158555));
#147510=CARTESIAN_POINT('Ctrl Pts',(17.1029865459476,-16.9788312001503,
11.5452650800471));
#147511=CARTESIAN_POINT('Ctrl Pts',(17.1709580995006,-16.9226461852919,
11.5496515420597));
#147512=CARTESIAN_POINT('Ctrl Pts',(17.2417585461137,-16.8700415621994,
11.5540380040722));
#147513=CARTESIAN_POINT('Ctrl Pts',(17.3149615008575,-16.8212889126042,
11.5584244660848));
#147514=CARTESIAN_POINT('Ctrl Pts',(17.3881644556012,-16.772536263009,11.5628109280973));
#147515=CARTESIAN_POINT('Ctrl Pts',(17.4637693807619,-16.7276358177823,
11.5671973901098));
#147516=CARTESIAN_POINT('Ctrl Pts',(17.5413224142637,-16.6868023979171,
11.5715838521224));
#147517=CARTESIAN_POINT('Ctrl Pts',(17.615307117733,-16.6478477842295,11.5757684865154));
#147518=CARTESIAN_POINT('Ctrl Pts',(17.6913399834857,-16.6124491640088,
11.5799531209085));
#147519=CARTESIAN_POINT('Ctrl Pts',(17.7690449301558,-16.5808269331021,
11.5841377553015));
#147520=CARTESIAN_POINT('Ctrl Pts',(17.8466392734524,-16.549249712527,11.5883164333855));
#147521=CARTESIAN_POINT('Ctrl Pts',(17.9259005477808,-16.5214383763015,
11.5924951114694));
#147522=CARTESIAN_POINT('Ctrl Pts',(18.0064282347098,-16.4975674125468,
11.5966737895534));
#147523=CARTESIAN_POINT('Ctrl Pts',(18.0883993225526,-16.4732685789225,
11.6009273674388));
#147524=CARTESIAN_POINT('Ctrl Pts',(18.1716822438314,-16.4530529941954,
11.6051809453242));
#147525=CARTESIAN_POINT('Ctrl Pts',(18.2558333466885,-16.4370533501362,
11.6094345232097));
#147526=CARTESIAN_POINT('Ctrl Pts',(18.3383530162095,-16.4213638903979,
11.6136056371876));
#147527=CARTESIAN_POINT('Ctrl Pts',(18.4217070321717,-16.4097284515022,
11.6177767511656));
#147528=CARTESIAN_POINT('Ctrl Pts',(18.5054636294717,-16.4022213571869,
11.6219478651435));
#147529=CARTESIAN_POINT('Ctrl Pts',(18.5891921214365,-16.3947167819496,
11.6261175794639));
#147530=CARTESIAN_POINT('Ctrl Pts',(18.6733224686331,-16.3913378410871,
11.6302872937843));
#147531=CARTESIAN_POINT('Ctrl Pts',(18.7574168390734,-16.3921071015279,
11.6344570081047));
#147532=CARTESIAN_POINT('Ctrl Pts',(18.8415082170751,-16.3928763345952,
11.6386265740487));
#147533=CARTESIAN_POINT('Ctrl Pts',(18.92556316086,-16.3977934704174,11.6427961399927));
#147534=CARTESIAN_POINT('Ctrl Pts',(19.0091442611991,-16.4068289575101,
11.6469657059368));
#147535=CARTESIAN_POINT('Ctrl Pts',(19.0956639699176,-16.4161821211824,
11.6512818686757));
#147536=CARTESIAN_POINT('Ctrl Pts',(19.1816753701877,-16.4299485702282,
11.6555980314146));
#147537=CARTESIAN_POINT('Ctrl Pts',(19.2667015333783,-16.4480373252909,
11.6599141941536));
#147538=CARTESIAN_POINT('Ctrl Pts',(19.3489579782461,-16.46553684106,11.6640897583452));
#147539=CARTESIAN_POINT('Ctrl Pts',(19.4302919452567,-16.4870812228023,
11.6682653225369));
#147540=CARTESIAN_POINT('Ctrl Pts',(19.5102860518794,-16.5125369513646,
11.6724408867286));
#147541=CARTESIAN_POINT('Ctrl Pts',(19.5943204706598,-16.5392783882614,
11.6768273487411));
#147542=CARTESIAN_POINT('Ctrl Pts',(19.6768755727334,-16.570336474695,11.6812138107537));
#147543=CARTESIAN_POINT('Ctrl Pts',(19.7574922067679,-16.605499690457,11.6856002727662));
#147544=CARTESIAN_POINT('Ctrl Pts',(19.8381088408023,-16.640662906219,11.6899867347788));
#147545=CARTESIAN_POINT('Ctrl Pts',(19.9167865216171,-16.6799309241434,
11.6943731967913));
#147546=CARTESIAN_POINT('Ctrl Pts',(19.9930989518199,-16.7230383965788,
11.6987596588038));
#147547=CARTESIAN_POINT('Ctrl Pts',(20.0659001339868,-16.7641624303068,
11.7029442931969));
#147548=CARTESIAN_POINT('Ctrl Pts',(20.1368199197938,-16.8089334362054,
11.7071289275899));
#147549=CARTESIAN_POINT('Ctrl Pts',(20.2054694255015,-16.8571544854538,
11.711313561983));
#147550=CARTESIAN_POINT('Ctrl Pts',(20.2740212171349,-16.9053068980071,
11.7154922400669));
#147551=CARTESIAN_POINT('Ctrl Pts',(20.3403087741461,-16.9568993375336,
11.7196709181509));
#147552=CARTESIAN_POINT('Ctrl Pts',(20.4039685866081,-17.0116894785262,
11.7238495962348));
#147553=CARTESIAN_POINT('Ctrl Pts',(20.4687694554571,-17.0674616934192,
11.7281031741202));
#147554=CARTESIAN_POINT('Ctrl Pts',(20.5308470287296,-17.1265471378127,
11.7323567520057));
#147555=CARTESIAN_POINT('Ctrl Pts',(20.5898495933096,-17.1886445942429,
11.7366103298911));
#147556=CARTESIAN_POINT('Ctrl Pts',(20.647708278041,-17.2495381703069,11.7407814438691));
#147557=CARTESIAN_POINT('Ctrl Pts',(20.7026097887106,-17.3133276642815,
11.744952557847));
#147558=CARTESIAN_POINT('Ctrl Pts',(20.7542579245552,-17.3796902600722,
11.749123671825));
#147559=CARTESIAN_POINT('Ctrl Pts',(20.8058887293691,-17.446030587253,11.7532933861453));
#147560=CARTESIAN_POINT('Ctrl Pts',(20.8542680451848,-17.5149419387271,
11.7574631004657));
#147561=CARTESIAN_POINT('Ctrl Pts',(20.8991399066356,-17.5860683821311,
11.7616328147861));
#147562=CARTESIAN_POINT('Ctrl Pts',(20.944010171353,-17.6571922945511,11.7658023807301));
#147563=CARTESIAN_POINT('Ctrl Pts',(20.9853729851228,-17.7305307526506,
11.7699719466742));
#147564=CARTESIAN_POINT('Ctrl Pts',(21.0230164347473,-17.8056999688315,
11.7741415126182));
#147565=CARTESIAN_POINT('Ctrl Pts',(21.0619833816224,-17.8835120419222,
11.7784576753571));
#147566=CARTESIAN_POINT('Ctrl Pts',(21.0969643161937,-17.9632855357174,
11.7827738380961));
#147567=CARTESIAN_POINT('Ctrl Pts',(21.12777758528,-18.0445701833138,11.787090000835));
#147568=CARTESIAN_POINT('Ctrl Pts',(21.1575871153666,-18.1232069920642,
11.7912655650267));
#147569=CARTESIAN_POINT('Ctrl Pts',(21.1834962335158,-18.2032575521564,
11.7954411292184));
#147570=CARTESIAN_POINT('Ctrl Pts',(21.205391286958,-18.284298639549,11.79961669341));
#147571=CARTESIAN_POINT('Ctrl Pts',(21.228392207499,-18.369432919609,11.8040031554226));
#147572=CARTESIAN_POINT('Ctrl Pts',(21.2469627828282,-18.4556598489483,
11.8083896174351));
#147573=CARTESIAN_POINT('Ctrl Pts',(21.2610323380594,-18.5424788620813,
11.8127760794477));
#147574=CARTESIAN_POINT('Ctrl Pts',(21.2751018932905,-18.6292978752144,
11.8171625414602));
#147575=CARTESIAN_POINT('Ctrl Pts',(21.2846704408995,-18.7167083870925,
11.8215490034728));
#147576=CARTESIAN_POINT('Ctrl Pts',(21.2897303495758,-18.8042083214207,
11.8259354654853));
#147577=CARTESIAN_POINT('Ctrl Pts',(21.2945575272398,-18.8876836874037,
11.8301201717332));
#147578=CARTESIAN_POINT('Ctrl Pts',(21.2952996738552,-18.9715511471385,
11.834304877981));
#147579=CARTESIAN_POINT('Ctrl Pts',(21.2919118781324,-19.0553770947037,
11.8384895842288));
#147580=CARTESIAN_POINT('Ctrl Pts',(21.2885289204162,-19.1390833330158,
11.8426683144266));
#147581=CARTESIAN_POINT('Ctrl Pts',(21.2810277540022,-19.2227477211518,
11.8468470446243));
#147582=CARTESIAN_POINT('Ctrl Pts',(21.2694153767464,-19.3059334222111,
11.8510257748221));
#147583=CARTESIAN_POINT('Ctrl Pts',(21.2578166868028,-19.3890210736947,
11.8551995796214));
#147584=CARTESIAN_POINT('Ctrl Pts',(21.2421164820724,-19.4716307064917,
11.8593733844208));
#147585=CARTESIAN_POINT('Ctrl Pts',(21.2223736966772,-19.5533288166098,
11.8635471892201));
#147586=CARTESIAN_POINT('Ctrl Pts',(21.2026437041557,-19.6349739882196,
11.8677182894893));
#147587=CARTESIAN_POINT('Ctrl Pts',(21.1788764395496,-19.7157083639712,
11.8718893897585));
#147588=CARTESIAN_POINT('Ctrl Pts',(21.1511820426485,-19.7951079247032,
11.8760604900277));
#147589=CARTESIAN_POINT('Ctrl Pts',(21.1234972832818,-19.8744798547202,
11.8802301387714));
#147590=CARTESIAN_POINT('Ctrl Pts',(21.0918882575024,-19.9525174584111,
11.8843997875152));
#147591=CARTESIAN_POINT('Ctrl Pts',(21.0565147608215,-20.0288125118916,
11.8885694362589));
#147592=CARTESIAN_POINT('Ctrl Pts',(21.0211429628483,-20.1051039015276,
11.8927388847676));
#147593=CARTESIAN_POINT('Ctrl Pts',(20.9820072479426,-20.1796524905174,
11.8969083332763));
#147594=CARTESIAN_POINT('Ctrl Pts',(20.9393147224056,-20.2520719115269,
11.901077781785));
#147595=CARTESIAN_POINT('Ctrl Pts',(20.8965841485734,-20.3245558739396,
11.9052509461761));
#147596=CARTESIAN_POINT('Ctrl Pts',(20.8502906654462,-20.3949064803433,
11.9094241105673));
#147597=CARTESIAN_POINT('Ctrl Pts',(20.8006860848122,-20.4627642525701,
11.9135972749584));
#147598=CARTESIAN_POINT('Ctrl Pts',(20.7510600241141,-20.5306514089642,
11.9177722464375));
#147599=CARTESIAN_POINT('Ctrl Pts',(20.6981202983344,-20.5960432219192,
11.9219472179166));
#147600=CARTESIAN_POINT('Ctrl Pts',(20.6421591183141,-20.6586132482771,
11.9261221893957));
#147601=CARTESIAN_POINT('Ctrl Pts',(20.5861048295069,-20.7212873792883,
11.9303041072353));
#147602=CARTESIAN_POINT('Ctrl Pts',(20.5270193651334,-20.7811300141776,
11.9344860250748));
#147603=CARTESIAN_POINT('Ctrl Pts',(20.4652317777506,-20.8378516727745,
11.9386679429144));
#147604=CARTESIAN_POINT('Ctrl Pts',(20.4100681196037,-20.8884924942875,
11.9424015388658));
#147605=CARTESIAN_POINT('Ctrl Pts',(20.3527513118673,-20.9366460444125,
11.9461351348173));
#147606=CARTESIAN_POINT('Ctrl Pts',(20.2935357468249,-20.9821350335323,
11.9498687307687));
#147607=CARTESIAN_POINT('Ctrl Pts',(20.292281765808,-20.9805345212664,11.1497835179515));
#147608=CARTESIAN_POINT('Ctrl Pts',(20.0792747299441,-21.1470794377456,
11.1632078226604));
#147609=CARTESIAN_POINT('Ctrl Pts',(19.0902279379876,-21.7011259077543,
11.2190240629297));
#147610=CARTESIAN_POINT('Ctrl Pts',(16.9631832264668,-21.35816637253,11.3135258905595));
#147611=CARTESIAN_POINT('Ctrl Pts',(16.1754043811927,-19.7256331452917,
11.3946034134805));
#147612=CARTESIAN_POINT('Ctrl Pts',(16.1705865782758,-18.9507193134542,
11.433289000841));
#147613=CARTESIAN_POINT('',(16.1740004874608,-18.9535798097909,11.3667098902285));
#147614=CARTESIAN_POINT('Ctrl Pts',(20.2948050232963,-20.9838171774959,
11.0834063370138));
#147615=CARTESIAN_POINT('Ctrl Pts',(19.7177436700502,-21.4186341460381,
11.1194278873312));
#147616=CARTESIAN_POINT('Ctrl Pts',(18.0373628489283,-21.8291475591767,
11.1978413732092));
#147617=CARTESIAN_POINT('Ctrl Pts',(16.3822353344203,-20.4522479494082,
11.2922755723059));
#147618=CARTESIAN_POINT('Ctrl Pts',(16.1753927157401,-19.2766421922516,
11.350688221085));
#147619=CARTESIAN_POINT('Ctrl Pts',(16.177204683354,-18.953597107844,11.3667089343037));
#147620=CARTESIAN_POINT('Ctrl Pts',(16.1740004874608,-18.9535798097909,
11.3667098902285));
#147621=CARTESIAN_POINT('Ctrl Pts',(16.1739481146197,-18.8687123476393,
11.3709134538372));
#147622=CARTESIAN_POINT('Ctrl Pts',(16.1781202862138,-18.7838299700766,
11.3751170174459));
#147623=CARTESIAN_POINT('Ctrl Pts',(16.1864949217896,-18.699377996817,11.3793205810546));
#147624=CARTESIAN_POINT('Ctrl Pts',(16.1948707822013,-18.6149136719983,
11.3835247594573));
#147625=CARTESIAN_POINT('Ctrl Pts',(16.2074502833288,-18.5308803238368,
11.3877289378599));
#147626=CARTESIAN_POINT('Ctrl Pts',(16.2241595327126,-18.447717510946,11.3919331162626));
#147627=CARTESIAN_POINT('Ctrl Pts',(16.2408759290274,-18.3645191274036,
11.3961390928892));
#147628=CARTESIAN_POINT('Ctrl Pts',(16.2617254950327,-18.2821924593937,
11.4003450695159));
#147629=CARTESIAN_POINT('Ctrl Pts',(16.2865836343726,-18.2011650425965,
11.4045510461425));
#147630=CARTESIAN_POINT('Ctrl Pts',(16.3114761780105,-18.1200254817903,
11.408762843948));
#147631=CARTESIAN_POINT('Ctrl Pts',(16.3403882340966,-18.0401891906195,
11.4129746417534));
#147632=CARTESIAN_POINT('Ctrl Pts',(16.3731460171586,-17.9620664306621,
11.4171864395589));
#147633=CARTESIAN_POINT('Ctrl Pts',(16.4059305542806,-17.8838798659902,
11.4214016772397));
#147634=CARTESIAN_POINT('Ctrl Pts',(16.4425668768385,-17.8074100228066,
11.4256169149205));
#147635=CARTESIAN_POINT('Ctrl Pts',(16.4828349986458,-17.7330430127859,
11.4298321526013));
#147636=CARTESIAN_POINT('Ctrl Pts',(16.5231739006091,-17.6585452862497,
11.4340547994973));
#147637=CARTESIAN_POINT('Ctrl Pts',(16.5671571084147,-17.5861581518398,
11.4382774463933));
#147638=CARTESIAN_POINT('Ctrl Pts',(16.6145212917447,-17.5162388759782,
11.4425000932893));
#147639=CARTESIAN_POINT('Ctrl Pts',(16.6269438222717,-17.4979006660113,
11.4436075959693));
#147640=CARTESIAN_POINT('Ctrl Pts',(16.6395987151329,-17.4797320374711,
11.4447150986492));
#147641=CARTESIAN_POINT('Ctrl Pts',(16.6524807786036,-17.4617390393098,
11.4458226013291));
#147642=CARTESIAN_POINT('Ctrl Pts',(16.7011549053849,-17.3937535433782,
11.4500072357222));
#147643=CARTESIAN_POINT('Ctrl Pts',(16.7532538754926,-17.3280286903787,
11.4541918701152));
#147644=CARTESIAN_POINT('Ctrl Pts',(16.8085402991528,-17.2649300724589,
11.4583765045082));
#147645=CARTESIAN_POINT('Ctrl Pts',(16.8637480294321,-17.2019212676117,
11.4625551825922));
#147646=CARTESIAN_POINT('Ctrl Pts',(16.9221339008884,-17.1415316158069,
11.4667338606761));
#147647=CARTESIAN_POINT('Ctrl Pts',(16.9834181011141,-17.0840966258147,
11.4709125387601));
#147648=CARTESIAN_POINT('Ctrl Pts',(17.0458007765846,-17.0256321549047,
11.4751661166455));
#147649=CARTESIAN_POINT('Ctrl Pts',(17.1111864272472,-16.9702297043271,
11.479419694531));
#147650=CARTESIAN_POINT('Ctrl Pts',(17.1792379481546,-16.9182067553113,
11.4836732724164));
#147651=CARTESIAN_POINT('Ctrl Pts',(17.2459701575375,-16.8671923726766,
11.4878443863943));
#147652=CARTESIAN_POINT('Ctrl Pts',(17.3152654110889,-16.8194279167438,
11.4920155003723));
#147653=CARTESIAN_POINT('Ctrl Pts',(17.3867710660549,-16.7751733648402,
11.4961866143502));
#147654=CARTESIAN_POINT('Ctrl Pts',(17.4582527266079,-16.7309336629788,
11.5003563286706));
#147655=CARTESIAN_POINT('Ctrl Pts',(17.5319429246537,-16.6902017679485,
11.504526042991));
#147656=CARTESIAN_POINT('Ctrl Pts',(17.6074603942083,-16.6531941107213,
11.5086957573114));
#147657=CARTESIAN_POINT('Ctrl Pts',(17.6829751765273,-16.6161877703852,
11.5128653232554));
#147658=CARTESIAN_POINT('Ctrl Pts',(17.7603166876031,-16.5829056060341,
11.5170348891995));
#147659=CARTESIAN_POINT('Ctrl Pts',(17.8390806772786,-16.5535172700601,
11.5212044551435));
#147660=CARTESIAN_POINT('Ctrl Pts',(17.9206139116649,-16.5230956764478,
11.5255206178824));
#147661=CARTESIAN_POINT('Ctrl Pts',(18.0036710203273,-16.4968470041692,
11.5298367806213));
#147662=CARTESIAN_POINT('Ctrl Pts',(18.0877848913439,-16.4749037093111,
11.5341529433603));
#147663=CARTESIAN_POINT('Ctrl Pts',(18.1691587618594,-16.453675214975,11.5383285075519));
#147664=CARTESIAN_POINT('Ctrl Pts',(18.2515211332009,-16.4364759603011,
11.5425040717436));
#147665=CARTESIAN_POINT('Ctrl Pts',(18.3344390537292,-16.4233736831601,
11.5466796359353));
#147666=CARTESIAN_POINT('Ctrl Pts',(18.4215449613047,-16.4096096411485,
11.5510660979478));
#147667=CARTESIAN_POINT('Ctrl Pts',(18.5092634338796,-16.4003673913993,
11.5554525599604));
#147668=CARTESIAN_POINT('Ctrl Pts',(18.5970892183629,-16.3956636688668,
11.5598390219729));
#147669=CARTESIAN_POINT('Ctrl Pts',(18.6849150028461,-16.3909599463343,
11.5642254839854));
#147670=CARTESIAN_POINT('Ctrl Pts',(18.7728475188788,-16.3907946760441,
11.568611945998));
#147671=CARTESIAN_POINT('Ctrl Pts',(18.8603867536229,-16.3951217493771,
11.5729984080105));
#147672=CARTESIAN_POINT('Ctrl Pts',(18.9438981784123,-16.3992497276517,
11.5771830424036));
#147673=CARTESIAN_POINT('Ctrl Pts',(19.0273625629856,-16.4074811003133,
11.5813676767966));
#147674=CARTESIAN_POINT('Ctrl Pts',(19.1103440076207,-16.4198141482253,
11.5855523111897));
#147675=CARTESIAN_POINT('Ctrl Pts',(19.1932073384403,-16.4321296415701,
11.5897309892736));
#147676=CARTESIAN_POINT('Ctrl Pts',(19.2755886435822,-16.4485351465588,
11.5939096673576));
#147677=CARTESIAN_POINT('Ctrl Pts',(19.3570543561167,-16.4689769897715,
11.5980883454415));
#147678=CARTESIAN_POINT('Ctrl Pts',(19.4399802830001,-16.4897852383326,
11.6023419233269));
#147679=CARTESIAN_POINT('Ctrl Pts',(19.5219569888747,-16.5147759273293,
11.6065955012124));
#147680=CARTESIAN_POINT('Ctrl Pts',(19.6025350537547,-16.5438374514167,
11.6108490790978));
#147681=CARTESIAN_POINT('Ctrl Pts',(19.681550955612,-16.5723355611508,11.6150201930758));
#147682=CARTESIAN_POINT('Ctrl Pts',(19.7592215106215,-16.6047479091041,
11.6191913070537));
#147683=CARTESIAN_POINT('Ctrl Pts',(19.8351372401589,-16.6409186993238,
11.6233624210317));
#147684=CARTESIAN_POINT('Ctrl Pts',(19.9110274954401,-16.6770773520855,
11.627532135352));
#147685=CARTESIAN_POINT('Ctrl Pts',(19.9851636797555,-16.716991744677,11.6317018496724));
#147686=CARTESIAN_POINT('Ctrl Pts',(20.0571574368627,-16.7604584427223,
11.6358715639928));
#147687=CARTESIAN_POINT('Ctrl Pts',(20.129148632123,-16.803923594036,11.6400411299368));
#147688=CARTESIAN_POINT('Ctrl Pts',(20.198997158373,-16.8509405609741,11.6442106958809));
#147689=CARTESIAN_POINT('Ctrl Pts',(20.2663415518561,-16.9012612627506,
11.6483802618249));
#147690=CARTESIAN_POINT('Ctrl Pts',(20.3360536911358,-16.9533511783243,
11.6526964245638));
#147691=CARTESIAN_POINT('Ctrl Pts',(20.403081908196,-17.008981154178,11.6570125873028));
#147692=CARTESIAN_POINT('Ctrl Pts',(20.4670619896056,-17.0678301190751,
11.6613287500417));
#147693=CARTESIAN_POINT('Ctrl Pts',(20.5289579265927,-17.1247620851305,
11.6655043142334));
#147694=CARTESIAN_POINT('Ctrl Pts',(20.5880009674137,-17.1847061749556,
11.6696798784251));
#147695=CARTESIAN_POINT('Ctrl Pts',(20.6438998067281,-17.2473350099624,
11.6738554426167));
#147696=CARTESIAN_POINT('Ctrl Pts',(20.7026219635295,-17.3131270785395,
11.6782419046293));
#147697=CARTESIAN_POINT('Ctrl Pts',(20.7578735784432,-17.3818817777297,
11.6826283666418));
#147698=CARTESIAN_POINT('Ctrl Pts',(20.809367096106,-17.4531833279548,11.6870148286544));
#147699=CARTESIAN_POINT('Ctrl Pts',(20.8608606137687,-17.5244848781798,
11.6914012906669));
#147700=CARTESIAN_POINT('Ctrl Pts',(20.9085957830846,-17.5983327508675,
11.6957877526794));
#147701=CARTESIAN_POINT('Ctrl Pts',(20.9523407266399,-17.6742815566288,
11.700174214692));
#147702=CARTESIAN_POINT('Ctrl Pts',(20.9940729004966,-17.746735845254,11.704358849085));
#147703=CARTESIAN_POINT('Ctrl Pts',(21.0323293070736,-17.8213716700563,
11.7085434834781));
#147704=CARTESIAN_POINT('Ctrl Pts',(21.0668754476401,-17.8978215778161,
11.7127281178711));
#147705=CARTESIAN_POINT('Ctrl Pts',(21.1013724160514,-17.9741626685948,
11.7169067959551));
#147706=CARTESIAN_POINT('Ctrl Pts',(21.1321694205717,-18.0523122977901,
11.721085474039));
#147707=CARTESIAN_POINT('Ctrl Pts',(21.159076910497,-18.131876851824,11.725264152123));
#147708=CARTESIAN_POINT('Ctrl Pts',(21.1864666978413,-18.2128675433069,
11.7295177300084));
#147709=CARTESIAN_POINT('Ctrl Pts',(21.2098259193361,-18.2953239658205,
11.7337713078938));
#147710=CARTESIAN_POINT('Ctrl Pts',(21.2290051549002,-18.3788078184225,
11.7380248857793));
#147711=CARTESIAN_POINT('Ctrl Pts',(21.2478125635577,-18.4606731736366,
11.7421959997572));
#147712=CARTESIAN_POINT('Ctrl Pts',(21.2626005065823,-18.5435260079661,
11.7463671137352));
#147713=CARTESIAN_POINT('Ctrl Pts',(21.2732783407021,-18.6269376852951,
11.7505382277131));
#147714=CARTESIAN_POINT('Ctrl Pts',(21.2839525917715,-18.7103213730302,
11.7547079420335));
#147715=CARTESIAN_POINT('Ctrl Pts',(21.2905194146576,-18.7942630754074,
11.7588776563539));
#147716=CARTESIAN_POINT('Ctrl Pts',(21.2929396556081,-18.8783261311164,
11.7630473706743));
#147717=CARTESIAN_POINT('Ctrl Pts',(21.295359810436,-18.9623861955009,11.7672169366183));
#147718=CARTESIAN_POINT('Ctrl Pts',(21.2936336643145,-19.0465671447645,
11.7713865025623));
#147719=CARTESIAN_POINT('Ctrl Pts',(21.2877741604491,-19.1304307636664,
11.7755560685064));
#147720=CARTESIAN_POINT('Ctrl Pts',(21.2817086436563,-19.2172429239521,
11.7798722312453));
#147721=CARTESIAN_POINT('Ctrl Pts',(21.2712137402018,-19.3037144978781,
11.7841883939842));
#147722=CARTESIAN_POINT('Ctrl Pts',(21.2563622783627,-19.389365449816,11.7885045567231));
#147723=CARTESIAN_POINT('Ctrl Pts',(21.2419946013309,-19.4722263310034,
11.7926801209148));
#147724=CARTESIAN_POINT('Ctrl Pts',(21.2235499863025,-19.5543187834628,
11.7968556851065));
#147725=CARTESIAN_POINT('Ctrl Pts',(21.2011460288054,-19.6352206616825,
11.8010312492982));
#147726=CARTESIAN_POINT('Ctrl Pts',(21.1776105006754,-19.7202087014452,
11.8054177113107));
#147727=CARTESIAN_POINT('Ctrl Pts',(21.1497053305465,-19.8038821804657,
11.8098041733232));
#147728=CARTESIAN_POINT('Ctrl Pts',(21.1176244749812,-19.8857742565901,
11.8141906353358));
#147729=CARTESIAN_POINT('Ctrl Pts',(21.085543619416,-19.9676663327146,11.8185770973483));
#147730=CARTESIAN_POINT('Ctrl Pts',(21.0492873869465,-20.0477765087051,
11.8229635593609));
#147731=CARTESIAN_POINT('Ctrl Pts',(21.0091047687183,-20.1256687315232,
11.8273500213734));
#147732=CARTESIAN_POINT('Ctrl Pts',(20.9707678090114,-20.1999832271766,
11.8315350054497));
#147733=CARTESIAN_POINT('Ctrl Pts',(20.9287145340163,-20.2725556853794,
11.8357199895261));
#147734=CARTESIAN_POINT('Ctrl Pts',(20.8831270316855,-20.3429899358654,
11.8399049736024));
#147735=CARTESIAN_POINT('Ctrl Pts',(20.837615826569,-20.4133063045453,11.8440829535085));
#147736=CARTESIAN_POINT('Ctrl Pts',(20.7885824023179,-20.4814911976132,
11.8482609334146));
#147737=CARTESIAN_POINT('Ctrl Pts',(20.7362550110441,-20.5471723639622,
11.8524389133207));
#147738=CARTESIAN_POINT('Ctrl Pts',(20.6839782703651,-20.6127899538542,
11.8566128491275));
#147739=CARTESIAN_POINT('Ctrl Pts',(20.6284141773795,-20.6759082704892,
11.8607867849342));
#147740=CARTESIAN_POINT('Ctrl Pts',(20.5698341380259,-20.736184132218,11.864960720741));
#147741=CARTESIAN_POINT('Ctrl Pts',(20.5112960173948,-20.7964168617272,
11.8691316697615));
#147742=CARTESIAN_POINT('Ctrl Pts',(20.4497465580618,-20.8538108487051,
11.873302618782));
#147743=CARTESIAN_POINT('Ctrl Pts',(20.3854963550761,-20.9080572049842,
11.8774735678025));
#147744=CARTESIAN_POINT('Ctrl Pts',(20.3554224770341,-20.9334485380407,
11.8794258824464));
#147745=CARTESIAN_POINT('Ctrl Pts',(20.3247574231983,-20.9581507568336,
11.8813781970903));
#147746=CARTESIAN_POINT('Ctrl Pts',(20.2935357468249,-20.9821350335323,
11.8833305117342));
#147747=CARTESIAN_POINT('Origin',(18.734,-18.952,-1.76670989022851));
#147748=CARTESIAN_POINT('',(20.2935357468249,-20.9821350335323,12.7499597608822));
#147749=CARTESIAN_POINT('',(20.2929505273092,-20.9813917755493,12.683192392576));
#147750=CARTESIAN_POINT('',(20.2935357468249,-20.9821350335323,-1.76670989022851));
#147751=CARTESIAN_POINT('',(16.1740010233873,-18.9542890482673,12.2332901098107));
#147752=CARTESIAN_POINT('Ctrl Pts',(16.1740010233873,-18.9542890482673,
12.2332901098107));
#147753=CARTESIAN_POINT('Ctrl Pts',(16.1739252094451,-18.869501140071,12.2375129674107));
#147754=CARTESIAN_POINT('Ctrl Pts',(16.1780663695147,-18.7845778436852,
12.2417358250107));
#147755=CARTESIAN_POINT('Ctrl Pts',(16.1864353355331,-18.6999796032861,
12.2459586826108));
#147756=CARTESIAN_POINT('Ctrl Pts',(16.1945865434513,-18.6175825848873,
12.2500716626647));
#147757=CARTESIAN_POINT('Ctrl Pts',(16.2067481850333,-18.5354944186516,
12.2541846427187));
#147758=CARTESIAN_POINT('Ctrl Pts',(16.2228775801224,-18.4541403888766,
12.2582976227727));
#147759=CARTESIAN_POINT('Ctrl Pts',(16.2389992540557,-18.3728253033474,
12.2624086339395));
#147760=CARTESIAN_POINT('Ctrl Pts',(16.2590848209399,-18.2922441216164,
12.2665196451063));
#147761=CARTESIAN_POINT('Ctrl Pts',(16.2830401055299,-18.2128142346481,
12.2706306562731));
#147762=CARTESIAN_POINT('Ctrl Pts',(16.3069915898917,-18.13339694831,12.2747410152756));
#147763=CARTESIAN_POINT('Ctrl Pts',(16.3348114354692,-18.0551310480635,
12.2788513742782));
#147764=CARTESIAN_POINT('Ctrl Pts',(16.3663553936721,-17.9784194855451,
12.2829617332808));
#147765=CARTESIAN_POINT('Ctrl Pts',(16.3994039228382,-17.8980489659369,
12.2872681465249));
#147766=CARTESIAN_POINT('Ctrl Pts',(16.4365404963283,-17.8193852938553,
12.2915745597691));
#147767=CARTESIAN_POINT('Ctrl Pts',(16.4775431085385,-17.74286713014,12.2958809730133));
#147768=CARTESIAN_POINT('Ctrl Pts',(16.5167281737212,-17.6697408322964,
12.2999964933322));
#147769=CARTESIAN_POINT('Ctrl Pts',(16.5594435017452,-17.5985742591835,
12.304112013651));
#147770=CARTESIAN_POINT('Ctrl Pts',(16.6054498638679,-17.5297221375653,
12.3082275339699));
#147771=CARTESIAN_POINT('Ctrl Pts',(16.6514869443888,-17.46082404346,12.3123458022172));
#147772=CARTESIAN_POINT('Ctrl Pts',(16.7008191449124,-17.394243852655,12.3164640704645));
#147773=CARTESIAN_POINT('Ctrl Pts',(16.7531665958489,-17.3303036582026,
12.3205823387118));
#147774=CARTESIAN_POINT('Ctrl Pts',(16.8055945346489,-17.2662651512335,
12.3247069390843));
#147775=CARTESIAN_POINT('Ctrl Pts',(16.8610466479906,-17.204875081261,12.3288315394568));
#147776=CARTESIAN_POINT('Ctrl Pts',(16.9192065009782,-17.1464184992341,
12.3329561398293));
#147777=CARTESIAN_POINT('Ctrl Pts',(16.9271149034353,-17.1384697484517,
12.3335169906232));
#147778=CARTESIAN_POINT('Ctrl Pts',(16.9350733229401,-17.1305751748483,
12.3340778414171));
#147779=CARTESIAN_POINT('Ctrl Pts',(16.9430809195059,-17.122735435449,12.334638692211));
#147780=CARTESIAN_POINT('Ctrl Pts',(17.0028274053095,-17.0642413698601,
12.338823326604));
#147781=CARTESIAN_POINT('Ctrl Pts',(17.0655538444184,-17.0085686402269,
12.3430079609971));
#147782=CARTESIAN_POINT('Ctrl Pts',(17.1309629349575,-16.9560360303603,
12.3471925953901));
#147783=CARTESIAN_POINT('Ctrl Pts',(17.1962789237522,-16.9035781941616,
12.3513712734741));
#147784=CARTESIAN_POINT('Ctrl Pts',(17.2642696237811,-16.8542518853561,
12.355549951558));
#147785=CARTESIAN_POINT('Ctrl Pts',(17.33460118292,-16.8083388908796,12.359728629642));
#147786=CARTESIAN_POINT('Ctrl Pts',(17.4061933847101,-16.7616029389743,
12.3639822075274));
#147787=CARTESIAN_POINT('Ctrl Pts',(17.4802108463248,-16.7184042096099,
12.3682357854128));
#147788=CARTESIAN_POINT('Ctrl Pts',(17.5562664269219,-16.6789967816027,
12.3724893632983));
#147789=CARTESIAN_POINT('Ctrl Pts',(17.6308475216787,-16.6403533434847,
12.3766604772762));
#147790=CARTESIAN_POINT('Ctrl Pts',(17.7073879875333,-16.6053557363939,
12.3808315912542));
#147791=CARTESIAN_POINT('Ctrl Pts',(17.7854953736987,-16.5741987101768,
12.3850027052321));
#147792=CARTESIAN_POINT('Ctrl Pts',(17.8635765501766,-16.5430521390006,
12.3891724195525));
#147793=CARTESIAN_POINT('Ctrl Pts',(17.9432231757915,-16.5157437595367,
12.3933421338729));
#147794=CARTESIAN_POINT('Ctrl Pts',(18.0240221782535,-16.4924204642606,
12.3975118481932));
#147795=CARTESIAN_POINT('Ctrl Pts',(18.1048183055401,-16.4690979989274,
12.4016814141373));
#147796=CARTESIAN_POINT('Ctrl Pts',(18.1867662859185,-16.4497604625989,
12.4058509800813));
#147797=CARTESIAN_POINT('Ctrl Pts',(18.2694385404883,-16.4345046871272,
12.4100205460254));
#147798=CARTESIAN_POINT('Ctrl Pts',(18.3550174495415,-16.4187125374101,
12.4143367087643));
#147799=CARTESIAN_POINT('Ctrl Pts',(18.4413719926989,-16.4072946141391,
12.4186528715032));
#147800=CARTESIAN_POINT('Ctrl Pts',(18.5280191484749,-16.400300196182,12.4229690342421));
#147801=CARTESIAN_POINT('Ctrl Pts',(18.6118437822652,-16.3935336206541,
12.4271445984338));
#147802=CARTESIAN_POINT('Ctrl Pts',(18.6959417854335,-16.3909067522804,
12.4313201626255));
#147803=CARTESIAN_POINT('Ctrl Pts',(18.7798750222016,-16.3924110716097,
12.4354957268172));
#147804=CARTESIAN_POINT('Ctrl Pts',(18.8680475272266,-16.3939913705322,
12.4398821888297));
#147805=CARTESIAN_POINT('Ctrl Pts',(18.9560376012526,-16.4001311167978,
12.4442686508422));
#147806=CARTESIAN_POINT('Ctrl Pts',(19.0433447687656,-16.4107590011891,
12.4486551128548));
#147807=CARTESIAN_POINT('Ctrl Pts',(19.1306519362786,-16.4213868855804,
12.4530415748673));
#147808=CARTESIAN_POINT('Ctrl Pts',(19.2172756387743,-16.4365027334242,
12.4574280368799));
#147809=CARTESIAN_POINT('Ctrl Pts',(19.3027314805895,-16.4559742583486,
12.4618144988924));
#147810=CARTESIAN_POINT('Ctrl Pts',(19.3842553724469,-16.4745498695475,
12.4659991332855));
#147811=CARTESIAN_POINT('Ctrl Pts',(19.4650199594566,-16.4971582855303,
12.4701837676785));
#147812=CARTESIAN_POINT('Ctrl Pts',(19.5445962710158,-16.5237220740996,
12.4743684020716));
#147813=CARTESIAN_POINT('Ctrl Pts',(19.6240593155451,-16.5502480524038,
12.4785470801555));
#147814=CARTESIAN_POINT('Ctrl Pts',(19.702337011573,-16.5807180759575,12.4827257582394));
#147815=CARTESIAN_POINT('Ctrl Pts',(19.7790117130572,-16.6150039538815,
12.4869044363234));
#147816=CARTESIAN_POINT('Ctrl Pts',(19.8570607534603,-16.6499043815265,
12.4911580142088));
#147817=CARTESIAN_POINT('Ctrl Pts',(19.9334482966285,-16.6887587003509,
12.4954115920943));
#147818=CARTESIAN_POINT('Ctrl Pts',(20.0077511504909,-16.7313789142172,
12.4996651699797));
#147819=CARTESIAN_POINT('Ctrl Pts',(20.0806134985411,-16.7731728520712,
12.5038362839577));
#147820=CARTESIAN_POINT('Ctrl Pts',(20.1514708500755,-16.8185877301275,
12.5080073979356));
#147821=CARTESIAN_POINT('Ctrl Pts',(20.2199470251256,-16.8673989737793,
12.5121785119136));
#147822=CARTESIAN_POINT('Ctrl Pts',(20.2884002223337,-16.9161938383468,
12.5163482262339));
#147823=CARTESIAN_POINT('Ctrl Pts',(20.3544734556457,-16.9683825382778,
12.5205179405543));
#147824=CARTESIAN_POINT('Ctrl Pts',(20.4178196235398,-17.0236972552572,
12.5246876548747));
#147825=CARTESIAN_POINT('Ctrl Pts',(20.4811635373054,-17.0790100039017,
12.5288572208188));
#147826=CARTESIAN_POINT('Ctrl Pts',(20.5417802326388,-17.1374482452018,
12.5330267867628));
#147827=CARTESIAN_POINT('Ctrl Pts',(20.5993568489269,-17.198704866213,12.5371963527068));
#147828=CARTESIAN_POINT('Ctrl Pts',(20.6589577880153,-17.2621151944506,
12.5415125154458));
#147829=CARTESIAN_POINT('Ctrl Pts',(20.7153005309283,-17.3285453940347,
12.5458286781847));
#147830=CARTESIAN_POINT('Ctrl Pts',(20.7680821915678,-17.3976159940521,
12.5501448409236));
#147831=CARTESIAN_POINT('Ctrl Pts',(20.8191444951638,-17.464436626539,12.5543204051153));
#147832=CARTESIAN_POINT('Ctrl Pts',(20.8668739298254,-17.5337278643778,
12.558495969307));
#147833=CARTESIAN_POINT('Ctrl Pts',(20.9110405044759,-17.6051166932985,
12.5626715334987));
#147834=CARTESIAN_POINT('Ctrl Pts',(20.957437827816,-17.680111202257,12.5670579955112));
#147835=CARTESIAN_POINT('Ctrl Pts',(20.999902631049,-17.7574202579858,12.5714444575237));
#147836=CARTESIAN_POINT('Ctrl Pts',(21.0382239760384,-17.8365844414525,
12.5758309195363));
#147837=CARTESIAN_POINT('Ctrl Pts',(21.0765453210278,-17.9157486249193,
12.5802173815488));
#147838=CARTESIAN_POINT('Ctrl Pts',(21.1107230523385,-17.9967673719632,
12.5846038435614));
#147839=CARTESIAN_POINT('Ctrl Pts',(21.1406062076889,-18.0791617783844,
12.5889903055739));
#147840=CARTESIAN_POINT('Ctrl Pts',(21.1691143947643,-18.1577650960285,
12.5931749399669));
#147841=CARTESIAN_POINT('Ctrl Pts',(21.193820633909,-18.2379128391996,12.59735957436));
#147842=CARTESIAN_POINT('Ctrl Pts',(21.2145578396958,-18.3192023989271,
12.601544208753));
#147843=CARTESIAN_POINT('Ctrl Pts',(21.2352655286369,-18.4003762530279,
12.605722886837));
#147844=CARTESIAN_POINT('Ctrl Pts',(21.25201529302,-18.4826882535134,12.6099015649209));
#147845=CARTESIAN_POINT('Ctrl Pts',(21.2646888572063,-18.5657178388641,
12.6140802430049));
#147846=CARTESIAN_POINT('Ctrl Pts',(21.2775895859224,-18.65023566986,12.6183338208903));
#147847=CARTESIAN_POINT('Ctrl Pts',(21.2862663809329,-18.7354966109228,
12.6225873987757));
#147848=CARTESIAN_POINT('Ctrl Pts',(21.2906482513971,-18.8210430657491,
12.6268409766612));
#147849=CARTESIAN_POINT('Ctrl Pts',(21.2949451707518,-18.9049310356184,
12.6310120906391));
#147850=CARTESIAN_POINT('Ctrl Pts',(21.2951121858363,-18.9890930669704,
12.6351832046171));
#147851=CARTESIAN_POINT('Ctrl Pts',(21.2911345092731,-19.0730912940082,
12.639354318595));
#147852=CARTESIAN_POINT('Ctrl Pts',(21.2871581674577,-19.1570613346296,
12.6435240329154));
#147853=CARTESIAN_POINT('Ctrl Pts',(21.2790399178703,-19.2408672209647,
12.6476937472358));
#147854=CARTESIAN_POINT('Ctrl Pts',(21.2668170738604,-19.3240721305896,
12.6518634615562));
#147855=CARTESIAN_POINT('Ctrl Pts',(21.2545946647916,-19.4072740794267,
12.6560330275002));
#147856=CARTESIAN_POINT('Ctrl Pts',(21.2382680194079,-19.4898746390487,
12.6602025934442));
#147857=CARTESIAN_POINT('Ctrl Pts',(21.2179260255778,-19.5714445087795,
12.6643721593883));
#147858=CARTESIAN_POINT('Ctrl Pts',(21.1968688323393,-19.6558822745029,
12.6686883221272));
#147859=CARTESIAN_POINT('Ctrl Pts',(21.1715088054102,-19.7392150119469,
12.6730044848661));
#147860=CARTESIAN_POINT('Ctrl Pts',(21.1420010732758,-19.8209826414278,
12.6773206476051));
#147861=CARTESIAN_POINT('Ctrl Pts',(21.113454552412,-19.9000866989788,12.6814962117967));
#147862=CARTESIAN_POINT('Ctrl Pts',(21.0810266246877,-19.9777256330122,
12.6856717759884));
#147863=CARTESIAN_POINT('Ctrl Pts',(21.0449064462655,-20.0535041518799,
12.6898473401801));
#147864=CARTESIAN_POINT('Ctrl Pts',(21.0069619234988,-20.1331100635892,
12.6942338021926));
#147865=CARTESIAN_POINT('Ctrl Pts',(20.9649426346355,-20.2106621684913,
12.6986202642052));
#147866=CARTESIAN_POINT('Ctrl Pts',(20.9191207015645,-20.2857344261862,
12.7030067262177));
#147867=CARTESIAN_POINT('Ctrl Pts',(20.8732987684935,-20.3608066838811,
12.7073931882303));
#147868=CARTESIAN_POINT('Ctrl Pts',(20.8236745814507,-20.433398658303,12.7117796502428));
#147869=CARTESIAN_POINT('Ctrl Pts',(20.7705691100602,-20.5031241923033,
12.7161661122553));
#147870=CARTESIAN_POINT('Ctrl Pts',(20.7199091712282,-20.5696388318498,
12.7203505755776));
#147871=CARTESIAN_POINT('Ctrl Pts',(20.6658929673645,-20.6337927963153,
12.7245350388999));
#147872=CARTESIAN_POINT('Ctrl Pts',(20.6087685573973,-20.6952277120889,
12.7287195022221));
#147873=CARTESIAN_POINT('Ctrl Pts',(20.5517322346214,-20.7565678937692,
12.7328975130029));
#147874=CARTESIAN_POINT('Ctrl Pts',(20.4915975412145,-20.815197025317,12.7370755237838));
#147875=CARTESIAN_POINT('Ctrl Pts',(20.4286539389059,-20.8707881663567,
12.7412535345646));
#147876=CARTESIAN_POINT('Ctrl Pts',(20.3849328735721,-20.9094021607936,
12.7441556100038));
#147877=CARTESIAN_POINT('Ctrl Pts',(20.3398574638174,-20.9465510096566,
12.747057685443));
#147878=CARTESIAN_POINT('Ctrl Pts',(20.2935357468249,-20.9821350335323,
12.7499597608822));
#147879=CARTESIAN_POINT('Ctrl Pts',(20.2935357468249,-20.9821350335323,
11.9498687307687));
#147880=CARTESIAN_POINT('Ctrl Pts',(20.2763932990299,-20.9953037438313,
11.9509495779013));
#147881=CARTESIAN_POINT('Ctrl Pts',(20.2590918338935,-21.0082493295476,
11.952030425034));
#147882=CARTESIAN_POINT('Ctrl Pts',(20.2416377781119,-21.0209679383717,
11.9531112721667));
#147883=CARTESIAN_POINT('Ctrl Pts',(20.1740622256448,-21.0702096177069,
11.9572959065597));
#147884=CARTESIAN_POINT('Ctrl Pts',(20.1039459219093,-21.1162287760929,
11.9614805409527));
#147885=CARTESIAN_POINT('Ctrl Pts',(20.0316291334116,-21.1587529612808,
11.9656651753458));
#147886=CARTESIAN_POINT('Ctrl Pts',(19.9594152789112,-21.2012166185545,
11.9698438534297));
#147887=CARTESIAN_POINT('Ctrl Pts',(19.8850075541825,-21.2401949526838,
11.9740225315137));
#147888=CARTESIAN_POINT('Ctrl Pts',(19.8087770431608,-21.2754574038476,
11.9782012095976));
#147889=CARTESIAN_POINT('Ctrl Pts',(19.731180155015,-21.311351909106,11.9824547874831));
#147890=CARTESIAN_POINT('Ctrl Pts',(19.6516948805992,-21.343395722762,11.9867083653685));
#147891=CARTESIAN_POINT('Ctrl Pts',(19.5707410268107,-21.3713934062181,
11.9909619432539));
#147892=CARTESIAN_POINT('Ctrl Pts',(19.4913566214465,-21.3988482999475,
11.9951330572319));
#147893=CARTESIAN_POINT('Ctrl Pts',(19.4105605259062,-21.4224123904405,
11.9993041712098));
#147894=CARTESIAN_POINT('Ctrl Pts',(19.3287692237674,-21.4419497124358,
12.0034752851878));
#147895=CARTESIAN_POINT('Ctrl Pts',(19.24700536749,-21.461480478494,12.0076449995082));
#147896=CARTESIAN_POINT('Ctrl Pts',(19.1642474149188,-21.4769870528098,
12.0118147138285));
#147897=CARTESIAN_POINT('Ctrl Pts',(19.0809253355101,-21.4883838060477,
12.0159844281489));
#147898=CARTESIAN_POINT('Ctrl Pts',(18.9976062210584,-21.4997801537403,
12.0201539940929));
#147899=CARTESIAN_POINT('Ctrl Pts',(18.9137234755861,-21.5070669096296,
12.024323560037));
#147900=CARTESIAN_POINT('Ctrl Pts',(18.8297141852437,-21.5102100763509,
12.028493125981));
#147901=CARTESIAN_POINT('Ctrl Pts',(18.7427512318893,-21.5134637529366,
12.0328092887199));
#147902=CARTESIAN_POINT('Ctrl Pts',(18.6556531965172,-21.5122770220956,
12.0371254514589));
#147903=CARTESIAN_POINT('Ctrl Pts',(18.5689051504098,-21.5066709554537,
12.0414416141978));
#147904=CARTESIAN_POINT('Ctrl Pts',(18.4849829127801,-21.501247505843,12.0456171783895));
#147905=CARTESIAN_POINT('Ctrl Pts',(18.4013886754049,-21.4916883190585,
12.0497927425811));
#147906=CARTESIAN_POINT('Ctrl Pts',(18.3185547392504,-21.4780651684627,
12.0539683067728));
#147907=CARTESIAN_POINT('Ctrl Pts',(18.2315370578995,-21.4637539449163,
12.0583547687854));
#147908=CARTESIAN_POINT('Ctrl Pts',(18.1453590723583,-21.444957551129,12.0627412307979));
#147909=CARTESIAN_POINT('Ctrl Pts',(18.0605056905582,-21.4218189033104,
12.0671276928105));
#147910=CARTESIAN_POINT('Ctrl Pts',(17.975652308758,-21.3986802554919,12.071514154823));
#147911=CARTESIAN_POINT('Ctrl Pts',(17.8921240580818,-21.371199607226,12.0759006168356));
#147912=CARTESIAN_POINT('Ctrl Pts',(17.8103811197836,-21.3395778865008,
12.0802870788481));
#147913=CARTESIAN_POINT('Ctrl Pts',(17.7323992952486,-21.3094111280208,
12.0844717132412));
#147914=CARTESIAN_POINT('Ctrl Pts',(17.6557518403844,-21.2753637103368,
12.0886563476342));
#147915=CARTESIAN_POINT('Ctrl Pts',(17.5808520242221,-21.2375742704973,
12.0928409820273));
#147916=CARTESIAN_POINT('Ctrl Pts',(17.5060588186775,-21.1998386192481,
12.0970196601112));
#147917=CARTESIAN_POINT('Ctrl Pts',(17.4330087179883,-21.1583717310105,
12.1011983381951));
#147918=CARTESIAN_POINT('Ctrl Pts',(17.3620964471735,-21.113360830991,12.1053770162791));
#147919=CARTESIAN_POINT('Ctrl Pts',(17.289913124868,-21.0675431429373,12.1096305941645));
#147920=CARTESIAN_POINT('Ctrl Pts',(17.2199454771429,-21.018053314544,12.11388417205));
#147921=CARTESIAN_POINT('Ctrl Pts',(17.1525850704414,-20.9651385497698,
12.1181377499354));
#147922=CARTESIAN_POINT('Ctrl Pts',(17.0865305766668,-20.9132496409654,
12.1223088639133));
#147923=CARTESIAN_POINT('Ctrl Pts',(17.0229835115634,-20.8580677061308,
12.1264799778913));
#147924=CARTESIAN_POINT('Ctrl Pts',(16.9622836350606,-20.7998693466276,
12.1306510918693));
#147925=CARTESIAN_POINT('Ctrl Pts',(16.9016041269875,-20.741690516146,12.1348208061896));
#147926=CARTESIAN_POINT('Ctrl Pts',(16.8437702418585,-20.6804975893352,
12.13899052051));
#147927=CARTESIAN_POINT('Ctrl Pts',(16.7890867147049,-20.6166057529284,
12.1431602348304));
#147928=CARTESIAN_POINT('Ctrl Pts',(16.7344051334259,-20.5527161900675,
12.1473298007744));
#147929=CARTESIAN_POINT('Ctrl Pts',(16.682873985715,-20.4861282586161,12.1514993667185));
#147930=CARTESIAN_POINT('Ctrl Pts',(16.6347584444192,-20.4171910767278,
12.1556689326625));
#147931=CARTESIAN_POINT('Ctrl Pts',(16.5849512200484,-20.3458301485675,
12.1599850954014));
#147932=CARTESIAN_POINT('Ctrl Pts',(16.5388045582795,-20.2719521294865,
12.1643012581404));
#147933=CARTESIAN_POINT('Ctrl Pts',(16.496563301095,-20.1959762933404,12.1686174208793));
#147934=CARTESIAN_POINT('Ctrl Pts',(16.4556980484202,-20.1224753620654,
12.172792985071));
#147935=CARTESIAN_POINT('Ctrl Pts',(16.4184878365308,-20.0470116310055,
12.1769685492626));
#147936=CARTESIAN_POINT('Ctrl Pts',(16.3851063117009,-19.9699874464201,
12.1811441134543));
#147937=CARTESIAN_POINT('Ctrl Pts',(16.350038765409,-19.8890729533789,12.1855305754669));
#147938=CARTESIAN_POINT('Ctrl Pts',(16.3191970489118,-19.8064367740456,
12.1899170374794));
#147939=CARTESIAN_POINT('Ctrl Pts',(16.2927234637601,-19.7225639970856,
12.1943034994919));
#147940=CARTESIAN_POINT('Ctrl Pts',(16.2662498786084,-19.6386912201256,
12.1986899615045));
#147941=CARTESIAN_POINT('Ctrl Pts',(16.2441444970407,-19.5535824262448,
12.203076423517));
#147942=CARTESIAN_POINT('Ctrl Pts',(16.2264874578015,-19.4677333135615,
12.2074628855296));
#147943=CARTESIAN_POINT('Ctrl Pts',(16.2025156137684,-19.3511814097151,
12.2134181072288));
#147944=CARTESIAN_POINT('Ctrl Pts',(16.1866633864905,-19.2329068373031,
12.219373328928));
#147945=CARTESIAN_POINT('Ctrl Pts',(16.1791211349008,-19.1138455580776,
12.2253285506272));
#147946=CARTESIAN_POINT('Ctrl Pts',(16.1757600463668,-19.060787728371,12.2279824036753));
#147947=CARTESIAN_POINT('Ctrl Pts',(16.1740486686438,-19.0075739736056,
12.2306362567234));
#147948=CARTESIAN_POINT('Ctrl Pts',(16.174001023388,-18.9542890490546,12.2332901097715));
#147949=CARTESIAN_POINT('',(16.1740007840082,-18.949996472737,12.1667098902285));
#147950=CARTESIAN_POINT('Ctrl Pts',(20.2935357468249,-20.9821350335323,
11.8833305117342));
#147951=CARTESIAN_POINT('Ctrl Pts',(20.2268566585352,-21.0333574497933,
11.8875000047157));
#147952=CARTESIAN_POINT('Ctrl Pts',(20.1576368543504,-21.0813024786675,
11.8916694976972));
#147953=CARTESIAN_POINT('Ctrl Pts',(20.0862362138371,-21.1257196741962,
11.8958389906787));
#147954=CARTESIAN_POINT('Ctrl Pts',(20.0148284980351,-21.1701412711487,
11.9000088968269));
#147955=CARTESIAN_POINT('Ctrl Pts',(19.9412399081108,-21.2110340987355,
11.9041788029752));
#147956=CARTESIAN_POINT('Ctrl Pts',(19.8658573753418,-21.2481922571693,
11.9083487091234));
#147957=CARTESIAN_POINT('Ctrl Pts',(19.7903949052723,-21.285389818934,11.912523037132));
#147958=CARTESIAN_POINT('Ctrl Pts',(19.7131351076393,-21.3188446006788,
11.9166973651407));
#147959=CARTESIAN_POINT('Ctrl Pts',(19.6344870159503,-21.3483979498625,
11.9208716931493));
#147960=CARTESIAN_POINT('Ctrl Pts',(19.5557947538892,-21.3779678968097,
11.9250483655457));
#147961=CARTESIAN_POINT('Ctrl Pts',(19.4757130835543,-21.4036319081676,
11.9292250379421));
#147962=CARTESIAN_POINT('Ctrl Pts',(19.3946660856504,-21.4252812867265,
11.9334017103385));
#147963=CARTESIAN_POINT('Ctrl Pts',(19.3134800547385,-21.4469678039617,
11.9375855476558));
#147964=CARTESIAN_POINT('Ctrl Pts',(19.2313258391223,-21.4646258381512,
11.9417693849731));
#147965=CARTESIAN_POINT('Ctrl Pts',(19.1486373175954,-21.478197912844,11.9459532222903));
#147966=CARTESIAN_POINT('Ctrl Pts',(19.0921615639953,-21.4874675567079,
11.9488107575452));
#147967=CARTESIAN_POINT('Ctrl Pts',(19.0354367233637,-21.4948322630722,
11.9516682928));
#147968=CARTESIAN_POINT('Ctrl Pts',(18.9786013944249,-21.5002876913421,
11.9545258280548));
#147969=CARTESIAN_POINT('Ctrl Pts',(18.8953705500055,-21.5082767346017,
11.9587104624479));
#147970=CARTESIAN_POINT('Ctrl Pts',(18.8115930039276,-21.5121986934545,
11.9628950968409));
#147971=CARTESIAN_POINT('Ctrl Pts',(18.7277003248363,-21.5119922488345,
11.967079731234));
#147972=CARTESIAN_POINT('Ctrl Pts',(18.6439270565898,-21.5117860980629,
11.9712584093179));
#147973=CARTESIAN_POINT('Ctrl Pts',(18.560039436939,-21.507463217065,11.9754370874018));
#147974=CARTESIAN_POINT('Ctrl Pts',(18.4764742375282,-21.4990140324826,
11.9796157654858));
#147975=CARTESIAN_POINT('Ctrl Pts',(18.391411191975,-21.4904134023389,11.9838693433712));
#147976=CARTESIAN_POINT('Ctrl Pts',(18.3066827190521,-21.4775370395473,
11.9881229212567));
#147977=CARTESIAN_POINT('Ctrl Pts',(18.2227496524054,-21.460430402081,11.9923764991421));
#147978=CARTESIAN_POINT('Ctrl Pts',(18.1404437920376,-21.4436554101629,
11.99654761312));
#147979=CARTESIAN_POINT('Ctrl Pts',(18.0589032436853,-21.4228128002076,
12.000718727098));
#147980=CARTESIAN_POINT('Ctrl Pts',(17.9785557081133,-21.3979975310404,
12.004889841076));
#147981=CARTESIAN_POINT('Ctrl Pts',(17.898235133933,-21.3731905888765,12.0090595553963));
#147982=CARTESIAN_POINT('Ctrl Pts',(17.819107216658,-21.3444137706279,12.0132292697167));
#147983=CARTESIAN_POINT('Ctrl Pts',(17.7415856439041,-21.3118122268127,
12.0173989840371));
#147984=CARTESIAN_POINT('Ctrl Pts',(17.6640668297004,-21.2792118431003,
12.0215685499811));
#147985=CARTESIAN_POINT('Ctrl Pts',(17.5881546700965,-21.2427871835461,
12.0257381159252));
#147986=CARTESIAN_POINT('Ctrl Pts',(17.5142426975068,-21.2027314639944,
12.0299076818692));
#147987=CARTESIAN_POINT('Ctrl Pts',(17.4377320711412,-21.1612674347574,
12.0342238446081));
#147988=CARTESIAN_POINT('Ctrl Pts',(17.3633653656329,-21.1159125099135,
12.0385400073471));
#147989=CARTESIAN_POINT('Ctrl Pts',(17.2915493867665,-21.0669317313763,
12.042856170086));
#147990=CARTESIAN_POINT('Ctrl Pts',(17.222072805858,-21.0195464965481,12.0470317342777));
#147991=CARTESIAN_POINT('Ctrl Pts',(17.1549836708369,-20.968768326667,12.0512072984694));
#147992=CARTESIAN_POINT('Ctrl Pts',(17.0906175572636,-20.914879045409,12.055382862661));
#147993=CARTESIAN_POINT('Ctrl Pts',(17.0230004643097,-20.8582679446643,
12.0597693246736));
#147994=CARTESIAN_POINT('Ctrl Pts',(16.9583891293619,-20.7982235859986,
12.0641557866861));
#147995=CARTESIAN_POINT('Ctrl Pts',(16.8971281979621,-20.735115807478,12.0685422486987));
#147996=CARTESIAN_POINT('Ctrl Pts',(16.8358672665623,-20.6720080289574,
12.0729287107112));
#147997=CARTESIAN_POINT('Ctrl Pts',(16.7779570635865,-20.6058373172987,
12.0773151727238));
#147998=CARTESIAN_POINT('Ctrl Pts',(16.7236914224212,-20.5370108589259,
12.0817016347363));
#147999=CARTESIAN_POINT('Ctrl Pts',(16.6719732357611,-20.4714154002739,
12.0858821780095));
#148000=CARTESIAN_POINT('Ctrl Pts',(16.62336875941,-20.403158891998,12.0900627212828));
#148001=CARTESIAN_POINT('Ctrl Pts',(16.5781640651477,-20.3325692383938,
12.094243264556));
#148002=CARTESIAN_POINT('Ctrl Pts',(16.5330221281564,-20.2620775837719,
12.0984180040186));
#148003=CARTESIAN_POINT('Ctrl Pts',(16.4912708487477,-20.1892595981085,
12.1025927434812));
#148004=CARTESIAN_POINT('Ctrl Pts',(16.4531558825332,-20.1144758542942,
12.1067674829437));
#148005=CARTESIAN_POINT('Ctrl Pts',(16.4150823671081,-20.0397734392997,
12.1109376822935));
#148006=CARTESIAN_POINT('Ctrl Pts',(16.380637519025,-19.9631099194743,12.1151078816432));
#148007=CARTESIAN_POINT('Ctrl Pts',(16.3500227648594,-19.8848732723855,
12.119278080993));
#148008=CARTESIAN_POINT('Ctrl Pts',(16.319430601241,-19.8066943559144,12.1234452031635));
#148009=CARTESIAN_POINT('Ctrl Pts',(16.2926630858425,-19.7269450449961,
12.1276123253341));
#148010=CARTESIAN_POINT('Ctrl Pts',(16.2698743296479,-19.6460350716728,
12.1317794475046));
#148011=CARTESIAN_POINT('Ctrl Pts',(16.2470959536797,-19.5651619526576,
12.1359446715605));
#148012=CARTESIAN_POINT('Ctrl Pts',(16.2282928589745,-19.4831296648129,
12.1401098956164));
#148013=CARTESIAN_POINT('Ctrl Pts',(16.2135694674,-19.4003636139762,12.1442751196724));
#148014=CARTESIAN_POINT('Ctrl Pts',(16.1988435352848,-19.3175832817472,
12.1484410624432));
#148015=CARTESIAN_POINT('Ctrl Pts',(16.1881988016354,-19.2340693856754,
12.1526070052141));
#148016=CARTESIAN_POINT('Ctrl Pts',(16.1816884763611,-19.1502571216887,
12.156772947985));
#148017=CARTESIAN_POINT('Ctrl Pts',(16.1765121589547,-19.0836185341113,
12.1600852620661));
#148018=CARTESIAN_POINT('Ctrl Pts',(16.1739485082683,-19.0167915973248,
12.1633975761473));
#148019=CARTESIAN_POINT('Ctrl Pts',(16.1740007840082,-18.949996472737,12.1667098902285));
#148020=CARTESIAN_POINT('Ctrl Pts',(16.1763510013672,-18.9499800105097,
12.1667107986216));
#148021=CARTESIAN_POINT('Ctrl Pts',(16.1742902547169,-18.6667985525942,
12.1807663462203));
#148022=CARTESIAN_POINT('Ctrl Pts',(16.3483939296849,-17.5319993745477,
12.2372138293795));
#148023=CARTESIAN_POINT('Ctrl Pts',(18.012168501089,-16.0122294088113,12.3360532480991));
#148024=CARTESIAN_POINT('Ctrl Pts',(20.815168138664,-16.7538118778759,12.4632290547806));
#148025=CARTESIAN_POINT('Ctrl Pts',(21.6282770393392,-19.2634826679177,
12.5789421029395));
#148026=CARTESIAN_POINT('Ctrl Pts',(20.782749793487,-20.5975255724166,12.652263215538));
#148027=CARTESIAN_POINT('Ctrl Pts',(20.2929505273095,-20.9813917755491,
12.683192392576));
#148028=CARTESIAN_POINT('Origin',(18.734,-18.952,-1.76670989022851));
#148029=CARTESIAN_POINT('',(20.2935357468249,-20.9821350335323,13.5498657043958));
#148030=CARTESIAN_POINT('',(20.2935357468249,-20.9821350335323,13.4833228568185));
#148031=CARTESIAN_POINT('',(20.2935357468249,-20.9821350335323,-1.76670989022851));
#148032=CARTESIAN_POINT('',(16.174000001606,-18.9520906788002,13.0332901097364));
#148033=CARTESIAN_POINT('Ctrl Pts',(16.174000001606,-18.9520906780897,13.0332901097715));
#148034=CARTESIAN_POINT('Ctrl Pts',(16.1739968821085,-18.8640218456489,
13.0376462156856));
#148035=CARTESIAN_POINT('Ctrl Pts',(16.1785426714359,-18.776035607655,13.0420023215996));
#148036=CARTESIAN_POINT('Ctrl Pts',(16.1875860737584,-18.6886065372053,
13.0463584275137));
#148037=CARTESIAN_POINT('Ctrl Pts',(16.1966529338892,-18.6009506832622,
13.050725832792));
#148038=CARTESIAN_POINT('Ctrl Pts',(16.2102406836425,-18.5138552818865,
13.0550932380704));
#148039=CARTESIAN_POINT('Ctrl Pts',(16.2282463851318,-18.4277874271108,
13.0594606433487));
#148040=CARTESIAN_POINT('Ctrl Pts',(16.2462755658188,-18.3416073409855,
13.0638337436661));
#148041=CARTESIAN_POINT('Ctrl Pts',(16.2687340840993,-18.2564578570398,
13.0682068439834));
#148042=CARTESIAN_POINT('Ctrl Pts',(16.2954690366781,-18.1727909517206,
13.0725799443007));
#148043=CARTESIAN_POINT('Ctrl Pts',(16.3222767415772,-18.0888963683653,
13.0769649448896));
#148044=CARTESIAN_POINT('Ctrl Pts',(16.3533840099471,-18.0064928038111,
13.0813499454785));
#148045=CARTESIAN_POINT('Ctrl Pts',(16.3885892814888,-17.9260133716794,
13.0857349460673));
#148046=CARTESIAN_POINT('Ctrl Pts',(16.4205927188907,-17.8528533488879,
13.0897211414781));
#148047=CARTESIAN_POINT('Ctrl Pts',(16.4559819492917,-17.7812832866316,
13.0937073368888));
#148048=CARTESIAN_POINT('Ctrl Pts',(16.4945737975983,-17.7116088181558,
13.0976935322996));
#148049=CARTESIAN_POINT('Ctrl Pts',(16.5350868078939,-17.638465846711,13.1018781666926));
#148050=CARTESIAN_POINT('Ctrl Pts',(16.5792624158945,-17.5671736686978,
13.1060628010856));
#148051=CARTESIAN_POINT('Ctrl Pts',(16.6269069559,-17.4981228031552,13.1102474354787));
#148052=CARTESIAN_POINT('Ctrl Pts',(16.6744836797999,-17.4291702229729,
13.1144261135626));
#148053=CARTESIAN_POINT('Ctrl Pts',(16.7255192690589,-17.3624529938655,
13.1186047916466));
#148054=CARTESIAN_POINT('Ctrl Pts',(16.779774450421,-17.2983366420662,13.1227834697305));
#148055=CARTESIAN_POINT('Ctrl Pts',(16.8350021169166,-17.2330710507404,
13.1270370476159));
#148056=CARTESIAN_POINT('Ctrl Pts',(16.8935656995715,-17.1705009170566,
13.1312906255014));
#148057=CARTESIAN_POINT('Ctrl Pts',(16.9551669364595,-17.110980463967,13.1355442033868));
#148058=CARTESIAN_POINT('Ctrl Pts',(17.0155739131654,-17.0526139310053,
13.1397153173648));
#148059=CARTESIAN_POINT('Ctrl Pts',(17.0789014673906,-16.9971802202222,
13.1438864313427));
#148060=CARTESIAN_POINT('Ctrl Pts',(17.1448292745175,-16.9449782250136,
13.1480575453207));
#148061=CARTESIAN_POINT('Ctrl Pts',(17.210734958932,-16.8927937466887,13.152227259641));
#148062=CARTESIAN_POINT('Ctrl Pts',(17.2792388030076,-16.8438391155733,
13.1563969739614));
#148063=CARTESIAN_POINT('Ctrl Pts',(17.3499870301182,-16.7983732683682,
13.1605666882818));
#148064=CARTESIAN_POINT('Ctrl Pts',(17.4207327397034,-16.752909039033,13.1647362542258));
#148065=CARTESIAN_POINT('Ctrl Pts',(17.4937222860637,-16.7109335947648,
13.1689058201699));
#148066=CARTESIAN_POINT('Ctrl Pts',(17.5685736694551,-16.6726620548781,
13.1730753861139));
#148067=CARTESIAN_POINT('Ctrl Pts',(17.6460567351474,-16.633044934862,13.1773915488529));
#148068=CARTESIAN_POINT('Ctrl Pts',(17.7255345286223,-16.5973972639688,
13.1817077115918));
#148069=CARTESIAN_POINT('Ctrl Pts',(17.8065583197872,-16.5659044592045,
13.1860238743307));
#148070=CARTESIAN_POINT('Ctrl Pts',(17.884942769477,-16.535437529243,13.1901994385224));
#148071=CARTESIAN_POINT('Ctrl Pts',(17.9647735800335,-16.508859036806,13.1943750027141));
#148072=CARTESIAN_POINT('Ctrl Pts',(18.0456284938941,-16.4862861744352,
13.1985505669057));
#148073=CARTESIAN_POINT('Ctrl Pts',(18.1305671972396,-16.4625732104479,
13.2029370289183));
#148074=CARTESIAN_POINT('Ctrl Pts',(18.2166356079045,-16.4432812873466,
13.2073234909308));
#148075=CARTESIAN_POINT('Ctrl Pts',(18.3033337697291,-16.4284852688949,
13.2117099529434));
#148076=CARTESIAN_POINT('Ctrl Pts',(18.3900319315537,-16.4136892504433,
13.2160964149559));
#148077=CARTESIAN_POINT('Ctrl Pts',(18.4773592594053,-16.4033891290646,
13.2204828769685));
#148078=CARTESIAN_POINT('Ctrl Pts',(18.5648137584887,-16.3975967398073,
13.224869338981));
#148079=CARTESIAN_POINT('Ctrl Pts',(18.6482443464305,-16.3920708669661,
13.2290539733741));
#148080=CARTESIAN_POINT('Ctrl Pts',(18.7321012046619,-16.3906264585577,
13.2332386077671));
#148081=CARTESIAN_POINT('Ctrl Pts',(18.8159511409017,-16.3933120529254,
13.2374232421602));
#148082=CARTESIAN_POINT('Ctrl Pts',(18.8996817271358,-16.3959938246819,
13.2416019202441));
#148083=CARTESIAN_POINT('Ctrl Pts',(18.9834049550842,-16.4027939079682,
13.245780598328));
#148084=CARTESIAN_POINT('Ctrl Pts',(19.0666839609553,-16.413708964259,13.249959276412));
#148085=CARTESIAN_POINT('Ctrl Pts',(19.151455683155,-16.4248196650893,13.2542128542974));
#148086=CARTESIAN_POINT('Ctrl Pts',(19.2357666201897,-16.4401943435876,
13.2584664321829));
#148087=CARTESIAN_POINT('Ctrl Pts',(19.3191574830896,-16.4597739428406,
13.2627200100683));
#148088=CARTESIAN_POINT('Ctrl Pts',(19.4009316513885,-16.4789739533557,
13.2668911240463));
#148089=CARTESIAN_POINT('Ctrl Pts',(19.4818206335823,-16.502217188393,13.2710622380242));
#148090=CARTESIAN_POINT('Ctrl Pts',(19.561399721986,-16.5293960909679,13.2752333520022));
#148091=CARTESIAN_POINT('Ctrl Pts',(19.6409521068579,-16.5565658733995,
13.2794030663226));
#148092=CARTESIAN_POINT('Ctrl Pts',(19.7191950359075,-16.5876685519741,
13.2835727806429));
#148093=CARTESIAN_POINT('Ctrl Pts',(19.7957192917694,-16.6225468140603,
13.2877424949633));
#148094=CARTESIAN_POINT('Ctrl Pts',(19.8722408245699,-16.6574238350283,
13.2919120609074));
#148095=CARTESIAN_POINT('Ctrl Pts',(19.9470433875299,-16.6960759808161,
13.2960816268514));
#148096=CARTESIAN_POINT('Ctrl Pts',(20.019739330133,-16.7382984900965,13.3002511927954));
#148097=CARTESIAN_POINT('Ctrl Pts',(20.0949911723979,-16.7820054907161,
13.3045673555344));
#148098=CARTESIAN_POINT('Ctrl Pts',(20.1679850444452,-16.8295383292521,
13.3088835182733));
#148099=CARTESIAN_POINT('Ctrl Pts',(20.2383221508273,-16.8806200574181,
13.3131996810122));
#148100=CARTESIAN_POINT('Ctrl Pts',(20.3063680333671,-16.9300378036621,
13.3173752452039));
#148101=CARTESIAN_POINT('Ctrl Pts',(20.3719272430123,-16.9827764479853,
13.3215508093956));
#148102=CARTESIAN_POINT('Ctrl Pts',(20.4346726793713,-17.0385443727015,
13.3257263735873));
#148103=CARTESIAN_POINT('Ctrl Pts',(20.5005872385575,-17.0971290027194,
13.3301128355998));
#148104=CARTESIAN_POINT('Ctrl Pts',(20.5633958911489,-17.1590565633927,
13.3344992976123));
#148105=CARTESIAN_POINT('Ctrl Pts',(20.6227650717809,-17.2239471930463,
13.3388857596249));
#148106=CARTESIAN_POINT('Ctrl Pts',(20.6821342524129,-17.2888378226999,
13.3432722216374));
#148107=CARTESIAN_POINT('Ctrl Pts',(20.738063650735,-17.3566910252287,13.3476586836499));
#148108=CARTESIAN_POINT('Ctrl Pts',(20.7902715950829,-17.4270911085396,
13.3520451456625));
#148109=CARTESIAN_POINT('Ctrl Pts',(20.8400773745207,-17.4942519796594,
13.3562297800555));
#148110=CARTESIAN_POINT('Ctrl Pts',(20.8866820202992,-17.5639804959204,
13.3604144144486));
#148111=CARTESIAN_POINT('Ctrl Pts',(20.9298102405872,-17.6359386840529,
13.3645990488416));
#148112=CARTESIAN_POINT('Ctrl Pts',(20.9728770731919,-17.7077944486113,
13.3687777269256));
#148113=CARTESIAN_POINT('Ctrl Pts',(21.0124770746365,-17.7818731899369,
13.3729564050095));
#148114=CARTESIAN_POINT('Ctrl Pts',(21.0483765860078,-17.8578057676359,
13.3771350830935));
#148115=CARTESIAN_POINT('Ctrl Pts',(21.0849195703199,-17.9350993822183,
13.3813886609789));
#148116=CARTESIAN_POINT('Ctrl Pts',(21.1176278099319,-18.0143135596366,
13.3856422388643));
#148117=CARTESIAN_POINT('Ctrl Pts',(21.1463023579538,-18.0950301441645,
13.3898958167498));
#148118=CARTESIAN_POINT('Ctrl Pts',(21.1744209939084,-18.1741818801958,
13.3940669307277));
#148119=CARTESIAN_POINT('Ctrl Pts',(21.1986607834443,-18.2547778355445,
13.3982380447057));
#148120=CARTESIAN_POINT('Ctrl Pts',(21.2188822787495,-18.3364026797032,
13.4024091586836));
#148121=CARTESIAN_POINT('Ctrl Pts',(21.2390969885367,-18.4180001338572,
13.406578873004));
#148122=CARTESIAN_POINT('Ctrl Pts',(21.2552959714612,-18.5006253449795,
13.4107485873244));
#148123=CARTESIAN_POINT('Ctrl Pts',(21.2673900009521,-18.5838490756821,
13.4149183016447));
#148124=CARTESIAN_POINT('Ctrl Pts',(21.2794836000854,-18.6670698449271,
13.4190878675888));
#148125=CARTESIAN_POINT('Ctrl Pts',(21.2874724709,-18.7508886360331,13.4232574335328));
#148126=CARTESIAN_POINT('Ctrl Pts',(21.2913189573956,-18.8348686628402,
13.4274269994769));
#148127=CARTESIAN_POINT('Ctrl Pts',(21.2953006816113,-18.9218013237893,
13.4317431622158));
#148128=CARTESIAN_POINT('Ctrl Pts',(21.2948432851383,-19.0089062426184,
13.4360593249547));
#148129=CARTESIAN_POINT('Ctrl Pts',(21.2899637772452,-19.095698188612,13.4403754876936));
#148130=CARTESIAN_POINT('Ctrl Pts',(21.2852432188086,-19.1796628960938,
13.4445510518853));
#148131=CARTESIAN_POINT('Ctrl Pts',(21.2763843217563,-19.2633342443401,
13.448726616077));
#148132=CARTESIAN_POINT('Ctrl Pts',(21.2634552371752,-19.3462793465638,
13.4529021802687));
#148133=CARTESIAN_POINT('Ctrl Pts',(21.249873135268,-19.4334138087177,13.4572886422812));
#148134=CARTESIAN_POINT('Ctrl Pts',(21.2317989893781,-19.5197461599058,
13.4616751042937));
#148135=CARTESIAN_POINT('Ctrl Pts',(21.2093716504546,-19.6047903125242,
13.4660615663063));
#148136=CARTESIAN_POINT('Ctrl Pts',(21.1869443115312,-19.6898344651427,
13.4704480283188));
#148137=CARTESIAN_POINT('Ctrl Pts',(21.1601640287334,-19.7735898897036,
13.4748344903314));
#148138=CARTESIAN_POINT('Ctrl Pts',(21.1292278697972,-19.855594738667,13.4792209523439));
#148139=CARTESIAN_POINT('Ctrl Pts',(21.0997172163826,-19.9338208908233,
13.483405290821));
#148140=CARTESIAN_POINT('Ctrl Pts',(21.0663154177823,-20.0107453980514,
13.487589629298));
#148141=CARTESIAN_POINT('Ctrl Pts',(21.0291576153325,-20.0859539323894,
13.491773967775));
#148142=CARTESIAN_POINT('Ctrl Pts',(20.9920502936115,-20.1610602921805,
13.4959526216194));
#148143=CARTESIAN_POINT('Ctrl Pts',(20.9511973024599,-20.2344548993957,
13.5001312754638));
#148144=CARTESIAN_POINT('Ctrl Pts',(20.9067825486354,-20.3057414806179,
13.5043099293083));
#148145=CARTESIAN_POINT('Ctrl Pts',(20.862419706075,-20.3769447432077,13.5084836992079));
#148146=CARTESIAN_POINT('Ctrl Pts',(20.8145036176995,-20.4460444889432,
13.5126574691076));
#148147=CARTESIAN_POINT('Ctrl Pts',(20.7632642938657,-20.512668582897,13.5168312390073));
#148148=CARTESIAN_POINT('Ctrl Pts',(20.7120601643895,-20.5792469152753,
13.5210021421019));
#148149=CARTESIAN_POINT('Ctrl Pts',(20.657537612992,-20.6433526098853,13.5251730451966));
#148150=CARTESIAN_POINT('Ctrl Pts',(20.5999695483209,-20.7046430454428,
13.5293439482913));
#148151=CARTESIAN_POINT('Ctrl Pts',(20.5424157972175,-20.7659182419125,
13.5335138143439));
#148152=CARTESIAN_POINT('Ctrl Pts',(20.4818183469846,-20.8243792304162,
13.5376836803965));
#148153=CARTESIAN_POINT('Ctrl Pts',(20.4184891456872,-20.8797179041712,
13.5418535464491));
#148154=CARTESIAN_POINT('Ctrl Pts',(20.3779280055904,-20.9151612644688,
13.5445242657647));
#148155=CARTESIAN_POINT('Ctrl Pts',(20.3362470404378,-20.9493245120241,
13.5471949850803));
#148156=CARTESIAN_POINT('Ctrl Pts',(20.2935357468249,-20.9821350335323,
13.5498657043958));
#148157=CARTESIAN_POINT('Ctrl Pts',(20.2935357468249,-20.9821350335323,
12.7499597608822));
#148158=CARTESIAN_POINT('Ctrl Pts',(20.226946636523,-21.0332883293229,12.7541315972059));
#148159=CARTESIAN_POINT('Ctrl Pts',(20.1577807455201,-21.0812060335431,
12.7583034335296));
#148160=CARTESIAN_POINT('Ctrl Pts',(20.0863882307441,-21.1256250995387,
12.7624752698533));
#148161=CARTESIAN_POINT('Ctrl Pts',(20.0150266132867,-21.17002494181,12.7666453006858));
#148162=CARTESIAN_POINT('Ctrl Pts',(19.9414406756441,-21.2109289098134,
12.7708153315183));
#148163=CARTESIAN_POINT('Ctrl Pts',(19.8660096662966,-21.2481171824215,
12.7749853623508));
#148164=CARTESIAN_POINT('Ctrl Pts',(19.7905886744805,-21.2853005162823,
12.779154839387));
#148165=CARTESIAN_POINT('Ctrl Pts',(19.713323510543,-21.3187689321608,12.7833243164232));
#148166=CARTESIAN_POINT('Ctrl Pts',(19.6346169149111,-21.3483491341155,
12.7874937934594));
#148167=CARTESIAN_POINT('Ctrl Pts',(19.5558971620611,-21.3779342809311,
12.7916639674985));
#148168=CARTESIAN_POINT('Ctrl Pts',(19.4757359300974,-21.4036297625856,
12.7958341415375));
#148169=CARTESIAN_POINT('Ctrl Pts',(19.3945534755297,-21.4253113645406,
12.8000043155765));
#148170=CARTESIAN_POINT('Ctrl Pts',(19.3132817233196,-21.4470168154411,
12.8041790766499));
#148171=CARTESIAN_POINT('Ctrl Pts',(19.2309869517452,-21.4646994560134,
12.8083538377233));
#148172=CARTESIAN_POINT('Ctrl Pts',(19.1481015024818,-21.4782858004672,
12.8125285987966));
#148173=CARTESIAN_POINT('Ctrl Pts',(19.0651644433043,-21.4918806046697,
12.81670595935));
#148174=CARTESIAN_POINT('Ctrl Pts',(18.9816364311649,-21.5013739840884,
12.8208833199033));
#148175=CARTESIAN_POINT('Ctrl Pts',(18.8979544650464,-21.5067443968803,
12.8250606804566));
#148176=CARTESIAN_POINT('Ctrl Pts',(18.8141346684161,-21.5121236551472,
12.8292449214379));
#148177=CARTESIAN_POINT('Ctrl Pts',(18.7301608710164,-21.5133663855053,
12.8334291624192));
#148178=CARTESIAN_POINT('Ctrl Pts',(18.6464691654977,-21.5105031469614,
12.8376134034005));
#148179=CARTESIAN_POINT('Ctrl Pts',(18.608275919502,-21.5091964897082,12.8395229085792));
#148180=CARTESIAN_POINT('Ctrl Pts',(18.5701413376032,-21.5070354322662,
12.8414324137579));
#148181=CARTESIAN_POINT('Ctrl Pts',(18.5321062576875,-21.5040264334084,
12.8433419189367));
#148182=CARTESIAN_POINT('Ctrl Pts',(18.4487533004234,-21.497432285223,12.8475265533297));
#148183=CARTESIAN_POINT('Ctrl Pts',(18.3655686284663,-21.4867379250515,
12.8517111877228));
#148184=CARTESIAN_POINT('Ctrl Pts',(18.2829879003454,-21.4719579532137,
12.8558958221158));
#148185=CARTESIAN_POINT('Ctrl Pts',(18.2005247156697,-21.4571990188365,
12.8600745001997));
#148186=CARTESIAN_POINT('Ctrl Pts',(18.1186642162802,-21.4383661042868,
12.8642531782836));
#148187=CARTESIAN_POINT('Ctrl Pts',(18.0378381935519,-21.4155256725358,
12.8684318563676));
#148188=CARTESIAN_POINT('Ctrl Pts',(17.9555634224545,-21.3922758424606,
12.872685434253));
#148189=CARTESIAN_POINT('Ctrl Pts',(17.8743610594202,-21.3648734505898,
12.8769390121385));
#148190=CARTESIAN_POINT('Ctrl Pts',(17.7946770299223,-21.3334433350144,
12.8811925900239));
#148191=CARTESIAN_POINT('Ctrl Pts',(17.7165378308269,-21.3026225535603,
12.8853637040018));
#148192=CARTESIAN_POINT('Ctrl Pts',(17.6398590665665,-21.2679290019,12.8895348179798));
#148193=CARTESIAN_POINT('Ctrl Pts',(17.5650454327543,-21.2295305090636,
12.8937059319577));
#148194=CARTESIAN_POINT('Ctrl Pts',(17.4902569033794,-21.1911449012122,
12.8978756462781));
#148195=CARTESIAN_POINT('Ctrl Pts',(17.4173326704122,-21.1490570311436,
12.9020453605985));
#148196=CARTESIAN_POINT('Ctrl Pts',(17.3466549084741,-21.103481721284,12.9062150749189));
#148197=CARTESIAN_POINT('Ctrl Pts',(17.2759796615542,-21.0579080331895,
12.9103846408629));
#148198=CARTESIAN_POINT('Ctrl Pts',(17.2075511128842,-21.0088474020655,
12.9145542068069));
#148199=CARTESIAN_POINT('Ctrl Pts',(17.1417232369321,-20.9565584825078,
12.918723772751));
#148200=CARTESIAN_POINT('Ctrl Pts',(17.0735809340688,-20.9024311490436,
12.9230399354899));
#148201=CARTESIAN_POINT('Ctrl Pts',(17.008225998861,-20.8448446181552,12.9273560982288));
#148202=CARTESIAN_POINT('Ctrl Pts',(16.9460129971983,-20.7841305842686,
12.9316722609678));
#148203=CARTESIAN_POINT('Ctrl Pts',(16.8858265775214,-20.72539430365,12.9358478251594));
#148204=CARTESIAN_POINT('Ctrl Pts',(16.8285808237904,-20.6637315251358,
12.9400233893511));
#148205=CARTESIAN_POINT('Ctrl Pts',(16.7745572392503,-20.5994780931307,
12.9441989535428));
#148206=CARTESIAN_POINT('Ctrl Pts',(16.7178050518837,-20.5319793730228,
12.9485854155553));
#148207=CARTESIAN_POINT('Ctrl Pts',(16.6646094437673,-20.4616218795449,
12.9529718775679));
#148208=CARTESIAN_POINT('Ctrl Pts',(16.6152455573352,-20.38882970866,12.9573583395805));
#148209=CARTESIAN_POINT('Ctrl Pts',(16.5658816709031,-20.3160375377752,
12.961744801593));
#148210=CARTESIAN_POINT('Ctrl Pts',(16.5203497415207,-20.2408112252451,
12.9661312636056));
#148211=CARTESIAN_POINT('Ctrl Pts',(16.4788683829465,-20.1636028184871,
12.9705177256181));
#148212=CARTESIAN_POINT('Ctrl Pts',(16.4371381237558,-20.0859311380873,
12.9749305077209));
#148213=CARTESIAN_POINT('Ctrl Pts',(16.3993648293879,-20.0059905501582,
12.9793432898236));
#148214=CARTESIAN_POINT('Ctrl Pts',(16.3657873879881,-19.9241980375972,
12.9837560719264));
#148215=CARTESIAN_POINT('Ctrl Pts',(16.3323070847553,-19.8426421474352,
12.9881560880307));
#148216=CARTESIAN_POINT('Ctrl Pts',(16.302998596953,-19.7592453620159,12.9925561041351));
#148217=CARTESIAN_POINT('Ctrl Pts',(16.278054237255,-19.6744475139794,12.9969561202394));
#148218=CARTESIAN_POINT('Ctrl Pts',(16.2531532512186,-19.5897971138313,
13.0013484855236));
#148219=CARTESIAN_POINT('Ctrl Pts',(16.2326014031163,-19.5037508664346,
13.0057408508078));
#148220=CARTESIAN_POINT('Ctrl Pts',(16.2165427462274,-19.4167676574675,
13.010133216092));
#148221=CARTESIAN_POINT('Ctrl Pts',(16.200521001668,-19.3299843875664,13.0145154851125));
#148222=CARTESIAN_POINT('Ctrl Pts',(16.1889719431305,-19.2422688247292,
13.018897754133));
#148223=CARTESIAN_POINT('Ctrl Pts',(16.1819893075699,-19.1540926166946,
13.0232800231536));
#148224=CARTESIAN_POINT('Ctrl Pts',(16.176672671659,-19.0869545296414,13.0266167186812));
#148225=CARTESIAN_POINT('Ctrl Pts',(16.1740023911013,-19.0195497546633,
13.0299534142088));
#148226=CARTESIAN_POINT('Ctrl Pts',(16.174000001606,-18.9520906788001,13.0332901097364));
#148227=CARTESIAN_POINT('',(16.1736697275687,-18.9513574892655,12.9667098340851));
#148228=CARTESIAN_POINT('Ctrl Pts',(20.2929505273095,-20.9813917755491,
12.683192392576));
#148229=CARTESIAN_POINT('Ctrl Pts',(20.11142449751,-21.1236576232965,12.6946551510985));
#148230=CARTESIAN_POINT('Ctrl Pts',(19.1726622067198,-21.6766233453797,
12.7485098451814));
#148231=CARTESIAN_POINT('Ctrl Pts',(17.0319370527368,-21.4324760457865,
12.8430154491732));
#148232=CARTESIAN_POINT('Ctrl Pts',(16.1727139550341,-19.7651271422422,
12.9260582946424));
#148233=CARTESIAN_POINT('Ctrl Pts',(16.1699654914217,-18.9513691601896,
12.9667092045512));
#148234=CARTESIAN_POINT('Ctrl Pts',(16.1740000808904,-18.9513564484225,
12.9667098902285));
#148235=CARTESIAN_POINT('Ctrl Pts',(16.1740088273484,-18.9165636940743,
12.9684506873211));
#148236=CARTESIAN_POINT('Ctrl Pts',(16.1747268399112,-18.881780730387,12.9701914844137));
#148237=CARTESIAN_POINT('Ctrl Pts',(16.1761531171477,-18.8470270326105,
12.9719322815063));
#148238=CARTESIAN_POINT('Ctrl Pts',(16.1795816894971,-18.7634839708603,
12.9761169158993));
#148239=CARTESIAN_POINT('Ctrl Pts',(16.1871139062631,-18.6799535889704,
12.9803015502924));
#148240=CARTESIAN_POINT('Ctrl Pts',(16.1987516982625,-18.5968717857769,
12.9844861846854));
#148241=CARTESIAN_POINT('Ctrl Pts',(16.2103729253055,-18.5139082392468,
12.9886648627694));
#148242=CARTESIAN_POINT('Ctrl Pts',(16.2260880567288,-18.4313924548469,
12.9928435408533));
#148243=CARTESIAN_POINT('Ctrl Pts',(16.2458470513543,-18.3497584337278,
12.9970222189372));
#148244=CARTESIAN_POINT('Ctrl Pts',(16.2659602117581,-18.2666611814494,
13.0012757968227));
#148245=CARTESIAN_POINT('Ctrl Pts',(16.2902636140324,-18.1844780963255,
13.0055293747081));
#148246=CARTESIAN_POINT('Ctrl Pts',(16.3186494198465,-18.1036595170853,
13.0097829525935));
#148247=CARTESIAN_POINT('Ctrl Pts',(16.3464849114244,-18.0244077637083,
13.0139540665715));
#148248=CARTESIAN_POINT('Ctrl Pts',(16.3782457689155,-17.9464685351598,
13.0181251805494));
#148249=CARTESIAN_POINT('Ctrl Pts',(16.4137796304914,-17.8702526002262,
13.0222962945274));
#148250=CARTESIAN_POINT('Ctrl Pts',(16.4493015683369,-17.7940622402856,
13.0264660088478));
#148251=CARTESIAN_POINT('Ctrl Pts',(16.4885938016076,-17.7195944421082,
13.0306357231681));
#148252=CARTESIAN_POINT('Ctrl Pts',(16.5314561548595,-17.6472392517271,
13.0348054374885));
#148253=CARTESIAN_POINT('Ctrl Pts',(16.5743169828848,-17.5748866360543,
13.0389750034325));
#148254=CARTESIAN_POINT('Ctrl Pts',(16.6207474431035,-17.5046468740728,
13.0431445693766));
#148255=CARTESIAN_POINT('Ctrl Pts',(16.6705024900493,-17.4368834941077,
13.0473141353206));
#148256=CARTESIAN_POINT('Ctrl Pts',(16.7220068630664,-17.366737637298,13.0516302980595));
#148257=CARTESIAN_POINT('Ctrl Pts',(16.7770736453878,-17.2992459668448,
13.0559464607985));
#148258=CARTESIAN_POINT('Ctrl Pts',(16.8353848266788,-17.234775371818,13.0602626235374));
#148259=CARTESIAN_POINT('Ctrl Pts',(16.8917965273724,-17.1724048996433,
13.0644381877291));
#148260=CARTESIAN_POINT('Ctrl Pts',(16.9512441342268,-17.1128620023875,
13.0686137519207));
#148261=CARTESIAN_POINT('Ctrl Pts',(17.0134027193002,-17.0564407163983,
13.0727893161124));
#148262=CARTESIAN_POINT('Ctrl Pts',(17.078700786738,-16.9971697253824,13.077175778125));
#148263=CARTESIAN_POINT('Ctrl Pts',(17.146990440611,-16.9413443477726,13.0815622401375));
#148264=CARTESIAN_POINT('Ctrl Pts',(17.2178583236867,-16.889255610274,13.0859487021501));
#148265=CARTESIAN_POINT('Ctrl Pts',(17.2887262067624,-16.8371668727754,
13.0903351641627));
#148266=CARTESIAN_POINT('Ctrl Pts',(17.3621717925896,-16.7888150309009,
13.0947216261752));
#148267=CARTESIAN_POINT('Ctrl Pts',(17.4377516489583,-16.7444356832877,
13.0991080881878));
#148268=CARTESIAN_POINT('Ctrl Pts',(17.5098539640989,-16.7020982952443,
13.1032927225808));
#148269=CARTESIAN_POINT('Ctrl Pts',(17.5841668423745,-16.6632182861073,
13.1074773569739));
#148270=CARTESIAN_POINT('Ctrl Pts',(17.6603248069611,-16.6280332231607,
13.1116619913669));
#148271=CARTESIAN_POINT('Ctrl Pts',(17.7363743701116,-16.5928982417961,
13.1158406694509));
#148272=CARTESIAN_POINT('Ctrl Pts',(17.8142633889644,-16.5614479512896,
13.1200193475348));
#148273=CARTESIAN_POINT('Ctrl Pts',(17.8935998508937,-16.5338751915209,
13.1241980256187));
#148274=CARTESIAN_POINT('Ctrl Pts',(17.9743583618848,-16.5058082098496,
13.1284516035042));
#148275=CARTESIAN_POINT('Ctrl Pts',(18.0566163014193,-16.4817593798135,
13.1327051813896));
#148276=CARTESIAN_POINT('Ctrl Pts',(18.1399366350505,-16.461881786255,13.136958759275));
#148277=CARTESIAN_POINT('Ctrl Pts',(18.221641641428,-16.4423895586354,13.141129873253));
#148278=CARTESIAN_POINT('Ctrl Pts',(18.3043677482547,-16.4269083873418,
13.145300987231));
#148279=CARTESIAN_POINT('Ctrl Pts',(18.3876870934188,-16.4155325015417,
13.1494721012089));
#148280=CARTESIAN_POINT('Ctrl Pts',(18.470978479972,-16.4041604330299,13.1536418155293));
#148281=CARTESIAN_POINT('Ctrl Pts',(18.5548622540878,-16.39689097632,13.1578115298496));
#148282=CARTESIAN_POINT('Ctrl Pts',(18.6389020976076,-16.3937669400618,
13.16198124417));
#148283=CARTESIAN_POINT('Ctrl Pts',(18.7229389506291,-16.3906430149703,
13.1661508101141));
#148284=CARTESIAN_POINT('Ctrl Pts',(18.8071314022655,-16.3916642332765,
13.1703203760581));
#148285=CARTESIAN_POINT('Ctrl Pts',(18.8910411442615,-16.3968213215102,
13.1744899420021));
#148286=CARTESIAN_POINT('Ctrl Pts',(18.9779010492722,-16.4021597266042,
13.1788061047411));
#148287=CARTESIAN_POINT('Ctrl Pts',(19.064457468181,-16.4119302148937,13.18312226748));
#148288=CARTESIAN_POINT('Ctrl Pts',(19.1502297723792,-16.4260639801085,
13.1874384302189));
#148289=CARTESIAN_POINT('Ctrl Pts',(19.2332080527898,-16.4397373394081,
13.1916139944106));
#148290=CARTESIAN_POINT('Ctrl Pts',(19.3154520685914,-16.4574939280207,
13.1957895586023));
#148291=CARTESIAN_POINT('Ctrl Pts',(19.3965387044157,-16.4792196892665,
13.1999651227939));
#148292=CARTESIAN_POINT('Ctrl Pts',(19.4817208334501,-16.5020427670648,
13.2043515848065));
#148293=CARTESIAN_POINT('Ctrl Pts',(19.5656250358877,-16.5292463408117,
13.208738046819));
#148294=CARTESIAN_POINT('Ctrl Pts',(19.6477828618953,-16.5606403697255,
13.2131245088315));
#148295=CARTESIAN_POINT('Ctrl Pts',(19.7299406879029,-16.5920343986394,
13.2175109708441));
#148296=CARTESIAN_POINT('Ctrl Pts',(19.8103516376767,-16.6276185783624,
13.2218974328566));
#148297=CARTESIAN_POINT('Ctrl Pts',(19.888577588602,-16.6671475776545,13.2262838948691));
#148298=CARTESIAN_POINT('Ctrl Pts',(19.9632042475667,-16.7048577890932,
13.2304685292622));
#148299=CARTESIAN_POINT('Ctrl Pts',(20.0361203339114,-16.7462981479268,
13.2346531636552));
#148300=CARTESIAN_POINT('Ctrl Pts',(20.1069282654733,-16.7912899366494,
13.2388377980483));
#148301=CARTESIAN_POINT('Ctrl Pts',(20.1776354107088,-16.8362176851296,
13.2430164761322));
#148302=CARTESIAN_POINT('Ctrl Pts',(20.2462399765314,-16.884686578031,13.2471951542162));
#148303=CARTESIAN_POINT('Ctrl Pts',(20.3123676261203,-16.9364713753421,
13.2513738323001));
#148304=CARTESIAN_POINT('Ctrl Pts',(20.379680566303,-16.9891843779279,13.2556274101855));
#148305=CARTESIAN_POINT('Ctrl Pts',(20.4444264890784,-17.0453331118989,
13.259880988071));
#148306=CARTESIAN_POINT('Ctrl Pts',(20.5062401158633,-17.1046329623692,
13.2641345659564));
#148307=CARTESIAN_POINT('Ctrl Pts',(20.5668553648736,-17.162783169524,13.2683056799344));
#148308=CARTESIAN_POINT('Ctrl Pts',(20.6246506525836,-17.2239630692774,
13.2724767939123));
#148309=CARTESIAN_POINT('Ctrl Pts',(20.6793151535296,-17.2878639017652,
13.2766479078903));
#148310=CARTESIAN_POINT('Ctrl Pts',(20.7339613112743,-17.3517432917116,
13.2808176222106));
#148311=CARTESIAN_POINT('Ctrl Pts',(20.7854784698982,-17.418341451807,13.284987336531));
#148312=CARTESIAN_POINT('Ctrl Pts',(20.8335944633575,-17.487314679039,13.2891570508514));
#148313=CARTESIAN_POINT('Ctrl Pts',(20.8817087446432,-17.5562854519076,
13.2933266167954));
#148314=CARTESIAN_POINT('Ctrl Pts',(20.9264218388937,-17.6276307460897,
13.2974961827395));
#148315=CARTESIAN_POINT('Ctrl Pts',(20.9675042956845,-17.7009769941527,
13.3016657486835));
#148316=CARTESIAN_POINT('Ctrl Pts',(21.0100311609753,-17.7769020058154,
13.3059819114224));
#148317=CARTESIAN_POINT('Ctrl Pts',(21.0486670744203,-17.8549708362667,
13.3102980741614));
#148318=CARTESIAN_POINT('Ctrl Pts',(21.0832097360536,-17.9347421093788,
13.3146142369003));
#148319=CARTESIAN_POINT('Ctrl Pts',(21.1166271741174,-18.0119148416597,
13.318789801092));
#148320=CARTESIAN_POINT('Ctrl Pts',(21.1462138190076,-18.0906803481868,
13.3229653652836));
#148321=CARTESIAN_POINT('Ctrl Pts',(21.1718365500182,-18.1706211191774,
13.3271409294753));
#148322=CARTESIAN_POINT('Ctrl Pts',(21.1987534242598,-18.2545995084698,
13.3315273914879));
#148323=CARTESIAN_POINT('Ctrl Pts',(21.2212952772081,-18.3398744431048,
13.3359138535004));
#148324=CARTESIAN_POINT('Ctrl Pts',(21.2393683400758,-18.4259491654358,
13.340300315513));
#148325=CARTESIAN_POINT('Ctrl Pts',(21.2574414029436,-18.5120238877669,
13.3446867775255));
#148326=CARTESIAN_POINT('Ctrl Pts',(21.2710456611134,-18.5988978127949,
13.349073239538));
#148327=CARTESIAN_POINT('Ctrl Pts',(21.2801502518719,-18.6860697555883,
13.3534597015506));
#148328=CARTESIAN_POINT('Ctrl Pts',(21.2888359269133,-18.7692307880738,
13.3576443359436));
#148329=CARTESIAN_POINT('Ctrl Pts',(21.2934592377886,-18.852972557727,13.3618289703367));
#148330=CARTESIAN_POINT('Ctrl Pts',(21.2939552539536,-18.9368640244713,
13.3660136047297));
#148331=CARTESIAN_POINT('Ctrl Pts',(21.294450564101,-19.0206360820962,13.3701922828137));
#148332=CARTESIAN_POINT('Ctrl Pts',(21.2908302458307,-19.1045569574875,
13.3743709608976));
#148333=CARTESIAN_POINT('Ctrl Pts',(21.2830810689264,-19.1881899744725,
13.3785496389816));
#148334=CARTESIAN_POINT('Ctrl Pts',(21.2751929935952,-19.2733220531809,
13.382803216867));
#148335=CARTESIAN_POINT('Ctrl Pts',(21.2630265340501,-19.3581553727241,
13.3870567947524));
#148336=CARTESIAN_POINT('Ctrl Pts',(21.2466232879999,-19.4422287349806,
13.3913103726379));
#148337=CARTESIAN_POINT('Ctrl Pts',(21.2305380508826,-19.5246721710542,
13.3954814866158));
#148338=CARTESIAN_POINT('Ctrl Pts',(21.2103789301821,-19.6063843810838,
13.3996526005938));
#148339=CARTESIAN_POINT('Ctrl Pts',(21.1862373001536,-19.6869368841851,
13.4038237145717));
#148340=CARTESIAN_POINT('Ctrl Pts',(21.1621037710821,-19.767462357116,13.4079934288921));
#148341=CARTESIAN_POINT('Ctrl Pts',(21.133990518692,-19.8468284556773,13.4121631432125));
#148342=CARTESIAN_POINT('Ctrl Pts',(21.1020392245072,-19.9246202913755,
13.4163328575329));
#148343=CARTESIAN_POINT('Ctrl Pts',(21.0700890672866,-20.0024093589063,
13.4205024234769));
#148344=CARTESIAN_POINT('Ctrl Pts',(21.0343013153838,-20.0786238497406,
13.4246719894209));
#148345=CARTESIAN_POINT('Ctrl Pts',(20.9948658827286,-20.1528686274168,
13.428841555365));
#148346=CARTESIAN_POINT('Ctrl Pts',(20.9540439489101,-20.2297237598852,
13.4331577181039));
#148347=CARTESIAN_POINT('Ctrl Pts',(20.9093133043205,-20.3044676260572,
13.4374738808428));
#148348=CARTESIAN_POINT('Ctrl Pts',(20.8609355752996,-20.3766912151498,
13.4417900435818));
#148349=CARTESIAN_POINT('Ctrl Pts',(20.8141337457131,-20.4465621284243,
13.4459656077734));
#148350=CARTESIAN_POINT('Ctrl Pts',(20.7639191093593,-20.5140740893661,
13.4501411719651));
#148351=CARTESIAN_POINT('Ctrl Pts',(20.7105706701799,-20.5788891744014,
13.4543167361568));
#148352=CARTESIAN_POINT('Ctrl Pts',(20.6545277281615,-20.6469779152986,
13.4587031981693));
#148353=CARTESIAN_POINT('Ctrl Pts',(20.5950264806454,-20.7120897510532,
13.4630896601819));
#148354=CARTESIAN_POINT('Ctrl Pts',(20.5324338669328,-20.7738769514622,
13.4674761221944));
#148355=CARTESIAN_POINT('Ctrl Pts',(20.4698412532202,-20.8356641518712,
13.4718625842069));
#148356=CARTESIAN_POINT('Ctrl Pts',(20.4041577572905,-20.8941263879947,
13.4762490462195));
#148357=CARTESIAN_POINT('Ctrl Pts',(20.3357880909558,-20.9489664272771,
13.480635508232));
#148358=CARTESIAN_POINT('Ctrl Pts',(20.3218259558186,-20.9601656049306,
13.4815312910942));
#148359=CARTESIAN_POINT('Ctrl Pts',(20.3077408189587,-20.9712227949802,
13.4824270739563));
#148360=CARTESIAN_POINT('Ctrl Pts',(20.2935357468249,-20.9821350335323,
13.4833228568185));
#148361=CARTESIAN_POINT('Origin',(18.734,-18.952,-1.76670989022851));
#148362=CARTESIAN_POINT('',(20.2947698132858,-20.9837129250579,14.3497865232697));
#148363=CARTESIAN_POINT('',(20.2923704978255,-20.9805871927216,14.2834124327049));
#148364=CARTESIAN_POINT('',(20.2935357468249,-20.9821350335323,-1.76670989022851));
#148365=CARTESIAN_POINT('',(16.1740010575059,-18.949673107456,13.8332901097715));
#148366=CARTESIAN_POINT('Ctrl Pts',(16.1735504202813,-18.9496726978525,
13.8332901097715));
#148367=CARTESIAN_POINT('Ctrl Pts',(16.1718449019213,-18.765781352641,13.8424428639771));
#148368=CARTESIAN_POINT('Ctrl Pts',(16.2739023737919,-17.7320561796712,
13.8939875537431));
#148369=CARTESIAN_POINT('Ctrl Pts',(17.6781137265109,-16.1150307104843,
13.9879241790696));
#148370=CARTESIAN_POINT('Ctrl Pts',(20.5479109989865,-16.5285690725847,
14.1150999857511));
#148371=CARTESIAN_POINT('Ctrl Pts',(21.6914148502026,-19.029541834012,14.2357207671511));
#148372=CARTESIAN_POINT('Ctrl Pts',(20.8607340421186,-20.5404053550185,
14.3139496129906));
#148373=CARTESIAN_POINT('Ctrl Pts',(20.2947698132858,-20.9837129250579,
14.3497865232697));
#148374=CARTESIAN_POINT('Ctrl Pts',(20.2935357468249,-20.9821350335323,
13.5498657043958));
#148375=CARTESIAN_POINT('Ctrl Pts',(20.2268456522252,-21.0333659047647,
13.5540358081023));
#148376=CARTESIAN_POINT('Ctrl Pts',(20.157642311523,-21.0812965736288,13.5582059118088));
#148377=CARTESIAN_POINT('Ctrl Pts',(20.0862913281455,-21.125685387498,13.5623760155153));
#148378=CARTESIAN_POINT('Ctrl Pts',(20.014862529641,-21.1701226116488,13.566550667122));
#148379=CARTESIAN_POINT('Ctrl Pts',(19.9412818046901,-21.2110100274126,
13.5707253187287));
#148380=CARTESIAN_POINT('Ctrl Pts',(19.8659411674346,-21.2481509518032,
13.5748999703354));
#148381=CARTESIAN_POINT('Ctrl Pts',(19.7905547245971,-21.2853144571238,
13.5790771600457));
#148382=CARTESIAN_POINT('Ctrl Pts',(19.7134066615509,-21.3187267542991,
13.583254349756));
#148383=CARTESIAN_POINT('Ctrl Pts',(19.6349086504671,-21.3482394712369,
13.5874315394664));
#148384=CARTESIAN_POINT('Ctrl Pts',(19.5562800787177,-21.3778012747683,
13.5916156768262));
#148385=CARTESIAN_POINT('Ctrl Pts',(19.4762975144192,-21.4034504101753,
13.595799814186));
#148386=CARTESIAN_POINT('Ctrl Pts',(19.3953870533626,-21.4250885883131,
13.5999839515459));
#148387=CARTESIAN_POINT('Ctrl Pts',(19.3540513159326,-21.4361431545371,
13.6021215540391));
#148388=CARTESIAN_POINT('Ctrl Pts',(19.3124735532324,-21.4461516842229,
13.6042591565322));
#148389=CARTESIAN_POINT('Ctrl Pts',(19.2707112385803,-21.4551062794819,
13.6063967590254));
#148390=CARTESIAN_POINT('Ctrl Pts',(19.1889560858866,-21.4726360622251,
13.6105813934184));
#148391=CARTESIAN_POINT('Ctrl Pts',(19.1061890642126,-21.486188888916,13.6147660278115));
#148392=CARTESIAN_POINT('Ctrl Pts',(19.022831797239,-21.4956541024486,13.6189506622045));
#148393=CARTESIAN_POINT('Ctrl Pts',(18.9395931790174,-21.5051058434214,
13.6231293402885));
#148394=CARTESIAN_POINT('Ctrl Pts',(18.8557664374669,-21.5104814765754,
13.6273080183724));
#148395=CARTESIAN_POINT('Ctrl Pts',(18.7717843292961,-21.5117211458398,
13.6314866964563));
#148396=CARTESIAN_POINT('Ctrl Pts',(18.6862969021932,-21.5129830352849,
13.6357402743418));
#148397=CARTESIAN_POINT('Ctrl Pts',(18.6006489552156,-21.5099591270341,
13.6399938522272));
#148398=CARTESIAN_POINT('Ctrl Pts',(18.5153034901263,-21.5026414559026,
13.6442474301127));
#148399=CARTESIAN_POINT('Ctrl Pts',(18.4316126134156,-21.4954656521053,
13.6484185440906));
#148400=CARTESIAN_POINT('Ctrl Pts',(18.3482130743118,-21.4841611267896,
13.6525896580686));
#148401=CARTESIAN_POINT('Ctrl Pts',(18.2655406684998,-21.4687729048785,
13.6567607720465));
#148402=CARTESIAN_POINT('Ctrl Pts',(18.1828960042121,-21.4533898466338,
13.6609304863669));
#148403=CARTESIAN_POINT('Ctrl Pts',(18.1009784405236,-21.4339258973909,
13.6651002006873));
#148404=CARTESIAN_POINT('Ctrl Pts',(18.0202156389588,-21.4104775544904,
13.6692699150076));
#148405=CARTESIAN_POINT('Ctrl Pts',(17.939455711281,-21.3870300459826,13.6734394809517));
#148406=CARTESIAN_POINT('Ctrl Pts',(17.8598509055783,-21.3595985548016,
13.6776090468957));
#148407=CARTESIAN_POINT('Ctrl Pts',(17.7818144029985,-21.3283296465059,
13.6817786128398));
#148408=CARTESIAN_POINT('Ctrl Pts',(17.7010342332564,-21.2959613619689,
13.6860947755787));
#148409=CARTESIAN_POINT('Ctrl Pts',(17.6219351912173,-21.2594809885574,
13.6904109383176));
#148410=CARTESIAN_POINT('Ctrl Pts',(17.5449519222896,-21.2191049091062,
13.6947271010565));
#148411=CARTESIAN_POINT('Ctrl Pts',(17.4704763752501,-21.1800440761963,
13.6989026652482));
#148412=CARTESIAN_POINT('Ctrl Pts',(17.3979812574152,-21.1373377246259,
13.7030782294399));
#148413=CARTESIAN_POINT('Ctrl Pts',(17.3278323932016,-21.091227117814,13.7072537936316));
#148414=CARTESIAN_POINT('Ctrl Pts',(17.2541404766197,-21.0427875738696,
13.7116402556441));
#148415=CARTESIAN_POINT('Ctrl Pts',(17.1830385318335,-20.9905911845411,
13.7160267176566));
#148416=CARTESIAN_POINT('Ctrl Pts',(17.1149115381732,-20.9349655954603,
13.7204131796692));
#148417=CARTESIAN_POINT('Ctrl Pts',(17.0467845445129,-20.8793400063795,
13.7247996416817));
#148418=CARTESIAN_POINT('Ctrl Pts',(16.9816328807925,-20.8202856635707,
13.7291861036943));
#148419=CARTESIAN_POINT('Ctrl Pts',(16.9197953580219,-20.7581731691688,
13.7335725657068));
#148420=CARTESIAN_POINT('Ctrl Pts',(16.8612222805613,-20.6993396360182,
13.7377274633762));
#148421=CARTESIAN_POINT('Ctrl Pts',(16.8053896617352,-20.6375286216453,
13.7418823610455));
#148422=CARTESIAN_POINT('Ctrl Pts',(16.7526212754374,-20.5730300274365,
13.7460372587149));
#148423=CARTESIAN_POINT('Ctrl Pts',(16.7002946208399,-20.5090713601742,
13.7501573751423));
#148424=CARTESIAN_POINT('Ctrl Pts',(16.6509814300939,-20.4424702805592,
13.7542774915697));
#148425=CARTESIAN_POINT('Ctrl Pts',(16.6049624110076,-20.3735480803186,
13.7583976079971));
#148426=CARTESIAN_POINT('Ctrl Pts',(16.5589874739682,-20.3046919012954,
13.7625137777266));
#148427=CARTESIAN_POINT('Ctrl Pts',(16.5163007099123,-20.2335194044224,
13.7666299474561));
#148428=CARTESIAN_POINT('Ctrl Pts',(16.4771421768208,-20.1603843618463,
13.7707461171856));
#148429=CARTESIAN_POINT('Ctrl Pts',(16.4380086398887,-20.0872960037358,
13.7748596594307));
#148430=CARTESIAN_POINT('Ctrl Pts',(16.4023990866291,-20.0122480031431,
13.7789732016757));
#148431=CARTESIAN_POINT('Ctrl Pts',(16.3705090605919,-19.9356211564092,
13.7830867439208));
#148432=CARTESIAN_POINT('Ctrl Pts',(16.3380758082443,-19.8576890200784,
13.7872703577417));
#148433=CARTESIAN_POINT('Ctrl Pts',(16.3094902338592,-19.7781241832446,
13.7914539715626));
#148434=CARTESIAN_POINT('Ctrl Pts',(16.2849076425233,-19.6973500013747,
13.7956375853835));
#148435=CARTESIAN_POINT('Ctrl Pts',(16.2607361379239,-19.6179265800639,
13.7997512379815));
#148436=CARTESIAN_POINT('Ctrl Pts',(16.2404348481341,-19.5373344318006,
13.8038648905795));
#148437=CARTESIAN_POINT('Ctrl Pts',(16.2241009663662,-19.455990913573,13.8079785431774));
#148438=CARTESIAN_POINT('Ctrl Pts',(16.2073503971231,-19.3725722716413,
13.8121971376098));
#148439=CARTESIAN_POINT('Ctrl Pts',(16.1947725425284,-19.2883639128979,
13.8164157320421));
#148440=CARTESIAN_POINT('Ctrl Pts',(16.1864159534739,-19.2038243949375,
13.8206343264745));
#148441=CARTESIAN_POINT('Ctrl Pts',(16.1780593644194,-19.1192848769771,
13.8248529209068));
#148442=CARTESIAN_POINT('Ctrl Pts',(16.1739240322153,-19.0344147354448,
13.8290715153392));
#148443=CARTESIAN_POINT('Ctrl Pts',(16.1740010575059,-18.949673107456,13.8332901097715));
#148444=CARTESIAN_POINT('',(16.1740010826188,-18.9543543591274,13.7667098774921));
#148445=CARTESIAN_POINT('Ctrl Pts',(20.2935357468249,-20.9821350335323,
13.4833228568185));
#148446=CARTESIAN_POINT('Ctrl Pts',(20.2271990631406,-21.0330944169343,
13.4875060995234));
#148447=CARTESIAN_POINT('Ctrl Pts',(20.1582439358111,-21.0808896740306,
13.4916893422283));
#148448=CARTESIAN_POINT('Ctrl Pts',(20.0870050715129,-21.1252411915064,
13.4958725849332));
#148449=CARTESIAN_POINT('Ctrl Pts',(20.0158625563524,-21.1695327244428,
13.5000501698861));
#148450=CARTESIAN_POINT('Ctrl Pts',(19.942442827238,-21.2103895284926,13.504227754839));
#148451=CARTESIAN_POINT('Ctrl Pts',(19.8671122352966,-21.247573275289,13.5084053397919));
#148452=CARTESIAN_POINT('Ctrl Pts',(19.7918615905526,-21.2847175595474,
13.5125784911382));
#148453=CARTESIAN_POINT('Ctrl Pts',(19.7147045242392,-21.3181963316418,
13.5167516424845));
#148454=CARTESIAN_POINT('Ctrl Pts',(19.6360336482658,-21.3478162069317,
13.5209247938308));
#148455=CARTESIAN_POINT('Ctrl Pts',(19.5574081725827,-21.3774189888445,
13.5250955368872));
#148456=CARTESIAN_POINT('Ctrl Pts',(19.4772710512136,-21.4031671335675,
13.5292662799435));
#148457=CARTESIAN_POINT('Ctrl Pts',(19.3960355903709,-21.4249150565845,
13.5334370229998));
#148458=CARTESIAN_POINT('Ctrl Pts',(19.3148226408376,-21.4466569529941,
13.5376066102938));
#148459=CARTESIAN_POINT('Ctrl Pts',(19.2325124005023,-21.4644007105937,
13.5417761975877));
#148460=CARTESIAN_POINT('Ctrl Pts',(19.1495327658116,-21.4780507755263,
13.5459457848817));
#148461=CARTESIAN_POINT('Ctrl Pts',(19.0665512339994,-21.4917011525335,
13.5501154675029));
#148462=CARTESIAN_POINT('Ctrl Pts',(18.982900731597,-21.5012575776353,13.554285150124));
#148463=CARTESIAN_POINT('Ctrl Pts',(18.8990174051097,-21.5066759591014,
13.5584548327451));
#148464=CARTESIAN_POINT('Ctrl Pts',(18.8150490006465,-21.5120998361166,
13.5626287444327));
#148465=CARTESIAN_POINT('Ctrl Pts',(18.7308477605494,-21.5133772563818,
13.5668026561202));
#148466=CARTESIAN_POINT('Ctrl Pts',(18.6468525185955,-21.5105162333831,
13.5709765678078));
#148467=CARTESIAN_POINT('Ctrl Pts',(18.5628158450396,-21.5076537991525,
13.5751525383244));
#148468=CARTESIAN_POINT('Ctrl Pts',(18.4789858309805,-21.5006488937704,
13.579328508841));
#148469=CARTESIAN_POINT('Ctrl Pts',(18.3957964105736,-21.4895614932646,
13.5835044793576));
#148470=CARTESIAN_POINT('Ctrl Pts',(18.312457595632,-21.4784541816086,13.5876879492314));
#148471=CARTESIAN_POINT('Ctrl Pts',(18.2297621264903,-21.4632498088279,
13.5918714191051));
#148472=CARTESIAN_POINT('Ctrl Pts',(18.1481338832284,-21.4440595685535,
13.5960548889789));
#148473=CARTESIAN_POINT('Ctrl Pts',(18.0716697338467,-21.4260833713406,
13.5999736976237));
#148474=CARTESIAN_POINT('Ctrl Pts',(17.9961422166987,-21.4046102585772,
13.6038925062686));
#148475=CARTESIAN_POINT('Ctrl Pts',(17.921884774769,-21.379770347654,13.6078113149135));
#148476=CARTESIAN_POINT('Ctrl Pts',(17.842590205016,-21.353245463438,13.6119959493065));
#148477=CARTESIAN_POINT('Ctrl Pts',(17.7644489508446,-21.3227823154618,
13.6161805836996));
#148478=CARTESIAN_POINT('Ctrl Pts',(17.6878802554244,-21.2885002632162,
13.6203652180926));
#148479=CARTESIAN_POINT('Ctrl Pts',(17.6114205460648,-21.2542670072286,
13.6245438961766));
#148480=CARTESIAN_POINT('Ctrl Pts',(17.5365293656821,-21.2162258304372,
13.6287225742605));
#148481=CARTESIAN_POINT('Ctrl Pts',(17.4636096823068,-21.1745454867587,
13.6329012523444));
#148482=CARTESIAN_POINT('Ctrl Pts',(17.3893829660135,-21.1321180528749,
13.6371548302299));
#148483=CARTESIAN_POINT('Ctrl Pts',(17.3171995773183,-21.0859198576824,
13.6414084081153));
#148484=CARTESIAN_POINT('Ctrl Pts',(17.2474621052953,-21.0361797157651,
13.6456619860008));
#148485=CARTESIAN_POINT('Ctrl Pts',(17.1790766302489,-20.9874038835589,
13.6498330999787));
#148486=CARTESIAN_POINT('Ctrl Pts',(17.1130434722312,-20.9352224936048,
13.6540042139567));
#148487=CARTESIAN_POINT('Ctrl Pts',(17.0497148300457,-20.879896124347,13.6581753279346));
#148488=CARTESIAN_POINT('Ctrl Pts',(16.9864074383977,-20.8245883203866,
13.662345042255));
#148489=CARTESIAN_POINT('Ctrl Pts',(16.9258031063752,-20.7661379354358,
13.6665147565754));
#148490=CARTESIAN_POINT('Ctrl Pts',(16.8682208314237,-20.7048457131495,
13.6706844708957));
#148491=CARTESIAN_POINT('Ctrl Pts',(16.8106406054966,-20.6435556719036,
13.6748540368398));
#148492=CARTESIAN_POINT('Ctrl Pts',(16.7560825371937,-20.5794243302491,
13.6790236027838));
#148493=CARTESIAN_POINT('Ctrl Pts',(16.7048276747609,-20.512788158106,13.6831931687279));
#148494=CARTESIAN_POINT('Ctrl Pts',(16.6517707545947,-20.4438091403549,
13.6875093314668));
#148495=CARTESIAN_POINT('Ctrl Pts',(16.6022539651132,-20.3721462932498,
13.6918254942057));
#148496=CARTESIAN_POINT('Ctrl Pts',(16.5565412927829,-20.2982071082729,
13.6961416569446));
#148497=CARTESIAN_POINT('Ctrl Pts',(16.5123177059456,-20.2266764844696,
13.7003172211363));
#148498=CARTESIAN_POINT('Ctrl Pts',(16.4716543903427,-20.1530159839383,
13.704492785328));
#148499=CARTESIAN_POINT('Ctrl Pts',(16.4347434295141,-20.0776194841408,
13.7086683495197));
#148500=CARTESIAN_POINT('Ctrl Pts',(16.3959681838015,-19.9984148863766,
13.7130548115322));
#148501=CARTESIAN_POINT('Ctrl Pts',(16.3613345469612,-19.9172948468639,
13.7174412735447));
#148502=CARTESIAN_POINT('Ctrl Pts',(16.3310071212994,-19.8347373476376,
13.7218277355573));
#148503=CARTESIAN_POINT('Ctrl Pts',(16.3006796956376,-19.7521798484113,
13.7262141975698));
#148504=CARTESIAN_POINT('Ctrl Pts',(16.2746585801944,-19.668185466211,13.7306006595824));
#148505=CARTESIAN_POINT('Ctrl Pts',(16.253046772176,-19.5832456584798,13.7349871215949));
#148506=CARTESIAN_POINT('Ctrl Pts',(16.2263033450823,-19.4781373050522,
13.7404151277539));
#148507=CARTESIAN_POINT('Ctrl Pts',(16.2062281520528,-19.3712684537335,
13.745843133913));
#148508=CARTESIAN_POINT('Ctrl Pts',(16.193006541868,-19.2633715557504,13.751271140072));
#148509=CARTESIAN_POINT('Ctrl Pts',(16.1804712473274,-19.161075437704,13.7564173858787));
#148510=CARTESIAN_POINT('Ctrl Pts',(16.1740962693079,-19.0578550605845,
13.7615636316854));
#148511=CARTESIAN_POINT('Ctrl Pts',(16.1740010826188,-18.9543543591274,
13.7667098774921));
#148512=CARTESIAN_POINT('Ctrl Pts',(16.1744182719781,-18.9543537193378,
13.7667098902285));
#148513=CARTESIAN_POINT('Ctrl Pts',(16.1802301241212,-18.3145386211268,
13.7985275695778));
#148514=CARTESIAN_POINT('Ctrl Pts',(16.7471749526305,-16.8130883553205,
13.8727371844876));
#148515=CARTESIAN_POINT('Ctrl Pts',(19.2691669536258,-15.9725892909193,
13.9893387349578));
#148516=CARTESIAN_POINT('Ctrl Pts',(21.5288886261234,-17.7892922081608,
14.1165145416392));
#148517=CARTESIAN_POINT('Ctrl Pts',(21.2942515057879,-20.0117708843731,
14.2145391075549));
#148518=CARTESIAN_POINT('Ctrl Pts',(20.505242856169,-20.8199787376498,14.2701717379101));
#148519=CARTESIAN_POINT('Ctrl Pts',(20.2923704978253,-20.9805871927218,
14.2834124327049));
#148520=CARTESIAN_POINT('Origin',(18.734,-18.952,-1.76670989022851));
#148521=CARTESIAN_POINT('',(20.2935357468249,-20.9821350335323,15.1499553861536));
#148522=CARTESIAN_POINT('',(20.2935357468249,-20.9821350335323,15.0832685855196));
#148523=CARTESIAN_POINT('',(20.2935357468249,-20.9821350335323,-1.76670989022851));
#148524=CARTESIAN_POINT('',(16.1738766836434,-18.9531301832654,14.6332901097715));
#148525=CARTESIAN_POINT('Ctrl Pts',(16.1740002494514,-18.9531301287164,
14.6332901097715));
#148526=CARTESIAN_POINT('Ctrl Pts',(16.1739637014967,-18.8703406609987,
14.6374299052976));
#148527=CARTESIAN_POINT('Ctrl Pts',(16.1779474618949,-18.787387492894,14.6415697008237));
#148528=CARTESIAN_POINT('Ctrl Pts',(16.1859729132155,-18.7046986352396,
14.6457094963498));
#148529=CARTESIAN_POINT('Ctrl Pts',(16.1939875490477,-18.6221212131097,
14.6498437128863));
#148530=CARTESIAN_POINT('Ctrl Pts',(16.2060330170348,-18.5398078587028,
14.6539779294227));
#148531=CARTESIAN_POINT('Ctrl Pts',(16.2220786798974,-18.4581869973217,
14.6581121459591));
#148532=CARTESIAN_POINT('Ctrl Pts',(16.2381078732803,-18.3766499126678,
14.6622421190812));
#148533=CARTESIAN_POINT('Ctrl Pts',(16.2581290152451,-18.2958043686403,
14.6663720922033));
#148534=CARTESIAN_POINT('Ctrl Pts',(16.2820597821146,-18.2160725797227,
14.6705020653254));
#148535=CARTESIAN_POINT('Ctrl Pts',(16.3059775967093,-18.1363839447938,
14.6746298031431));
#148536=CARTESIAN_POINT('Ctrl Pts',(16.3338007023324,-18.0578083185529,
14.6787575409609));
#148537=CARTESIAN_POINT('Ctrl Pts',(16.3653962152435,-17.9807553805363,
14.6828852787787));
#148538=CARTESIAN_POINT('Ctrl Pts',(16.3969845852848,-17.9037198620533,
14.6870120834293));
#148539=CARTESIAN_POINT('Ctrl Pts',(16.4323434905918,-17.8282067834232,
14.69113888808));
#148540=CARTESIAN_POINT('Ctrl Pts',(16.4712914723378,-17.7546069488907,
14.6952656927306));
#148541=CARTESIAN_POINT('Ctrl Pts',(16.510242924153,-17.6810005569833,14.6993928650588));
#148542=CARTESIAN_POINT('Ctrl Pts',(16.5527838651356,-17.609308162424,14.703520037387));
#148543=CARTESIAN_POINT('Ctrl Pts',(16.5986870593953,-17.5398956675635,
14.7076472097152));
#148544=CARTESIAN_POINT('Ctrl Pts',(16.6446377721095,-17.4704113176929,
14.7117786544443));
#148545=CARTESIAN_POINT('Ctrl Pts',(16.6939574240315,-17.4032119705958,
14.7159100991734));
#148546=CARTESIAN_POINT('Ctrl Pts',(16.746376041612,-17.3386336435756,14.7200415439026));
#148547=CARTESIAN_POINT('Ctrl Pts',(16.7988250781874,-17.2740178411719,
14.7241753861462));
#148548=CARTESIAN_POINT('Ctrl Pts',(16.8543763437697,-17.2120264344659,
14.7283092283899));
#148549=CARTESIAN_POINT('Ctrl Pts',(16.9127219511753,-17.1529596255589,
14.7324430706335));
#148550=CARTESIAN_POINT('Ctrl Pts',(16.9711635405876,-17.0937956482256,
14.7365837132944));
#148551=CARTESIAN_POINT('Ctrl Pts',(17.0324082986517,-17.0375661867597,
14.7407243559553));
#148552=CARTESIAN_POINT('Ctrl Pts',(17.0961145829386,-16.9845317383557,
14.7448649986161));
#148553=CARTESIAN_POINT('Ctrl Pts',(17.1274705472736,-16.9584284066154,
14.7469030054635));
#148554=CARTESIAN_POINT('Ctrl Pts',(17.1594223751532,-16.9330984310461,
14.7489410123109));
#148555=CARTESIAN_POINT('Ctrl Pts',(17.1919269101816,-16.9085689182999,
14.7509790191583));
#148556=CARTESIAN_POINT('Ctrl Pts',(17.2586683911458,-16.8582025307613,
14.7551636535514));
#148557=CARTESIAN_POINT('Ctrl Pts',(17.3280042311001,-16.8110156651531,
14.7593482879444));
#148558=CARTESIAN_POINT('Ctrl Pts',(17.3995987737075,-16.767286433587,14.7635329223375));
#148559=CARTESIAN_POINT('Ctrl Pts',(17.4710914103451,-16.7236194451695,
14.7677116004214));
#148560=CARTESIAN_POINT('Ctrl Pts',(17.5448359744308,-16.6834005528598,
14.7718902785053));
#148561=CARTESIAN_POINT('Ctrl Pts',(17.6204652949934,-16.6468664982813,
14.7760689565893));
#148562=CARTESIAN_POINT('Ctrl Pts',(17.6974502167732,-16.6096775970311,
14.7803225344747));
#148563=CARTESIAN_POINT('Ctrl Pts',(17.7763877432994,-16.5763072247155,
14.7845761123602));
#148564=CARTESIAN_POINT('Ctrl Pts',(17.8568613993349,-16.5469578225687,
14.7888296902456));
#148565=CARTESIAN_POINT('Ctrl Pts',(17.9357749165169,-16.5181774158532,
14.7930008042235));
#148566=CARTESIAN_POINT('Ctrl Pts',(18.0161650809,-16.4932636267837,14.7971719182015));
#148567=CARTESIAN_POINT('Ctrl Pts',(18.0976177441666,-16.4723593759457,
14.8013430321794));
#148568=CARTESIAN_POINT('Ctrl Pts',(18.1790430752053,-16.451462139731,14.8055127464998));
#148569=CARTESIAN_POINT('Ctrl Pts',(18.2615297518284,-16.434571883947,14.8096824608202));
#148570=CARTESIAN_POINT('Ctrl Pts',(18.3446492988108,-16.4217814261445,
14.8138521751405));
#148571=CARTESIAN_POINT('Ctrl Pts',(18.4277658880431,-16.4089914234813,
14.8180217410846));
#148572=CARTESIAN_POINT('Ctrl Pts',(18.5115148480479,-16.4003009978601,
14.8221913070286));
#148573=CARTESIAN_POINT('Ctrl Pts',(18.5954597232801,-16.3957514612764,
14.8263608729727));
#148574=CARTESIAN_POINT('Ctrl Pts',(18.6823559967683,-16.3910419685989,
14.8306770357116));
#148575=CARTESIAN_POINT('Ctrl Pts',(18.7694616919212,-16.3907699986349,
14.8349931984505));
#148576=CARTESIAN_POINT('Ctrl Pts',(18.8562914526112,-16.3949226056652,
14.8393093611894));
#148577=CARTESIAN_POINT('Ctrl Pts',(18.9402927429795,-16.3989399419582,
14.8434849253811));
#148578=CARTESIAN_POINT('Ctrl Pts',(19.0240353356995,-16.4070979281598,
14.8476604895728));
#148579=CARTESIAN_POINT('Ctrl Pts',(19.1070857885139,-16.4193320402372,
14.8518360537645));
#148580=CARTESIAN_POINT('Ctrl Pts',(19.1943309222662,-16.4321840682319,
14.856222515777));
#148581=CARTESIAN_POINT('Ctrl Pts',(19.2808115861347,-16.4495346990029,
14.8606089777895));
#148582=CARTESIAN_POINT('Ctrl Pts',(19.3660405469235,-16.471249156597,14.8649954398021));
#148583=CARTESIAN_POINT('Ctrl Pts',(19.4512695077123,-16.4929636141912,
14.8693819018146));
#148584=CARTESIAN_POINT('Ctrl Pts',(19.5352462338659,-16.5190416538915,
14.8737683638271));
#148585=CARTESIAN_POINT('Ctrl Pts',(19.6175072439393,-16.549290082031,14.8781548258397));
#148586=CARTESIAN_POINT('Ctrl Pts',(19.6959833029992,-16.5781467351528,
14.8823394602327));
#148587=CARTESIAN_POINT('Ctrl Pts',(19.7731901646014,-16.6109058485357,
14.8865240946257));
#148588=CARTESIAN_POINT('Ctrl Pts',(19.848712296063,-16.6474357251303,14.8907087290188));
#148589=CARTESIAN_POINT('Ctrl Pts',(19.9241269311184,-16.683913605967,14.8948874071027));
#148590=CARTESIAN_POINT('Ctrl Pts',(19.9978611886366,-16.7241513904372,
14.8990660851867));
#148591=CARTESIAN_POINT('Ctrl Pts',(20.0695172636948,-16.7679684896108,
14.9032447632706));
#148592=CARTESIAN_POINT('Ctrl Pts',(20.1424577224,-16.8125709787961,14.9074983411561));
#148593=CARTESIAN_POINT('Ctrl Pts',(20.2132443104816,-16.860882196855,14.9117519190415));
#148594=CARTESIAN_POINT('Ctrl Pts',(20.281481376752,-16.9126615316221,14.9160054969269));
#148595=CARTESIAN_POINT('Ctrl Pts',(20.3483955343389,-16.9634370229456,
14.9201766109049));
#148596=CARTESIAN_POINT('Ctrl Pts',(20.4128577595142,-17.0175470676764,
14.9243477248828));
#148597=CARTESIAN_POINT('Ctrl Pts',(20.4745237080537,-17.074720792822,14.9285188388608));
#148598=CARTESIAN_POINT('Ctrl Pts',(20.5361689639887,-17.1318753327719,
14.9326885531812));
#148599=CARTESIAN_POINT('Ctrl Pts',(20.5950194697347,-17.1920911989055,
14.9368582675015));
#148600=CARTESIAN_POINT('Ctrl Pts',(20.6507652549076,-17.2550583517459,
14.9410279818219));
#148601=CARTESIAN_POINT('Ctrl Pts',(20.7065090564062,-17.3180232639449,
14.9451975477659));
#148602=CARTESIAN_POINT('Ctrl Pts',(20.75914805269,-17.3837389231869,14.94936711371));
#148603=CARTESIAN_POINT('Ctrl Pts',(20.8084112617999,-17.4518607008288,
14.953536679654));
#148604=CARTESIAN_POINT('Ctrl Pts',(20.8594065045693,-17.5223775561353,
14.957852842393));
#148605=CARTESIAN_POINT('Ctrl Pts',(20.9067838489651,-17.5954724488007,
14.9621690051319));
#148606=CARTESIAN_POINT('Ctrl Pts',(20.9502914662219,-17.6707302638585,
14.9664851678708));
#148607=CARTESIAN_POINT('Ctrl Pts',(20.9923818274227,-17.7435365635066,
14.9706607320625));
#148608=CARTESIAN_POINT('Ctrl Pts',(21.0308505291919,-17.8183665946339,
14.9748362962542));
#148609=CARTESIAN_POINT('Ctrl Pts',(21.0655172119571,-17.8948209752611,
14.9790118604458));
#148610=CARTESIAN_POINT('Ctrl Pts',(21.1019348264565,-17.9751368849007,
14.9833983224584));
#148611=CARTESIAN_POINT('Ctrl Pts',(21.1341560348915,-18.0572450047082,
14.9877847844709));
#148612=CARTESIAN_POINT('Ctrl Pts',(21.1620304324222,-18.1406626970047,
14.9921712464835));
#148613=CARTESIAN_POINT('Ctrl Pts',(21.1899048299529,-18.2240803893013,
14.996557708496));
#148614=CARTESIAN_POINT('Ctrl Pts',(21.2134323346265,-18.3088070746723,
15.0009441705086));
#148615=CARTESIAN_POINT('Ctrl Pts',(21.2325245180281,-18.3943484665022,
15.0053306325211));
#148616=CARTESIAN_POINT('Ctrl Pts',(21.25073824177,-18.4759539720913,15.0095152669141));
#148617=CARTESIAN_POINT('Ctrl Pts',(21.2649836214983,-18.5586046111965,
15.0136999013072));
#148618=CARTESIAN_POINT('Ctrl Pts',(21.2751464736302,-18.6418797014761,
15.0178845357002));
#148619=CARTESIAN_POINT('Ctrl Pts',(21.2852948602001,-18.725036259972,15.0220632137842));
#148620=CARTESIAN_POINT('Ctrl Pts',(21.2913722063418,-18.8088150514091,
15.0262418918681));
#148621=CARTESIAN_POINT('Ctrl Pts',(21.2933150345072,-18.8927838354387,
15.0304205699521));
#148622=CARTESIAN_POINT('Ctrl Pts',(21.2952926864712,-18.9782576995749,
15.0346741478375));
#148623=CARTESIAN_POINT('Ctrl Pts',(21.2929860350544,-19.0639279639717,
15.0389277257229));
#148624=CARTESIAN_POINT('Ctrl Pts',(21.2863832385264,-19.1493317097919,
15.0431813036084));
#148625=CARTESIAN_POINT('Ctrl Pts',(21.2799084500935,-19.2330797373477,
15.0473524175863));
#148626=CARTESIAN_POINT('Ctrl Pts',(21.2693026454397,-19.3165710082865,
15.0515235315643));
#148627=CARTESIAN_POINT('Ctrl Pts',(21.2546071988876,-19.3993693651963,
15.0556946455422));
#148628=CARTESIAN_POINT('Ctrl Pts',(21.2399166835345,-19.4821399383178,
15.0598643598626));
#148629=CARTESIAN_POINT('Ctrl Pts',(21.2211393320557,-19.5642176066098,
15.064034074183));
#148630=CARTESIAN_POINT('Ctrl Pts',(21.1983680574964,-19.6451739155445,
15.0682037885034));
#148631=CARTESIAN_POINT('Ctrl Pts',(21.1755975932368,-19.7261273437063,
15.0723733544474));
#148632=CARTESIAN_POINT('Ctrl Pts',(21.1488336138537,-19.8059590492309,
15.0765429203915));
#148633=CARTESIAN_POINT('Ctrl Pts',(21.1182192201024,-19.8842546382263,
15.0807124863355));
#148634=CARTESIAN_POINT('Ctrl Pts',(21.0865284620338,-19.9653030035426,
15.0850286490744));
#148635=CARTESIAN_POINT('Ctrl Pts',(21.0507116827588,-20.0447047315976,
15.0893448118133));
#148636=CARTESIAN_POINT('Ctrl Pts',(21.0109816181364,-20.1220233803941,
15.0936609745523));
#148637=CARTESIAN_POINT('Ctrl Pts',(20.9725457561902,-20.1968233823388,
15.0978365387439));
#148638=CARTESIAN_POINT('Ctrl Pts',(20.9304479207723,-20.2696735493081,
15.1020121029356));
#148639=CARTESIAN_POINT('Ctrl Pts',(20.884926303708,-20.3402060495536,15.1061876671273));
#148640=CARTESIAN_POINT('Ctrl Pts',(20.8371054979832,-20.4143009787113,
15.1105741291398));
#148641=CARTESIAN_POINT('Ctrl Pts',(20.7855062921192,-20.4858374838363,
15.1149605911524));
#148642=CARTESIAN_POINT('Ctrl Pts',(20.7304530967375,-20.5544278556389,
15.1193470531649));
#148643=CARTESIAN_POINT('Ctrl Pts',(20.6753999013558,-20.6230182274415,
15.1237335151775));
#148644=CARTESIAN_POINT('Ctrl Pts',(20.6168931592929,-20.6886620833861,
15.12811997719));
#148645=CARTESIAN_POINT('Ctrl Pts',(20.5553006227462,-20.7510175211999,
15.1325064392025));
#148646=CARTESIAN_POINT('Ctrl Pts',(20.4965457256971,-20.810500171771,15.1366908118296));
#148647=CARTESIAN_POINT('Ctrl Pts',(20.4347644264919,-20.8672121309936,
15.1408751844566));
#148648=CARTESIAN_POINT('Ctrl Pts',(20.3702485909567,-20.9208297408847,
15.1450595570836));
#148649=CARTESIAN_POINT('Ctrl Pts',(20.3450868338478,-20.9417410918058,
15.146691500107));
#148650=CARTESIAN_POINT('Ctrl Pts',(20.3195095726725,-20.9621821194541,
15.1483234431303));
#148651=CARTESIAN_POINT('Ctrl Pts',(20.2935357468249,-20.9821350335323,
15.1499553861536));
#148652=CARTESIAN_POINT('Ctrl Pts',(20.2947698132858,-20.9837129250579,
14.3497865232697));
#148653=CARTESIAN_POINT('Ctrl Pts',(20.1912477797316,-21.0647995005029,
14.3563415485511));
#148654=CARTESIAN_POINT('Ctrl Pts',(19.3719149991153,-21.60811723892,14.405288509393));
#148655=CARTESIAN_POINT('Ctrl Pts',(17.2895133775451,-21.6122159629899,
14.4966274057954));
#148656=CARTESIAN_POINT('Ctrl Pts',(16.2008983314107,-19.9284205945985,
14.5845735760146));
#148657=CARTESIAN_POINT('Ctrl Pts',(16.1700292378907,-19.0164624118087,
14.6301278106733));
#148658=CARTESIAN_POINT('Ctrl Pts',(16.1703790167221,-18.9531317273334,
14.6332901097715));
#148659=CARTESIAN_POINT('',(16.1743645121285,-18.9514398261319,14.566709915053));
#148660=CARTESIAN_POINT('Ctrl Pts',(20.2923704978253,-20.9805871927218,
14.2834124327049));
#148661=CARTESIAN_POINT('Ctrl Pts',(19.8237022393519,-21.3341891611517,
14.3125636734706));
#148662=CARTESIAN_POINT('Ctrl Pts',(18.3750627815534,-21.8243382151095,
14.3841068497969));
#148663=CARTESIAN_POINT('Ctrl Pts',(16.5197423660721,-20.7321305462553,
14.478539335638));
#148664=CARTESIAN_POINT('Ctrl Pts',(16.1790023713152,-19.4133917175901,
14.5438205807135));
#148665=CARTESIAN_POINT('Ctrl Pts',(16.1781028623508,-18.9514411453429,
14.5667098902285));
#148666=CARTESIAN_POINT('Ctrl Pts',(16.1740000613162,-18.9514396975223,
14.5667099174731));
#148667=CARTESIAN_POINT('Ctrl Pts',(16.1740197372988,-18.8615409084374,
14.571157199272));
#148668=CARTESIAN_POINT('Ctrl Pts',(16.1787790795978,-18.7717655181971,
14.575604481071));
#148669=CARTESIAN_POINT('Ctrl Pts',(16.1882138900512,-18.6826060832318,
14.58005176287));
#148670=CARTESIAN_POINT('Ctrl Pts',(16.1976832329536,-18.5931203148802,
14.5845153222119));
#148671=CARTESIAN_POINT('Ctrl Pts',(16.211862232535,-18.504255369482,14.5889788815538));
#148672=CARTESIAN_POINT('Ctrl Pts',(16.23063522025,-18.4164957707849,14.5934424408956));
#148673=CARTESIAN_POINT('Ctrl Pts',(16.2494446598934,-18.3285657673207,
14.5979146672301));
#148674=CARTESIAN_POINT('Ctrl Pts',(16.2728657964755,-18.241745739755,14.6023868935646));
#148675=CARTESIAN_POINT('Ctrl Pts',(16.3007333122773,-18.1565044145825,
14.606859119899));
#148676=CARTESIAN_POINT('Ctrl Pts',(16.3286838403159,-18.0710091710796,
14.6113446681784));
#148677=CARTESIAN_POINT('Ctrl Pts',(16.3611071025136,-17.9871023685302,
14.6158302164579));
#148678=CARTESIAN_POINT('Ctrl Pts',(16.3977895032111,-17.9052333045547,
14.6203157647373));
#148679=CARTESIAN_POINT('Ctrl Pts',(16.4111522146039,-17.8754099382236,
14.6219497659465));
#148680=CARTESIAN_POINT('Ctrl Pts',(16.4250796827618,-17.8458567318514,
14.6235837671557));
#148681=CARTESIAN_POINT('Ctrl Pts',(16.4395601204677,-17.8165945045,14.625217768365));
#148682=CARTESIAN_POINT('Ctrl Pts',(16.4766441429939,-17.7416547050056,
14.629402402758));
#148683=CARTESIAN_POINT('Ctrl Pts',(16.5174725051856,-17.6683941847451,
14.6335870371511));
#148684=CARTESIAN_POINT('Ctrl Pts',(16.5618698248529,-17.5972120083883,
14.6377716715441));
#148685=CARTESIAN_POINT('Ctrl Pts',(16.6062039504309,-17.526131151049,14.6419503496281));
#148686=CARTESIAN_POINT('Ctrl Pts',(16.6540967016935,-17.4571231485616,
14.646129027712));
#148687=CARTESIAN_POINT('Ctrl Pts',(16.7053259809371,-17.3905642106128,
14.6503077057959));
#148688=CARTESIAN_POINT('Ctrl Pts',(16.7574735081934,-17.3228122515363,
14.6545612836814));
#148689=CARTESIAN_POINT('Ctrl Pts',(16.8130781406444,-17.2575984516733,
14.6588148615668));
#148690=CARTESIAN_POINT('Ctrl Pts',(16.8718583319471,-17.1952904599505,
14.6630684394522));
#148691=CARTESIAN_POINT('Ctrl Pts',(16.9294989545412,-17.1341904302313,
14.6672395534302));
#148692=CARTESIAN_POINT('Ctrl Pts',(16.9901927757376,-17.0758848946116,
14.6714106674081));
#148693=CARTESIAN_POINT('Ctrl Pts',(17.0536336491124,-17.0206872529793,
14.6755817813861));
#148694=CARTESIAN_POINT('Ctrl Pts',(17.1170532342894,-16.9655081334488,
14.6797514957065));
#148695=CARTESIAN_POINT('Ctrl Pts',(17.1832176941668,-16.9134351384329,
14.6839212100268));
#148696=CARTESIAN_POINT('Ctrl Pts',(17.2517856166926,-16.8647433023424,
14.6880909243472));
#148697=CARTESIAN_POINT('Ctrl Pts',(17.3203510992775,-16.8160531989163,
14.6922604902913));
#148698=CARTESIAN_POINT('Ctrl Pts',(17.3913194988899,-16.7707442808557,
14.6964300562353));
#148699=CARTESIAN_POINT('Ctrl Pts',(17.4643191824368,-16.7290491185112,
14.7005996221793));
#148700=CARTESIAN_POINT('Ctrl Pts',(17.5398854448024,-16.6858880056951,
14.7049157849183));
#148701=CARTESIAN_POINT('Ctrl Pts',(17.6176280306768,-16.6465997576134,
14.7092319476572));
#148702=CARTESIAN_POINT('Ctrl Pts',(17.6971072733112,-16.6113903628884,
14.7135481103961));
#148703=CARTESIAN_POINT('Ctrl Pts',(17.7739974879764,-16.5773279104931,
14.7177236745878));
#148704=CARTESIAN_POINT('Ctrl Pts',(17.8525124972025,-16.5470827802973,
14.7218992387795));
#148705=CARTESIAN_POINT('Ctrl Pts',(17.9322359204945,-16.5207915842498,
14.7260748029711));
#148706=CARTESIAN_POINT('Ctrl Pts',(18.0159859843727,-16.4931724823913,
14.7304612649837));
#148707=CARTESIAN_POINT('Ctrl Pts',(18.1010691812454,-16.4699173921691,
14.7348477269962));
#148708=CARTESIAN_POINT('Ctrl Pts',(18.1869895560292,-16.4511242385542,
14.7392341890088));
#148709=CARTESIAN_POINT('Ctrl Pts',(18.272909930813,-16.4323310849393,14.7436206510213));
#148710=CARTESIAN_POINT('Ctrl Pts',(18.3596668986516,-16.4179998874471,
14.7480071130339));
#148711=CARTESIAN_POINT('Ctrl Pts',(18.446759550604,-16.4081657042506,14.7523935750464));
#148712=CARTESIAN_POINT('Ctrl Pts',(18.5298449405377,-16.3987840064008,
14.7565782094394));
#148713=CARTESIAN_POINT('Ctrl Pts',(18.6135450624313,-16.3934596676543,
14.7607628438325));
#148714=CARTESIAN_POINT('Ctrl Pts',(18.6974294349979,-16.3922612254811,
14.7649474782255));
#148715=CARTESIAN_POINT('Ctrl Pts',(18.7811944085429,-16.3910644891421,
14.7691261563095));
#148716=CARTESIAN_POINT('Ctrl Pts',(18.8651426557822,-16.3939819908556,
14.7733048343934));
#148717=CARTESIAN_POINT('Ctrl Pts',(18.9488376266314,-16.4010306167687,
14.7774835124774));
#148718=CARTESIAN_POINT('Ctrl Pts',(19.0340327696825,-16.4082055842356,
14.7817370903628));
#148719=CARTESIAN_POINT('Ctrl Pts',(19.1189649879801,-16.4196612875147,
14.7859906682482));
#148720=CARTESIAN_POINT('Ctrl Pts',(19.2031727512631,-16.4353599920783,
14.7902442461337));
#148721=CARTESIAN_POINT('Ctrl Pts',(19.285747982737,-16.4507543466204,14.7944153601116));
#148722=CARTESIAN_POINT('Ctrl Pts',(19.3676261254063,-16.4702285646622,
14.7985864740896));
#148723=CARTESIAN_POINT('Ctrl Pts',(19.4483779483093,-16.493694862925,14.8027575880675));
#148724=CARTESIAN_POINT('Ctrl Pts',(19.5291026741582,-16.5171532868448,
14.8069273023879));
#148725=CARTESIAN_POINT('Ctrl Pts',(19.6087013894598,-16.5446010022893,
14.8110970167083));
#148726=CARTESIAN_POINT('Ctrl Pts',(19.6867580339315,-16.5758998066624,
14.8152667310286));
#148727=CARTESIAN_POINT('Ctrl Pts',(19.7648119008129,-16.6071974972898,
14.8194362969727));
#148728=CARTESIAN_POINT('Ctrl Pts',(19.8413233792982,-16.6423458323765,
14.8236058629167));
#148729=CARTESIAN_POINT('Ctrl Pts',(19.9158957565829,-16.6811582132233,
14.8277754288608));
#148730=CARTESIAN_POINT('Ctrl Pts',(19.993090006658,-16.7213351895004,14.8320915915997));
#148731=CARTESIAN_POINT('Ctrl Pts',(20.0682057930236,-16.7654384176637,
14.8364077543386));
#148732=CARTESIAN_POINT('Ctrl Pts',(20.1408319285747,-16.8132097052907,
14.8407239170775));
#148733=CARTESIAN_POINT('Ctrl Pts',(20.2110922753992,-16.8594248482479,
14.8448994812692));
#148734=CARTESIAN_POINT('Ctrl Pts',(20.2790223288375,-16.9090724304067,
14.8490750454609));
#148735=CARTESIAN_POINT('Ctrl Pts',(20.3442818409952,-16.9618762871215,
14.8532506096526));
#148736=CARTESIAN_POINT('Ctrl Pts',(20.4128374559721,-17.0173471411098,
14.8576370716651));
#148737=CARTESIAN_POINT('Ctrl Pts',(20.4784452273879,-17.0763011057023,
14.8620235336777));
#148738=CARTESIAN_POINT('Ctrl Pts',(20.5407543647586,-17.13837416609,14.8664099956902));
#148739=CARTESIAN_POINT('Ctrl Pts',(20.6030635021293,-17.2004472264776,
14.8707964577027));
#148740=CARTESIAN_POINT('Ctrl Pts',(20.6620736724741,-17.2656389014522,
14.8751829197153));
#148741=CARTESIAN_POINT('Ctrl Pts',(20.7174842649081,-17.3335469821889,
14.8795693817278));
#148742=CARTESIAN_POINT('Ctrl Pts',(20.770345333846,-17.398330511467,14.8837540161209));
#148743=CARTESIAN_POINT('Ctrl Pts',(20.8201275486196,-17.4658271045687,
14.8879386505139));
#148744=CARTESIAN_POINT('Ctrl Pts',(20.866540268707,-17.5357118928893,14.892123284907));
#148745=CARTESIAN_POINT('Ctrl Pts',(20.912886926032,-17.6054972088638,14.8963019629909));
#148746=CARTESIAN_POINT('Ctrl Pts',(20.9558733628218,-17.6776635880367,
14.9004806410749));
#148747=CARTESIAN_POINT('Ctrl Pts',(20.9952490842181,-17.7518531010236,
14.9046593191588));
#148748=CARTESIAN_POINT('Ctrl Pts',(21.0353305871216,-17.8273724077116,
14.9089128970442));
#148749=CARTESIAN_POINT('Ctrl Pts',(21.0716703524657,-17.9049877173954,
14.9131664749297));
#148750=CARTESIAN_POINT('Ctrl Pts',(21.1040502914402,-17.9842905311797,
14.9174200528151));
#148751=CARTESIAN_POINT('Ctrl Pts',(21.1358024821133,-18.0620559051722,
14.9215911667931));
#148752=CARTESIAN_POINT('Ctrl Pts',(21.1637468322872,-18.1414434905284,
14.925762280771));
#148753=CARTESIAN_POINT('Ctrl Pts',(21.1877248192283,-18.222044856513,14.929933394749));
#148754=CARTESIAN_POINT('Ctrl Pts',(21.2116947601243,-18.3026191759307,
14.9341031090694));
#148755=CARTESIAN_POINT('Ctrl Pts',(21.2317008500143,-18.3844060265126,
14.9382728233897));
#148756=CARTESIAN_POINT('Ctrl Pts',(21.2476340898709,-18.46698076096,14.9424425377101));
#148757=CARTESIAN_POINT('Ctrl Pts',(21.2635667627544,-18.5495525570439,
14.9466121036542));
#148758=CARTESIAN_POINT('Ctrl Pts',(21.2754267874402,-18.6329117293876,
14.9507816695982));
#148759=CARTESIAN_POINT('Ctrl Pts',(21.2831563307877,-18.7166237029669,
14.9549512355422));
#148760=CARTESIAN_POINT('Ctrl Pts',(21.2911576353439,-18.8032788862672,
14.9592673982812));
#148761=CARTESIAN_POINT('Ctrl Pts',(21.2947325504218,-18.8903116161907,
14.9635835610201));
#148762=CARTESIAN_POINT('Ctrl Pts',(21.2938756072079,-18.9772363947924,
14.967899723759));
#148763=CARTESIAN_POINT('Ctrl Pts',(21.293046578829,-19.0613296078741,14.9720752879507));
#148764=CARTESIAN_POINT('Ctrl Pts',(21.2880700686645,-19.1453213272334,
14.9762508521424));
#148765=CARTESIAN_POINT('Ctrl Pts',(21.2789941177451,-19.2287759755517,
14.9804264163341));
#148766=CARTESIAN_POINT('Ctrl Pts',(21.2694597621209,-19.3164457197619,
14.9848128783466));
#148767=CARTESIAN_POINT('Ctrl Pts',(21.2554010498833,-19.4035221357511,
14.9891993403591));
#148768=CARTESIAN_POINT('Ctrl Pts',(21.2369341836446,-19.4895132299242,
14.9935858023717));
#148769=CARTESIAN_POINT('Ctrl Pts',(21.2184673174058,-19.5755043240972,
14.9979722643842));
#148770=CARTESIAN_POINT('Ctrl Pts',(21.1955925215497,-19.6604095560011,
15.0023587263968));
#148771=CARTESIAN_POINT('Ctrl Pts',(21.1684852750765,-19.7437584514458,
15.0067451884093));
#148772=CARTESIAN_POINT('Ctrl Pts',(21.1426284959746,-19.8232624313143,
15.0109293012962));
#148773=CARTESIAN_POINT('Ctrl Pts',(21.112824919157,-19.9016463915127,15.0151134141831));
#148774=CARTESIAN_POINT('Ctrl Pts',(21.0791903430324,-19.9784902605226,
15.01929752707));
#148775=CARTESIAN_POINT('Ctrl Pts',(21.0456010518522,-20.0552306684295,
15.023476006548));
#148776=CARTESIAN_POINT('Ctrl Pts',(21.0081911857059,-20.1304346847173,
15.027654486026));
#148777=CARTESIAN_POINT('Ctrl Pts',(20.967126087575,-20.2036979975186,15.031832965504));
#148778=CARTESIAN_POINT('Ctrl Pts',(20.9250013387184,-20.2788518092133,
15.036119267172));
#148779=CARTESIAN_POINT('Ctrl Pts',(20.8790302479734,-20.3519629039354,
15.0404055688399));
#148780=CARTESIAN_POINT('Ctrl Pts',(20.8294436809226,-20.422617482584,15.0446918705079));
#148781=CARTESIAN_POINT('Ctrl Pts',(20.7811918137342,-20.4913702829484,
15.0488627996751));
#148782=CARTESIAN_POINT('Ctrl Pts',(20.7295169285826,-20.5577967390327,
15.0530337288422));
#148783=CARTESIAN_POINT('Ctrl Pts',(20.6746769388215,-20.6215427575017,
15.0572046580094));
#148784=CARTESIAN_POINT('Ctrl Pts',(20.6175615471624,-20.6879337037333,
15.0615486459278));
#148785=CARTESIAN_POINT('Ctrl Pts',(20.5570129676201,-20.751416498399,15.0658926338461));
#148786=CARTESIAN_POINT('Ctrl Pts',(20.4933694474881,-20.811628765976,15.0702366217645));
#148787=CARTESIAN_POINT('Ctrl Pts',(20.4297259273561,-20.871841033553,15.0745806096829));
#148788=CARTESIAN_POINT('Ctrl Pts',(20.3629878766118,-20.9287823858972,
15.0789245976012));
#148789=CARTESIAN_POINT('Ctrl Pts',(20.2935357468249,-20.9821350335323,
15.0832685855196));
#148790=CARTESIAN_POINT('Origin',(18.734,-18.952,-1.76670989022851));
#148791=CARTESIAN_POINT('',(20.2935357468249,-20.9821350335323,15.9499155251885));
#148792=CARTESIAN_POINT('',(20.2954006447972,-20.9845255200926,15.8832287071313));
#148793=CARTESIAN_POINT('',(20.2935357468249,-20.9821350335323,-1.76670989022851));
#148794=CARTESIAN_POINT('',(16.174000571626,-18.9537107672549,15.4332901097416));
#148795=CARTESIAN_POINT('Ctrl Pts',(16.1740005716256,-18.9537107666516,
15.4332901097715));
#148796=CARTESIAN_POINT('Ctrl Pts',(16.1739440307447,-18.8691027211111,
15.437482057942));
#148797=CARTESIAN_POINT('Ctrl Pts',(16.1780862675835,-18.7844696898645,
15.4416740061124));
#148798=CARTESIAN_POINT('Ctrl Pts',(16.1864081330308,-18.7002547332075,
15.4458659542829));
#148799=CARTESIAN_POINT('Ctrl Pts',(16.1947304086796,-18.6160356254258,
15.4500581090829));
#148800=CARTESIAN_POINT('Ctrl Pts',(16.2072326772703,-18.5322350838834,
15.4542502638829));
#148801=CARTESIAN_POINT('Ctrl Pts',(16.2238439368849,-18.4492908009531,
15.4584424186829));
#148802=CARTESIAN_POINT('Ctrl Pts',(16.2404607969944,-18.3663185533138,
15.4626359868701));
#148803=CARTESIAN_POINT('Ctrl Pts',(16.2611893110379,-18.2842035816671,
15.4668295550574));
#148804=CARTESIAN_POINT('Ctrl Pts',(16.2859076895265,-18.2033718951305,
15.4710231232446));
#148805=CARTESIAN_POINT('Ctrl Pts',(16.3106584247114,-18.122434398808,15.4752221808701));
#148806=CARTESIAN_POINT('Ctrl Pts',(16.3394093150966,-18.0427839738199,
15.4794212384956));
#148807=CARTESIAN_POINT('Ctrl Pts',(16.3719892689075,-17.9648296468169,
15.4836202961211));
#148808=CARTESIAN_POINT('Ctrl Pts',(16.4045936038559,-17.8868169828627,
15.4878224961022));
#148809=CARTESIAN_POINT('Ctrl Pts',(16.4410325111314,-17.8105033515335,
15.4920246960833));
#148810=CARTESIAN_POINT('Ctrl Pts',(16.4810885578785,-17.7362738655611,
15.4962268960645));
#148811=CARTESIAN_POINT('Ctrl Pts',(16.5212156880346,-17.6619126520384,
15.5004365532643));
#148812=CARTESIAN_POINT('Ctrl Pts',(16.5649725361192,-17.5896433529152,
15.5046462104641));
#148813=CARTESIAN_POINT('Ctrl Pts',(16.612098119287,-17.5198224940229,15.5088558676639));
#148814=CARTESIAN_POINT('Ctrl Pts',(16.6314200308983,-17.4911953158863,
15.5105818648582));
#148815=CARTESIAN_POINT('Ctrl Pts',(16.6513077816386,-17.4629793510679,
15.5123078620525));
#148816=CARTESIAN_POINT('Ctrl Pts',(16.6717415022699,-17.4351974787271,
15.5140338592469));
#148817=CARTESIAN_POINT('Ctrl Pts',(16.7212825156696,-17.3678410665133,
15.5182184936399));
#148818=CARTESIAN_POINT('Ctrl Pts',(16.7742191330187,-17.3027889832897,
15.522403128033));
#148819=CARTESIAN_POINT('Ctrl Pts',(16.8303093008605,-17.2404037502934,
15.526587762426));
#148820=CARTESIAN_POINT('Ctrl Pts',(16.8863196312909,-17.1781073149545,
15.53076644051));
#148821=CARTESIAN_POINT('Ctrl Pts',(16.9454742913219,-17.1184705290969,
15.5349451185939));
#148822=CARTESIAN_POINT('Ctrl Pts',(17.0074891937055,-17.0618252896231,
15.5391237966778));
#148823=CARTESIAN_POINT('Ctrl Pts',(17.070615668645,-17.004164724942,15.5433773745633));
#148824=CARTESIAN_POINT('Ctrl Pts',(17.1367056485332,-16.949604396855,15.5476309524487));
#148825=CARTESIAN_POINT('Ctrl Pts',(17.2054179892121,-16.8984574422974,
15.5518845303342));
#148826=CARTESIAN_POINT('Ctrl Pts',(17.272798207086,-16.8483020712589,15.5560556443121));
#148827=CARTESIAN_POINT('Ctrl Pts',(17.3426996279386,-16.8014291923403,
15.5602267582901));
#148828=CARTESIAN_POINT('Ctrl Pts',(17.4147663076937,-16.7580942442566,
15.564397872268));
#148829=CARTESIAN_POINT('Ctrl Pts',(17.4868088047783,-16.7147738376334,
15.5685675865884));
#148830=CARTESIAN_POINT('Ctrl Pts',(17.5610147238612,-16.6749892409427,
15.5727373009088));
#148831=CARTESIAN_POINT('Ctrl Pts',(17.6370000578043,-16.6389519834594,
15.5769070152291));
#148832=CARTESIAN_POINT('Ctrl Pts',(17.7129826878632,-16.6029160083363,
15.5810765811732));
#148833=CARTESIAN_POINT('Ctrl Pts',(17.7907441908667,-16.5706273036551,
15.5852461471172));
#148834=CARTESIAN_POINT('Ctrl Pts',(17.8698781766136,-16.5422503295265,
15.5894157130613));
#148835=CARTESIAN_POINT('Ctrl Pts',(17.951794415677,-16.5128756559943,15.5937318758002));
#148836=CARTESIAN_POINT('Ctrl Pts',(18.0351809497172,-16.4876930819298,
15.5980480385391));
#148837=CARTESIAN_POINT('Ctrl Pts',(18.1195690084031,-16.4668290689441,
15.602364201278));
#148838=CARTESIAN_POINT('Ctrl Pts',(18.2012081349533,-16.4466446989869,
15.6065397654697));
#148839=CARTESIAN_POINT('Ctrl Pts',(18.2837840674898,-16.4305019005907,
15.6107153296614));
#148840=CARTESIAN_POINT('Ctrl Pts',(18.3668630221883,-16.4184628600466,
15.6148908938531));
#148841=CARTESIAN_POINT('Ctrl Pts',(18.4541380973871,-16.4058157561848,
15.6192773558656));
#148842=CARTESIAN_POINT('Ctrl Pts',(18.5419677640929,-16.3976979204099,
15.6236638178781));
#148843=CARTESIAN_POINT('Ctrl Pts',(18.6298465962985,-16.3941196141146,
15.6280502798907));
#148844=CARTESIAN_POINT('Ctrl Pts',(18.7177254285042,-16.3905413078192,
15.6324367419032));
#148845=CARTESIAN_POINT('Ctrl Pts',(18.8056528468588,-16.391502448601,15.6368232039158));
#148846=CARTESIAN_POINT('Ctrl Pts',(18.8931294701919,-16.3969505265619,
15.6412096659283));
#148847=CARTESIAN_POINT('Ctrl Pts',(18.9765811644139,-16.4021479303798,
15.6453943003213));
#148848=CARTESIAN_POINT('Ctrl Pts',(19.0599332586381,-16.4114477893304,
15.6495789347144));
#148849=CARTESIAN_POINT('Ctrl Pts',(19.1427499109294,-16.4248428006325,
15.6537635691074));
#148850=CARTESIAN_POINT('Ctrl Pts',(19.2254486839666,-16.4382187457938,
15.6579422471914));
#148851=CARTESIAN_POINT('Ctrl Pts',(19.3076130786645,-16.4556781923683,
15.6621209252753));
#148852=CARTESIAN_POINT('Ctrl Pts',(19.3888102512128,-16.4771619174365,
15.6662996033592));
#148853=CARTESIAN_POINT('Ctrl Pts',(19.4714628247241,-16.4990307228366,
15.6705531812447));
#148854=CARTESIAN_POINT('Ctrl Pts',(19.5531126789041,-16.5250694661815,
15.6748067591301));
#148855=CARTESIAN_POINT('Ctrl Pts',(19.633311860283,-16.5551607943055,15.6790603370155));
#148856=CARTESIAN_POINT('Ctrl Pts',(19.7119562240349,-16.5846687433154,
15.6832314509935));
#148857=CARTESIAN_POINT('Ctrl Pts',(19.7892052107338,-16.6180733757685,
15.6874025649714));
#148858=CARTESIAN_POINT('Ctrl Pts',(19.8646513710665,-16.6552136631577,
15.6915736789494));
#148859=CARTESIAN_POINT('Ctrl Pts',(19.9400722147116,-16.6923414877648,
15.6957433932698));
#148860=CARTESIAN_POINT('Ctrl Pts',(20.0136910210525,-16.733202274758,15.6999131075901));
#148861=CARTESIAN_POINT('Ctrl Pts',(20.085122071664,-16.7775876316893,15.7040828219105));
#148862=CARTESIAN_POINT('Ctrl Pts',(20.1565505804521,-16.8219714091991,
15.7082523878546));
#148863=CARTESIAN_POINT('Ctrl Pts',(20.2257910980031,-16.8698792637602,
15.7124219537986));
#148864=CARTESIAN_POINT('Ctrl Pts',(20.2924853680819,-16.9210585046647,
15.7165915197426));
#148865=CARTESIAN_POINT('Ctrl Pts',(20.3615245264204,-16.974037144543,15.7209076824816));
#148866=CARTESIAN_POINT('Ctrl Pts',(20.4278346353052,-17.03052117375,15.7252238452205));
#148867=CARTESIAN_POINT('Ctrl Pts',(20.4910556240452,-17.0901848818932,
15.7295400079594));
#148868=CARTESIAN_POINT('Ctrl Pts',(20.5522171957265,-17.147905051019,15.7337155721511));
#148869=CARTESIAN_POINT('Ctrl Pts',(20.61048752063,-17.2086005517579,15.7378911363428));
#148870=CARTESIAN_POINT('Ctrl Pts',(20.6655795109694,-17.2719403008216,
15.7420667005344));
#148871=CARTESIAN_POINT('Ctrl Pts',(20.7234540667722,-17.3384791900349,
15.746453162547));
#148872=CARTESIAN_POINT('Ctrl Pts',(20.7778204147501,-17.4079360098505,
15.7508396245595));
#148873=CARTESIAN_POINT('Ctrl Pts',(20.8283963491844,-17.4798913312792,
15.7552260865721));
#148874=CARTESIAN_POINT('Ctrl Pts',(20.8789722836188,-17.5518466527079,
15.7596125485847));
#148875=CARTESIAN_POINT('Ctrl Pts',(20.9257575602052,-17.6262999440045,
15.7639990105972));
#148876=CARTESIAN_POINT('Ctrl Pts',(20.9685260259021,-17.7028028820213,
15.7683854726098));
#148877=CARTESIAN_POINT('Ctrl Pts',(21.009326651094,-17.7757858064551,15.7725701070028));
#148878=CARTESIAN_POINT('Ctrl Pts',(21.0466238491571,-17.850905564207,15.7767547413958));
#148879=CARTESIAN_POINT('Ctrl Pts',(21.0801878476018,-17.9277917283259,
15.7809393757889));
#148880=CARTESIAN_POINT('Ctrl Pts',(21.1137040718491,-18.0045684545068,
15.7851180538728));
#148881=CARTESIAN_POINT('Ctrl Pts',(21.1434974687763,-18.0831061749367,
15.7892967319568));
#148882=CARTESIAN_POINT('Ctrl Pts',(21.1693835453415,-18.1630088802274,
15.7934754100407));
#148883=CARTESIAN_POINT('Ctrl Pts',(21.195733611225,-18.2443437840853,15.7977289879262));
#148884=CARTESIAN_POINT('Ctrl Pts',(21.218034666248,-18.3270926679897,15.8019825658116));
#148885=CARTESIAN_POINT('Ctrl Pts',(21.2361429171342,-18.41081535292,15.806236143697));
#148886=CARTESIAN_POINT('Ctrl Pts',(21.2539001042416,-18.4929149102316,
15.810407257675));
#148887=CARTESIAN_POINT('Ctrl Pts',(21.2676255061034,-18.575950377106,15.8145783716529));
#148888=CARTESIAN_POINT('Ctrl Pts',(21.2772339776254,-18.6594919914747,
15.8187494856309));
#148889=CARTESIAN_POINT('Ctrl Pts',(21.2868392249321,-18.7430055726479,
15.8229191999513));
#148890=CARTESIAN_POINT('Ctrl Pts',(21.2923302330118,-18.8270245073654,
15.8270889142716));
#148891=CARTESIAN_POINT('Ctrl Pts',(21.2936734448665,-18.9111116685929,
15.831258628592));
#148892=CARTESIAN_POINT('Ctrl Pts',(21.295016608924,-18.9951958376384,15.8354281945361));
#148893=CARTESIAN_POINT('Ctrl Pts',(21.2922122637205,-19.0793477683789,
15.8395977604801));
#148894=CARTESIAN_POINT('Ctrl Pts',(21.285278964847,-19.1631294473286,15.8437673264242));
#148895=CARTESIAN_POINT('Ctrl Pts',(21.2781018997383,-19.2498567867541,
15.8480834891631));
#148896=CARTESIAN_POINT('Ctrl Pts',(21.2665001742353,-19.3361868282292,
15.852399651902));
#148897=CARTESIAN_POINT('Ctrl Pts',(21.2505527597975,-19.4216405084271,
15.8567158146409));
#148898=CARTESIAN_POINT('Ctrl Pts',(21.2351248307076,-19.5043105439807,
15.8608913788326));
#148899=CARTESIAN_POINT('Ctrl Pts',(21.2156301415435,-19.5861599891146,
15.8650669430243));
#148900=CARTESIAN_POINT('Ctrl Pts',(21.1921916857819,-19.6667682393284,
15.8692425072159));
#148901=CARTESIAN_POINT('Ctrl Pts',(21.1675694093395,-19.7514478206324,
15.8736289692285));
#148902=CARTESIAN_POINT('Ctrl Pts',(21.1385946886758,-19.8347569748338,
15.878015431241));
#148903=CARTESIAN_POINT('Ctrl Pts',(21.1054674445918,-19.9162313826263,
15.8824018932535));
#148904=CARTESIAN_POINT('Ctrl Pts',(21.0723402005077,-19.9977057904188,
15.8867883552661));
#148905=CARTESIAN_POINT('Ctrl Pts',(21.0350607478796,-20.0773449585575,
15.8911748172786));
#148906=CARTESIAN_POINT('Ctrl Pts',(20.9938836431737,-20.1547160593073,
15.8955612792911));
#148907=CARTESIAN_POINT('Ctrl Pts',(20.9545971350275,-20.2285347602967,
15.8997463422483));
#148908=CARTESIAN_POINT('Ctrl Pts',(20.9116167922609,-20.3005638940076,
15.9039314052055));
#148909=CARTESIAN_POINT('Ctrl Pts',(20.8651297737826,-20.3704096331094,
15.9081164681627));
#148910=CARTESIAN_POINT('Ctrl Pts',(20.8187208419206,-20.4401380487601,
15.9122945012561));
#148911=CARTESIAN_POINT('Ctrl Pts',(20.7688171985821,-20.5076899820961,
15.9164725343495));
#148912=CARTESIAN_POINT('Ctrl Pts',(20.7156518556524,-20.5726961229637,
15.920650567443));
#148913=CARTESIAN_POINT('Ctrl Pts',(20.6625380463667,-20.6376392527956,
15.9248245507314));
#148914=CARTESIAN_POINT('Ctrl Pts',(20.6061691036063,-20.7000411350043,
15.9289985340199));
#148915=CARTESIAN_POINT('Ctrl Pts',(20.546820818089,-20.7595620823372,15.9331725173083));
#148916=CARTESIAN_POINT('Ctrl Pts',(20.4875162743664,-20.8190391606174,
15.9373434242228));
#148917=CARTESIAN_POINT('Ctrl Pts',(20.4252370755883,-20.8756391988914,
15.9415143311373));
#148918=CARTESIAN_POINT('Ctrl Pts',(20.3602977399997,-20.9290573236181,
15.9456852380518));
#148919=CARTESIAN_POINT('Ctrl Pts',(20.3383431194471,-20.9471168656256,
15.947095333764));
#148920=CARTESIAN_POINT('Ctrl Pts',(20.3160847638627,-20.9648130339878,
15.9485054294762));
#148921=CARTESIAN_POINT('Ctrl Pts',(20.2935357468249,-20.9821350335323,
15.9499155251885));
#148922=CARTESIAN_POINT('Ctrl Pts',(20.2935357468249,-20.9821350335323,
15.1499553861536));
#148923=CARTESIAN_POINT('Ctrl Pts',(20.2270593471735,-21.0332017457777,
15.1541321176549));
#148924=CARTESIAN_POINT('Ctrl Pts',(20.157982906757,-21.081068370004,15.1583088491561));
#148925=CARTESIAN_POINT('Ctrl Pts',(20.086648755646,-21.1254629842372,15.1624855806574));
#148926=CARTESIAN_POINT('Ctrl Pts',(20.015384561649,-21.1698140608515,15.166658216055));
#148927=CARTESIAN_POINT('Ctrl Pts',(19.9418674462888,-21.2106996525442,
15.1708308514525));
#148928=CARTESIAN_POINT('Ctrl Pts',(19.8664701158255,-21.2478901186168,
15.1750034868501));
#148929=CARTESIAN_POINT('Ctrl Pts',(19.7911123063922,-21.2850610905572,
15.1791739350767));
#148930=CARTESIAN_POINT('Ctrl Pts',(19.7138766504389,-21.318540579423,15.1833443833033));
#148931=CARTESIAN_POINT('Ctrl Pts',(19.6351609242639,-21.3481446092796,
15.1875148315299));
#148932=CARTESIAN_POINT('Ctrl Pts',(19.5564628454869,-21.3777420021639,
15.1916843447775));
#148933=CARTESIAN_POINT('Ctrl Pts',(19.4762857860939,-21.403465500195,15.195853858025));
#148934=CARTESIAN_POINT('Ctrl Pts',(19.3950467213204,-21.4251795794547,
15.2000233712725));
#148935=CARTESIAN_POINT('Ctrl Pts',(19.3138015000959,-21.4468953042486,
15.2041932004937));
#148936=CARTESIAN_POINT('Ctrl Pts',(19.2314945584613,-21.464600889432,15.2083630297148));
#148937=CARTESIAN_POINT('Ctrl Pts',(19.1485558905415,-21.4782112765201,
15.212532858936));
#148938=CARTESIAN_POINT('Ctrl Pts',(19.0655304261605,-21.4918359070663,
15.216707051941));
#148939=CARTESIAN_POINT('Ctrl Pts',(18.9818723702625,-21.5013567070332,
15.220881244946));
#148940=CARTESIAN_POINT('Ctrl Pts',(18.8980192295312,-21.5067402397003,
15.2250554379511));
#148941=CARTESIAN_POINT('Ctrl Pts',(18.8141207480157,-21.5121266833329,
15.2292318880115));
#148942=CARTESIAN_POINT('Ctrl Pts',(18.7300274318276,-21.513371398164,15.2334083380719));
#148943=CARTESIAN_POINT('Ctrl Pts',(18.6461767539422,-21.5104931263249,
15.2375847881324));
#148944=CARTESIAN_POINT('Ctrl Pts',(18.5621802082572,-21.5076098474043,
15.2417685036031));
#148945=CARTESIAN_POINT('Ctrl Pts',(18.4784276028385,-21.5005892941992,
15.2459522190739));
#148946=CARTESIAN_POINT('Ctrl Pts',(18.3953510434448,-21.4895020954128,
15.2501359345446));
#148947=CARTESIAN_POINT('Ctrl Pts',(18.3321636121995,-21.4810692520676,
15.2533180383244));
#148948=CARTESIAN_POINT('Ctrl Pts',(18.2693671652201,-21.4702849264138,
15.2565001421042));
#148949=CARTESIAN_POINT('Ctrl Pts',(18.20714644876,-21.4571996598167,15.259682245884));
#148950=CARTESIAN_POINT('Ctrl Pts',(18.125322923169,-21.4399918437196,15.263866880277));
#148951=CARTESIAN_POINT('Ctrl Pts',(18.0441910630359,-21.41873907309,15.2680515146701));
#148952=CARTESIAN_POINT('Ctrl Pts',(17.9641810754837,-21.3935115857715,
15.2722361490631));
#148953=CARTESIAN_POINT('Ctrl Pts',(17.8842849722453,-21.3683200066586,
15.2764148271471));
#148954=CARTESIAN_POINT('Ctrl Pts',(17.8055080047354,-21.3391650856198,
15.280593505231));
#148955=CARTESIAN_POINT('Ctrl Pts',(17.728269907104,-21.3061680017032,15.284772183315));
#148956=CARTESIAN_POINT('Ctrl Pts',(17.6496473720827,-21.2725794687721,
15.2890257612004));
#148957=CARTESIAN_POINT('Ctrl Pts',(17.5726198898779,-21.2350097758299,
15.2932793390859));
#148958=CARTESIAN_POINT('Ctrl Pts',(17.4976137413827,-21.1936398059239,
15.2975329169713));
#148959=CARTESIAN_POINT('Ctrl Pts',(17.4240617334387,-21.1530718736114,
15.3017040309492));
#148960=CARTESIAN_POINT('Ctrl Pts',(17.3524538049873,-21.1088499333756,
15.3058751449272));
#148961=CARTESIAN_POINT('Ctrl Pts',(17.2831698439507,-21.0611922288634,
15.3100462589051));
#148962=CARTESIAN_POINT('Ctrl Pts',(17.2139091318162,-21.0135505163542,
15.3142159732255));
#148963=CARTESIAN_POINT('Ctrl Pts',(17.1469712170494,-20.9624755897518,
15.3183856875459));
#148964=CARTESIAN_POINT('Ctrl Pts',(17.0827076373574,-20.9082294172919,
15.3225554018663));
#148965=CARTESIAN_POINT('Ctrl Pts',(17.0184463444393,-20.8539851751436,
15.3267249678103));
#148966=CARTESIAN_POINT('Ctrl Pts',(16.9568595483704,-20.7965702088949,
15.3308945337544));
#148967=CARTESIAN_POINT('Ctrl Pts',(16.8982652087742,-20.7362863492957,
15.3350640996984));
#148968=CARTESIAN_POINT('Ctrl Pts',(16.8376107644816,-20.6738829835612,
15.3393802624373));
#148969=CARTESIAN_POINT('Ctrl Pts',(16.7801634890496,-20.6084056085283,
15.3436964251763));
#148970=CARTESIAN_POINT('Ctrl Pts',(16.7262325806843,-20.5402285698017,
15.3480125879152));
#148971=CARTESIAN_POINT('Ctrl Pts',(16.6740584659864,-20.4742723909407,
15.3521881521069));
#148972=CARTESIAN_POINT('Ctrl Pts',(16.6251753803869,-20.4057901412944,
15.3563637162985));
#148973=CARTESIAN_POINT('Ctrl Pts',(16.5798195291698,-20.335150931422,15.3605392804902));
#148974=CARTESIAN_POINT('Ctrl Pts',(16.532172861731,-20.2609439029878,15.3649257425028));
#148975=CARTESIAN_POINT('Ctrl Pts',(16.488419403819,-20.1843567987727,15.3693122045153));
#148976=CARTESIAN_POINT('Ctrl Pts',(16.4487777573746,-20.1058454410405,
15.3736986665278));
#148977=CARTESIAN_POINT('Ctrl Pts',(16.4091361109301,-20.0273340833083,
15.3780851285404));
#148978=CARTESIAN_POINT('Ctrl Pts',(16.3736064408137,-19.9468990335382,
15.3824715905529));
#148979=CARTESIAN_POINT('Ctrl Pts',(16.3423477078172,-19.8650166007783,
15.3868580525655));
#148980=CARTESIAN_POINT('Ctrl Pts',(16.3083133302778,-19.7758633510063,
15.3916340140292));
#148981=CARTESIAN_POINT('Ctrl Pts',(16.2792349760223,-19.6847190703936,
15.396409975493));
#148982=CARTESIAN_POINT('Ctrl Pts',(16.2553188691393,-19.5921092496716,
15.4011859369567));
#148983=CARTESIAN_POINT('Ctrl Pts',(16.2315006236314,-19.4998783754247,
15.405942355852));
#148984=CARTESIAN_POINT('Ctrl Pts',(16.212802591162,-19.406194112186,15.4106987747473));
#148985=CARTESIAN_POINT('Ctrl Pts',(16.1993817363336,-19.3115973546745,
15.4154551936426));
#148986=CARTESIAN_POINT('Ctrl Pts',(16.1860549755609,-19.2176638181479,
15.4201782651282));
#148987=CARTESIAN_POINT('Ctrl Pts',(16.1779317634136,-19.1228307363238,
15.4249013366138));
#148988=CARTESIAN_POINT('Ctrl Pts',(16.1751178968034,-19.0276464271479,
15.4296244080995));
#148989=CARTESIAN_POINT('Ctrl Pts',(16.1743899245164,-19.0030214008619,
15.4308463086469));
#148990=CARTESIAN_POINT('Ctrl Pts',(16.1740170525925,-18.9783729560401,
15.4320682091942));
#148991=CARTESIAN_POINT('Ctrl Pts',(16.174000571626,-18.9537107672549,15.4332901097416));
#148992=CARTESIAN_POINT('',(16.1740008768645,-18.949881145288,15.3667098902285));
#148993=CARTESIAN_POINT('Ctrl Pts',(20.2935357468249,-20.9821350335323,
15.0832685855196));
#148994=CARTESIAN_POINT('Ctrl Pts',(20.2260494149554,-21.03397756875,15.0874896196505));
#148995=CARTESIAN_POINT('Ctrl Pts',(20.156001045364,-21.0824316029258,15.0917106537815));
#148996=CARTESIAN_POINT('Ctrl Pts',(20.0837719873172,-21.1272506941164,
15.0959316879124));
#148997=CARTESIAN_POINT('Ctrl Pts',(20.0123180971675,-21.1715887833167,
15.1001074215751));
#148998=CARTESIAN_POINT('Ctrl Pts',(19.9387305383576,-21.2123694058899,
15.1042831552377));
#148999=CARTESIAN_POINT('Ctrl Pts',(19.8634030839696,-21.2494004165404,
15.1084588889004));
#149000=CARTESIAN_POINT('Ctrl Pts',(19.7868498441635,-21.2870340238569,
15.1127025732655));
#149001=CARTESIAN_POINT('Ctrl Pts',(19.7085000337302,-21.3207947028272,
15.1169462576305));
#149002=CARTESIAN_POINT('Ctrl Pts',(19.6287860118066,-21.350532466546,15.1211899419956));
#149003=CARTESIAN_POINT('Ctrl Pts',(19.549071989883,-21.3802702302648,15.1254336263606));
#149004=CARTESIAN_POINT('Ctrl Pts',(19.4679942448969,-21.4059849931164,
15.1296773107257));
#149005=CARTESIAN_POINT('Ctrl Pts',(19.3859971465586,-21.4275806835729,
15.1339209950908));
#149006=CARTESIAN_POINT('Ctrl Pts',(19.3051410205324,-21.4488758745561,
15.1381056294838));
#149007=CARTESIAN_POINT('Ctrl Pts',(19.2230900288836,-21.4662452083819,
15.1422902638769));
#149008=CARTESIAN_POINT('Ctrl Pts',(19.1402602214101,-21.4795586308728,
15.1464748982699));
#149009=CARTESIAN_POINT('Ctrl Pts',(19.0575483119153,-21.4928531033548,
15.1506535763538));
#149010=CARTESIAN_POINT('Ctrl Pts',(18.974060238839,-21.5021030592902,15.1548322544378));
#149011=CARTESIAN_POINT('Ctrl Pts',(18.8902255244996,-21.5072286757734,
15.1590109325217));
#149012=CARTESIAN_POINT('Ctrl Pts',(18.8048881331567,-21.5124461652484,
15.1632645104072));
#149013=CARTESIAN_POINT('Ctrl Pts',(18.7191920174691,-21.5133898805874,
15.1675180882926));
#149014=CARTESIAN_POINT('Ctrl Pts',(18.6335993142633,-21.510030434202,15.171771666178));
#149015=CARTESIAN_POINT('Ctrl Pts',(18.5496659926296,-21.5067361172402,
15.175942780156));
#149016=CARTESIAN_POINT('Ctrl Pts',(18.4658325904026,-21.4993040188572,
15.1801138941339));
#149017=CARTESIAN_POINT('Ctrl Pts',(18.3825365202413,-21.4877589440631,
15.1842850081119));
#149018=CARTESIAN_POINT('Ctrl Pts',(18.2992684008808,-21.4762177433303,
15.1884547224323));
#149019=CARTESIAN_POINT('Ctrl Pts',(18.2165377107911,-21.4605663702896,
15.1926244367526));
#149020=CARTESIAN_POINT('Ctrl Pts',(18.1347761196902,-21.4408814237055,
15.196794151073));
#149021=CARTESIAN_POINT('Ctrl Pts',(18.0530174380175,-21.4211971775963,
15.200963717017));
#149022=CARTESIAN_POINT('Ctrl Pts',(17.9722282338226,-21.3974797518311,
15.2051332829611));
#149023=CARTESIAN_POINT('Ctrl Pts',(17.8928280294726,-21.3698564299807,
15.2093028489051));
#149024=CARTESIAN_POINT('Ctrl Pts',(17.8106362118883,-21.3412619062111,
15.213619011644));
#149025=CARTESIAN_POINT('Ctrl Pts',(17.729933384083,-21.3084818866878,15.217935174383));
#149026=CARTESIAN_POINT('Ctrl Pts',(17.6511637413075,-21.2717124039115,
15.2222513371219));
#149027=CARTESIAN_POINT('Ctrl Pts',(17.5749600113602,-21.2361406831691,
15.2264269013136));
#149028=CARTESIAN_POINT('Ctrl Pts',(17.5005658480113,-21.1968356830554,
15.2306024655052));
#149029=CARTESIAN_POINT('Ctrl Pts',(17.4283578509295,-21.1540214755017,
15.2347780296969));
#149030=CARTESIAN_POINT('Ctrl Pts',(17.3525027995735,-21.1090448241056,
15.2391644917095));
#149031=CARTESIAN_POINT('Ctrl Pts',(17.2790610511148,-21.0601954720667,
15.243550953722));
#149032=CARTESIAN_POINT('Ctrl Pts',(17.2084323379748,-21.007782894321,15.2479374157345));
#149033=CARTESIAN_POINT('Ctrl Pts',(17.1378036248349,-20.9553703165754,
15.252323877747));
#149034=CARTESIAN_POINT('Ctrl Pts',(17.0699883460669,-20.8993949411349,
15.2567103397596));
#149035=CARTESIAN_POINT('Ctrl Pts',(17.0053421035814,-20.8402112903883,
15.2610968017721));
#149036=CARTESIAN_POINT('Ctrl Pts',(16.9445899812057,-20.7845927075508,
15.2652190348167));
#149037=CARTESIAN_POINT('Ctrl Pts',(16.8863955977248,-20.7259204795934,
15.2693412678613));
#149038=CARTESIAN_POINT('Ctrl Pts',(16.8310887538618,-20.6644627847987,
15.2734635009059));
#149039=CARTESIAN_POINT('Ctrl Pts',(16.7758743514522,-20.6031078121671,
15.2775788439313));
#149040=CARTESIAN_POINT('Ctrl Pts',(16.7235382140149,-20.5389769727691,
15.2816941869567));
#149041=CARTESIAN_POINT('Ctrl Pts',(16.6743754759298,-20.4723771965696,
15.2858095299821));
#149042=CARTESIAN_POINT('Ctrl Pts',(16.6252589923643,-20.4058400804408,
15.2899210011073));
#149043=CARTESIAN_POINT('Ctrl Pts',(16.5793102664141,-20.336839014796,15.2940324722326));
#149044=CARTESIAN_POINT('Ctrl Pts',(16.5367853878613,-20.2657153223604,
15.2981439433578));
#149045=CARTESIAN_POINT('Ctrl Pts',(16.4942868717937,-20.1946357216976,
15.3022528656552));
#149046=CARTESIAN_POINT('Ctrl Pts',(16.4552082342186,-20.1214365120742,
15.3063617879525));
#149047=CARTESIAN_POINT('Ctrl Pts',(16.4197623875945,-20.0464881330228,
15.3104707102498));
#149048=CARTESIAN_POINT('Ctrl Pts',(16.3843271437787,-19.971562173052,15.3145784034577));
#149049=CARTESIAN_POINT('Ctrl Pts',(16.3525227351499,-19.894888512104,15.3186860966657));
#149050=CARTESIAN_POINT('Ctrl Pts',(16.3245154961056,-19.8168609284116,
15.3227937898736));
#149051=CARTESIAN_POINT('Ctrl Pts',(16.2964946934766,-19.7387955568548,
15.3269034723902));
#149052=CARTESIAN_POINT('Ctrl Pts',(16.272274898332,-19.6593753990486,15.3310131549069));
#149053=CARTESIAN_POINT('Ctrl Pts',(16.2519734104534,-19.5790119686126,
15.3351228374235));
#149054=CARTESIAN_POINT('Ctrl Pts',(16.231666738396,-19.4986280166076,15.3392335693868));
#149055=CARTESIAN_POINT('Ctrl Pts',(16.2152804642378,-19.4173007774467,
15.3433443013501));
#149056=CARTESIAN_POINT('Ctrl Pts',(16.2028808242122,-19.3354523672626,
15.3474550333134));
#149057=CARTESIAN_POINT('Ctrl Pts',(16.1904661338132,-19.2535046115225,
15.3515707547805));
#149058=CARTESIAN_POINT('Ctrl Pts',(16.1820477886731,-19.1710348943536,
15.3556864762476));
#149059=CARTESIAN_POINT('Ctrl Pts',(16.1776401048971,-19.0884700945614,
15.3598021977147));
#149060=CARTESIAN_POINT('Ctrl Pts',(16.1751742007241,-19.04227873994,15.362104761886));
#149061=CARTESIAN_POINT('Ctrl Pts',(16.173962657598,-18.9960576424388,15.3644073260572));
#149062=CARTESIAN_POINT('Ctrl Pts',(16.1740008768645,-18.949881145288,15.3667098902285));
#149063=CARTESIAN_POINT('Ctrl Pts',(16.1723624843679,-18.9498797892267,
15.3667098902285));
#149064=CARTESIAN_POINT('Ctrl Pts',(16.1710770695818,-18.8056440598866,
15.3738974629702));
#149065=CARTESIAN_POINT('Ctrl Pts',(16.2478506876061,-17.8120819459935,
15.4234769712724));
#149066=CARTESIAN_POINT('Ctrl Pts',(17.5479306946412,-16.1669449835732,
15.515448415135));
#149067=CARTESIAN_POINT('Ctrl Pts',(20.4337937048959,-16.4472059560846,
15.6426242218164));
#149068=CARTESIAN_POINT('Ctrl Pts',(21.7124086028558,-18.932560808362,15.7652176524819));
#149069=CARTESIAN_POINT('Ctrl Pts',(20.8926534809929,-20.5182931343282,
15.8454191475868));
#149070=CARTESIAN_POINT('Ctrl Pts',(20.2954006447972,-20.9845255200926,
15.8832287071313));
#149071=CARTESIAN_POINT('Origin',(18.734,-18.952,-1.76670989022851));
#149072=CARTESIAN_POINT('',(20.2935357468249,-20.9821350335323,16.7498176655673));
#149073=CARTESIAN_POINT('',(20.2935357468249,-20.9821350335323,16.6833822574076));
#149074=CARTESIAN_POINT('',(20.2935357468249,-20.9821350335323,-1.76670989022851));
#149075=CARTESIAN_POINT('',(16.1740007055014,-18.9500994299064,16.2332901098004));
#149076=CARTESIAN_POINT('Ctrl Pts',(16.1740007055014,-18.9500994299065,
16.2332901098004));
#149077=CARTESIAN_POINT('Ctrl Pts',(16.1740727513108,-18.8530563258851,
16.2381006886061));
#149078=CARTESIAN_POINT('Ctrl Pts',(16.1796667621363,-18.7562381388328,
16.2429112674118));
#149079=CARTESIAN_POINT('Ctrl Pts',(16.1906824963738,-18.6602191305988,
16.2477218462176));
#149080=CARTESIAN_POINT('Ctrl Pts',(16.2018903455192,-18.5625255464786,
16.2526163217372));
#149081=CARTESIAN_POINT('Ctrl Pts',(16.2187106399962,-18.465659449398,16.2575107972569));
#149082=CARTESIAN_POINT('Ctrl Pts',(16.2409867483463,-18.3702054253614,
16.2624052727765));
#149083=CARTESIAN_POINT('Ctrl Pts',(16.2632628566963,-18.2747514013248,
16.2672997482962));
#149084=CARTESIAN_POINT('Ctrl Pts',(16.2909946214078,-18.1807095711099,
16.2721942238158));
#149085=CARTESIAN_POINT('Ctrl Pts',(16.3239764935689,-18.088642195582,16.2770886993355));
#149086=CARTESIAN_POINT('Ctrl Pts',(16.3521750361989,-18.0099272639074,
16.2812733337285));
#149087=CARTESIAN_POINT('Ctrl Pts',(16.3842865295797,-17.9324488089606,
16.2854579681216));
#149088=CARTESIAN_POINT('Ctrl Pts',(16.4201827606336,-17.8566234515881,
16.2896426025146));
#149089=CARTESIAN_POINT('Ctrl Pts',(16.4560278978456,-17.7809060222267,
16.2938212805986));
#149090=CARTESIAN_POINT('Ctrl Pts',(16.4956468770877,-17.7068374289188,
16.2979999586825));
#149091=CARTESIAN_POINT('Ctrl Pts',(16.5388624466768,-17.6348169747563,
16.3021786367664));
#149092=CARTESIAN_POINT('Ctrl Pts',(16.5828526242923,-17.561505605713,16.3064322146519));
#149093=CARTESIAN_POINT('Ctrl Pts',(16.6305694356435,-17.4903169777092,
16.3106857925373));
#149094=CARTESIAN_POINT('Ctrl Pts',(16.6817755898823,-17.4216487427662,
16.3149393704227));
#149095=CARTESIAN_POINT('Ctrl Pts',(16.7319890129005,-17.3543117755527,
16.3191104844007));
#149096=CARTESIAN_POINT('Ctrl Pts',(16.7855574030481,-17.289398733779,16.3232815983786));
#149097=CARTESIAN_POINT('Ctrl Pts',(16.8422127801053,-17.2272562176824,
16.3274527123566));
#149098=CARTESIAN_POINT('Ctrl Pts',(16.8988491459036,-17.1651345541072,
16.331622426677));
#149099=CARTESIAN_POINT('Ctrl Pts',(16.9585701316816,-17.1057819095285,
16.3357921409973));
#149100=CARTESIAN_POINT('Ctrl Pts',(17.0210683042877,-17.0495108394989,
16.3399618553177));
#149101=CARTESIAN_POINT('Ctrl Pts',(17.0835642529406,-16.9932417718355,
16.3441314212617));
#149102=CARTESIAN_POINT('Ctrl Pts',(17.1488368494855,-16.9400543678788,
16.3483009872058));
#149103=CARTESIAN_POINT('Ctrl Pts',(17.2165437463576,-16.8902224857465,
16.3524705531498));
#149104=CARTESIAN_POINT('Ctrl Pts',(17.2866311341982,-16.8386385761127,
16.3567867158888));
#149105=CARTESIAN_POINT('Ctrl Pts',(17.3593267625534,-16.790650851497,16.3611028786277));
#149106=CARTESIAN_POINT('Ctrl Pts',(17.4342176396319,-16.7465146076938,
16.3654190413666));
#149107=CARTESIAN_POINT('Ctrl Pts',(17.5066689542667,-16.7038160973902,
16.3695946055583));
#149108=CARTESIAN_POINT('Ctrl Pts',(17.5811742544606,-16.664722174367,16.37377016975));
#149109=CARTESIAN_POINT('Ctrl Pts',(17.6573356824289,-16.6294165359951,
16.3779457339416));
#149110=CARTESIAN_POINT('Ctrl Pts',(17.7373438430673,-16.5923276937602,
16.3823321959542));
#149111=CARTESIAN_POINT('Ctrl Pts',(17.8191792885611,-16.5594201038736,
16.3867186579667));
#149112=CARTESIAN_POINT('Ctrl Pts',(17.902360657527,-16.5308482071437,16.3911051199793));
#149113=CARTESIAN_POINT('Ctrl Pts',(17.985542026493,-16.5022763104139,16.3954915819918));
#149114=CARTESIAN_POINT('Ctrl Pts',(18.0700687402227,-16.4780401936422,
16.3998780440043));
#149115=CARTESIAN_POINT('Ctrl Pts',(18.155447269861,-16.4582324209244,16.4042645060169));
#149116=CARTESIAN_POINT('Ctrl Pts',(18.2368974067893,-16.4393360331914,
16.4084491404099));
#149117=CARTESIAN_POINT('Ctrl Pts',(18.3194258684926,-16.4243990992031,
16.412633774803));
#149118=CARTESIAN_POINT('Ctrl Pts',(18.4026129434635,-16.4135393210136,
16.416818409196));
#149119=CARTESIAN_POINT('Ctrl Pts',(18.4856816119296,-16.4026950003742,
16.42099708728));
#149120=CARTESIAN_POINT('Ctrl Pts',(18.5694065793229,-16.3959163673419,
16.4251757653639));
#149121=CARTESIAN_POINT('Ctrl Pts',(18.6533561519601,-16.393270516492,16.4293544434479));
#149122=CARTESIAN_POINT('Ctrl Pts',(18.7388104603535,-16.390577240667,16.4336080213333));
#149123=CARTESIAN_POINT('Ctrl Pts',(18.8244970356235,-16.392166473525,16.4378615992187));
#149124=CARTESIAN_POINT('Ctrl Pts',(18.9099530743146,-16.3980539325116,
16.4421151771042));
#149125=CARTESIAN_POINT('Ctrl Pts',(18.993752380942,-16.4038272516174,16.4462862910821));
#149126=CARTESIAN_POINT('Ctrl Pts',(19.0773295299442,-16.4137335920112,
16.4504574050601));
#149127=CARTESIAN_POINT('Ctrl Pts',(19.1602480327619,-16.4277352328714,
16.454628519038));
#149128=CARTESIAN_POINT('Ctrl Pts',(19.2431387114752,-16.4417321753459,
16.4587982333584));
#149129=CARTESIAN_POINT('Ctrl Pts',(19.3253707297098,-16.4598216125358,
16.4629679476788));
#149130=CARTESIAN_POINT('Ctrl Pts',(19.4065148699749,-16.4819142222055,
16.4671376619991));
#149131=CARTESIAN_POINT('Ctrl Pts',(19.4876561227832,-16.5040060457254,
16.4713072279432));
#149132=CARTESIAN_POINT('Ctrl Pts',(19.5677091309388,-16.5301006368244,
16.4754767938872));
#149133=CARTESIAN_POINT('Ctrl Pts',(19.6462583168597,-16.5600583695833,
16.4796463598313));
#149134=CARTESIAN_POINT('Ctrl Pts',(19.7275691952567,-16.5910693792692,
16.4839625225702));
#149135=CARTESIAN_POINT('Ctrl Pts',(19.8072680422835,-16.626220053208,16.4882786853091));
#149136=CARTESIAN_POINT('Ctrl Pts',(19.8849166499546,-16.6653013174322,
16.492594848048));
#149137=CARTESIAN_POINT('Ctrl Pts',(19.9600358623981,-16.7031095135849,
16.4967704122397));
#149138=CARTESIAN_POINT('Ctrl Pts',(20.0332359708034,-16.7445958812711,
16.5009459764314));
#149139=CARTESIAN_POINT('Ctrl Pts',(20.1041471618793,-16.7895253169588,
16.5051215406231));
#149140=CARTESIAN_POINT('Ctrl Pts',(20.178639908641,-16.8367240316335,16.5095080026356));
#149141=CARTESIAN_POINT('Ctrl Pts',(20.2506059585104,-16.88772243629,16.5138944646482));
#149142=CARTESIAN_POINT('Ctrl Pts',(20.3196548994213,-16.9421993780623,
16.5182809266607));
#149143=CARTESIAN_POINT('Ctrl Pts',(20.3887038403321,-16.9966763198345,
16.5226673886732));
#149144=CARTESIAN_POINT('Ctrl Pts',(20.4548352860544,-17.0546313591046,
16.5270538506858));
#149145=CARTESIAN_POINT('Ctrl Pts',(20.5177042670234,-17.115699619397,16.5314403126983));
#149146=CARTESIAN_POINT('Ctrl Pts',(20.5776805529838,-17.1739580385085,
16.5356249470914));
#149147=CARTESIAN_POINT('Ctrl Pts',(20.6349112416909,-17.2352663353223,
16.5398095814844));
#149148=CARTESIAN_POINT('Ctrl Pts',(20.6890701824651,-17.2993353087707,
16.5439942158775));
#149149=CARTESIAN_POINT('Ctrl Pts',(20.7431520346907,-17.3633130879656,
16.5481728939614));
#149150=CARTESIAN_POINT('Ctrl Pts',(20.7941705292093,-17.4300433902867,
16.5523515720454));
#149151=CARTESIAN_POINT('Ctrl Pts',(20.8418355824981,-17.4991995466841,
16.5565302501293));
#149152=CARTESIAN_POINT('Ctrl Pts',(20.8903549976109,-17.5695952774834,
16.5607838280147));
#149153=CARTESIAN_POINT('Ctrl Pts',(20.9353992222982,-17.6425043486948,
16.5650374059002));
#149154=CARTESIAN_POINT('Ctrl Pts',(20.9767045339425,-17.7175461234077,
16.5692909837856));
#149155=CARTESIAN_POINT('Ctrl Pts',(21.01720906152,-17.7911330668859,16.5734620977636));
#149156=CARTESIAN_POINT('Ctrl Pts',(21.0541181225501,-17.8667703369927,
16.5776332117415));
#149157=CARTESIAN_POINT('Ctrl Pts',(21.0872271712957,-17.9440704983604,
16.5818043257195));
#149158=CARTESIAN_POINT('Ctrl Pts',(21.1203251099803,-18.0213447209124,
16.5859740400398));
#149159=CARTESIAN_POINT('Ctrl Pts',(21.149625387836,-18.1002803040063,16.5901437543602));
#149160=CARTESIAN_POINT('Ctrl Pts',(21.1749707834401,-18.1804679952253,
16.5943134686806));
#149161=CARTESIAN_POINT('Ctrl Pts',(21.2003152771464,-18.2606528330222,
16.5984830346246));
#149162=CARTESIAN_POINT('Ctrl Pts',(21.2217050305798,-18.3420892514567,
16.6026526005687));
#149163=CARTESIAN_POINT('Ctrl Pts',(21.2390325027794,-18.4243522386871,
16.6068221665127));
#149164=CARTESIAN_POINT('Ctrl Pts',(21.2569691875258,-18.5095074910661,
16.6111383292517));
#149165=CARTESIAN_POINT('Ctrl Pts',(21.2705525077454,-18.5955480019175,
16.6154544919906));
#149166=CARTESIAN_POINT('Ctrl Pts',(21.2797210678871,-18.6819921399001,
16.6197706547295));
#149167=CARTESIAN_POINT('Ctrl Pts',(21.2885909631465,-18.7656203691803,
16.6239462189212));
#149168=CARTESIAN_POINT('Ctrl Pts',(21.2933293236125,-18.8496258601582,
16.6281217831129));
#149169=CARTESIAN_POINT('Ctrl Pts',(21.2939336612287,-18.9335704012973,
16.6322973473045));
#149170=CARTESIAN_POINT('Ctrl Pts',(21.2945685225012,-19.0217547816502,
16.6366838093171));
#149171=CARTESIAN_POINT('Ctrl Pts',(21.2906407927078,-19.1098713098954,
16.6410702713296));
#149172=CARTESIAN_POINT('Ctrl Pts',(21.2822091879386,-19.197417877314,16.6454567333422));
#149173=CARTESIAN_POINT('Ctrl Pts',(21.2737775831694,-19.2849644447327,
16.6498431953547));
#149174=CARTESIAN_POINT('Ctrl Pts',(21.2608422640144,-19.3719404886095,
16.6542296573672));
#149175=CARTESIAN_POINT('Ctrl Pts',(21.2435233083642,-19.4578584434176,
16.6586161193798));
#149176=CARTESIAN_POINT('Ctrl Pts',(21.2270051786282,-19.5398035648691,
16.6627997520461));
#149177=CARTESIAN_POINT('Ctrl Pts',(21.2064383857991,-19.6210912295844,
16.6669833847125));
#149178=CARTESIAN_POINT('Ctrl Pts',(21.1818895089887,-19.7012909660358,
16.6711670173788));
#149179=CARTESIAN_POINT('Ctrl Pts',(21.1573729381804,-19.7813851606791,
16.675345144439));
#149180=CARTESIAN_POINT('Ctrl Pts',(21.1288848202252,-19.8603938336786,
16.6795232714993));
#149181=CARTESIAN_POINT('Ctrl Pts',(21.0965427533342,-19.9378964137616,
16.6837013985596));
#149182=CARTESIAN_POINT('Ctrl Pts',(21.0642335424449,-20.0153202597021,
16.6878752810998));
#149183=CARTESIAN_POINT('Ctrl Pts',(21.0280783340562,-20.0912406291167,
16.6920491636401));
#149184=CARTESIAN_POINT('Ctrl Pts',(20.9882441729195,-20.1652531511843,
16.6962230461803));
#149185=CARTESIAN_POINT('Ctrl Pts',(20.9484385271419,-20.2392126912487,
16.7003939408389));
#149186=CARTESIAN_POINT('Ctrl Pts',(20.904959378607,-20.311266693636,16.7045648354975));
#149187=CARTESIAN_POINT('Ctrl Pts',(20.8580208517639,-20.3810330371521,
16.708735730156));
#149188=CARTESIAN_POINT('Ctrl Pts',(20.8110938747831,-20.4507822137115,
16.7129055985093));
#149189=CARTESIAN_POINT('Ctrl Pts',(20.7607094614786,-20.5182444646023,
16.7170754668626));
#149190=CARTESIAN_POINT('Ctrl Pts',(20.7071258294298,-20.5830654374479,
16.7212453352159));
#149191=CARTESIAN_POINT('Ctrl Pts',(20.65354927458,-20.6478778488932,16.7254146528228));
#149192=CARTESIAN_POINT('Ctrl Pts',(20.596774638736,-20.710049325155,16.7295839704298));
#149193=CARTESIAN_POINT('Ctrl Pts',(20.5371002850679,-20.7692587493222,
16.7337532880367));
#149194=CARTESIAN_POINT('Ctrl Pts',(20.4773989743808,-20.8284949204833,
16.7379244890721));
#149195=CARTESIAN_POINT('Ctrl Pts',(20.4147956627455,-20.8847660496243,
16.7420956901075));
#149196=CARTESIAN_POINT('Ctrl Pts',(20.3496246776639,-20.9377887352192,
16.7462668911429));
#149197=CARTESIAN_POINT('Ctrl Pts',(20.3311322047064,-20.9528340898087,
16.7474504826177));
#149198=CARTESIAN_POINT('Ctrl Pts',(20.312433194898,-20.9676181441102,16.7486340740925));
#149199=CARTESIAN_POINT('Ctrl Pts',(20.2935357468249,-20.9821350335323,
16.7498176655673));
#149200=CARTESIAN_POINT('Ctrl Pts',(20.2935357468249,-20.9821350335323,
15.9499155251885));
#149201=CARTESIAN_POINT('Ctrl Pts',(20.2268602525147,-21.0333546889229,
15.954085056325));
#149202=CARTESIAN_POINT('Ctrl Pts',(20.1576411760024,-21.0812997212592,
15.9582545874615));
#149203=CARTESIAN_POINT('Ctrl Pts',(20.0862377278026,-21.1257187323817,
15.962424118598));
#149204=CARTESIAN_POINT('Ctrl Pts',(20.0148299885625,-21.1701404128959,
15.9665939003054));
#149205=CARTESIAN_POINT('Ctrl Pts',(19.9412380082957,-21.2110354095534,
15.9707636820128));
#149206=CARTESIAN_POINT('Ctrl Pts',(19.8658482018833,-21.2481967790008,
15.9749334637202));
#149207=CARTESIAN_POINT('Ctrl Pts',(19.7903802125541,-21.2853966866059,
15.9791075696952));
#149208=CARTESIAN_POINT('Ctrl Pts',(19.7131110872639,-21.3188550307645,
15.9832816756702));
#149209=CARTESIAN_POINT('Ctrl Pts',(19.6344495258896,-21.3484120370515,
15.9874557816452));
#149210=CARTESIAN_POINT('Ctrl Pts',(19.5557465373968,-21.3779846095385,
15.9916320859135));
#149211=CARTESIAN_POINT('Ctrl Pts',(19.4756500908118,-21.4036516119134,
15.9958083901818));
#149212=CARTESIAN_POINT('Ctrl Pts',(19.3945841120992,-21.4253031821518,
15.99998469445));
#149213=CARTESIAN_POINT('Ctrl Pts',(19.3133757752575,-21.4469927742223,
16.0041683326317));
#149214=CARTESIAN_POINT('Ctrl Pts',(19.2311949555798,-21.4646527513623,
16.0083519708133));
#149215=CARTESIAN_POINT('Ctrl Pts',(19.1484756590802,-21.4782244413413,
16.0125356089949));
#149216=CARTESIAN_POINT('Ctrl Pts',(19.0812407977607,-21.4892556122074,
16.0159361013208));
#149217=CARTESIAN_POINT('Ctrl Pts',(19.0136504400821,-21.4975868104144,
16.0193365936467));
#149218=CARTESIAN_POINT('Ctrl Pts',(18.9459382820314,-21.5032119011579,
16.0227370859726));
#149219=CARTESIAN_POINT('Ctrl Pts',(18.862611928595,-21.5101341188644,16.0269217203656));
#149220=CARTESIAN_POINT('Ctrl Pts',(18.7787910168742,-21.5129825827272,
16.0311063547587));
#149221=CARTESIAN_POINT('Ctrl Pts',(18.6949078655889,-21.5117015070174,
16.0352909891517));
#149222=CARTESIAN_POINT('Ctrl Pts',(18.6111441115869,-21.5104222547604,
16.0394696672357));
#149223=CARTESIAN_POINT('Ctrl Pts',(18.5273187500337,-21.5050251452316,
16.0436483453196));
#149224=CARTESIAN_POINT('Ctrl Pts',(18.4438686393695,-21.4955062008139,
16.0478270234036));
#149225=CARTESIAN_POINT('Ctrl Pts',(18.3589227454461,-21.4858166361586,
16.052080601289));
#149226=CARTESIAN_POINT('Ctrl Pts',(18.2743661679608,-21.471855975481,16.0563341791744));
#149227=CARTESIAN_POINT('Ctrl Pts',(18.1906591204414,-21.453675576209,16.0605877570599));
#149228=CARTESIAN_POINT('Ctrl Pts',(18.1085748973791,-21.435847639453,16.0647588710378));
#149229=CARTESIAN_POINT('Ctrl Pts',(18.0273080288928,-21.4139622218931,
16.0689299850158));
#149230=CARTESIAN_POINT('Ctrl Pts',(17.9472849642521,-21.3881197533225,
16.0731010989937));
#149231=CARTESIAN_POINT('Ctrl Pts',(17.8672887521235,-21.3622859564418,
16.0772708133141));
#149232=CARTESIAN_POINT('Ctrl Pts',(17.7885359523435,-21.3324978868905,
16.0814405276345));
#149233=CARTESIAN_POINT('Ctrl Pts',(17.7114383592366,-21.2989059825309,
16.0856102419549));
#149234=CARTESIAN_POINT('Ctrl Pts',(17.6343435095931,-21.2653152735154,
16.0897798078989));
#149235=CARTESIAN_POINT('Ctrl Pts',(17.5589041709151,-21.2279211833515,
16.0939493738429));
#149236=CARTESIAN_POINT('Ctrl Pts',(17.4855113682731,-21.1869219531001,
16.098118939787));
#149237=CARTESIAN_POINT('Ctrl Pts',(17.4095381652298,-21.1444812404909,
16.1024351025259));
#149238=CARTESIAN_POINT('Ctrl Pts',(17.3357585487131,-21.098177414705,16.1067512652648));
#149239=CARTESIAN_POINT('Ctrl Pts',(17.2645758959971,-21.0482807070083,
16.1110674280037));
#149240=CARTESIAN_POINT('Ctrl Pts',(17.1957120107063,-21.0000093793167,
16.1152429921954));
#149241=CARTESIAN_POINT('Ctrl Pts',(17.1292788382186,-20.948375977651,16.1194185563871));
#149242=CARTESIAN_POINT('Ctrl Pts',(17.0656083164573,-20.8936666012181,
16.1235941205788));
#149243=CARTESIAN_POINT('Ctrl Pts',(16.9987219480043,-20.8361939842407,
16.1279805825913));
#149244=CARTESIAN_POINT('Ctrl Pts',(16.9348850702689,-20.7753268941812,
16.1323670446039));
#149245=CARTESIAN_POINT('Ctrl Pts',(16.8744375629656,-20.7114395535996,
16.1367535066164));
#149246=CARTESIAN_POINT('Ctrl Pts',(16.8139900556624,-20.647552213018,16.141139968629));
#149247=CARTESIAN_POINT('Ctrl Pts',(16.7569322374057,-20.5806451127529,
16.1455264306415));
#149248=CARTESIAN_POINT('Ctrl Pts',(16.703552701499,-20.5111291697643,16.149912892654));
#149249=CARTESIAN_POINT('Ctrl Pts',(16.6525544398241,-20.4447143500982,
16.1541036735168));
#149250=CARTESIAN_POINT('Ctrl Pts',(16.6047208600206,-20.3756679864259,
16.1582944543796));
#149251=CARTESIAN_POINT('Ctrl Pts',(16.5603345705066,-20.304323408296,16.1624852352424));
#149252=CARTESIAN_POINT('Ctrl Pts',(16.516010837252,-20.2330793803581,16.1666701097864));
#149253=CARTESIAN_POINT('Ctrl Pts',(16.4751249866854,-20.1595439541278,
16.1708549843304));
#149254=CARTESIAN_POINT('Ctrl Pts',(16.437918752824,-20.0840825528056,16.1750398588744));
#149255=CARTESIAN_POINT('Ctrl Pts',(16.4007539244065,-20.0087051296905,
16.1792200762261));
#149256=CARTESIAN_POINT('Ctrl Pts',(16.3672607802463,-19.9314063968238,
16.1834002935778));
#149257=CARTESIAN_POINT('Ctrl Pts',(16.3376364602565,-19.8525785836828,
16.1875805109294));
#149258=CARTESIAN_POINT('Ctrl Pts',(16.3080359860442,-19.7738142221415,
16.1917573634601));
#149259=CARTESIAN_POINT('Ctrl Pts',(16.2822983085876,-19.6935236530688,
16.1959342159908));
#149260=CARTESIAN_POINT('Ctrl Pts',(16.2605729619717,-19.6121202068944,
16.2001110685215));
#149261=CARTESIAN_POINT('Ctrl Pts',(16.2388581016535,-19.5307560521889,
16.2042859049868));
#149262=CARTESIAN_POINT('Ctrl Pts',(16.2211518401956,-19.4482805298204,
16.2084607414521));
#149263=CARTESIAN_POINT('Ctrl Pts',(16.2075538451849,-19.3651220483341,
16.2126355779174));
#149264=CARTESIAN_POINT('Ctrl Pts',(16.1939550163507,-19.2819584676039,
16.216810670382));
#149265=CARTESIAN_POINT('Ctrl Pts',(16.1844650395067,-19.1981122945307,
16.2209857628465));
#149266=CARTESIAN_POINT('Ctrl Pts',(16.1791322578279,-19.1140210480408,
16.2251608553111));
#149267=CARTESIAN_POINT('Ctrl Pts',(16.1756711337436,-19.0594434830796,
16.2278706067979));
#149268=CARTESIAN_POINT('Ctrl Pts',(16.1739601228212,-19.0047628516759,
16.2305803582847));
#149269=CARTESIAN_POINT('Ctrl Pts',(16.174000705501,-18.9500994304892,16.2332901097715));
#149270=CARTESIAN_POINT('',(16.1740005630998,-18.9536979607663,16.1667098902285));
#149271=CARTESIAN_POINT('Ctrl Pts',(20.2954006447972,-20.9845255200926,
15.8832287071313));
#149272=CARTESIAN_POINT('Ctrl Pts',(20.2230158536215,-21.0410311268267,
15.8878110831473));
#149273=CARTESIAN_POINT('Ctrl Pts',(19.4492534979044,-21.5779135325709,
15.9347853947238));
#149274=CARTESIAN_POINT('Ctrl Pts',(17.414194801089,-21.6762257759895,16.0241516418607));
#149275=CARTESIAN_POINT('Ctrl Pts',(16.2227678370508,-20.0081650868305,
16.1140629935438));
#149276=CARTESIAN_POINT('Ctrl Pts',(16.1704459057083,-19.0564768309817,
16.1615824096664));
#149277=CARTESIAN_POINT('Ctrl Pts',(16.1712325076282,-18.9536997967236,
16.1667098902285));
#149278=CARTESIAN_POINT('Ctrl Pts',(16.1740005630998,-18.9536979607663,
16.1667098902285));
#149279=CARTESIAN_POINT('Ctrl Pts',(16.1739457994085,-18.8711312597184,
16.1708335669039));
#149280=CARTESIAN_POINT('Ctrl Pts',(16.1778897355288,-18.7884072256501,
16.1749572435793));
#149281=CARTESIAN_POINT('Ctrl Pts',(16.185851592152,-18.7059518510905,16.1790809202548));
#149282=CARTESIAN_POINT('Ctrl Pts',(16.193849980064,-18.6231181475504,16.1832235175451));
#149283=CARTESIAN_POINT('Ctrl Pts',(16.2059033176551,-18.5405560554534,
16.1873661148355));
#149284=CARTESIAN_POINT('Ctrl Pts',(16.2219780566694,-18.4586991220099,
16.1915087121259));
#149285=CARTESIAN_POINT('Ctrl Pts',(16.23794569149,-18.3773875921872,16.1956237077524));
#149286=CARTESIAN_POINT('Ctrl Pts',(16.2578812222445,-18.2967723256482,
16.1997387033789));
#149287=CARTESIAN_POINT('Ctrl Pts',(16.2816998746989,-18.2172727748012,
16.2038536990054));
#149288=CARTESIAN_POINT('Ctrl Pts',(16.3055083094402,-18.1378073276299,
16.2079669293832));
#149289=CARTESIAN_POINT('Ctrl Pts',(16.33319642467,-18.0594570997615,16.2120801597611));
#149290=CARTESIAN_POINT('Ctrl Pts',(16.3646289972004,-17.9826285278118,
16.2161933901389));
#149291=CARTESIAN_POINT('Ctrl Pts',(16.3960581246075,-17.9058083765508,
16.2203061696919));
#149292=CARTESIAN_POINT('Ctrl Pts',(16.4312307139714,-17.8305099882011,
16.2244189492448));
#149293=CARTESIAN_POINT('Ctrl Pts',(16.4699631644818,-17.7571204213743,
16.2285317287977));
#149294=CARTESIAN_POINT('Ctrl Pts',(16.5091807554343,-17.6828116189603,
16.2326960226666));
#149295=CARTESIAN_POINT('Ctrl Pts',(16.5520477937181,-17.6104602387452,
16.2368603165354));
#149296=CARTESIAN_POINT('Ctrl Pts',(16.5983263505015,-17.5404412648289,
16.2410246104042));
#149297=CARTESIAN_POINT('Ctrl Pts',(16.6440925485816,-17.4711974842891,
16.2451428005836));
#149298=CARTESIAN_POINT('Ctrl Pts',(16.6931947649454,-17.404235069768,16.2492609907631));
#149299=CARTESIAN_POINT('Ctrl Pts',(16.7453611252722,-17.3398847975652,
16.2533791809425));
#149300=CARTESIAN_POINT('Ctrl Pts',(16.7984034996616,-17.2744539105174,
16.257566526656));
#149301=CARTESIAN_POINT('Ctrl Pts',(16.8546135316781,-17.2117240820489,
16.2617538723695));
#149302=CARTESIAN_POINT('Ctrl Pts',(16.9136665630955,-17.1520038393131,
16.265941218083));
#149303=CARTESIAN_POINT('Ctrl Pts',(16.9727195945129,-17.0922835965773,
16.2701285637965));
#149304=CARTESIAN_POINT('Ctrl Pts',(17.0346152026565,-17.0355732283015,
16.27431590951));
#149305=CARTESIAN_POINT('Ctrl Pts',(17.098995528925,-16.9821369642626,16.2785032552236));
#149306=CARTESIAN_POINT('Ctrl Pts',(17.1633341687151,-16.9287353003848,
16.2826878896166));
#149307=CARTESIAN_POINT('Ctrl Pts',(17.2304115572044,-16.8783896656035,
16.2868725240096));
#149308=CARTESIAN_POINT('Ctrl Pts',(17.2999052707799,-16.8313934104547,
16.2910571584027));
#149309=CARTESIAN_POINT('Ctrl Pts',(17.3693000686557,-16.7844640486581,
16.2952358364866));
#149310=CARTESIAN_POINT('Ctrl Pts',(17.4411039821924,-16.7408748523863,
16.2994145145706));
#149311=CARTESIAN_POINT('Ctrl Pts',(17.5149611920067,-16.7008793047448,
16.3035931926545));
#149312=CARTESIAN_POINT('Ctrl Pts',(17.5901422392268,-16.6601668656561,
16.3078467705399));
#149313=CARTESIAN_POINT('Ctrl Pts',(17.6674505464318,-16.6231784826193,
16.3121003484254));
#149314=CARTESIAN_POINT('Ctrl Pts',(17.746479455157,-16.5901356572587,16.3163539263108));
#149315=CARTESIAN_POINT('Ctrl Pts',(17.8239762342742,-16.5577334315455,
16.3205250402888));
#149316=CARTESIAN_POINT('Ctrl Pts',(17.9031270518496,-16.5291253296779,
16.3246961542667));
#149317=CARTESIAN_POINT('Ctrl Pts',(17.9835248188146,-16.5044732887209,
16.3288672682447));
#149318=CARTESIAN_POINT('Ctrl Pts',(18.0638956075325,-16.4798295199942,
16.333036982565));
#149319=CARTESIAN_POINT('Ctrl Pts',(18.1455120751841,-16.4591393105014,
16.3372066968854));
#149320=CARTESIAN_POINT('Ctrl Pts',(18.2279505020323,-16.4425152111227,
16.3413764112058));
#149321=CARTESIAN_POINT('Ctrl Pts',(18.3103859953677,-16.4258917033007,
16.3455459771498));
#149322=CARTESIAN_POINT('Ctrl Pts',(18.3936429386218,-16.4133341080144,
16.3497155430939));
#149323=CARTESIAN_POINT('Ctrl Pts',(18.4772872562556,-16.404903895178,16.3538851090379));
#149324=CARTESIAN_POINT('Ctrl Pts',(18.5638724049111,-16.3961772864581,
16.3582012717768));
#149325=CARTESIAN_POINT('Ctrl Pts',(18.6508721501763,-16.3918737507556,
16.3625174345158));
#149326=CARTESIAN_POINT('Ctrl Pts',(18.7378010569179,-16.3920028218831,
16.3668335972547));
#149327=CARTESIAN_POINT('Ctrl Pts',(18.8218982636657,-16.3921276885323,
16.3710091614464));
#149328=CARTESIAN_POINT('Ctrl Pts',(18.9059287081099,-16.3964007414036,
16.3751847256381));
#149329=CARTESIAN_POINT('Ctrl Pts',(18.9894564259427,-16.4047775883436,
16.3793602898297));
#149330=CARTESIAN_POINT('Ctrl Pts',(19.0772029302351,-16.4135775299086,
16.3837467518423));
#149331=CARTESIAN_POINT('Ctrl Pts',(19.1643940106306,-16.4269066375599,
16.3881332138548));
#149332=CARTESIAN_POINT('Ctrl Pts',(19.2505367177894,-16.4446528323395,
16.3925196758674));
#149333=CARTESIAN_POINT('Ctrl Pts',(19.3366794249481,-16.462399027119,16.3969061378799));
#149334=CARTESIAN_POINT('Ctrl Pts',(19.4217732165569,-16.4845620891763,
16.4012925998925));
#149335=CARTESIAN_POINT('Ctrl Pts',(19.5053461655912,-16.510970485056,16.405679061905));
#149336=CARTESIAN_POINT('Ctrl Pts',(19.5850737993556,-16.5361637914947,
16.4098636962981));
#149337=CARTESIAN_POINT('Ctrl Pts',(19.6637142290033,-16.5653141227607,
16.4140483306911));
#149338=CARTESIAN_POINT('Ctrl Pts',(19.7408462713706,-16.5983091567015,
16.4182329650842));
#149339=CARTESIAN_POINT('Ctrl Pts',(19.817868525823,-16.6312572262956,16.4224116431681));
#149340=CARTESIAN_POINT('Ctrl Pts',(19.8933862382763,-16.6680389491569,
16.4265903212521));
#149341=CARTESIAN_POINT('Ctrl Pts',(19.96699367127,-16.7084923430913,16.430768999336));
#149342=CARTESIAN_POINT('Ctrl Pts',(20.0419204645992,-16.7496708350385,
16.4350225772214));
#149343=CARTESIAN_POINT('Ctrl Pts',(20.1148673616167,-16.7946537768954,
16.4392761551069));
#149344=CARTESIAN_POINT('Ctrl Pts',(20.1854279979956,-16.8432191278764,
16.4435297329923));
#149345=CARTESIAN_POINT('Ctrl Pts',(20.2546206787505,-16.8908429447611,
16.4477008469703));
#149346=CARTESIAN_POINT('Ctrl Pts',(20.3215184014304,-16.9419112335083,
16.4518719609482));
#149347=CARTESIAN_POINT('Ctrl Pts',(20.3857646529992,-16.9961693500964,
16.4560430749262));
#149348=CARTESIAN_POINT('Ctrl Pts',(20.4499893461177,-17.0504092598493,
16.4602127892466));
#149349=CARTESIAN_POINT('Ctrl Pts',(20.5115639839655,-17.1078365750807,
16.4643825035669));
#149350=CARTESIAN_POINT('Ctrl Pts',(20.5701645776068,-17.1681559362035,
16.4685522178873));
#149351=CARTESIAN_POINT('Ctrl Pts',(20.6287630859875,-17.2284731509046,
16.4727217838313));
#149352=CARTESIAN_POINT('Ctrl Pts',(20.6843874406312,-17.2916818763295,
16.4768913497754));
#149353=CARTESIAN_POINT('Ctrl Pts',(20.7367509982117,-17.3574503961425,
16.4810609157194));
#149354=CARTESIAN_POINT('Ctrl Pts',(20.7909555938793,-17.425531255978,16.4853770784584));
#149355=CARTESIAN_POINT('Ctrl Pts',(20.8416654983872,-17.4963548514851,
16.4896932411973));
#149356=CARTESIAN_POINT('Ctrl Pts',(20.8886099384769,-17.5695181690103,
16.4940094039362));
#149357=CARTESIAN_POINT('Ctrl Pts',(20.9340251683684,-17.6402981991626,
16.4981849681279));
#149358=CARTESIAN_POINT('Ctrl Pts',(20.9759162929431,-17.7132674273084,
16.5023605323196));
#149359=CARTESIAN_POINT('Ctrl Pts',(21.0140846597657,-17.788035247827,16.5065360965112));
#149360=CARTESIAN_POINT('Ctrl Pts',(21.0541808200598,-17.8665794132165,
16.5109225585238));
#149361=CARTESIAN_POINT('Ctrl Pts',(21.0901680280105,-17.9471081067066,
16.5153090205363));
#149362=CARTESIAN_POINT('Ctrl Pts',(21.1218737001564,-18.029146169699,16.5196954825489));
#149363=CARTESIAN_POINT('Ctrl Pts',(21.1535793723024,-18.1111842326914,
16.5240819445614));
#149364=CARTESIAN_POINT('Ctrl Pts',(21.1810033999592,-18.1947310901858,
16.5284684065739));
#149365=CARTESIAN_POINT('Ctrl Pts',(21.2040345704695,-18.2792970784325,
16.5328548685865));
#149366=CARTESIAN_POINT('Ctrl Pts',(21.2260060426843,-18.3599720602032,
16.5370395029795));
#149367=CARTESIAN_POINT('Ctrl Pts',(21.244061800264,-18.4418747378537,16.5412241373726));
#149368=CARTESIAN_POINT('Ctrl Pts',(21.2580683099057,-18.5245901651463,
16.5454087717656));
#149369=CARTESIAN_POINT('Ctrl Pts',(21.2720548830146,-18.607187857266,16.5495874498496));
#149370=CARTESIAN_POINT('Ctrl Pts',(21.2820035803663,-18.6905955514661,
16.5537661279335));
#149371=CARTESIAN_POINT('Ctrl Pts',(21.28783098536,-18.7743844088621,16.5579448060174));
#149372=CARTESIAN_POINT('Ctrl Pts',(21.2937628424001,-18.859675121309,16.5621983839029));
#149373=CARTESIAN_POINT('Ctrl Pts',(21.2954240788116,-18.9453603308621,
16.5664519617883));
#149374=CARTESIAN_POINT('Ctrl Pts',(21.2927814384536,-19.0309781629653,
16.5707055396737));
#149375=CARTESIAN_POINT('Ctrl Pts',(21.2901900308356,-19.1149361263236,
16.5748766536517));
#149376=CARTESIAN_POINT('Ctrl Pts',(21.2834601502021,-19.1988288204155,
16.5790477676297));
#149377=CARTESIAN_POINT('Ctrl Pts',(21.2726129381323,-19.2822186402176,
16.5832188816076));
#149378=CARTESIAN_POINT('Ctrl Pts',(21.2617693659493,-19.3655804777602,
16.587388595928));
#149379=CARTESIAN_POINT('Ctrl Pts',(21.2468112655211,-19.448439320332,16.5915583102483));
#149380=CARTESIAN_POINT('Ctrl Pts',(21.2278116184526,-19.5303628719679,
16.5957280245687));
#149381=CARTESIAN_POINT('Ctrl Pts',(21.208812647473,-19.6122835084123,16.5998975905128));
#149382=CARTESIAN_POINT('Ctrl Pts',(21.1857725205577,-19.6932684721469,
16.6040671564568));
#149383=CARTESIAN_POINT('Ctrl Pts',(21.1588150040537,-19.7728971897357,
16.6082367224008));
#149384=CARTESIAN_POINT('Ctrl Pts',(21.1309096945252,-19.8553255548022,
16.6125528851398));
#149385=CARTESIAN_POINT('Ctrl Pts',(21.0988065683014,-19.9363000284493,
16.6168690478787));
#149386=CARTESIAN_POINT('Ctrl Pts',(21.0626979316575,-20.0153747895704,
16.6211852106176));
#149387=CARTESIAN_POINT('Ctrl Pts',(21.0277655300544,-20.0918736986652,
16.6253607748093));
#149388=CARTESIAN_POINT('Ctrl Pts',(20.9890848280188,-20.1665943642428,
16.629536339001));
#149389=CARTESIAN_POINT('Ctrl Pts',(20.9468767362675,-20.2391583236285,
16.6337119031926));
#149390=CARTESIAN_POINT('Ctrl Pts',(20.902536814142,-20.3153873160984,16.6380983652052));
#149391=CARTESIAN_POINT('Ctrl Pts',(20.8543041199711,-20.3892355173246,
16.6424848272177));
#149392=CARTESIAN_POINT('Ctrl Pts',(20.8024847707863,-20.4603006175909,
16.6468712892303));
#149393=CARTESIAN_POINT('Ctrl Pts',(20.7506654216016,-20.5313657178571,
16.6512577512428));
#149394=CARTESIAN_POINT('Ctrl Pts',(20.6952598420585,-20.5996473145404,
16.6556442132554));
#149395=CARTESIAN_POINT('Ctrl Pts',(20.6366195645772,-20.664786849695,16.6600306752679));
#149396=CARTESIAN_POINT('Ctrl Pts',(20.5806916320421,-20.7269134235104,
16.6642142460497));
#149397=CARTESIAN_POINT('Ctrl Pts',(20.5216135032521,-20.78641336654,16.6683978168314));
#149398=CARTESIAN_POINT('Ctrl Pts',(20.4596615870938,-20.8429500487398,
16.6725813876132));
#149399=CARTESIAN_POINT('Ctrl Pts',(20.406347116845,-20.8916042865426,16.6761816775447));
#149400=CARTESIAN_POINT('Ctrl Pts',(20.3509051444086,-20.9380642575358,
16.6797819674761));
#149401=CARTESIAN_POINT('Ctrl Pts',(20.2935357468249,-20.9821350335323,
16.6833822574076));
#149402=CARTESIAN_POINT('Origin',(18.734,-18.952,-1.76670989022851));
#149403=CARTESIAN_POINT('',(20.296105573652,-20.9854858072394,17.5498940756793));
#149404=CARTESIAN_POINT('',(20.2910030417442,-20.978827659161,17.4833253052881));
#149405=CARTESIAN_POINT('',(20.2935357468249,-20.9821350335323,-1.76670989022851));
#149406=CARTESIAN_POINT('',(16.1737370593341,-18.9511644347003,17.0332901097715));
#149407=CARTESIAN_POINT('Ctrl Pts',(16.1700998810729,-18.9511632476738,
17.0332901097715));
#149408=CARTESIAN_POINT('Ctrl Pts',(16.1699051733629,-18.905425756545,17.0355745863224));
#149409=CARTESIAN_POINT('Ctrl Pts',(16.1917620149477,-18.0111494804083,
17.0802509984337));
#149410=CARTESIAN_POINT('Ctrl Pts',(17.2348044654712,-16.3222275152694,
17.1673193461055));
#149411=CARTESIAN_POINT('Ctrl Pts',(20.1337363807921,-16.2679678398935,
17.294495152787));
#149412=CARTESIAN_POINT('Ctrl Pts',(21.7484970441735,-18.6761410815923,
17.4216709594683));
#149413=CARTESIAN_POINT('Ctrl Pts',(20.9781023854704,-20.4576174664893,
17.5068039337658));
#149414=CARTESIAN_POINT('Ctrl Pts',(20.3016498302087,-20.9812337545997,
17.5495449725028));
#149415=CARTESIAN_POINT('Ctrl Pts',(20.296105573652,-20.9854858072394,17.5498940756793));
#149416=CARTESIAN_POINT('Ctrl Pts',(20.2935357468249,-20.9821350335323,
16.7498176655673));
#149417=CARTESIAN_POINT('Ctrl Pts',(20.2268584845006,-21.0333560470992,
16.7539938188206));
#149418=CARTESIAN_POINT('Ctrl Pts',(20.1577087866918,-21.081247541242,16.758169972074));
#149419=CARTESIAN_POINT('Ctrl Pts',(20.0864599732948,-21.1255804610447,
16.7623461253273));
#149420=CARTESIAN_POINT('Ctrl Pts',(20.0150847863021,-21.169992013883,16.7665296857988));
#149421=CARTESIAN_POINT('Ctrl Pts',(19.9416034481486,-21.2108321584005,
16.7707132462703));
#149422=CARTESIAN_POINT('Ctrl Pts',(19.8664139461467,-21.2479178240025,
16.7748968067418));
#149423=CARTESIAN_POINT('Ctrl Pts',(19.8011427015957,-21.2801115144034,
16.7785285131816));
#149424=CARTESIAN_POINT('Ctrl Pts',(19.7345847459897,-21.3094765936477,
16.7821602196214));
#149425=CARTESIAN_POINT('Ctrl Pts',(19.6670104728628,-21.3359235427187,
16.7857919260613));
#149426=CARTESIAN_POINT('Ctrl Pts',(19.5891480045999,-21.3663970445028,
16.7899765604543));
#149427=CARTESIAN_POINT('Ctrl Pts',(19.5096461031211,-21.3931085897472,
16.7941611948473));
#149428=CARTESIAN_POINT('Ctrl Pts',(19.4289030536307,-21.4158810332593,
16.7983458292404));
#149429=CARTESIAN_POINT('Ctrl Pts',(19.3482749318772,-21.4386210630167,
16.8025245073243));
#149430=CARTESIAN_POINT('Ctrl Pts',(19.2664096101498,-21.4574330041518,
16.8067031854083));
#149431=CARTESIAN_POINT('Ctrl Pts',(19.1837245465112,-21.4721880549406,
16.8108818634922));
#149432=CARTESIAN_POINT('Ctrl Pts',(19.0995574125316,-21.4872075794106,
16.8151354413777));
#149433=CARTESIAN_POINT('Ctrl Pts',(19.0145413088146,-21.49802316776,16.8193890192631));
#149434=CARTESIAN_POINT('Ctrl Pts',(18.9291319041929,-21.5045523579284,
16.8236425971485));
#149435=CARTESIAN_POINT('Ctrl Pts',(18.8453783275425,-21.5109549670048,
16.8278137111265));
#149436=CARTESIAN_POINT('Ctrl Pts',(18.7612470435307,-21.5132358584627,
16.8319848251044));
#149437=CARTESIAN_POINT('Ctrl Pts',(18.6771754083916,-21.5113692515517,
16.8361559390824));
#149438=CARTESIAN_POINT('Ctrl Pts',(18.5931319843017,-21.5095032709988,
16.8403256534027));
#149439=CARTESIAN_POINT('Ctrl Pts',(18.5091486288698,-21.5034925662839,
16.8444953677231));
#149440=CARTESIAN_POINT('Ctrl Pts',(18.4256629639196,-21.4933634671532,
16.8486650820435));
#149441=CARTESIAN_POINT('Ctrl Pts',(18.3421802697477,-21.4832347284594,
16.8528346479875));
#149442=CARTESIAN_POINT('Ctrl Pts',(18.2591956874268,-21.4689879429832,
16.8570042139316));
#149443=CARTESIAN_POINT('Ctrl Pts',(18.1771406148225,-21.4507011876452,
16.8611737798756));
#149444=CARTESIAN_POINT('Ctrl Pts',(18.0922005870914,-21.4317714925488,
16.8654899426145));
#149445=CARTESIAN_POINT('Ctrl Pts',(18.0082571631379,-21.4085125658604,
16.8698061053535));
#149446=CARTESIAN_POINT('Ctrl Pts',(17.9257741739147,-21.3810679311309,
16.8741222680924));
#149447=CARTESIAN_POINT('Ctrl Pts',(17.8459780593898,-21.3545173024911,
16.8782978322841));
#149448=CARTESIAN_POINT('Ctrl Pts',(17.7675491154084,-21.3240496914869,
16.8824733964757));
#149449=CARTESIAN_POINT('Ctrl Pts',(17.6908872600138,-21.2898442659165,
16.8866489606674));
#149450=CARTESIAN_POINT('Ctrl Pts',(17.6103533965495,-21.2539112056161,
16.8910354226799));
#149451=CARTESIAN_POINT('Ctrl Pts',(17.5317703445183,-21.2138530785411,
16.8954218846925));
#149452=CARTESIAN_POINT('Ctrl Pts',(17.4555708448951,-21.169931219713,16.899808346705));
#149453=CARTESIAN_POINT('Ctrl Pts',(17.3793713452718,-21.1260093608849,
16.9041948087175));
#149454=CARTESIAN_POINT('Ctrl Pts',(17.3055558437865,-21.0782241494638,
16.9085812707301));
#149455=CARTESIAN_POINT('Ctrl Pts',(17.2345184376722,-21.0268867545577,
16.9129677327426));
#149456=CARTESIAN_POINT('Ctrl Pts',(17.167299168743,-20.9783086554537,16.9171184300413));
#149457=CARTESIAN_POINT('Ctrl Pts',(17.1023079512147,-20.9263629083338,
16.9212691273401));
#149458=CARTESIAN_POINT('Ctrl Pts',(17.0399060592653,-20.8712826055498,
16.9254198246388));
#149459=CARTESIAN_POINT('Ctrl Pts',(16.9775932241692,-20.8162809106139,
16.9295645982704));
#149460=CARTESIAN_POINT('Ctrl Pts',(16.9178627255451,-20.7581538490648,
16.9337093719019));
#149461=CARTESIAN_POINT('Ctrl Pts',(16.8610458812396,-20.6971770308534,
16.9378541455334));
#149462=CARTESIAN_POINT('Ctrl Pts',(16.8042942087153,-20.6362701561228,
16.9419941649009));
#149463=CARTESIAN_POINT('Ctrl Pts',(16.7504498675423,-20.5725203603437,
16.9461341842684));
#149464=CARTESIAN_POINT('Ctrl Pts',(16.6998090154257,-20.506241628022,16.9502742036359));
#149465=CARTESIAN_POINT('Ctrl Pts',(16.6491995836852,-20.4400040186794,
16.9544116543072));
#149466=CARTESIAN_POINT('Ctrl Pts',(16.6017899801564,-20.3712409577298,
16.9585491049784));
#149467=CARTESIAN_POINT('Ctrl Pts',(16.5578367768806,-20.3003002730633,
16.9626865556497));
#149468=CARTESIAN_POINT('Ctrl Pts',(16.5138971231855,-20.2293814574863,
16.9668227308571));
#149469=CARTESIAN_POINT('Ctrl Pts',(16.4734120005631,-20.1562867489274,
16.9709589060645));
#149470=CARTESIAN_POINT('Ctrl Pts',(16.4365944037611,-20.0813925475095,
16.9750950812719));
#149471=CARTESIAN_POINT('Ctrl Pts',(16.3997766632186,-20.0064980536954,
16.9792312726275));
#149472=CARTESIAN_POINT('Ctrl Pts',(16.366626681762,-19.9298044742117,16.983367463983));
#149473=CARTESIAN_POINT('Ctrl Pts',(16.3373106052886,-19.8517110343203,
16.9875036553386));
#149474=CARTESIAN_POINT('Ctrl Pts',(16.3079666664254,-19.773543373383,16.9916437777855));
#149475=CARTESIAN_POINT('Ctrl Pts',(16.2824640727847,-19.6939736349118,
16.9957839002324));
#149476=CARTESIAN_POINT('Ctrl Pts',(16.2609198329124,-19.6134185415892,
16.9999240226793));
#149477=CARTESIAN_POINT('Ctrl Pts',(16.2393648184702,-19.532823161559,17.0040662156583));
#149478=CARTESIAN_POINT('Ctrl Pts',(16.2217721969233,-19.4512419037245,
17.0082084086373));
#149479=CARTESIAN_POINT('Ctrl Pts',(16.2082078057625,-19.3691016561093,
17.0123506016162));
#149480=CARTESIAN_POINT('Ctrl Pts',(16.1946210138151,-19.2868257587522,
17.016499635181));
#149481=CARTESIAN_POINT('Ctrl Pts',(16.1850757885661,-19.2039894937103,
17.0206486687457));
#149482=CARTESIAN_POINT('Ctrl Pts',(16.1795860271471,-19.1210244221821,
17.0247977023105));
#149483=CARTESIAN_POINT('Ctrl Pts',(16.1758404729028,-19.06441901585,17.0276285047975));
#149484=CARTESIAN_POINT('Ctrl Pts',(16.1739816679355,-19.0077536994294,
17.0304593072845));
#149485=CARTESIAN_POINT('Ctrl Pts',(16.1740001363332,-18.9511645205579,
17.0332901097715));
#149486=CARTESIAN_POINT('',(16.1741505163153,-18.9531967450726,16.9667098397546));
#149487=CARTESIAN_POINT('Ctrl Pts',(20.2935357468249,-20.9821350335323,
16.6833822574076));
#149488=CARTESIAN_POINT('Ctrl Pts',(20.2246022566296,-21.0350892658062,
16.6877082667635));
#149489=CARTESIAN_POINT('Ctrl Pts',(20.1528852371741,-21.0845926182251,
16.6920342761194));
#149490=CARTESIAN_POINT('Ctrl Pts',(20.0787695024221,-21.13034684689,16.6963602854753));
#149491=CARTESIAN_POINT('Ctrl Pts',(20.0073031503783,-21.1744655191827,
16.7005316548695));
#149492=CARTESIAN_POINT('Ctrl Pts',(19.9336070873761,-21.2150982835844,
16.7047030242637));
#149493=CARTESIAN_POINT('Ctrl Pts',(19.8580574571334,-21.2520206157908,
16.7088743936579));
#149494=CARTESIAN_POINT('Ctrl Pts',(19.7825359322864,-21.2889292124336,
16.7130442112512));
#149495=CARTESIAN_POINT('Ctrl Pts',(19.7051626224655,-21.3221299162682,
16.7172140288444));
#149496=CARTESIAN_POINT('Ctrl Pts',(19.6263379680376,-21.3514443004159,
16.7213838464377));
#149497=CARTESIAN_POINT('Ctrl Pts',(19.5475189918506,-21.3807565728622,
16.7255533636525));
#149498=CARTESIAN_POINT('Ctrl Pts',(19.4672493102343,-21.4061829222831,
16.7297228808673));
#149499=CARTESIAN_POINT('Ctrl Pts',(19.3859477373509,-21.4275936960178,
16.7338923980821));
#149500=CARTESIAN_POINT('Ctrl Pts',(19.3046276330426,-21.4490093500042,
16.7380628656733));
#149501=CARTESIAN_POINT('Ctrl Pts',(19.2222756155235,-21.4664074949664,
16.7422333332645));
#149502=CARTESIAN_POINT('Ctrl Pts',(19.1393226562911,-21.4797091494666,
16.7464038008557));
#149503=CARTESIAN_POINT('Ctrl Pts',(19.0562756364042,-21.49302588676,16.7505789973549));
#149504=CARTESIAN_POINT('Ctrl Pts',(18.9726267700264,-21.502236793061,16.7547541938541));
#149505=CARTESIAN_POINT('Ctrl Pts',(18.8888135740022,-21.5073146102397,
16.7589293903533));
#149506=CARTESIAN_POINT('Ctrl Pts',(18.8049436233579,-21.5123958658936,
16.7631074141124));
#149507=CARTESIAN_POINT('Ctrl Pts',(18.7209095809406,-21.5133384579587,
16.7672854378716));
#149508=CARTESIAN_POINT('Ctrl Pts',(18.6371480220447,-21.5101672530087,
16.7714634616307));
#149509=CARTESIAN_POINT('Ctrl Pts',(18.5532533885427,-21.5069910098663,
16.7756481231467));
#149510=CARTESIAN_POINT('Ctrl Pts',(18.4696325590993,-21.4996879708117,
16.7798327846628));
#149511=CARTESIAN_POINT('Ctrl Pts',(18.3867154767371,-21.4883346506134,
16.7840174461788));
#149512=CARTESIAN_POINT('Ctrl Pts',(18.3656523998608,-21.4854506145459,
16.7850804581023));
#149513=CARTESIAN_POINT('Ctrl Pts',(18.3446346721039,-21.4823054722714,
16.7861434700258));
#149514=CARTESIAN_POINT('Ctrl Pts',(18.3236691980734,-21.4789009939035,
16.7872064819493));
#149515=CARTESIAN_POINT('Ctrl Pts',(18.2411368748191,-21.4654989831134,
16.7913911163424));
#149516=CARTESIAN_POINT('Ctrl Pts',(18.1591082470636,-21.4480243381486,
16.7955757507354));
#149517=CARTESIAN_POINT('Ctrl Pts',(18.078016311923,-21.4265273085939,16.7997603851285));
#149518=CARTESIAN_POINT('Ctrl Pts',(17.9970398011148,-21.4050608773999,
16.8039390632124));
#149519=CARTESIAN_POINT('Ctrl Pts',(17.9169977755057,-21.3795835508678,
16.8081177412964));
#149520=CARTESIAN_POINT('Ctrl Pts',(17.838315128377,-21.3501969499492,16.8122964193803));
#149521=CARTESIAN_POINT('Ctrl Pts',(17.7582221513469,-21.320283615329,16.8165499972657));
#149522=CARTESIAN_POINT('Ctrl Pts',(17.6795382417638,-21.2863195576312,
16.8208035751512));
#149523=CARTESIAN_POINT('Ctrl Pts',(17.6026975961515,-21.2484657347861,
16.8250571530366));
#149524=CARTESIAN_POINT('Ctrl Pts',(17.5273466563966,-21.2113457821625,
16.8292282670146));
#149525=CARTESIAN_POINT('Ctrl Pts',(17.4537685795461,-21.1704857525211,
16.8333993809925));
#149526=CARTESIAN_POINT('Ctrl Pts',(17.3823529481858,-21.1260860717373,
16.8375704949705));
#149527=CARTESIAN_POINT('Ctrl Pts',(17.3109612810302,-21.0817012896951,
16.8417402092908));
#149528=CARTESIAN_POINT('Ctrl Pts',(17.241731008612,-21.0337794581183,16.8459099236112));
#149529=CARTESIAN_POINT('Ctrl Pts',(17.1750254175663,-20.9825659928516,
16.8500796379316));
#149530=CARTESIAN_POINT('Ctrl Pts',(17.1083222001917,-20.9313543499799,
16.8542492038756));
#149531=CARTESIAN_POINT('Ctrl Pts',(17.0441438499412,-20.876851587128,16.8584187698197));
#149532=CARTESIAN_POINT('Ctrl Pts',(16.9828219564699,-20.8193444941569,
16.8625883357637));
#149533=CARTESIAN_POINT('Ctrl Pts',(16.9193440608729,-20.7598155227396,
16.8669044985026));
#149534=CARTESIAN_POINT('Ctrl Pts',(16.8589276101186,-20.6970673867193,
16.8712206612416));
#149535=CARTESIAN_POINT('Ctrl Pts',(16.8018987983274,-20.6314597186284,
16.8755368239805));
#149536=CARTESIAN_POINT('Ctrl Pts',(16.7467276940819,-20.5679892134248,
16.8797123881722));
#149537=CARTESIAN_POINT('Ctrl Pts',(16.6947271674387,-20.5018430132076,
16.8838879523639));
#149538=CARTESIAN_POINT('Ctrl Pts',(16.6461502555165,-20.4333788996945,
16.8880635165555));
#149539=CARTESIAN_POINT('Ctrl Pts',(16.5951198392538,-20.3614568265659,
16.8924499785681));
#149540=CARTESIAN_POINT('Ctrl Pts',(16.5478682932595,-20.2869770238509,
16.8968364405806));
#149541=CARTESIAN_POINT('Ctrl Pts',(16.5046350837973,-20.2103847068382,
16.9012229025932));
#149542=CARTESIAN_POINT('Ctrl Pts',(16.461401874335,-20.1337923898256,16.9056093646057));
#149543=CARTESIAN_POINT('Ctrl Pts',(16.4221871920777,-20.0550881117615,
16.9099958266183));
#149544=CARTESIAN_POINT('Ctrl Pts',(16.3871718743353,-19.9747403133684,
16.9143822886308));
#149545=CARTESIAN_POINT('Ctrl Pts',(16.3503471043863,-19.8902404606612,
16.9189954255353));
#149546=CARTESIAN_POINT('Ctrl Pts',(16.3180481684136,-19.8036540013278,
16.9236085624399));
#149547=CARTESIAN_POINT('Ctrl Pts',(16.290492039707,-19.7154584782324,16.9282216993444));
#149548=CARTESIAN_POINT('Ctrl Pts',(16.2630147812854,-19.6275153855894,
16.9328216326736));
#149549=CARTESIAN_POINT('Ctrl Pts',(16.2402533773008,-19.5379726851084,
16.9374215660028));
#149550=CARTESIAN_POINT('Ctrl Pts',(16.2223767943064,-19.4473270360289,
16.9420214993319));
#149551=CARTESIAN_POINT('Ctrl Pts',(16.2045882581333,-19.3571278403507,
16.9465987767929));
#149552=CARTESIAN_POINT('Ctrl Pts',(16.1916366671696,-19.2658368103364,
16.9511760542539));
#149553=CARTESIAN_POINT('Ctrl Pts',(16.1836406660146,-19.17396231111,16.9557533317148));
#149554=CARTESIAN_POINT('Ctrl Pts',(16.1772607284146,-19.100656472263,16.9594055003442));
#149555=CARTESIAN_POINT('Ctrl Pts',(16.1740347749072,-19.0269796000837,
16.9630576689735));
#149556=CARTESIAN_POINT('Ctrl Pts',(16.1740002797795,-18.9531968587196,
16.9667098376028));
#149557=CARTESIAN_POINT('Ctrl Pts',(16.1776746515055,-18.9531940792248,
16.9667098902285));
#149558=CARTESIAN_POINT('Ctrl Pts',(16.1797896608842,-18.4498774694967,
16.9916592919231));
#149559=CARTESIAN_POINT('Ctrl Pts',(16.5671404047359,-17.0883638912152,
17.0590006291781));
#149560=CARTESIAN_POINT('Ctrl Pts',(18.7821183118115,-15.9252894968784,
17.1687339019936));
#149561=CARTESIAN_POINT('Ctrl Pts',(21.3050300753512,-17.3541588961109,
17.2959097086751));
#149562=CARTESIAN_POINT('Ctrl Pts',(21.4403822622981,-19.7410800555469,
17.4007735097732));
#149563=CARTESIAN_POINT('Ctrl Pts',(20.6127493499943,-20.732395496243,17.4632453753109));
#149564=CARTESIAN_POINT('Ctrl Pts',(20.2910030417442,-20.978827659161,17.4833253052881));
#149565=CARTESIAN_POINT('Origin',(18.734,-18.952,-1.76670989022851));
#149566=CARTESIAN_POINT('',(20.2935357468249,-20.9821350335323,18.3499540480962));
#149567=CARTESIAN_POINT('',(20.2935357468249,-20.9821350335323,18.283231855311));
#149568=CARTESIAN_POINT('',(20.2935357468249,-20.9821350335323,-1.76670989022851));
#149569=CARTESIAN_POINT('',(16.1740010840393,-18.9543559031924,17.8332901097715));
#149570=CARTESIAN_POINT('Ctrl Pts',(16.1740010840393,-18.9543559031924,
17.8332901097715));
#149571=CARTESIAN_POINT('Ctrl Pts',(16.1739248258781,-18.8714913735434,
17.837412174938));
#149572=CARTESIAN_POINT('Ctrl Pts',(16.177876160498,-18.7885152466554,17.8415342401044));
#149573=CARTESIAN_POINT('Ctrl Pts',(16.1858608731257,-18.7058557534858,
17.8456563052709));
#149574=CARTESIAN_POINT('Ctrl Pts',(16.1938402258665,-18.6232517470386,
17.8497756034244));
#149575=CARTESIAN_POINT('Ctrl Pts',(16.205847540348,-18.5409644216311,17.853894901578));
#149576=CARTESIAN_POINT('Ctrl Pts',(16.2218365582967,-18.4594202174575,
17.8580141997315));
#149577=CARTESIAN_POINT('Ctrl Pts',(16.2378199266111,-18.3779048264942,
17.862132042353));
#149578=CARTESIAN_POINT('Ctrl Pts',(16.2577821151893,-18.2971324990612,
17.8662498849744));
#149579=CARTESIAN_POINT('Ctrl Pts',(16.2816254461127,-18.2175212409839,
17.8703677275959));
#149580=CARTESIAN_POINT('Ctrl Pts',(16.3054679320359,-18.1379128043045,
17.8744854242824));
#149581=CARTESIAN_POINT('Ctrl Pts',(16.3331911499574,-18.0594658076281,
17.8786031209688));
#149582=CARTESIAN_POINT('Ctrl Pts',(16.364647494651,-17.9825833169392,17.8827208176552));
#149583=CARTESIAN_POINT('Ctrl Pts',(16.396133878009,-17.905627408714,17.8868424464612));
#149584=CARTESIAN_POINT('Ctrl Pts',(16.4313603282317,-17.8302394286303,
17.8909640752672));
#149585=CARTESIAN_POINT('Ctrl Pts',(16.470131238009,-17.7568020128526,17.8950857040732));
#149586=CARTESIAN_POINT('Ctrl Pts',(16.5089205032735,-17.683329829267,17.8992092842006));
#149587=CARTESIAN_POINT('Ctrl Pts',(16.5512573267501,-17.6118104548626,
17.903332864328));
#149588=CARTESIAN_POINT('Ctrl Pts',(16.5969016205558,-17.5425992349311,
17.9074564444553));
#149589=CARTESIAN_POINT('Ctrl Pts',(16.6426258760308,-17.4732667677586,
17.9115872484506));
#149590=CARTESIAN_POINT('Ctrl Pts',(16.691668894117,-17.4062509123682,17.915718052446));
#149591=CARTESIAN_POINT('Ctrl Pts',(16.743749207993,-17.3418752269108,17.9198488564413));
#149592=CARTESIAN_POINT('Ctrl Pts',(16.7879829276106,-17.2871985975131,
17.9233572996922));
#149593=CARTESIAN_POINT('Ctrl Pts',(16.8344068718464,-17.2344260450368,
17.9268657429432));
#149594=CARTESIAN_POINT('Ctrl Pts',(16.8828286089277,-17.1837340469049,
17.9303741861941));
#149595=CARTESIAN_POINT('Ctrl Pts',(16.9405827898754,-17.1232720517519,
17.9345588205871));
#149596=CARTESIAN_POINT('Ctrl Pts',(17.0014097311533,-17.0655300202436,
17.9387434549801));
#149597=CARTESIAN_POINT('Ctrl Pts',(17.0650229727702,-17.0108365131759,
17.9429280893731));
#149598=CARTESIAN_POINT('Ctrl Pts',(17.1285456688114,-16.9562208555457,
17.947106767457));
#149599=CARTESIAN_POINT('Ctrl Pts',(17.1948464417155,-16.9046454006956,
17.9512854455409));
#149600=CARTESIAN_POINT('Ctrl Pts',(17.2636010628235,-16.8564029572577,
17.9554641236248));
#149601=CARTESIAN_POINT('Ctrl Pts',(17.3335880611029,-16.8072958026917,
17.9597177015102));
#149602=CARTESIAN_POINT('Ctrl Pts',(17.4061174102901,-16.7616426719214,
17.9639712793957));
#149603=CARTESIAN_POINT('Ctrl Pts',(17.4808106950313,-16.7197104654835,
17.9682248572811));
#149604=CARTESIAN_POINT('Ctrl Pts',(17.5540559046947,-16.6785911966919,
17.972395971259));
#149605=CARTESIAN_POINT('Ctrl Pts',(17.6293814748148,-16.6410501005271,
17.9765670852369));
#149606=CARTESIAN_POINT('Ctrl Pts',(17.7064016963165,-16.6072949596449,
17.9807381992148));
#149607=CARTESIAN_POINT('Ctrl Pts',(17.7833960729392,-16.5735511456261,
17.9849079135351));
#149608=CARTESIAN_POINT('Ctrl Pts',(17.8620835505887,-16.5435909483339,
17.9890776278554));
#149609=CARTESIAN_POINT('Ctrl Pts',(17.9420562076481,-16.517575010448,17.9932473421758));
#149610=CARTESIAN_POINT('Ctrl Pts',(18.0220260189372,-16.4915599983208,
17.9974169081198));
#149611=CARTESIAN_POINT('Ctrl Pts',(18.1032804809781,-16.4694891080429,
18.0015864740638));
#149612=CARTESIAN_POINT('Ctrl Pts',(18.1853954972949,-16.4514734355317,
18.0057560400077));
#149613=CARTESIAN_POINT('Ctrl Pts',(18.2703975762878,-16.4328243541992,
18.0100722027467));
#149614=CARTESIAN_POINT('Ctrl Pts',(18.3563213344859,-16.4185210722995,
18.0143883654857));
#149615=CARTESIAN_POINT('Ctrl Pts',(18.4426856715119,-16.4086290160463,
18.0187045282247));
#149616=CARTESIAN_POINT('Ctrl Pts',(18.5262366993411,-16.3990591924853,
18.0228800924163));
#149617=CARTESIAN_POINT('Ctrl Pts',(18.6101995699754,-16.3936175999791,
18.0270556566079));
#149618=CARTESIAN_POINT('Ctrl Pts',(18.6941361080738,-16.3923103957471,
18.0312312207996));
#149619=CARTESIAN_POINT('Ctrl Pts',(18.7823120811748,-16.3909371677368,
18.0356176828122));
#149620=CARTESIAN_POINT('Ctrl Pts',(18.8704584082174,-16.3941269389876,
18.0400041448249));
#149621=CARTESIAN_POINT('Ctrl Pts',(18.9580725064408,-16.4018251997447,
18.0443906068375));
#149622=CARTESIAN_POINT('Ctrl Pts',(19.0456866046642,-16.4095234605017,
18.0487770688502));
#149623=CARTESIAN_POINT('Ctrl Pts',(19.1327679100281,-16.4217300548923,
18.0531635308629));
#149624=CARTESIAN_POINT('Ctrl Pts',(19.2188278686569,-16.4383289917386,
18.0575499928755));
#149625=CARTESIAN_POINT('Ctrl Pts',(19.3009280810132,-16.4541641868943,
18.0617346272685));
#149626=CARTESIAN_POINT('Ctrl Pts',(19.3824044612753,-16.4740553519454,
18.0659192616614));
#149627=CARTESIAN_POINT('Ctrl Pts',(19.4628256864494,-16.4979394630997,
18.0701038960543));
#149628=CARTESIAN_POINT('Ctrl Pts',(19.5431324419637,-16.521789578178,18.0742825741382));
#149629=CARTESIAN_POINT('Ctrl Pts',(19.6223865883779,-16.5496212203604,
18.078461252222));
#149630=CARTESIAN_POINT('Ctrl Pts',(19.7001664211471,-16.5813202564142,
18.0826399303058));
#149631=CARTESIAN_POINT('Ctrl Pts',(19.7793404015218,-16.6135874749087,
18.0868935081913));
#149632=CARTESIAN_POINT('Ctrl Pts',(19.8569862208225,-16.6498620057509,
18.0911470860768));
#149633=CARTESIAN_POINT('Ctrl Pts',(19.9326746288818,-16.689970129712,18.0954006639622));
#149634=CARTESIAN_POINT('Ctrl Pts',(20.0068956694545,-16.7293006794241,
18.0995717779401));
#149635=CARTESIAN_POINT('Ctrl Pts',(20.0792340927645,-16.7723172800336,
18.1037428919179));
#149636=CARTESIAN_POINT('Ctrl Pts',(20.1493064094736,-16.8188080800587,
18.1079140058957));
#149637=CARTESIAN_POINT('Ctrl Pts',(20.21935521274,-16.8652832796468,18.112083720216));
#149638=CARTESIAN_POINT('Ctrl Pts',(20.2871390365835,-16.9152301092314,
18.1162534345362));
#149639=CARTESIAN_POINT('Ctrl Pts',(20.3523020056982,-16.9683925241235,
18.1204231488565));
#149640=CARTESIAN_POINT('Ctrl Pts',(20.4174626560349,-17.0215530472687,
18.1245927148004));
#149641=CARTESIAN_POINT('Ctrl Pts',(20.4800022811538,-17.0779286367467,
18.1287622807444));
#149642=CARTESIAN_POINT('Ctrl Pts',(20.5395979115911,-17.1372228286486,
18.1329318466883));
#149643=CARTESIAN_POINT('Ctrl Pts',(20.601288850879,-17.1986017311943,18.1372480094273));
#149644=CARTESIAN_POINT('Ctrl Pts',(20.6598245480543,-17.2631079189011,
18.1415641721664));
#149645=CARTESIAN_POINT('Ctrl Pts',(20.7148895795158,-17.3303722764562,
18.1458803349055));
#149646=CARTESIAN_POINT('Ctrl Pts',(20.768160873366,-17.395445504635,18.150055899097));
#149647=CARTESIAN_POINT('Ctrl Pts',(20.8181839009053,-17.4630995606093,
18.1542314632886));
#149648=CARTESIAN_POINT('Ctrl Pts',(20.864716308885,-17.532969341046,18.1584070274802));
#149649=CARTESIAN_POINT('Ctrl Pts',(20.9135989581757,-17.6063680779992,
18.162793489493));
#149650=CARTESIAN_POINT('Ctrl Pts',(20.9586288003487,-17.682211752265,18.1671799515058));
#149651=CARTESIAN_POINT('Ctrl Pts',(20.9995796309652,-17.7600482661804,
18.1715664135186));
#149652=CARTESIAN_POINT('Ctrl Pts',(21.0405304615818,-17.8378847800959,
18.1759528755314));
#149653=CARTESIAN_POINT('Ctrl Pts',(21.077402106402,-17.9177135750215,18.1803393375442));
#149654=CARTESIAN_POINT('Ctrl Pts',(21.1100276507034,-17.9990610706384,
18.184725799557));
#149655=CARTESIAN_POINT('Ctrl Pts',(21.1411520453503,-18.0766656473997,
18.1889104339505));
#149656=CARTESIAN_POINT('Ctrl Pts',(21.1685283427045,-18.1559410996702,
18.193095068344));
#149657=CARTESIAN_POINT('Ctrl Pts',(21.1919760688458,-18.2364906394873,
18.1972797027375));
#149658=CARTESIAN_POINT('Ctrl Pts',(21.2153904200512,-18.3169255270044,
18.2014583808218));
#149659=CARTESIAN_POINT('Ctrl Pts',(21.2348871797097,-18.3986304619534,
18.2056370589062));
#149660=CARTESIAN_POINT('Ctrl Pts',(21.2503340551361,-18.4811890793935,
18.2098157369906));
#149661=CARTESIAN_POINT('Ctrl Pts',(21.266057804701,-18.5652275007064,18.2140693148759));
#149662=CARTESIAN_POINT('Ctrl Pts',(21.2775848741471,-18.6501500625615,
18.2183228927613));
#149663=CARTESIAN_POINT('Ctrl Pts',(21.2848289888802,-18.7355018025748,
18.2225764706466));
#149664=CARTESIAN_POINT('Ctrl Pts',(21.2919326623144,-18.8191988325688,
18.226747584625));
#149665=CARTESIAN_POINT('Ctrl Pts',(21.2949179252555,-18.9033080688144,
18.2309186986034));
#149666=CARTESIAN_POINT('Ctrl Pts',(21.2937553357682,-18.9873923862781,
18.2350898125817));
#149667=CARTESIAN_POINT('Ctrl Pts',(21.2925931363989,-19.071448488437,18.2392595269026));
#149668=CARTESIAN_POINT('Ctrl Pts',(21.287285855196,-19.1554792288143,18.2434292412234));
#149669=CARTESIAN_POINT('Ctrl Pts',(21.2778561566697,-19.2390467804621,
18.2475989555442));
#149670=CARTESIAN_POINT('Ctrl Pts',(21.2684267936926,-19.3226113584178,
18.2517685214887));
#149671=CARTESIAN_POINT('Ctrl Pts',(21.2548753574853,-19.4057123233787,
18.2559380874331));
#149672=CARTESIAN_POINT('Ctrl Pts',(21.2372763100333,-19.4879176388457,
18.2601076533776));
#149673=CARTESIAN_POINT('Ctrl Pts',(21.2190585017878,-19.5730131917741,
18.264423816116));
#149674=CARTESIAN_POINT('Ctrl Pts',(21.1965032689152,-19.6571484255578,
18.2687399788544));
#149675=CARTESIAN_POINT('Ctrl Pts',(21.1697502461668,-19.7398583237475,
18.2730561415928));
#149676=CARTESIAN_POINT('Ctrl Pts',(21.1438687003148,-19.819873955721,18.2772317057849));
#149677=CARTESIAN_POINT('Ctrl Pts',(21.1140588617648,-19.8985552629124,
18.281407269977));
#149678=CARTESIAN_POINT('Ctrl Pts',(21.0804965434243,-19.9755008410831,
18.2855828341691));
#149679=CARTESIAN_POINT('Ctrl Pts',(21.0452390721828,-20.0563327574599,
18.2899692961807));
#149680=CARTESIAN_POINT('Ctrl Pts',(21.0058403441651,-20.1352484709672,
18.2943557581922));
#149681=CARTESIAN_POINT('Ctrl Pts',(20.9625580617869,-20.2118130675798,
18.2987422202038));
#149682=CARTESIAN_POINT('Ctrl Pts',(20.9192757794087,-20.2883776641924,
18.3031286822153));
#149683=CARTESIAN_POINT('Ctrl Pts',(20.8721103180846,-20.3625906950211,
18.3075151442269));
#149684=CARTESIAN_POINT('Ctrl Pts',(20.8213695361433,-20.4340554711552,
18.3119016062384));
#149685=CARTESIAN_POINT('Ctrl Pts',(20.7729692668527,-20.5022238019799,
18.3160857345563));
#149686=CARTESIAN_POINT('Ctrl Pts',(20.7211361130876,-20.5681455333702,
18.3202698628741));
#149687=CARTESIAN_POINT('Ctrl Pts',(20.6661059352987,-20.6314542729064,
18.324453991192));
#149688=CARTESIAN_POINT('Ctrl Pts',(20.6102092801907,-20.6957598398038,
18.328704000676));
#149689=CARTESIAN_POINT('Ctrl Pts',(20.5510142592993,-20.7573689829837,
18.3329540101601));
#149690=CARTESIAN_POINT('Ctrl Pts',(20.4888142341046,-20.815927842966,18.3372040196441));
#149691=CARTESIAN_POINT('Ctrl Pts',(20.4266142089099,-20.8744867029483,
18.3414540291282));
#149692=CARTESIAN_POINT('Ctrl Pts',(20.3614094943359,-20.9299948882878,
18.3457040386122));
#149693=CARTESIAN_POINT('Ctrl Pts',(20.2935357468249,-20.9821350335323,
18.3499540480962));
#149694=CARTESIAN_POINT('Ctrl Pts',(20.296105573652,-20.9854858072394,17.5498940756793));
#149695=CARTESIAN_POINT('Ctrl Pts',(19.6284054070939,-21.4975646092715,
17.5919369080633));
#149696=CARTESIAN_POINT('Ctrl Pts',(17.7316712702996,-21.8042997980315,
17.6763716760077));
#149697=CARTESIAN_POINT('Ctrl Pts',(16.2862274700061,-20.2077259602722,
17.7708370079896));
#149698=CARTESIAN_POINT('Ctrl Pts',(16.1722336653236,-19.1559927438033,
17.8232595075876));
#149699=CARTESIAN_POINT('Ctrl Pts',(16.1740883619038,-18.9543565896946,
17.833290071625));
#149700=CARTESIAN_POINT('',(16.1740009581142,-18.9497851537726,17.7667099127478));
#149701=CARTESIAN_POINT('Ctrl Pts',(20.2910030417442,-20.978827659161,17.4833253052881));
#149702=CARTESIAN_POINT('Ctrl Pts',(19.9334915646509,-21.2526531058221,
17.5056373108713));
#149703=CARTESIAN_POINT('Ctrl Pts',(18.6971962619643,-21.7882233586031,
17.5703412520151));
#149704=CARTESIAN_POINT('Ctrl Pts',(16.6895185822271,-21.0089844641567,
17.6648027803286));
#149705=CARTESIAN_POINT('Ctrl Pts',(16.1805386002103,-19.5488856395492,
17.7369523030588));
#149706=CARTESIAN_POINT('Ctrl Pts',(16.1756126004107,-18.9497870014945,
17.7667098902285));
#149707=CARTESIAN_POINT('Ctrl Pts',(16.1740009581142,-18.9497851537726,
17.7667099127478));
#149708=CARTESIAN_POINT('Ctrl Pts',(16.1740887027229,-18.8483667747388,
17.7717442924632));
#149709=CARTESIAN_POINT('Ctrl Pts',(16.1802070184517,-18.74721232135,17.7767786721785));
#149710=CARTESIAN_POINT('Ctrl Pts',(16.1922394471764,-18.6469536230176,
17.7818130518939));
#149711=CARTESIAN_POINT('Ctrl Pts',(16.2044426849046,-18.5452716801573,
17.78691889826));
#149712=CARTESIAN_POINT('Ctrl Pts',(16.2227290670666,-18.4445110968517,
17.7920247446261));
#149713=CARTESIAN_POINT('Ctrl Pts',(16.2469282568539,-18.3453088558055,
17.7971305909922));
#149714=CARTESIAN_POINT('Ctrl Pts',(16.2587491290733,-18.2968503319625,
17.7996247057951));
#149715=CARTESIAN_POINT('Ctrl Pts',(16.2719801580747,-18.2487633198967,
17.8021188205979));
#149716=CARTESIAN_POINT('Ctrl Pts',(16.2865973915759,-18.201120201178,17.8046129354008));
#149717=CARTESIAN_POINT('Ctrl Pts',(16.3111222362101,-18.1211844127561,
17.8087975697938));
#149718=CARTESIAN_POINT('Ctrl Pts',(16.3396130703746,-18.0423026572186,
17.8129822041869));
#149719=CARTESIAN_POINT('Ctrl Pts',(16.3719611025222,-17.9648970434642,
17.8171668385799));
#149720=CARTESIAN_POINT('Ctrl Pts',(16.4042630912499,-17.8876016070201,
17.8213455166639));
#149721=CARTESIAN_POINT('Ctrl Pts',(16.440411196743,-17.8117785597319,17.8255241947478));
#149722=CARTESIAN_POINT('Ctrl Pts',(16.4802468398231,-17.7378349811527,
17.8297028728318));
#149723=CARTESIAN_POINT('Ctrl Pts',(16.5207965081759,-17.6625660170697,
17.8339564507172));
#149724=CARTESIAN_POINT('Ctrl Pts',(16.5651670712163,-17.5892450243182,
17.8382100286026));
#149725=CARTESIAN_POINT('Ctrl Pts',(16.6131398985284,-17.5182802121802,
17.8424636064881));
#149726=CARTESIAN_POINT('Ctrl Pts',(16.6601826789718,-17.448691191402,17.846634720466));
#149727=CARTESIAN_POINT('Ctrl Pts',(16.7106890267627,-17.3813682068563,
17.8508058344439));
#149728=CARTESIAN_POINT('Ctrl Pts',(16.7644072919755,-17.3166698912768,
17.8549769484219));
#149729=CARTESIAN_POINT('Ctrl Pts',(16.8181075315056,-17.2519932858419,
17.8591466627423));
#149730=CARTESIAN_POINT('Ctrl Pts',(16.875017254325,-17.1899399538654,17.8633163770626));
#149731=CARTESIAN_POINT('Ctrl Pts',(16.9348438240379,-17.130836346042,17.867486091383));
#149732=CARTESIAN_POINT('Ctrl Pts',(16.9946682648648,-17.0717348413786,
17.871655657327));
#149733=CARTESIAN_POINT('Ctrl Pts',(17.0574090183537,-17.0155831748761,
17.8758252232711));
#149734=CARTESIAN_POINT('Ctrl Pts',(17.1227367799309,-16.9626707573525,
17.8799947892151));
#149735=CARTESIAN_POINT('Ctrl Pts',(17.1903613850148,-16.9078980045032,
17.884310951954));
#149736=CARTESIAN_POINT('Ctrl Pts',(17.2607578915087,-16.8565968547187,
17.888627114693));
#149737=CARTESIAN_POINT('Ctrl Pts',(17.3335255671369,-16.8090414462952,
17.8929432774319));
#149738=CARTESIAN_POINT('Ctrl Pts',(17.4039228433851,-16.7630351502992,
17.8971188416236));
#149739=CARTESIAN_POINT('Ctrl Pts',(17.476538749062,-16.7205345053978,17.9012944058152));
#149740=CARTESIAN_POINT('Ctrl Pts',(17.5509843556046,-16.6817414276969,
17.9054699700069));
#149741=CARTESIAN_POINT('Ctrl Pts',(17.6291900327563,-16.640989003863,17.9098564320195));
#149742=CARTESIAN_POINT('Ctrl Pts',(17.7094145736834,-16.604328771398,17.914242894032));
#149743=CARTESIAN_POINT('Ctrl Pts',(17.7911842815275,-16.5719372863302,
17.9186293560446));
#149744=CARTESIAN_POINT('Ctrl Pts',(17.8729539893716,-16.5395458012624,
17.9230158180571));
#149745=CARTESIAN_POINT('Ctrl Pts',(17.9562682900626,-16.5114231770868,
17.9274022800697));
#149746=CARTESIAN_POINT('Ctrl Pts',(18.0406384682269,-16.4876847226345,
17.9317887420822));
#149747=CARTESIAN_POINT('Ctrl Pts',(18.1211266494267,-16.4650385096604,
17.9359733764752));
#149748=CARTESIAN_POINT('Ctrl Pts',(18.2028752706869,-16.4462975942589,
17.9401580108683));
#149749=CARTESIAN_POINT('Ctrl Pts',(18.2854705184226,-16.4315989794963,
17.9443426452613));
#149750=CARTESIAN_POINT('Ctrl Pts',(18.3679482020464,-16.4169212863925,
17.9485213233452));
#149751=CARTESIAN_POINT('Ctrl Pts',(18.4512696694584,-16.4062745451513,
17.9527000014292));
#149752=CARTESIAN_POINT('Ctrl Pts',(18.5350067952746,-16.3997457602204,
17.9568786795131));
#149753=CARTESIAN_POINT('Ctrl Pts',(18.6202448488908,-16.3930999515116,
17.9611322573985));
#149754=CARTESIAN_POINT('Ctrl Pts',(18.7059131447157,-16.3907213105009,
17.965385835284));
#149755=CARTESIAN_POINT('Ctrl Pts',(18.7915501028463,-16.3926469595497,
17.9696394131694));
#149756=CARTESIAN_POINT('Ctrl Pts',(18.8755268214363,-16.394535276134,17.9738105271473));
#149757=CARTESIAN_POINT('Ctrl Pts',(18.9594729254762,-16.40056246717,17.9779816411253));
#149758=CARTESIAN_POINT('Ctrl Pts',(19.0429506482601,-16.4107110559915,
17.9821527551032));
#149759=CARTESIAN_POINT('Ctrl Pts',(19.126400359288,-16.4208562393561,17.9863224694236));
#149760=CARTESIAN_POINT('Ctrl Pts',(19.2093815449112,-16.4351200184238,
17.9904921837439));
#149761=CARTESIAN_POINT('Ctrl Pts',(19.2914613132267,-16.4534330338661,
17.9946618980643));
#149762=CARTESIAN_POINT('Ctrl Pts',(19.3735381607919,-16.4717453976528,
17.9988314640083));
#149763=CARTESIAN_POINT('Ctrl Pts',(19.4547132060174,-16.4941066103199,
18.0030010299523));
#149764=CARTESIAN_POINT('Ctrl Pts',(19.5345648538857,-16.5203964314216,
18.0071705958964));
#149765=CARTESIAN_POINT('Ctrl Pts',(19.6172239871861,-16.5476105702015,
18.0114867586353));
#149766=CARTESIAN_POINT('Ctrl Pts',(19.6984644293621,-16.5790345522992,
18.0158029213743));
#149767=CARTESIAN_POINT('Ctrl Pts',(19.7778387647095,-16.6144798111482,
18.0201190841132));
#149768=CARTESIAN_POINT('Ctrl Pts',(19.854627489431,-16.6487704444181,18.0242946483049));
#149769=CARTESIAN_POINT('Ctrl Pts',(19.9296694183934,-16.6868241363793,
18.0284702124965));
#149770=CARTESIAN_POINT('Ctrl Pts',(20.0025842524509,-16.7284231530182,
18.0326457766882));
#149771=CARTESIAN_POINT('Ctrl Pts',(20.0791818414392,-16.7721232370959,
18.0370322387008));
#149772=CARTESIAN_POINT('Ctrl Pts',(20.1534313177604,-16.81973589169,18.0414187007134));
#149773=CARTESIAN_POINT('Ctrl Pts',(20.2249278226101,-16.8709583791363,
18.0458051627259));
#149774=CARTESIAN_POINT('Ctrl Pts',(20.2964243274599,-16.9221808665826,
18.0501916247385));
#149775=CARTESIAN_POINT('Ctrl Pts',(20.3651674546736,-16.9770127656117,
18.0545780867511));
#149776=CARTESIAN_POINT('Ctrl Pts',(20.43079571541,-17.0351055584184,18.0589645487637));
#149777=CARTESIAN_POINT('Ctrl Pts',(20.4934043225857,-17.0905254157142,
18.0631491831568));
#149778=CARTESIAN_POINT('Ctrl Pts',(20.5534114448282,-17.1491189671382,
18.0673338175499));
#149779=CARTESIAN_POINT('Ctrl Pts',(20.6104778947948,-17.2106124181141,
18.071518451943));
#149780=CARTESIAN_POINT('Ctrl Pts',(20.6674631177333,-17.2720183407739,
18.075697130027));
#149781=CARTESIAN_POINT('Ctrl Pts',(20.721515672228,-17.3363156298581,18.079875808111));
#149782=CARTESIAN_POINT('Ctrl Pts',(20.7723306651571,-17.4031913935285,
18.084054486195));
#149783=CARTESIAN_POINT('Ctrl Pts',(20.8240564803134,-17.4712658571987,
18.0883080640804));
#149784=CARTESIAN_POINT('Ctrl Pts',(20.8724271646771,-17.5420118234208,
18.0925616419659));
#149785=CARTESIAN_POINT('Ctrl Pts',(20.9171616597699,-17.6150612701732,
18.0968152198513));
#149786=CARTESIAN_POINT('Ctrl Pts',(20.9610288893838,-17.6866945108573,
18.1009863338293));
#149787=CARTESIAN_POINT('Ctrl Pts',(21.0013994094996,-17.7605423037904,
18.1051574478073));
#149788=CARTESIAN_POINT('Ctrl Pts',(21.0380509604127,-17.8362270966629,
18.1093285617853));
#149789=CARTESIAN_POINT('Ctrl Pts',(21.0746902125439,-17.9118864927723,
18.1134982761058));
#149790=CARTESIAN_POINT('Ctrl Pts',(21.1076127735552,-17.9893812509009,
18.1176679904262));
#149791=CARTESIAN_POINT('Ctrl Pts',(21.136642647489,-18.068309834576,18.1218377047466));
#149792=CARTESIAN_POINT('Ctrl Pts',(21.1656714884152,-18.1472356096333,
18.1260072706907));
#149793=CARTESIAN_POINT('Ctrl Pts',(21.1908077596747,-18.2275946767429,
18.1301768366348));
#149794=CARTESIAN_POINT('Ctrl Pts',(21.2119243630671,-18.3089674573408,
18.1343464025789));
#149795=CARTESIAN_POINT('Ctrl Pts',(21.2337834001839,-18.3932012045179,
18.1386625653178));
#149796=CARTESIAN_POINT('Ctrl Pts',(21.2513347146948,-18.478520765314,18.1429787280566));
#149797=CARTESIAN_POINT('Ctrl Pts',(21.264494683606,-18.5644478664209,18.1472948907955));
#149798=CARTESIAN_POINT('Ctrl Pts',(21.2772259679145,-18.6475759012496,
18.1514704549872));
#149799=CARTESIAN_POINT('Ctrl Pts',(21.2858476079666,-18.731272029579,18.1556460191789));
#149800=CARTESIAN_POINT('Ctrl Pts',(21.290336834896,-18.8150986247191,18.1598215833707));
#149801=CARTESIAN_POINT('Ctrl Pts',(21.2950528020053,-18.9031591018971,
18.1642080453831));
#149802=CARTESIAN_POINT('Ctrl Pts',(21.295207927637,-18.9913629881317,18.1685945073955));
#149803=CARTESIAN_POINT('Ctrl Pts',(21.2908376238656,-19.0792059950831,
18.1729809694079));
#149804=CARTESIAN_POINT('Ctrl Pts',(21.2864673200943,-19.1670490020345,
18.1773674314203));
#149805=CARTESIAN_POINT('Ctrl Pts',(21.2775717212915,-19.2545305601574,
18.1817538934327));
#149806=CARTESIAN_POINT('Ctrl Pts',(21.2642482087235,-19.3411580684654,
18.1861403554451));
#149807=CARTESIAN_POINT('Ctrl Pts',(21.2515412573713,-19.4237767869309,
18.1903238287684));
#149808=CARTESIAN_POINT('Ctrl Pts',(21.234759861393,-19.5059261893835,18.1945073020916));
#149809=CARTESIAN_POINT('Ctrl Pts',(21.2139505970119,-19.5871732333625,
18.1986907754148));
#149810=CARTESIAN_POINT('Ctrl Pts',(21.1931684634955,-19.6683143484382,
18.2028687943766));
#149811=CARTESIAN_POINT('Ctrl Pts',(21.1683689994537,-19.7485549992071,
18.2070468133384));
#149812=CARTESIAN_POINT('Ctrl Pts',(21.1396501998678,-19.8274696544575,
18.2112248323002));
#149813=CARTESIAN_POINT('Ctrl Pts',(21.1109602255684,-19.9063051024438,
18.2153986577513));
#149814=CARTESIAN_POINT('Ctrl Pts',(21.0783588838323,-19.9838167679928,
18.2195724832024));
#149815=CARTESIAN_POINT('Ctrl Pts',(21.0419943136806,-20.0595929974581,
18.2237463086536));
#149816=CARTESIAN_POINT('Ctrl Pts',(21.0056553325342,-20.1353159047383,
18.2279171970689));
#149817=CARTESIAN_POINT('Ctrl Pts',(20.9655585822445,-20.2093053885048,
18.2320880854843));
#149818=CARTESIAN_POINT('Ctrl Pts',(20.9219002659528,-20.2811698259604,
18.2362589738997));
#149819=CARTESIAN_POINT('Ctrl Pts',(20.8782487043936,-20.3530231446856,
18.240429217003));
#149820=CARTESIAN_POINT('Ctrl Pts',(20.8310368995146,-20.4227516709466,
18.2445994601064));
#149821=CARTESIAN_POINT('Ctrl Pts',(20.7805064538477,-20.4899893804444,
18.2487697032098));
#149822=CARTESIAN_POINT('Ctrl Pts',(20.7299824361662,-20.5572185366233,
18.2529394158159));
#149823=CARTESIAN_POINT('Ctrl Pts',(20.6761408980474,-20.6219571415484,
18.257109128422));
#149824=CARTESIAN_POINT('Ctrl Pts',(20.6192651021132,-20.6838705190499,
18.2612788410281));
#149825=CARTESIAN_POINT('Ctrl Pts',(20.5623509461028,-20.7458256542418,
18.2654513659113));
#149826=CARTESIAN_POINT('Ctrl Pts',(20.5023987594139,-20.8049514195305,
18.2696238907944));
#149827=CARTESIAN_POINT('Ctrl Pts',(20.4397297081187,-20.8609489681082,
18.2737964156776));
#149828=CARTESIAN_POINT('Ctrl Pts',(20.392491319937,-20.9031585417695,18.276941562222));
#149829=CARTESIAN_POINT('Ctrl Pts',(20.3437100762383,-20.9435914593361,
18.2800867087665));
#149830=CARTESIAN_POINT('Ctrl Pts',(20.2935357468249,-20.9821350335323,
18.283231855311));
#149831=CARTESIAN_POINT('Origin',(18.734,-18.952,-1.76670989022851));
#149832=CARTESIAN_POINT('',(20.2912840470176,-20.9792340293575,19.149828721203));
#149833=CARTESIAN_POINT('',(20.2935357468249,-20.9821350335323,19.0833436973871));
#149834=CARTESIAN_POINT('',(20.2935357468249,-20.9821350335323,-1.76670989022851));
#149835=CARTESIAN_POINT('',(16.1743944468539,-18.9516176052701,18.6332901348849));
#149836=CARTESIAN_POINT('Ctrl Pts',(16.178162963747,-18.9516133246024,18.6332903748342));
#149837=CARTESIAN_POINT('Ctrl Pts',(16.1776269370726,-18.5470182282415,
18.6533365919837));
#149838=CARTESIAN_POINT('Ctrl Pts',(16.4590847030962,-17.2875284349863,
18.7157747446936));
#149839=CARTESIAN_POINT('Ctrl Pts',(18.4329096448176,-15.9399184650897,
18.8206048329641));
#149840=CARTESIAN_POINT('Ctrl Pts',(21.1037093988242,-17.0684480546079,
18.9477806396456));
#149841=CARTESIAN_POINT('Ctrl Pts',(21.532350067299,-19.5334127108451,19.0575219357252));
#149842=CARTESIAN_POINT('Ctrl Pts',(20.689118793848,-20.6706543549497,19.1248712962443));
#149843=CARTESIAN_POINT('Ctrl Pts',(20.2912840470176,-20.9792340293575,
19.149828721203));
#149844=CARTESIAN_POINT('Ctrl Pts',(20.2935357468249,-20.9821350335323,
18.3499540480962));
#149845=CARTESIAN_POINT('Ctrl Pts',(20.2269224998199,-21.0333068709719,
18.3541251295808));
#149846=CARTESIAN_POINT('Ctrl Pts',(20.1577388901063,-21.0812344067916,
18.3582962110655));
#149847=CARTESIAN_POINT('Ctrl Pts',(20.0863370407774,-21.1256569481271,
18.3624672925501));
#149848=CARTESIAN_POINT('Ctrl Pts',(20.0149588057502,-21.1700647978644,
18.3666369945581));
#149849=CARTESIAN_POINT('Ctrl Pts',(19.9413641784025,-21.2109697124809,
18.3708066965662));
#149850=CARTESIAN_POINT('Ctrl Pts',(19.8659339889943,-21.2481544905689,
18.3749763985743));
#149851=CARTESIAN_POINT('Ctrl Pts',(19.7905061189634,-21.2853381252747,
18.3791459723696));
#149852=CARTESIAN_POINT('Ctrl Pts',(19.7132432121151,-21.3188016482936,
18.3833155461649));
#149853=CARTESIAN_POINT('Ctrl Pts',(19.6345491728624,-21.3483745924327,
18.3874851199602));
#149854=CARTESIAN_POINT('Ctrl Pts',(19.5534056690215,-21.3788680367789,
18.3917844777068));
#149855=CARTESIAN_POINT('Ctrl Pts',(19.4707409474977,-21.4052244983156,
18.3960838354535));
#149856=CARTESIAN_POINT('Ctrl Pts',(19.3870163747539,-21.4273120236251,
18.4003831932001));
#149857=CARTESIAN_POINT('Ctrl Pts',(19.3057019498923,-21.4487637236256,
18.4045587869474));
#149858=CARTESIAN_POINT('Ctrl Pts',(19.2233883403865,-21.4661889020904,
18.4087343806946));
#149859=CARTESIAN_POINT('Ctrl Pts',(19.1405083157769,-21.4795187416129,
18.4129099744419));
#149860=CARTESIAN_POINT('Ctrl Pts',(19.0539434631163,-21.4934412229307,
18.4172712141882));
#149861=CARTESIAN_POINT('Ctrl Pts',(18.9667612220343,-21.5028956728378,
18.4216324539346));
#149862=CARTESIAN_POINT('Ctrl Pts',(18.8794581082821,-21.5078642254109,
18.4259936936809));
#149863=CARTESIAN_POINT('Ctrl Pts',(18.7921549945299,-21.5128327779839,
18.4303549334272));
#149864=CARTESIAN_POINT('Ctrl Pts',(18.7047315721785,-21.5133155043339,
18.4347161731735));
#149865=CARTESIAN_POINT('Ctrl Pts',(18.6176794289205,-21.5093559636358,
18.4390774129198));
#149866=CARTESIAN_POINT('Ctrl Pts',(18.5341524013308,-21.5055567617695,
18.4432620473123));
#149867=CARTESIAN_POINT('Ctrl Pts',(18.4506562604967,-21.4976540121365,
18.4474466817048));
#149868=CARTESIAN_POINT('Ctrl Pts',(18.3676269095302,-21.4856477179315,
18.4516313160972));
#149869=CARTESIAN_POINT('Ctrl Pts',(18.2847157405684,-21.4736585132003,
18.4558099941806));
#149870=CARTESIAN_POINT('Ctrl Pts',(18.2022704931349,-21.4575774310126,
18.4599886722639));
#149871=CARTESIAN_POINT('Ctrl Pts',(18.1207249420864,-21.4374564376269,
18.4641673503473));
#149872=CARTESIAN_POINT('Ctrl Pts',(18.0377177456262,-21.4169747898918,
18.4684209282328));
#149873=CARTESIAN_POINT('Ctrl Pts',(17.9556432985578,-21.392306997499,18.4726745061184));
#149874=CARTESIAN_POINT('Ctrl Pts',(17.8749514567217,-21.3635628957777,
18.476928084004));
#149875=CARTESIAN_POINT('Ctrl Pts',(17.7958239837111,-21.3353760545627,
18.4810991979814));
#149876=CARTESIAN_POINT('Ctrl Pts',(17.7180264386452,-21.3032697094724,
18.4852703119587));
#149877=CARTESIAN_POINT('Ctrl Pts',(17.6419689102695,-21.2673980433312,
18.4894414259361));
#149878=CARTESIAN_POINT('Ctrl Pts',(17.565936903732,-21.231538414274,18.4936111402558));
#149879=CARTESIAN_POINT('Ctrl Pts',(17.4916441700225,-21.1919161695519,
18.4977808545756));
#149880=CARTESIAN_POINT('Ctrl Pts',(17.4194798631978,-21.1487332131921,
18.5019505688953));
#149881=CARTESIAN_POINT('Ctrl Pts',(17.3473181242889,-21.1055517934673,
18.5061201348388));
#149882=CARTESIAN_POINT('Ctrl Pts',(17.2772850559933,-21.0588101509786,
18.5102897007822));
#149883=CARTESIAN_POINT('Ctrl Pts',(17.209743095842,-21.0087549416804,18.5144592667256));
#149884=CARTESIAN_POINT('Ctrl Pts',(17.1398264436719,-20.9569398529568,
18.5187754294653));
#149885=CARTESIAN_POINT('Ctrl Pts',(17.0725797574073,-20.9015741660661,
18.5230915922049));
#149886=CARTESIAN_POINT('Ctrl Pts',(17.008368511561,-20.8429775160239,18.5274077549446));
#149887=CARTESIAN_POINT('Ctrl Pts',(16.9462489403138,-20.7862896457112,
18.5315833191356));
#149888=CARTESIAN_POINT('Ctrl Pts',(16.8869703858408,-20.7265784444842,
18.5357588833267));
#149889=CARTESIAN_POINT('Ctrl Pts',(16.8308254399577,-20.6641701416646,
18.5399344475178));
#149890=CARTESIAN_POINT('Ctrl Pts',(16.7718447463026,-20.5986097438008,
18.5443209095317));
#149891=CARTESIAN_POINT('Ctrl Pts',(16.7163229051915,-20.5300730764181,
18.5487073715456));
#149892=CARTESIAN_POINT('Ctrl Pts',(16.6645491064846,-20.4589747839059,
18.5530938335595));
#149893=CARTESIAN_POINT('Ctrl Pts',(16.6127753077778,-20.3878764913938,
18.5574802955735));
#149894=CARTESIAN_POINT('Ctrl Pts',(16.5647498046499,-20.314217101332,18.5618667575874));
#149895=CARTESIAN_POINT('Ctrl Pts',(16.5207062260026,-20.2384410868689,
18.5662532196013));
#149896=CARTESIAN_POINT('Ctrl Pts',(16.4770273612297,-20.1632925546556,
18.5706033584189));
#149897=CARTESIAN_POINT('Ctrl Pts',(16.4371122169919,-20.0858014915384,
18.5749534972364));
#149898=CARTESIAN_POINT('Ctrl Pts',(16.4012086273382,-20.0063644586359,
18.579303636054));
#149899=CARTESIAN_POINT('Ctrl Pts',(16.3640774712897,-19.924211423433,18.5838025088638));
#149900=CARTESIAN_POINT('Ctrl Pts',(16.3312374248383,-19.8399772763342,
18.5883013816736));
#149901=CARTESIAN_POINT('Ctrl Pts',(16.3029130373491,-19.7541322709061,
18.5928002544834));
#149902=CARTESIAN_POINT('Ctrl Pts',(16.2756354411693,-19.6714598603193,
18.5971328613515));
#149903=CARTESIAN_POINT('Ctrl Pts',(16.252545805577,-19.5872939815205,18.6014654682196));
#149904=CARTESIAN_POINT('Ctrl Pts',(16.2337970621825,-19.5020775124732,
18.6057980750876));
#149905=CARTESIAN_POINT('Ctrl Pts',(16.2150725182341,-19.416971034336,18.6101250897577));
#149906=CARTESIAN_POINT('Ctrl Pts',(16.2006778102741,-19.3308170607077,
18.6144521044277));
#149907=CARTESIAN_POINT('Ctrl Pts',(16.190716084581,-19.244073493441,18.6187791190978));
#149908=CARTESIAN_POINT('Ctrl Pts',(16.180768168227,-19.1574501735471,18.6231001354885));
#149909=CARTESIAN_POINT('Ctrl Pts',(16.1752410444518,-19.0702392928349,
18.6274211518792));
#149910=CARTESIAN_POINT('Ctrl Pts',(16.1741865858058,-18.9829076772249,
18.6317421682699));
#149911=CARTESIAN_POINT('Ctrl Pts',(16.1740606709629,-18.9724792486655,
18.6322581487704));
#149912=CARTESIAN_POINT('Ctrl Pts',(16.1739984722012,-18.9620491070313,
18.632774129271));
#149913=CARTESIAN_POINT('Ctrl Pts',(16.1740000284928,-18.9516180532909,
18.6332901097715));
#149914=CARTESIAN_POINT('',(16.1740000028035,-18.9518801919504,18.5667098901964));
#149915=CARTESIAN_POINT('Ctrl Pts',(20.2935357468249,-20.9821350335323,
18.283231855311));
#149916=CARTESIAN_POINT('Ctrl Pts',(20.2268916049204,-21.0333306042209,
18.2874094017789));
#149917=CARTESIAN_POINT('Ctrl Pts',(20.1577889841688,-21.0811911374411,
18.2915869482468));
#149918=CARTESIAN_POINT('Ctrl Pts',(20.086602957854,-21.1254914856987,18.2957644947147));
#149919=CARTESIAN_POINT('Ctrl Pts',(20.0153008952338,-21.1698640454422,
18.2999488507643));
#149920=CARTESIAN_POINT('Ctrl Pts',(19.9419090508425,-21.2106646154573,
18.3041332068138));
#149921=CARTESIAN_POINT('Ctrl Pts',(19.8668262210657,-21.247714431907,18.3083175628634));
#149922=CARTESIAN_POINT('Ctrl Pts',(19.8369284324813,-21.2624675729726,
18.3099837626177));
#149923=CARTESIAN_POINT('Ctrl Pts',(19.8067627272952,-21.2766265326087,
18.3116499623721));
#149924=CARTESIAN_POINT('Ctrl Pts',(19.7763550154486,-21.2901822045703,
18.3133161621265));
#149925=CARTESIAN_POINT('Ctrl Pts',(19.6999865269343,-21.3242270608135,
18.3175007965194));
#149926=CARTESIAN_POINT('Ctrl Pts',(19.6218062328674,-21.3545898770089,
18.3216854309123));
#149927=CARTESIAN_POINT('Ctrl Pts',(19.5422037920528,-21.3810752624222,
18.3258700653053));
#149928=CARTESIAN_POINT('Ctrl Pts',(19.4627146554598,-21.4075229491676,
18.3300487433891));
#149929=CARTESIAN_POINT('Ctrl Pts',(19.3818078256885,-21.4301040236941,
18.3342274214729));
#149930=CARTESIAN_POINT('Ctrl Pts',(19.2998943515241,-21.4486704994679,
18.3384060995568));
#149931=CARTESIAN_POINT('Ctrl Pts',(19.2165126372027,-21.467569765977,18.3426596774422));
#149932=CARTESIAN_POINT('Ctrl Pts',(19.1320882756879,-21.4823088984316,
18.3469132553277));
#149933=CARTESIAN_POINT('Ctrl Pts',(19.0470726305021,-21.4927844316334,
18.3511668332132));
#149934=CARTESIAN_POINT('Ctrl Pts',(18.9637051794954,-21.5030568761824,
18.355337947191));
#149935=CARTESIAN_POINT('Ctrl Pts',(18.8797696442091,-21.5092295037566,
18.3595090611688));
#149936=CARTESIAN_POINT('Ctrl Pts',(18.7957017187999,-21.5112563173502,
18.3636801751467));
#149937=CARTESIAN_POINT('Ctrl Pts',(18.7116620031949,-21.513282450827,18.3678498894669));
#149938=CARTESIAN_POINT('Ctrl Pts',(18.6274904452119,-21.5111655221263,
18.3720196037872));
#149939=CARTESIAN_POINT('Ctrl Pts',(18.5436254163484,-21.5049115765924,
18.3761893181075));
#149940=CARTESIAN_POINT('Ctrl Pts',(18.4597633717625,-21.4986578536007,
18.3803588840514));
#149941=CARTESIAN_POINT('Ctrl Pts',(18.3762082933047,-21.4882674415331,
18.3845284499953));
#149942=CARTESIAN_POINT('Ctrl Pts',(18.2933947304044,-21.4737983655329,
18.3886980159393));
#149943=CARTESIAN_POINT('Ctrl Pts',(18.2076695447891,-21.4588205746693,
18.3930141786783));
#149944=CARTESIAN_POINT('Ctrl Pts',(18.1227395078358,-21.4394720625982,
18.3973303414174));
#149945=CARTESIAN_POINT('Ctrl Pts',(18.0390745966241,-21.415874729718,18.4016465041564));
#149946=CARTESIAN_POINT('Ctrl Pts',(17.9581350610998,-21.3930460774757,
18.405822068348));
#149947=CARTESIAN_POINT('Ctrl Pts',(17.878379925585,-21.3662413589922,18.4099976325396));
#149948=CARTESIAN_POINT('Ctrl Pts',(17.8002169726158,-21.3356210390432,
18.4141731967311));
#149949=CARTESIAN_POINT('Ctrl Pts',(17.7181061946998,-21.3034541595236,
18.4185596587439));
#149950=CARTESIAN_POINT('Ctrl Pts',(17.6377532005344,-21.2670763374213,
18.4229461207567));
#149951=CARTESIAN_POINT('Ctrl Pts',(17.559602363678,-21.2267285973938,18.4273325827695));
#149952=CARTESIAN_POINT('Ctrl Pts',(17.4814515268215,-21.1863808573663,
18.4317190447823));
#149953=CARTESIAN_POINT('Ctrl Pts',(17.4055033100765,-21.1420635575358,
18.4361055067951));
#149954=CARTESIAN_POINT('Ctrl Pts',(17.3321657913464,-21.0940692919344,
18.4404919688079));
#149955=CARTESIAN_POINT('Ctrl Pts',(17.2622960528831,-21.0483444454524,
18.4446710160258));
#149956=CARTESIAN_POINT('Ctrl Pts',(17.19453408493,-20.9991112651902,18.4488500632436));
#149957=CARTESIAN_POINT('Ctrl Pts',(17.1292545139165,-20.9465906660001,
18.4530291104615));
#149958=CARTESIAN_POINT('Ctrl Pts',(17.0640679209105,-20.8941448721524,
18.4572022054423));
#149959=CARTESIAN_POINT('Ctrl Pts',(17.0013570587501,-20.8384212459578,
18.461375300423));
#149960=CARTESIAN_POINT('Ctrl Pts',(16.9414683281885,-20.7796843834625,
18.4655483954038));
#149961=CARTESIAN_POINT('Ctrl Pts',(16.8809773183908,-20.7203568256503,
18.4697634576868));
#149962=CARTESIAN_POINT('Ctrl Pts',(16.8233659292103,-20.6579553356915,
18.4739785199699));
#149963=CARTESIAN_POINT('Ctrl Pts',(16.7689574885196,-20.5927949073772,
18.4781935822529));
#149964=CARTESIAN_POINT('Ctrl Pts',(16.715187711247,-20.5283993526991,18.4823591668069));
#149965=CARTESIAN_POINT('Ctrl Pts',(16.6645463875622,-20.4613096522779,
18.4865247513609));
#149966=CARTESIAN_POINT('Ctrl Pts',(16.6173078768047,-20.3918661241945,
18.4906903359149));
#149967=CARTESIAN_POINT('Ctrl Pts',(16.5700850499656,-20.3224456524398,
18.4948545374302));
#149968=CARTESIAN_POINT('Ctrl Pts',(16.5262630517185,-20.2506732862345,
18.4990187389455));
#149969=CARTESIAN_POINT('Ctrl Pts',(16.4860739671284,-20.1769198140034,
18.5031829404608));
#149970=CARTESIAN_POINT('Ctrl Pts',(16.4458860826634,-20.1031685441962,
18.5073470176248));
#149971=CARTESIAN_POINT('Ctrl Pts',(16.4093311160888,-20.0274366916313,
18.5115110947889));
#149972=CARTESIAN_POINT('Ctrl Pts',(16.3765953977372,-19.9501200034215,
18.5156751719529));
#149973=CARTESIAN_POINT('Ctrl Pts',(16.3431614559385,-19.8711542197504,
18.5199280651399));
#149974=CARTESIAN_POINT('Ctrl Pts',(16.313711777103,-19.7905356687049,18.5241809583268));
#149975=CARTESIAN_POINT('Ctrl Pts',(16.2883925214925,-19.7087060598861,
18.5284338515138));
#149976=CARTESIAN_POINT('Ctrl Pts',(16.2635663208297,-19.6284699613234,
18.5326039259141));
#149977=CARTESIAN_POINT('Ctrl Pts',(16.2427111716313,-19.5470700198228,
18.5367740003145));
#149978=CARTESIAN_POINT('Ctrl Pts',(16.2259135016087,-19.4649348073461,
18.5409440747148));
#149979=CARTESIAN_POINT('Ctrl Pts',(16.2086154222952,-19.3803527541242,
18.5452383772951));
#149980=CARTESIAN_POINT('Ctrl Pts',(16.1956204803925,-19.294991452669,18.5495326798753));
#149981=CARTESIAN_POINT('Ctrl Pts',(16.1869656326132,-19.2093245642189,
18.5538269824556));
#149982=CARTESIAN_POINT('Ctrl Pts',(16.1783107848339,-19.1236576757689,
18.5581212850358));
#149983=CARTESIAN_POINT('Ctrl Pts',(16.1739959871027,-19.0376857298059,
18.5624155876161));
#149984=CARTESIAN_POINT('Ctrl Pts',(16.1740000028035,-18.9518801919504,
18.5667098901964));
#149985=CARTESIAN_POINT('Ctrl Pts',(16.1740000028035,-18.9518801913083,
18.5667098902285));
#149986=CARTESIAN_POINT('Ctrl Pts',(16.1740003013853,-18.945500276023,18.5670291853155));
#149987=CARTESIAN_POINT('Ctrl Pts',(16.1740244495167,-18.9391204260769,
18.5673484804024));
#149988=CARTESIAN_POINT('Ctrl Pts',(16.1740724460423,-18.9327407557765,
18.5676677754894));
#149989=CARTESIAN_POINT('Ctrl Pts',(16.1747014814392,-18.8491297362399,
18.5718524098819));
#149990=CARTESIAN_POINT('Ctrl Pts',(16.1794322843349,-18.7653939703416,
18.5760370442745));
#149991=CARTESIAN_POINT('Ctrl Pts',(16.1882813814472,-18.6819690477863,
18.580221678667));
#149992=CARTESIAN_POINT('Ctrl Pts',(16.1971178829649,-18.5986628702823,
18.5844003567505));
#149993=CARTESIAN_POINT('Ctrl Pts',(16.2100609870472,-18.515667110836,18.5885790348339));
#149994=CARTESIAN_POINT('Ctrl Pts',(16.2270752140172,-18.433417202922,18.5927577129174));
#149995=CARTESIAN_POINT('Ctrl Pts',(16.2443944087803,-18.3496930245081,
18.5970112908029));
#149996=CARTESIAN_POINT('Ctrl Pts',(16.2659321081157,-18.2667421815311,
18.6012648686885));
#149997=CARTESIAN_POINT('Ctrl Pts',(16.2915956147072,-18.1850183713396,
18.605518446574));
#149998=CARTESIAN_POINT('Ctrl Pts',(16.3167615841415,-18.1048789366913,
18.6096895605515));
#149999=CARTESIAN_POINT('Ctrl Pts',(16.3458946705844,-18.0259198416596,
18.613860674529));
#150000=CARTESIAN_POINT('Ctrl Pts',(16.3788563531112,-17.9485567268056,
18.6180317885065));
#150001=CARTESIAN_POINT('Ctrl Pts',(16.411806975027,-17.8712195718919,18.6222015028263));
#150002=CARTESIAN_POINT('Ctrl Pts',(16.4485834613785,-17.79547775642,18.6263712171462));
#150003=CARTESIAN_POINT('Ctrl Pts',(16.4889988104968,-17.7217278109584,
18.6305409314661));
#150004=CARTESIAN_POINT('Ctrl Pts',(16.5294127214635,-17.6479804898363,
18.6347104974097));
#150005=CARTESIAN_POINT('Ctrl Pts',(16.5734650159172,-17.5762253008164,
18.6388800633533));
#150006=CARTESIAN_POINT('Ctrl Pts',(16.620922959331,-17.5068337741985,18.6430496292968));
#150007=CARTESIAN_POINT('Ctrl Pts',(16.6700494655017,-17.4350025270905,
18.6473657920363));
#150008=CARTESIAN_POINT('Ctrl Pts',(16.7228252639786,-17.3657046830183,
18.6516819547758));
#150009=CARTESIAN_POINT('Ctrl Pts',(16.7789448088305,-17.2993175745228,
18.6559981175153));
#150010=CARTESIAN_POINT('Ctrl Pts',(16.8332362653982,-17.2350930191197,
18.6601736817066));
#150011=CARTESIAN_POINT('Ctrl Pts',(16.8906566126944,-17.1735927891267,
18.6643492458978));
#150012=CARTESIAN_POINT('Ctrl Pts',(16.9508909514351,-17.1151216368725,
18.668524810089));
#150013=CARTESIAN_POINT('Ctrl Pts',(17.0141675834549,-17.0536972456977,
18.6729112721026));
#150014=CARTESIAN_POINT('Ctrl Pts',(17.0805495076473,-16.9956163559342,
18.6772977341163));
#150015=CARTESIAN_POINT('Ctrl Pts',(17.1496333442479,-16.9411836731961,
18.6816841961299));
#150016=CARTESIAN_POINT('Ctrl Pts',(17.2187171808487,-16.886750990458,18.6860706581436));
#150017=CARTESIAN_POINT('Ctrl Pts',(17.2905024122582,-16.835966787744,18.6904571201572));
#150018=CARTESIAN_POINT('Ctrl Pts',(17.3645537444778,-16.7890813808106,
18.6948435821709));
#150019=CARTESIAN_POINT('Ctrl Pts',(17.4351978651041,-16.7443532409684,
18.6990282165633));
#150020=CARTESIAN_POINT('Ctrl Pts',(17.5081670866298,-16.703006515634,18.7032128509558));
#150021=CARTESIAN_POINT('Ctrl Pts',(17.5831040926459,-16.665290877607,18.7073974853483));
#150022=CARTESIAN_POINT('Ctrl Pts',(17.6579344351092,-16.6276289231224,
18.7115761634316));
#150023=CARTESIAN_POINT('Ctrl Pts',(17.734726591191,-16.5935879949174,18.715754841515));
#150024=CARTESIAN_POINT('Ctrl Pts',(17.813095225772,-16.5633739520795,18.7199335195984));
#150025=CARTESIAN_POINT('Ctrl Pts',(17.8928685618193,-16.532618344233,18.7241870974839));
#150026=CARTESIAN_POINT('Ctrl Pts',(17.974275041662,-16.5058284229431,18.7284406753695));
#150027=CARTESIAN_POINT('Ctrl Pts',(18.0568830023301,-16.4831718222066,
18.7326942532551));
#150028=CARTESIAN_POINT('Ctrl Pts',(18.13788944647,-16.4609544638901,18.7368653672325));
#150029=CARTESIAN_POINT('Ctrl Pts',(18.2200507369796,-16.4427117186152,
18.7410364812098));
#150030=CARTESIAN_POINT('Ctrl Pts',(18.3029424071743,-16.428552090558,18.7452075951871));
#150031=CARTESIAN_POINT('Ctrl Pts',(18.3858062622686,-16.4143972139007,
18.7493773095069));
#150032=CARTESIAN_POINT('Ctrl Pts',(18.4693995572162,-16.4043228107592,
18.7535470238267));
#150033=CARTESIAN_POINT('Ctrl Pts',(18.5532876521047,-16.3983862767994,
18.7577167381465));
#150034=CARTESIAN_POINT('Ctrl Pts',(18.6371727618947,-16.3924499540871,
18.7618863040899));
#150035=CARTESIAN_POINT('Ctrl Pts',(18.7213521918228,-16.3906512394234,
18.7660558700333));
#150036=CARTESIAN_POINT('Ctrl Pts',(18.8053875689175,-16.3929955422071,
18.7702254359768));
#150037=CARTESIAN_POINT('Ctrl Pts',(18.892377526229,-16.3954222677854,18.7745415987164));
#150038=CARTESIAN_POINT('Ctrl Pts',(18.9792125852184,-16.4022887536939,
18.778857761456));
#150039=CARTESIAN_POINT('Ctrl Pts',(19.0654100827153,-16.413542327106,18.7831739241957));
#150040=CARTESIAN_POINT('Ctrl Pts',(19.1487997057718,-16.4244293165444,
18.7873494883867));
#150041=CARTESIAN_POINT('Ctrl Pts',(19.2315922114997,-16.4394218336012,
18.7915250525778));
#150042=CARTESIAN_POINT('Ctrl Pts',(19.3133609024087,-16.4584200544679,
18.7957006167689));
#150043=CARTESIAN_POINT('Ctrl Pts',(19.3992595355482,-16.4783778303156,
18.8000870787828));
#150044=CARTESIAN_POINT('Ctrl Pts',(19.4840276488778,-16.5027564393573,
18.8044735407967));
#150045=CARTESIAN_POINT('Ctrl Pts',(19.567190691381,-16.5313816344174,18.8088600028106));
#150046=CARTESIAN_POINT('Ctrl Pts',(19.6503537338843,-16.5600068294774,
18.8132464648245));
#150047=CARTESIAN_POINT('Ctrl Pts',(19.7319111958456,-16.5928783231054,
18.8176329268384));
#150048=CARTESIAN_POINT('Ctrl Pts',(19.8114169849416,-16.6297655931066,
18.8220193888523));
#150049=CARTESIAN_POINT('Ctrl Pts',(19.8872645948574,-16.6649556251499,
18.8262040232484));
#150050=CARTESIAN_POINT('Ctrl Pts',(19.961527503306,-16.7039309946397,18.8303886576445));
#150051=CARTESIAN_POINT('Ctrl Pts',(20.0338023663788,-16.7465263981729,
18.8345732920406));
#150052=CARTESIAN_POINT('Ctrl Pts',(20.10597435513,-16.7890611724216,18.8387519701276));
#150053=CARTESIAN_POINT('Ctrl Pts',(20.1761635263181,-16.8352055143118,
18.8429306482147));
#150054=CARTESIAN_POINT('Ctrl Pts',(20.2439882104361,-16.8847468456079,
18.8471093263017));
#150055=CARTESIAN_POINT('Ctrl Pts',(20.3130286032089,-16.9351761696166,
18.8513629041863));
#150056=CARTESIAN_POINT('Ctrl Pts',(20.3796184709323,-16.9891252600217,
18.855616482071));
#150057=CARTESIAN_POINT('Ctrl Pts',(20.4433832089661,-17.0463218936806,
18.8598700599557));
#150058=CARTESIAN_POINT('Ctrl Pts',(20.5059117431836,-17.1024096590374,
18.8640411739367));
#150059=CARTESIAN_POINT('Ctrl Pts',(20.5657233532606,-17.1616198500918,
18.8682122879177));
#150060=CARTESIAN_POINT('Ctrl Pts',(20.62249704859,-17.2236542887874,18.8723834018987));
#150061=CARTESIAN_POINT('Ctrl Pts',(20.6792516929575,-17.285667911228,18.8765531162222));
#150062=CARTESIAN_POINT('Ctrl Pts',(20.7329701367994,-17.3505035600743,
18.8807228305456));
#150063=CARTESIAN_POINT('Ctrl Pts',(20.7833688571022,-17.4178268391281,
18.884892544869));
#150064=CARTESIAN_POINT('Ctrl Pts',(20.833765784002,-17.4851477225305,18.8890621108161));
#150065=CARTESIAN_POINT('Ctrl Pts',(20.8808429472263,-17.5549556913558,
18.8932316767632));
#150066=CARTESIAN_POINT('Ctrl Pts',(20.9243585153512,-17.6268850713133,
18.8974012427103));
#150067=CARTESIAN_POINT('Ctrl Pts',(20.9694040370984,-17.7013433994185,
18.9017174054456));
#150068=CARTESIAN_POINT('Ctrl Pts',(21.010632579499,-17.7780746406022,18.9060335681809));
#150069=CARTESIAN_POINT('Ctrl Pts',(21.0478271756457,-17.8566444407211,
18.9103497309162));
#150070=CARTESIAN_POINT('Ctrl Pts',(21.0838101617912,-17.9326548379834,
18.9145252951108));
#150071=CARTESIAN_POINT('Ctrl Pts',(21.1160178406327,-18.0103853983034,
18.9187008593055));
#150072=CARTESIAN_POINT('Ctrl Pts',(21.1443031849367,-18.0894233038831,
18.9228764235001));
#150073=CARTESIAN_POINT('Ctrl Pts',(21.1740171546712,-18.1724532259881,
18.9272628855057));
#150074=CARTESIAN_POINT('Ctrl Pts',(21.1994019743872,-18.2569254729962,
18.9316493475113));
#150075=CARTESIAN_POINT('Ctrl Pts',(21.2203472929199,-18.3423467059141,
18.9360358095169));
#150076=CARTESIAN_POINT('Ctrl Pts',(21.2412926114527,-18.4277679388319,
18.9404222715225));
#150077=CARTESIAN_POINT('Ctrl Pts',(21.2577983946029,-18.514137573478,18.9448087335281));
#150078=CARTESIAN_POINT('Ctrl Pts',(21.2698170137415,-18.6009557395155,
18.9491951955337));
#150079=CARTESIAN_POINT('Ctrl Pts',(21.2812826384042,-18.6837792730856,
18.9533798299225));
#150080=CARTESIAN_POINT('Ctrl Pts',(21.2887076244828,-18.7673192548721,
18.9575644643113));
#150081=CARTESIAN_POINT('Ctrl Pts',(21.2920126435715,-18.851147060883,18.9617490987001));
#150082=CARTESIAN_POINT('Ctrl Pts',(21.2953129583745,-18.934855548388,18.9659277767799));
#150083=CARTESIAN_POINT('Ctrl Pts',(21.294504936491,-19.0188505906155,18.9701064548596));
#150084=CARTESIAN_POINT('Ctrl Pts',(21.2895607321101,-19.1026961993451,
18.9742851329393));
#150085=CARTESIAN_POINT('Ctrl Pts',(21.2845279064127,-19.1880446804597,
18.9785387108258));
#150086=CARTESIAN_POINT('Ctrl Pts',(21.2752090914542,-19.2732378406073,
18.9827922887123));
#150087=CARTESIAN_POINT('Ctrl Pts',(21.2616304174303,-19.3578133473421,
18.9870458665988));
#150088=CARTESIAN_POINT('Ctrl Pts',(21.2483149925156,-19.4407491927399,
18.9912169805726));
#150089=CARTESIAN_POINT('Ctrl Pts',(21.2309034822292,-19.5230906447102,
18.9953880945464));
#150090=CARTESIAN_POINT('Ctrl Pts',(21.2094728610011,-19.6044064028251,
18.9995592085202));
#150091=CARTESIAN_POINT('Ctrl Pts',(21.1880494310247,-19.6856948746526,
19.0037289228364));
#150092=CARTESIAN_POINT('Ctrl Pts',(21.1626096856898,-19.7659578917013,
19.0078986371526));
#150093=CARTESIAN_POINT('Ctrl Pts',(21.1332813336496,-19.8447760536666,
19.0120683514689));
#150094=CARTESIAN_POINT('Ctrl Pts',(21.1039540252378,-19.9235914109442,
19.0162379174088));
#150095=CARTESIAN_POINT('Ctrl Pts',(21.0707385464732,-20.0009615845084,
19.0204074833488));
#150096=CARTESIAN_POINT('Ctrl Pts',(21.0338114728018,-20.0764852998459,
19.0245770492887));
#150097=CARTESIAN_POINT('Ctrl Pts',(20.9955860886931,-20.1546643360123,
19.0288932120326));
#150098=CARTESIAN_POINT('Ctrl Pts',(20.9533834858384,-20.2308641813314,
19.0332093747765));
#150099=CARTESIAN_POINT('Ctrl Pts',(20.9074514472649,-20.3046672933068,
19.0375255375203));
#150100=CARTESIAN_POINT('Ctrl Pts',(20.8630156401099,-20.3760662765228,
19.041701101708));
#150101=CARTESIAN_POINT('Ctrl Pts',(20.815089945817,-20.4452219153955,19.0458766658958));
#150102=CARTESIAN_POINT('Ctrl Pts',(20.7639418957712,-20.5117871328463,
19.0500522300835));
#150103=CARTESIAN_POINT('Ctrl Pts',(20.7102104791443,-20.5817144014031,
19.0544386921054));
#150104=CARTESIAN_POINT('Ctrl Pts',(20.6529230087043,-20.6487822429891,
19.0588251541273));
#150105=CARTESIAN_POINT('Ctrl Pts',(20.5924345734849,-20.7126308346942,
19.0632116161493));
#150106=CARTESIAN_POINT('Ctrl Pts',(20.5319461382654,-20.7764794263994,
19.0675980781712));
#150107=CARTESIAN_POINT('Ctrl Pts',(20.4682572109593,-20.837108423261,19.0719845401932));
#150108=CARTESIAN_POINT('Ctrl Pts',(20.4017623229462,-20.8942072068039,
19.0763710022151));
#150109=CARTESIAN_POINT('Ctrl Pts',(20.3665290238934,-20.9244618410507,
19.0786952339391));
#150110=CARTESIAN_POINT('Ctrl Pts',(20.3304358504976,-20.9537886281019,
19.0810194656631));
#150111=CARTESIAN_POINT('Ctrl Pts',(20.2935357468249,-20.9821350335323,
19.0833436973871));
#150112=CARTESIAN_POINT('Origin',(18.734,-18.952,-1.76670989022851));
#150113=CARTESIAN_POINT('',(20.2935357468249,-20.9821350335323,19.9498236325831));
#150114=CARTESIAN_POINT('',(20.2935357468249,-20.9821350335323,19.8833624910577));
#150115=CARTESIAN_POINT('',(20.2935357468249,-20.9821350335323,-1.76670989022851));
#150116=CARTESIAN_POINT('',(16.1740009418753,-18.9498040034616,19.4332901097715));
#150117=CARTESIAN_POINT('Ctrl Pts',(16.1740009418753,-18.9498040034616,
19.4332901097715));
#150118=CARTESIAN_POINT('Ctrl Pts',(16.1741094126172,-18.8233534412475,
19.4395926510339));
#150119=CARTESIAN_POINT('Ctrl Pts',(16.1835900621658,-18.6972910723228,
19.4458951922963));
#150120=CARTESIAN_POINT('Ctrl Pts',(16.2022529884095,-18.572715055265,19.4521977335588));
#150121=CARTESIAN_POINT('Ctrl Pts',(16.2064836512073,-18.5444751579424,
19.4536264444963));
#150122=CARTESIAN_POINT('Ctrl Pts',(16.2111860003678,-18.5163115073012,
19.4550551554338));
#150123=CARTESIAN_POINT('Ctrl Pts',(16.2163575306343,-18.4882367021355,
19.4564838663713));
#150124=CARTESIAN_POINT('Ctrl Pts',(16.2315047248245,-18.4060067810516,
19.4606685004925));
#150125=CARTESIAN_POINT('Ctrl Pts',(16.25071296974,-18.3243667083971,19.4648531346137));
#150126=CARTESIAN_POINT('Ctrl Pts',(16.2739228554016,-18.2437483197165,
19.469037768735));
#150127=CARTESIAN_POINT('Ctrl Pts',(16.2970997046629,-18.1632446813365,
19.4732164465473));
#150128=CARTESIAN_POINT('Ctrl Pts',(16.3242667547544,-18.0837602766464,
19.4773951243597));
#150129=CARTESIAN_POINT('Ctrl Pts',(16.3553134075097,-18.0057177510347,
19.4815738021721));
#150130=CARTESIAN_POINT('Ctrl Pts',(16.3869165517615,-17.9262763628078,
19.4858273801254));
#150131=CARTESIAN_POINT('Ctrl Pts',(16.4225396637624,-17.8483295278622,
19.4900809580788));
#150132=CARTESIAN_POINT('Ctrl Pts',(16.4620126245779,-17.7723079359755,
19.4943345360321));
#150133=CARTESIAN_POINT('Ctrl Pts',(16.5007203219077,-17.6977601769908,
19.498505649741));
#150134=CARTESIAN_POINT('Ctrl Pts',(16.5431297041304,-17.6250641048156,
19.5026767634499));
#150135=CARTESIAN_POINT('Ctrl Pts',(16.5890321382659,-17.5546049691916,
19.5068478771588));
#150136=CARTESIAN_POINT('Ctrl Pts',(16.634919169412,-17.484169476787,19.5110175912116));
#150137=CARTESIAN_POINT('Ctrl Pts',(16.6842966737064,-17.4159698153114,
19.5151873052644));
#150138=CARTESIAN_POINT('Ctrl Pts',(16.7369115952916,-17.3503639914827,
19.5193570193173));
#150139=CARTESIAN_POINT('Ctrl Pts',(16.7895246446353,-17.2847605021618,
19.5235265849956));
#150140=CARTESIAN_POINT('Ctrl Pts',(16.8453745937438,-17.2217510253186,
19.527696150674));
#150141=CARTESIAN_POINT('Ctrl Pts',(16.9041676934287,-17.1616610014224,
19.5318657163523));
#150142=CARTESIAN_POINT('Ctrl Pts',(16.9650278943521,-17.0994582778473,
19.5361818794107));
#150143=CARTESIAN_POINT('Ctrl Pts',(17.0290416909462,-17.0403845007301,
19.540498042469));
#150144=CARTESIAN_POINT('Ctrl Pts',(17.0958426218327,-16.984758173392,19.5448142055274));
#150145=CARTESIAN_POINT('Ctrl Pts',(17.1604675106391,-16.9309438751296,
19.5489897694607));
#150146=CARTESIAN_POINT('Ctrl Pts',(17.2277003349621,-16.8803561190544,
19.5531653333939));
#150147=CARTESIAN_POINT('Ctrl Pts',(17.2971780335747,-16.8332403069725,
19.5573408973272));
#150148=CARTESIAN_POINT('Ctrl Pts',(17.370164900217,-16.7837447773015,19.5617273599481));
#150149=CARTESIAN_POINT('Ctrl Pts',(17.4456288796107,-16.7380814487272,
19.5661138225691));
#150150=CARTESIAN_POINT('Ctrl Pts',(17.523119783767,-16.696480303359,19.57050028519));
#150151=CARTESIAN_POINT('Ctrl Pts',(17.6006106879233,-16.6548791579908,
19.5748867478109));
#150152=CARTESIAN_POINT('Ctrl Pts',(17.6801279596806,-16.6173403747401,
19.5792732104318));
#150153=CARTESIAN_POINT('Ctrl Pts',(17.7611994326909,-16.5840348279075,
19.5836596730528));
#150154=CARTESIAN_POINT('Ctrl Pts',(17.8385406770861,-16.5522617227492,
19.587844307487));
#150155=CARTESIAN_POINT('Ctrl Pts',(17.9175841221718,-16.5242225928453,
19.5920289419213));
#150156=CARTESIAN_POINT('Ctrl Pts',(17.9979345050501,-16.5001012282021,
19.5962135763556));
#150157=CARTESIAN_POINT('Ctrl Pts',(18.078170519057,-16.4760141973499,19.6003922544782));
#150158=CARTESIAN_POINT('Ctrl Pts',(18.1597093389465,-16.4558339863015,
19.6045709326009));
#150159=CARTESIAN_POINT('Ctrl Pts',(18.2421357220942,-16.4396963694409,
19.6087496107236));
#150160=CARTESIAN_POINT('Ctrl Pts',(18.3260395379465,-16.4232694975869,
19.613003188599));
#150161=CARTESIAN_POINT('Ctrl Pts',(18.4108626031779,-16.411031755533,19.6172567664745));
#150162=CARTESIAN_POINT('Ctrl Pts',(18.4961506937665,-16.4030732243699,
19.6215103443499));
#150163=CARTESIAN_POINT('Ctrl Pts',(18.5797853091396,-16.3952689847841,
19.6256814583603));
#150164=CARTESIAN_POINT('Ctrl Pts',(18.6638666007976,-16.3915795598322,
19.6298525723707));
#150165=CARTESIAN_POINT('Ctrl Pts',(18.7479577055537,-16.3920380505844,
19.634023686381));
#150166=CARTESIAN_POINT('Ctrl Pts',(18.8320205926793,-16.3924963874854,
19.6381934007314));
#150167=CARTESIAN_POINT('Ctrl Pts',(18.9160928267199,-16.3970998732974,
19.6423631150818));
#150168=CARTESIAN_POINT('Ctrl Pts',(18.9997364062972,-16.4058295103493,
19.6465328294322));
#150169=CARTESIAN_POINT('Ctrl Pts',(19.0833770094284,-16.4145588367581,
19.6507023954039));
#150170=CARTESIAN_POINT('Ctrl Pts',(19.1665885309651,-16.4274139738732,
19.6548719613755));
#150171=CARTESIAN_POINT('Ctrl Pts',(19.2489383260598,-16.444324079879,19.6590415273471));
#150172=CARTESIAN_POINT('Ctrl Pts',(19.3341834370064,-16.461828724073,19.6633576900461));
#150173=CARTESIAN_POINT('Ctrl Pts',(19.4185045808358,-16.4836786817424,
19.667673852745));
#150174=CARTESIAN_POINT('Ctrl Pts',(19.5014355882166,-16.5097382167469,
19.6719900154439));
#150175=CARTESIAN_POINT('Ctrl Pts',(19.5816651279085,-16.5349488655021,
19.6761655796569));
#150176=CARTESIAN_POINT('Ctrl Pts',(19.6605932821671,-16.5640988419222,
19.68034114387));
#150177=CARTESIAN_POINT('Ctrl Pts',(19.7378171886914,-16.597015700331,19.684516708083));
#150178=CARTESIAN_POINT('Ctrl Pts',(19.81894148943,-16.6315951102716,19.6889031700249));
#150179=CARTESIAN_POINT('Ctrl Pts',(19.8981843303164,-16.6703316765417,
19.6932896319667));
#150180=CARTESIAN_POINT('Ctrl Pts',(19.9751086547792,-16.7129713474294,
19.6976760939086));
#150181=CARTESIAN_POINT('Ctrl Pts',(20.0520329792421,-16.7556110183172,
19.7020625558505));
#150182=CARTESIAN_POINT('Ctrl Pts',(20.1266383352645,-16.8021534221799,
19.7064490177923));
#150183=CARTESIAN_POINT('Ctrl Pts',(20.1985254700754,-16.8522940330845,
19.7108354797342));
#150184=CARTESIAN_POINT('Ctrl Pts',(20.2671049874831,-16.9001276114767,
19.7150201150503));
#150185=CARTESIAN_POINT('Ctrl Pts',(20.3334661901338,-16.9514136024954,
19.7192047503663));
#150186=CARTESIAN_POINT('Ctrl Pts',(20.3972405913418,-17.0059191344364,
19.7233893856824));
#150187=CARTESIAN_POINT('Ctrl Pts',(20.4609242176689,-17.0603470845722,
19.7275680646937));
#150188=CARTESIAN_POINT('Ctrl Pts',(20.5220280094205,-17.117985176789,19.7317467437049));
#150189=CARTESIAN_POINT('Ctrl Pts',(20.5802130388192,-17.1785577496591,
19.7359254227162));
#150190=CARTESIAN_POINT('Ctrl Pts',(20.6394409766887,-17.2402160253296,
19.7401790003703));
#150191=CARTESIAN_POINT('Ctrl Pts',(20.6956440915883,-17.304914740034,19.7444325780245));
#150192=CARTESIAN_POINT('Ctrl Pts',(20.7485007769389,-17.3723207225159,
19.7486861556786));
#150193=CARTESIAN_POINT('Ctrl Pts',(20.8003327466916,-17.4384199268452,
19.7528572705877));
#150194=CARTESIAN_POINT('Ctrl Pts',(20.8489465843956,-17.5071219871298,
19.7570283854968));
#150195=CARTESIAN_POINT('Ctrl Pts',(20.8940779914901,-17.5780774873814,
19.7611995004059));
#150196=CARTESIAN_POINT('Ctrl Pts',(20.9391942543019,-17.6490091778247,
19.7653692156568));
#150197=CARTESIAN_POINT('Ctrl Pts',(20.9808301606011,-17.7221924186382,
19.7695389309077));
#150198=CARTESIAN_POINT('Ctrl Pts',(21.0187646025466,-17.7972486367404,
19.7737086461586));
#150199=CARTESIAN_POINT('Ctrl Pts',(21.0566976946058,-17.8723021839882,
19.7778782130313));
#150200=CARTESIAN_POINT('Ctrl Pts',(21.0909293774472,-17.9492281650514,
19.7820477799041));
#150201=CARTESIAN_POINT('Ctrl Pts',(21.1212850353415,-18.0276244485954,
19.7862173467768));
#150202=CARTESIAN_POINT('Ctrl Pts',(21.1527079456952,-18.1087770099546,
19.7905335084134));
#150203=CARTESIAN_POINT('Ctrl Pts',(21.1799770112843,-18.1915046958175,
19.79484967005));
#150204=CARTESIAN_POINT('Ctrl Pts',(21.2029540362447,-18.275342060631,19.7991658316865));
#150205=CARTESIAN_POINT('Ctrl Pts',(21.2251825975804,-18.3564484705861,
19.8033413967929));
#150206=CARTESIAN_POINT('Ctrl Pts',(21.2433943908903,-18.438592905029,19.8075169618993));
#150207=CARTESIAN_POINT('Ctrl Pts',(21.2575163539161,-18.5213432787964,
19.8116925270058));
#150208=CARTESIAN_POINT('Ctrl Pts',(21.2723515733336,-18.6082731163458,
19.8160789869074));
#150209=CARTESIAN_POINT('Ctrl Pts',(21.2826728879139,-18.6958711330843,
19.8204654468091));
#150210=CARTESIAN_POINT('Ctrl Pts',(21.2884573444653,-18.7836323210737,
19.8248519067107));
#150211=CARTESIAN_POINT('Ctrl Pts',(21.2942418010168,-18.8713935090632,
19.8292383666124));
#150212=CARTESIAN_POINT('Ctrl Pts',(21.2954894673635,-18.959317287068,19.833624826514));
#150213=CARTESIAN_POINT('Ctrl Pts',(21.2922402934573,-19.0469031133929,
19.8380112864157));
#150214=CARTESIAN_POINT('Ctrl Pts',(21.2891403572398,-19.1304660383082,
19.8421962719868));
#150215=CARTESIAN_POINT('Ctrl Pts',(21.2819360687556,-19.214032439079,19.8463812575579));
#150216=CARTESIAN_POINT('Ctrl Pts',(21.2706237823411,-19.2971663176808,
19.8505662431291));
#150217=CARTESIAN_POINT('Ctrl Pts',(21.2593308428958,-19.380158015602,19.8547440712801));
#150218=CARTESIAN_POINT('Ctrl Pts',(21.2439439373072,-19.4627182103198,
19.8589218994311));
#150219=CARTESIAN_POINT('Ctrl Pts',(21.2245113674097,-19.5444129715016,
19.8630997275821));
#150220=CARTESIAN_POINT('Ctrl Pts',(21.2050977076966,-19.6260282340369,
19.8672734902131));
#150221=CARTESIAN_POINT('Ctrl Pts',(21.1816463054655,-19.7067792901258,
19.8714472528441));
#150222=CARTESIAN_POINT('Ctrl Pts',(21.1542568723985,-19.7862401762129,
19.8756210154751));
#150223=CARTESIAN_POINT('Ctrl Pts',(21.1268858754546,-19.8656475763201,
19.8797919687015));
#150224=CARTESIAN_POINT('Ctrl Pts',(21.0955822614975,-19.9437660975122,
19.8839629219279));
#150225=CARTESIAN_POINT('Ctrl Pts',(21.060495805953,-20.0201840969061,19.8881338751542));
#150226=CARTESIAN_POINT('Ctrl Pts',(21.0254224420283,-20.0965735828645,
19.8923032720953));
#150227=CARTESIAN_POINT('Ctrl Pts',(20.9865692332683,-20.1712633904095,
19.8964726690364));
#150228=CARTESIAN_POINT('Ctrl Pts',(20.9441338701724,-20.2438623285462,
19.9006420659775));
#150229=CARTESIAN_POINT('Ctrl Pts',(20.901681864461,-20.316489739073,19.9048130981037));
#150230=CARTESIAN_POINT('Ctrl Pts',(20.8556451222065,-20.3870242397313,
19.9089841302298));
#150231=CARTESIAN_POINT('Ctrl Pts',(20.8062666824532,-20.4551003947822,
19.9131551623559));
#150232=CARTESIAN_POINT('Ctrl Pts',(20.756880639097,-20.5231870326279,19.9173268367638));
#150233=CARTESIAN_POINT('Ctrl Pts',(20.7041521537777,-20.5888142054936,
19.9214985111717));
#150234=CARTESIAN_POINT('Ctrl Pts',(20.6483656430248,-20.651648253259,19.9256701855796));
#150235=CARTESIAN_POINT('Ctrl Pts',(20.592510493086,-20.7145596114319,19.9298469927755));
#150236=CARTESIAN_POINT('Ctrl Pts',(20.5335901158211,-20.7746706419221,
19.9340237999715));
#150237=CARTESIAN_POINT('Ctrl Pts',(20.4719267478643,-20.8316836486648,
19.9382006071674));
#150238=CARTESIAN_POINT('Ctrl Pts',(20.4147287607129,-20.8845680326222,
19.9420749489727));
#150239=CARTESIAN_POINT('Ctrl Pts',(20.3551712738705,-20.9347870462732,
19.9459492907779));
#150240=CARTESIAN_POINT('Ctrl Pts',(20.2935357468249,-20.9821350335323,
19.9498236325831));
#150241=CARTESIAN_POINT('Ctrl Pts',(20.2912840470176,-20.9792340293575,
19.149828721203));
#150242=CARTESIAN_POINT('Ctrl Pts',(20.0133685920828,-21.1947985603089,
19.1672632318048));
#150243=CARTESIAN_POINT('Ctrl Pts',(18.9167592873257,-21.7455418715826,
19.2270896779671));
#150244=CARTESIAN_POINT('Ctrl Pts',(16.8320816481898,-21.2027757351818,
19.3215765971073));
#150245=CARTESIAN_POINT('Ctrl Pts',(16.1790132429278,-19.6455867561426,
19.3986290056455));
#150246=CARTESIAN_POINT('Ctrl Pts',(16.1726852643248,-18.9498155443718,
19.4332894786233));
#150247=CARTESIAN_POINT('',(16.1740010149448,-18.9542795868247,19.3667098901939));
#150248=CARTESIAN_POINT('Ctrl Pts',(20.2935357468249,-20.9821350335323,
19.0833436973871));
#150249=CARTESIAN_POINT('Ctrl Pts',(20.2271546507136,-21.0331285342547,
19.0875248522918));
#150250=CARTESIAN_POINT('Ctrl Pts',(20.1581601935485,-21.0809470712519,
19.0917060071965));
#150251=CARTESIAN_POINT('Ctrl Pts',(20.0868893516481,-21.1253132314964,
19.0958871621012));
#150252=CARTESIAN_POINT('Ctrl Pts',(20.0157068422532,-21.1696244046804,
19.1000631349163));
#150253=CARTESIAN_POINT('Ctrl Pts',(19.9422539410436,-21.210491460075,19.1042391077314));
#150254=CARTESIAN_POINT('Ctrl Pts',(19.8668989098351,-21.2476785620148,
19.1084150805465));
#150255=CARTESIAN_POINT('Ctrl Pts',(19.7916121680322,-21.2848319636821,
19.1125872689467));
#150256=CARTESIAN_POINT('Ctrl Pts',(19.7144271328449,-21.3183118364559,
19.116759457347));
#150257=CARTESIAN_POINT('Ctrl Pts',(19.6357379828143,-21.3479275052368,
19.1209316457472));
#150258=CARTESIAN_POINT('Ctrl Pts',(19.5570861865498,-21.3775291154496,
19.1251018536082));
#150259=CARTESIAN_POINT('Ctrl Pts',(19.4769321230311,-21.4032700021637,
19.1292720614691));
#150260=CARTESIAN_POINT('Ctrl Pts',(19.3956902332643,-21.4250074878986,
19.1334422693301));
#150261=CARTESIAN_POINT('Ctrl Pts',(19.3144625382898,-21.4467411756041,
19.1376117485617));
#150262=CARTESIAN_POINT('Ctrl Pts',(19.232147839027,-21.4644727333422,19.1417812277932));
#150263=CARTESIAN_POINT('Ctrl Pts',(19.1491747117678,-21.4781096489877,
19.1459507070247));
#150264=CARTESIAN_POINT('Ctrl Pts',(19.0661911921266,-21.4917482726564,
19.1501207084834));
#150265=CARTESIAN_POINT('Ctrl Pts',(18.9825495348782,-21.5012911625872,
19.1542907099421));
#150266=CARTESIAN_POINT('Ctrl Pts',(18.898686097081,-21.506697338126,19.1584607114008));
#150267=CARTESIAN_POINT('Ctrl Pts',(18.8147324386056,-21.5121093296538,
19.1626351989665));
#150268=CARTESIAN_POINT('Ctrl Pts',(18.7305569831965,-21.5133756931289,
19.1668096865322));
#150269=CARTESIAN_POINT('Ctrl Pts',(18.6465982461443,-21.5105075597744,
19.170984174098));
#150270=CARTESIAN_POINT('Ctrl Pts',(18.56259038681,-21.5076377483426,19.1751611040582));
#150271=CARTESIAN_POINT('Ctrl Pts',(18.4787999566344,-21.5006286627532,
19.1793380340184));
#150272=CARTESIAN_POINT('Ctrl Pts',(18.3956600869716,-21.489543320468,19.1835149639786));
#150273=CARTESIAN_POINT('Ctrl Pts',(18.3123798101434,-21.478439257183,19.187698947966));
#150274=CARTESIAN_POINT('Ctrl Pts',(18.2297527398045,-21.4632452754277,
19.1918829319533));
#150275=CARTESIAN_POINT('Ctrl Pts',(18.1482012305168,-21.4440754004789,
19.1960669159406));
#150276=CARTESIAN_POINT('Ctrl Pts',(18.0996034855829,-21.4326517897902,
19.1985602135926));
#150277=CARTESIAN_POINT('Ctrl Pts',(18.0513874070201,-21.4198172442631,
19.2010535112446));
#150278=CARTESIAN_POINT('Ctrl Pts',(18.0036392138265,-21.4056041086573,
19.2035468088966));
#150279=CARTESIAN_POINT('Ctrl Pts',(17.9235008748327,-21.3817494451997,
19.2077314433107));
#150280=CARTESIAN_POINT('Ctrl Pts',(17.8443833236107,-21.3539201055369,
19.2119160777248));
#150281=CARTESIAN_POINT('Ctrl Pts',(17.7667095652025,-21.3222213429866,
19.2161007121389));
#150282=CARTESIAN_POINT('Ctrl Pts',(17.6891463657735,-21.2905676997005,
19.2202793902439));
#150283=CARTESIAN_POINT('Ctrl Pts',(17.6130232994484,-21.2550557457776,
19.224458068349));
#150284=CARTESIAN_POINT('Ctrl Pts',(17.5387487593335,-21.2158406462658,
19.228636746454));
#150285=CARTESIAN_POINT('Ctrl Pts',(17.4631429019428,-21.1759226445297,
19.2328903243342));
#150286=CARTESIAN_POINT('Ctrl Pts',(17.3894529543292,-21.1321675712374,
19.2371439022144));
#150287=CARTESIAN_POINT('Ctrl Pts',(17.3180889421044,-21.0847906311049,
19.2413974800945));
#150288=CARTESIAN_POINT('Ctrl Pts',(17.2481084600712,-21.0383321851128,
19.2455685940936));
#150289=CARTESIAN_POINT('Ctrl Pts',(17.1803649335769,-20.9883913190988,
19.2497397080926));
#150290=CARTESIAN_POINT('Ctrl Pts',(17.1152190899104,-20.9352166712514,
19.2539108220917));
#150291=CARTESIAN_POINT('Ctrl Pts',(17.0500951065615,-20.882059866671,19.2580805364331));
#150292=CARTESIAN_POINT('Ctrl Pts',(16.987567430963,-20.8256717259896,19.2622502507746));
#150293=CARTESIAN_POINT('Ctrl Pts',(16.9279649526829,-20.7663421418967,
19.266419965116));
#150294=CARTESIAN_POINT('Ctrl Pts',(16.8683645953157,-20.707014669006,19.270589531081));
#150295=CARTESIAN_POINT('Ctrl Pts',(16.8116895537435,-20.6447462859623,
19.2747590970461));
#150296=CARTESIAN_POINT('Ctrl Pts',(16.7582319859876,-20.5798638624914,
19.2789286630111));
#150297=CARTESIAN_POINT('Ctrl Pts',(16.7028949166956,-20.5127002537797,
19.283244825725));
#150298=CARTESIAN_POINT('Ctrl Pts',(16.6510061189315,-20.4427357723036,
19.2875609884389));
#150299=CARTESIAN_POINT('Ctrl Pts',(16.6028430768027,-20.370368840855,19.2918771511528));
#150300=CARTESIAN_POINT('Ctrl Pts',(16.5562489402055,-20.3003592538355,
19.2960527153651));
#150301=CARTESIAN_POINT('Ctrl Pts',(16.5131417547233,-20.2281017614849,
19.3002282795774));
#150302=CARTESIAN_POINT('Ctrl Pts',(16.4737266859787,-20.1539835880423,
19.3044038437897));
#150303=CARTESIAN_POINT('Ctrl Pts',(16.4323208564678,-20.0761218830912,
19.3087903057544));
#150304=CARTESIAN_POINT('Ctrl Pts',(16.3949901703475,-19.9962071202823,
19.3131767677191));
#150305=CARTESIAN_POINT('Ctrl Pts',(16.3619151438293,-19.9147115015028,
19.3175632296838));
#150306=CARTESIAN_POINT('Ctrl Pts',(16.3288401173112,-19.8332158827234,
19.3219496916486));
#150307=CARTESIAN_POINT('Ctrl Pts',(16.3000208686933,-19.7501399810729,
19.3263361536133));
#150308=CARTESIAN_POINT('Ctrl Pts',(16.2755767948947,-19.6659715292643,
19.330722615578));
#150309=CARTESIAN_POINT('Ctrl Pts',(16.2465257453528,-19.5659398453678,
19.3359357942364));
#150310=CARTESIAN_POINT('Ctrl Pts',(16.2235642356486,-19.464065347825,19.3411489728948));
#150311=CARTESIAN_POINT('Ctrl Pts',(16.2068848499427,-19.3610098022674,
19.3463621515532));
#150312=CARTESIAN_POINT('Ctrl Pts',(16.1904712789856,-19.2595966243872,
19.3514922492277));
#150313=CARTESIAN_POINT('Ctrl Pts',(16.1801412137013,-19.1570396545395,
19.3566223469021));
#150314=CARTESIAN_POINT('Ctrl Pts',(16.1760324691903,-19.0539907413612,
19.3617524445766));
#150315=CARTESIAN_POINT('Ctrl Pts',(16.1747089805837,-19.0207971314519,
19.363404926449));
#150316=CARTESIAN_POINT('Ctrl Pts',(16.1740306434087,-18.9875526505075,
19.3650574083215));
#150317=CARTESIAN_POINT('Ctrl Pts',(16.1740010149447,-18.9542795868247,
19.3667098901939));
#150318=CARTESIAN_POINT('Ctrl Pts',(16.1740010149441,-18.9542795861284,
19.3667098902285));
#150319=CARTESIAN_POINT('Ctrl Pts',(16.173926819566,-18.8709574030249,19.3708480242598));
#150320=CARTESIAN_POINT('Ctrl Pts',(16.1779248169782,-18.7875513930795,
19.374986158291));
#150321=CARTESIAN_POINT('Ctrl Pts',(16.1859928190662,-18.7044936245066,
19.3791242923222));
#150322=CARTESIAN_POINT('Ctrl Pts',(16.1940571655296,-18.6214734895413,
19.3832605513584));
#150323=CARTESIAN_POINT('Ctrl Pts',(16.2061878113244,-18.5388017480886,
19.3873968103945));
#150324=CARTESIAN_POINT('Ctrl Pts',(16.2223305526747,-18.456907496146,19.3915330694306));
#150325=CARTESIAN_POINT('Ctrl Pts',(16.238471016352,-18.3750247991377,19.3956687448579));
#150326=CARTESIAN_POINT('Ctrl Pts',(16.2586223602409,-18.2939198329686,
19.3998044202853));
#150327=CARTESIAN_POINT('Ctrl Pts',(16.2826791433887,-18.2140121559657,
19.4039400957127));
#150328=CARTESIAN_POINT('Ctrl Pts',(16.3067400382202,-18.1340908214803,
19.4080764779922));
#150329=CARTESIAN_POINT('Ctrl Pts',(16.3347075604887,-18.0553676300741,
19.4122128602717));
#150330=CARTESIAN_POINT('Ctrl Pts',(16.3664266589084,-17.9782461940757,
19.4163492425513));
#150331=CARTESIAN_POINT('Ctrl Pts',(16.3981808282496,-17.9010394870584,
19.4204901983132));
#150332=CARTESIAN_POINT('Ctrl Pts',(16.4336946710468,-17.8254385023485,
19.4246311540751));
#150333=CARTESIAN_POINT('Ctrl Pts',(16.4727655806441,-17.7518254707252,
19.4287721098371));
#150334=CARTESIAN_POINT('Ctrl Pts',(16.511861777281,-17.6781647960941,19.4329157456624));
#150335=CARTESIAN_POINT('Ctrl Pts',(16.5545193804023,-17.6064950352306,
19.4370593814876));
#150336=CARTESIAN_POINT('Ctrl Pts',(16.6004918491533,-17.5371703387789,
19.4412030173129));
#150337=CARTESIAN_POINT('Ctrl Pts',(16.6465392454185,-17.4677326545476,
19.4453534065787));
#150338=CARTESIAN_POINT('Ctrl Pts',(16.6959120078393,-17.4006480348314,
19.4495037958445));
#150339=CARTESIAN_POINT('Ctrl Pts',(16.7483230702929,-17.3362379102018,
19.4536541851102));
#150340=CARTESIAN_POINT('Ctrl Pts',(16.7661884610673,-17.3142823917967,
19.4550689308266));
#150341=CARTESIAN_POINT('Ctrl Pts',(16.7844065661398,-17.292637312599,19.4564836765431));
#150342=CARTESIAN_POINT('Ctrl Pts',(16.8029650799467,-17.2713143846827,
19.4578984222595));
#150343=CARTESIAN_POINT('Ctrl Pts',(16.857858757406,-17.2082439287342,19.4620830566462));
#150344=CARTESIAN_POINT('Ctrl Pts',(16.9159478005841,-17.1477482923964,
19.466267691033));
#150345=CARTESIAN_POINT('Ctrl Pts',(16.9769612646036,-17.0901689436695,
19.4704523254198));
#150346=CARTESIAN_POINT('Ctrl Pts',(17.0378878835037,-17.0326715520237,
19.4746310034971));
#150347=CARTESIAN_POINT('Ctrl Pts',(17.1017303233984,-16.9780825158866,
19.4788096815744));
#150348=CARTESIAN_POINT('Ctrl Pts',(17.1681782563647,-16.9267093376113,
19.4829883596517));
#150349=CARTESIAN_POINT('Ctrl Pts',(17.2358172209073,-16.8744153319337,
19.4872419375387));
#150350=CARTESIAN_POINT('Ctrl Pts',(17.306155687672,-16.8254539702902,19.4914955154258));
#150351=CARTESIAN_POINT('Ctrl Pts',(17.3788280009098,-16.780109382846,19.4957490933128));
#150352=CARTESIAN_POINT('Ctrl Pts',(17.4500914193922,-16.7356438888086,
19.4999202072833));
#150353=CARTESIAN_POINT('Ctrl Pts',(17.5235985912761,-16.6946564386902,
19.5040913212538));
#150354=CARTESIAN_POINT('Ctrl Pts',(17.5989738385239,-16.657372445741,19.5082624352243));
#150355=CARTESIAN_POINT('Ctrl Pts',(17.6743237928742,-16.6201009637983,
19.5124321495369));
#150356=CARTESIAN_POINT('Ctrl Pts',(17.7515401656506,-16.5865306747361,
19.5166018638495));
#150357=CARTESIAN_POINT('Ctrl Pts',(17.8302229081151,-16.556840930505,19.5207715781621));
#150358=CARTESIAN_POINT('Ctrl Pts',(17.9089028507046,-16.5271522427644,
19.5249411440981));
#150359=CARTESIAN_POINT('Ctrl Pts',(17.9890486285237,-16.5013439869149,
19.5291107100341));
#150360=CARTESIAN_POINT('Ctrl Pts',(18.070241741943,-16.4795467699346,19.5332802759701));
#150361=CARTESIAN_POINT('Ctrl Pts',(18.1542895053982,-16.4569831896062,
19.5375964387176));
#150362=CARTESIAN_POINT('Ctrl Pts',(18.2394591140174,-16.4387180891091,
19.5419126014652));
#150363=CARTESIAN_POINT('Ctrl Pts',(18.3252730114505,-16.4248390932053,
19.5462287642128));
#150364=CARTESIAN_POINT('Ctrl Pts',(18.4082915298621,-16.4114122041881,
19.5504043283958));
#150365=CARTESIAN_POINT('Ctrl Pts',(18.4919125329018,-16.402090058559,19.5545798925788));
#150366=CARTESIAN_POINT('Ctrl Pts',(18.5756985998716,-16.3968990887408,
19.5587554567618));
#150367=CARTESIAN_POINT('Ctrl Pts',(18.6637165024315,-16.3914459353448,
19.5631419187917));
#150368=CARTESIAN_POINT('Ctrl Pts',(18.75191599805,-16.3905522627807,19.5675283808215));
#150369=CARTESIAN_POINT('Ctrl Pts',(18.8397925195445,-16.3941868827437,
19.5719148428514));
#150370=CARTESIAN_POINT('Ctrl Pts',(18.927669041039,-16.3978215027067,19.5763013048812));
#150371=CARTESIAN_POINT('Ctrl Pts',(19.0152220177589,-16.4059842855989,
19.580687766911));
#150372=CARTESIAN_POINT('Ctrl Pts',(19.1019580505821,-16.4185819782334,
19.5850742289409));
#150373=CARTESIAN_POINT('Ctrl Pts',(19.1847032324225,-16.4306000327129,
19.5892588634749));
#150374=CARTESIAN_POINT('Ctrl Pts',(19.2670129891878,-16.4466985853912,
19.5934434980089));
#150375=CARTESIAN_POINT('Ctrl Pts',(19.3484535429803,-16.4668346446325,
19.5976281325429));
#150376=CARTESIAN_POINT('Ctrl Pts',(19.4297781762392,-16.4869420426893,
19.6018068107684));
#150377=CARTESIAN_POINT('Ctrl Pts',(19.5102356212338,-16.5110754227039,
19.6059854889938));
#150378=CARTESIAN_POINT('Ctrl Pts',(19.5893993425081,-16.5391402931715,
19.6101641672193));
#150379=CARTESIAN_POINT('Ctrl Pts',(19.6699820131946,-16.5677082050677,
19.6144177450694));
#150380=CARTESIAN_POINT('Ctrl Pts',(19.7492236469542,-16.6003498680241,
19.6186713229195));
#150381=CARTESIAN_POINT('Ctrl Pts',(19.8266874127979,-16.6369116176886,
19.6229249007697));
#150382=CARTESIAN_POINT('Ctrl Pts',(19.9026493955953,-16.6727645480079,
19.6270960148894));
#150383=CARTESIAN_POINT('Ctrl Pts',(19.9769013948655,-16.7123867192901,
19.6312671290091));
#150384=CARTESIAN_POINT('Ctrl Pts',(20.0490505263221,-16.7555842576552,
19.6354382431289));
#150385=CARTESIAN_POINT('Ctrl Pts',(20.1211754474381,-16.7987673006675,
19.6396079575908));
#150386=CARTESIAN_POINT('Ctrl Pts',(20.1911985077801,-16.8455230919237,
19.6437776720528));
#150387=CARTESIAN_POINT('Ctrl Pts',(20.2587523619284,-16.8956123335339,
19.6479473865147));
#150388=CARTESIAN_POINT('Ctrl Pts',(20.3263038122145,-16.9456997927494,
19.6521169526));
#150389=CARTESIAN_POINT('Ctrl Pts',(20.3913858619795,-16.9991201917914,
19.6562865186852));
#150390=CARTESIAN_POINT('Ctrl Pts',(20.4536621654943,-17.0555923337617,
19.6604560847705));
#150391=CARTESIAN_POINT('Ctrl Pts',(20.5181280223232,-17.1140499623236,
19.6647722473415));
#150392=CARTESIAN_POINT('Ctrl Pts',(20.5795867716016,-17.1757775704163,
19.6690884099125));
#150393=CARTESIAN_POINT('Ctrl Pts',(20.637706242632,-17.2404210384081,19.6734045724834));
#150394=CARTESIAN_POINT('Ctrl Pts',(20.6939324820634,-17.3029587567415,
19.6775801368139));
#150395=CARTESIAN_POINT('Ctrl Pts',(20.747033395186,-17.3682248892184,19.6817557011444));
#150396=CARTESIAN_POINT('Ctrl Pts',(20.796749988967,-17.4358659416078,19.6859312654749));
#150397=CARTESIAN_POINT('Ctrl Pts',(20.848977644148,-17.506923375185,19.6903177271661));
#150398=CARTESIAN_POINT('Ctrl Pts',(20.8974697909667,-17.5806014598665,
19.6947041888574));
#150399=CARTESIAN_POINT('Ctrl Pts',(20.9419795412608,-17.6564590529923,
19.6990906505486));
#150400=CARTESIAN_POINT('Ctrl Pts',(20.9864892915549,-17.732316646118,19.7034771122398));
#150401=CARTESIAN_POINT('Ctrl Pts',(21.0270164454133,-17.8103531977127,
19.7078635739311));
#150402=CARTESIAN_POINT('Ctrl Pts',(21.0633723464495,-17.8901033611523,
19.7122500356223));
#150403=CARTESIAN_POINT('Ctrl Pts',(21.0980554588832,-17.9661841020042,
19.7164346697446));
#150404=CARTESIAN_POINT('Ctrl Pts',(21.1290718315276,-18.0441074153777,
19.7206193038669));
#150405=CARTESIAN_POINT('Ctrl Pts',(21.1562228177886,-18.1234852922341,
19.7248039379892));
#150406=CARTESIAN_POINT('Ctrl Pts',(21.1833351579802,-18.202750184505,19.7289826158026));
#150407=CARTESIAN_POINT('Ctrl Pts',(21.2065928926806,-18.2834650962591,
19.7331612936161));
#150408=CARTESIAN_POINT('Ctrl Pts',(21.225844598729,-18.3652202322973,19.7373399714295));
#150409=CARTESIAN_POINT('Ctrl Pts',(21.2454413793526,-18.4484407771037,
19.7415935493826));
#150410=CARTESIAN_POINT('Ctrl Pts',(21.2608869019324,-18.5327387665076,
19.7458471273357));
#150411=CARTESIAN_POINT('Ctrl Pts',(21.2720739254929,-18.6176637190892,
19.7501007052888));
#150412=CARTESIAN_POINT('Ctrl Pts',(21.2830440658926,-18.700942229072,19.7542718189987));
#150413=CARTESIAN_POINT('Ctrl Pts',(21.2899192902196,-18.7848231321656,
19.7584429327087));
#150414=CARTESIAN_POINT('Ctrl Pts',(21.2926499549078,-18.8688711346757,
19.7626140464186));
#150415=CARTESIAN_POINT('Ctrl Pts',(21.2953797032961,-18.9528909340954,
19.7667837604725));
#150416=CARTESIAN_POINT('Ctrl Pts',(21.2939676391625,-19.0370772621646,
19.7709534745263));
#150417=CARTESIAN_POINT('Ctrl Pts',(21.2884161370488,-19.1209917121783,
19.7751231885802));
#150418=CARTESIAN_POINT('Ctrl Pts',(21.2828648324788,-19.2049031761927,
19.7792927542596));
#150419=CARTESIAN_POINT('Ctrl Pts',(21.2731744140114,-19.2885423224137,
19.783462319939));
#150420=CARTESIAN_POINT('Ctrl Pts',(21.2593992661682,-19.371474130832,19.7876318856184));
#150421=CARTESIAN_POINT('Ctrl Pts',(21.245139799164,-19.4573217311045,19.7919480486755));
#150422=CARTESIAN_POINT('Ctrl Pts',(21.2265031054957,-19.5424108076164,
19.7962642117326));
#150423=CARTESIAN_POINT('Ctrl Pts',(21.2036071461082,-19.6262703789217,
19.8005803747897));
#150424=CARTESIAN_POINT('Ctrl Pts',(21.181457023188,-19.7073982225301,19.804755938724));
#150425=CARTESIAN_POINT('Ctrl Pts',(21.1553210566128,-19.7873750003199,
19.8089315026582));
#150426=CARTESIAN_POINT('Ctrl Pts',(21.1253562910768,-19.8657916004908,
19.8131070665925));
#150427=CARTESIAN_POINT('Ctrl Pts',(21.0938780701787,-19.9481688531774,
19.817493529211));
#150428=CARTESIAN_POINT('Ctrl Pts',(21.0581743348026,-20.0288236424594,
19.8218799918296));
#150429=CARTESIAN_POINT('Ctrl Pts',(21.0184823804606,-20.1073095919992,
19.8262664544481));
#150430=CARTESIAN_POINT('Ctrl Pts',(20.9787904261185,-20.1857955415389,
19.8306529170666));
#150431=CARTESIAN_POINT('Ctrl Pts',(20.9351106070456,-20.262112185551,19.8350393796852));
#150432=CARTESIAN_POINT('Ctrl Pts',(20.887732090269,-20.3358490103134,19.8394258423037));
#150433=CARTESIAN_POINT('Ctrl Pts',(20.8425432910186,-20.4061779019346,
19.8436095735004));
#150434=CARTESIAN_POINT('Ctrl Pts',(20.7938219698895,-20.474421896084,19.847793304697));
#150435=CARTESIAN_POINT('Ctrl Pts',(20.7417867108824,-20.5402041819628,
19.8519770358936));
#150436=CARTESIAN_POINT('Ctrl Pts',(20.689816339456,-20.6059044378207,19.8561555500086));
#150437=CARTESIAN_POINT('Ctrl Pts',(20.6345405135828,-20.6691487197569,
19.8603340641236));
#150438=CARTESIAN_POINT('Ctrl Pts',(20.5762218026503,-20.7295879246439,
19.8645125782385));
#150439=CARTESIAN_POINT('Ctrl Pts',(20.5179688787956,-20.7899589504061,
19.8686863787337));
#150440=CARTESIAN_POINT('Ctrl Pts',(20.456680209172,-20.8475308583584,19.8728601792288));
#150441=CARTESIAN_POINT('Ctrl Pts',(20.3926584428826,-20.9019877358215,
19.8770339797239));
#150442=CARTESIAN_POINT('Ctrl Pts',(20.3603008450493,-20.9295110898671,
19.8791434835019));
#150443=CARTESIAN_POINT('Ctrl Pts',(20.3272457158191,-20.9562392675845,
19.8812529872798));
#150444=CARTESIAN_POINT('Ctrl Pts',(20.2935357468249,-20.9821350335323,
19.8833624910577));
#150445=CARTESIAN_POINT('Origin',(18.734,-18.952,-1.76670989022851));
#150446=CARTESIAN_POINT('',(20.293535746825,-20.9821350335323,20.7499611453528));
#150447=CARTESIAN_POINT('',(20.2916962225612,-20.9797764771361,20.6832232103036));
#150448=CARTESIAN_POINT('',(20.2935357468249,-20.9821350335323,-1.76670989022851));
#150449=CARTESIAN_POINT('',(16.1740004726297,-18.9535555911146,20.2332901098006));
#150450=CARTESIAN_POINT('Ctrl Pts',(16.1740004726297,-18.9535555911146,
20.2332901098006));
#150451=CARTESIAN_POINT('Ctrl Pts',(16.173950276098,-18.8709483454626,20.2374173417138));
#150452=CARTESIAN_POINT('Ctrl Pts',(16.1779027082632,-18.7881812209217,
20.2415445736269));
#150453=CARTESIAN_POINT('Ctrl Pts',(16.1858778001745,-18.7056805838826,
20.24567180554));
#150454=CARTESIAN_POINT('Ctrl Pts',(16.1940130436929,-18.6215232123815,
20.2498819183568));
#150455=CARTESIAN_POINT('Ctrl Pts',(16.2063343518257,-18.5376436404924,
20.2540920311735));
#150456=CARTESIAN_POINT('Ctrl Pts',(16.2228070334153,-18.4544963471735,
20.2583021439902));
#150457=CARTESIAN_POINT('Ctrl Pts',(16.2389199317137,-18.3731650913156,
20.2624203028504));
#150458=CARTESIAN_POINT('Ctrl Pts',(16.2590046102178,-18.2925349422861,
20.2665384617107));
#150459=CARTESIAN_POINT('Ctrl Pts',(16.2829763019886,-18.2130258246822,
20.270656620571));
#150460=CARTESIAN_POINT('Ctrl Pts',(16.306937024594,-18.1335530895192,20.27477289501));
#150461=CARTESIAN_POINT('Ctrl Pts',(16.3347810947711,-18.0552008202622,
20.2788891694489));
#150462=CARTESIAN_POINT('Ctrl Pts',(16.3663732871523,-17.9783759716349,
20.2830054438879));
#150463=CARTESIAN_POINT('Ctrl Pts',(16.3979610860963,-17.9015618068228,
20.2871211458883));
#150464=CARTESIAN_POINT('Ctrl Pts',(16.4332957915605,-17.8262750781318,
20.2912368478886));
#150465=CARTESIAN_POINT('Ctrl Pts',(16.4721937794553,-17.7529034147721,
20.2953525498889));
#150466=CARTESIAN_POINT('Ctrl Pts',(16.5126461134818,-17.6765998526872,
20.2996327134933));
#150467=CARTESIAN_POINT('Ctrl Pts',(16.5569522564909,-17.6023681227906,
20.3039128770976));
#150468=CARTESIAN_POINT('Ctrl Pts',(16.6048536565105,-17.5306148136394,
20.308193040702));
#150469=CARTESIAN_POINT('Ctrl Pts',(16.6509736167644,-17.4615299901315,
20.3123140262104));
#150470=CARTESIAN_POINT('Ctrl Pts',(16.7004258077716,-17.3947428571309,
20.3164350117188));
#150471=CARTESIAN_POINT('Ctrl Pts',(16.752937145384,-17.3305839626854,20.3205559972272));
#150472=CARTESIAN_POINT('Ctrl Pts',(16.8054841274566,-17.2663815174707,
20.3246797800421));
#150473=CARTESIAN_POINT('Ctrl Pts',(16.8610940674614,-17.2048112072835,
20.3288035628569));
#150474=CARTESIAN_POINT('Ctrl Pts',(16.9194565997149,-17.1461671593191,
20.3329273456718));
#150475=CARTESIAN_POINT('Ctrl Pts',(16.9779086863938,-17.0874331249574,
20.3370574562278));
#150476=CARTESIAN_POINT('Ctrl Pts',(17.0391214358428,-17.0316346193019,
20.3411875667839));
#150477=CARTESIAN_POINT('Ctrl Pts',(17.1027516837168,-16.9790253598631,
20.34531767734));
#150478=CARTESIAN_POINT('Ctrl Pts',(17.1099251001079,-16.9730944050642,
20.3457832892737));
#150479=CARTESIAN_POINT('Ctrl Pts',(17.117129212341,-16.9672039375623,20.3462489012075));
#150480=CARTESIAN_POINT('Ctrl Pts',(17.1243635072392,-16.9613542853705,
20.3467145131413));
#150481=CARTESIAN_POINT('Ctrl Pts',(17.1893810782662,-16.9087810654215,
20.3508991582797));
#150482=CARTESIAN_POINT('Ctrl Pts',(17.2570980357154,-16.8592987213468,
20.3550838034181));
#150483=CARTESIAN_POINT('Ctrl Pts',(17.3271882231892,-16.8131964502025,
20.3592684485566));
#150484=CARTESIAN_POINT('Ctrl Pts',(17.3971786444276,-16.7671598009406,
20.3634471372793));
#150485=CARTESIAN_POINT('Ctrl Pts',(17.4695352047632,-16.7244939187135,
20.367625826002));
#150486=CARTESIAN_POINT('Ctrl Pts',(17.5438988654958,-16.6854477085997,
20.3718045147248));
#150487=CARTESIAN_POINT('Ctrl Pts',(17.6195952011134,-16.6457017494008,
20.3760580899372));
#150488=CARTESIAN_POINT('Ctrl Pts',(17.6973709112956,-16.6097067832357,
20.3803116651496));
#150489=CARTESIAN_POINT('Ctrl Pts',(17.7768165359456,-16.5776790831607,
20.384565240362));
#150490=CARTESIAN_POINT('Ctrl Pts',(17.8547221935641,-16.5462722052193,
20.388736364645));
#150491=CARTESIAN_POINT('Ctrl Pts',(17.9342331580126,-16.5186803432953,
20.392907488928));
#150492=CARTESIAN_POINT('Ctrl Pts',(18.0149402978771,-16.4950602073346,
20.3970786132109));
#150493=CARTESIAN_POINT('Ctrl Pts',(18.0956203529298,-16.4714479981438,
20.4012483376907));
#150494=CARTESIAN_POINT('Ctrl Pts',(18.1774953450108,-16.4518049968894,
20.4054180621704));
#150495=CARTESIAN_POINT('Ctrl Pts',(18.2601401459595,-16.4362383183758,
20.4095877866501));
#150496=CARTESIAN_POINT('Ctrl Pts',(18.3427820029266,-16.42067219438,20.4137573625955));
#150497=CARTESIAN_POINT('Ctrl Pts',(18.4261931620004,-16.4091821887308,
20.4179269385409));
#150498=CARTESIAN_POINT('Ctrl Pts',(18.5099387943011,-16.401824206824,20.4220965144863));
#150499=CARTESIAN_POINT('Ctrl Pts',(18.5966283648553,-16.3942075673155,
20.426412664931));
#150500=CARTESIAN_POINT('Ctrl Pts',(18.6836758372579,-16.3910189213194,
20.4307288153757));
#150501=CARTESIAN_POINT('Ctrl Pts',(18.7705956997935,-16.3922615847012,
20.4350449658204));
#150502=CARTESIAN_POINT('Ctrl Pts',(18.8546845879848,-16.3934637746163,
20.4392205395221));
#150503=CARTESIAN_POINT('Ctrl Pts',(18.9386535841082,-16.3988129731103,
20.4433961132238));
#150504=CARTESIAN_POINT('Ctrl Pts',(19.022067326425,-16.4082592082827,20.4475716869256));
#150505=CARTESIAN_POINT('Ctrl Pts',(19.1096934356114,-16.4181824752605,
20.4519581257418));
#150506=CARTESIAN_POINT('Ctrl Pts',(19.1967061584434,-16.432627374484,20.456344564558));
#150507=CARTESIAN_POINT('Ctrl Pts',(19.28261403032,-16.4514755258674,20.4607310033742));
#150508=CARTESIAN_POINT('Ctrl Pts',(19.3685219021965,-16.4703236772508,
20.4651174421904));
#150509=CARTESIAN_POINT('Ctrl Pts',(19.4533243836861,-16.4935748540295,
20.4695038810066));
#150510=CARTESIAN_POINT('Ctrl Pts',(19.5365517912807,-16.5210514973961,
20.4738903198228));
#150511=CARTESIAN_POINT('Ctrl Pts',(19.6159508694346,-16.547264258518,20.478074989374));
#150512=CARTESIAN_POINT('Ctrl Pts',(19.6942121039237,-16.5774198563297,
20.4822596589251));
#150513=CARTESIAN_POINT('Ctrl Pts',(19.7709157801343,-16.6114005757267,
20.4864443284763));
#150514=CARTESIAN_POINT('Ctrl Pts',(19.847510283723,-16.645332930242,20.4906230419721));
#150515=CARTESIAN_POINT('Ctrl Pts',(19.9225512154519,-16.683079407488,20.4948017554679));
#150516=CARTESIAN_POINT('Ctrl Pts',(19.995634941963,-16.7244728344602,20.4989804689636));
#150517=CARTESIAN_POINT('Ctrl Pts',(20.070027857031,-16.7666077644113,20.5032340380278));
#150518=CARTESIAN_POINT('Ctrl Pts',(20.1423922959442,-16.8125214422593,
20.507487607092));
#150519=CARTESIAN_POINT('Ctrl Pts',(20.212324780906,-16.8619866406745,20.5117411761562));
#150520=CARTESIAN_POINT('Ctrl Pts',(20.280902218561,-16.9104933763104,20.5159123259083));
#150521=CARTESIAN_POINT('Ctrl Pts',(20.3471407144074,-16.9624149500114,
20.5200834756603));
#150522=CARTESIAN_POINT('Ctrl Pts',(20.4106870430868,-17.0174921660679,
20.5242546254124));
#150523=CARTESIAN_POINT('Ctrl Pts',(20.4742120492289,-17.0725509013401,
20.5284243755636));
#150524=CARTESIAN_POINT('Ctrl Pts',(20.5350463349135,-17.1307628750204,
20.5325941257149));
#150525=CARTESIAN_POINT('Ctrl Pts',(20.5928697180021,-17.19182859599,20.5367638758661));
#150526=CARTESIAN_POINT('Ctrl Pts',(20.6506910436328,-17.2528921441335,
20.5409334776502));
#150527=CARTESIAN_POINT('Ctrl Pts',(20.7055013639975,-17.3168089030567,
20.5451030794344));
#150528=CARTESIAN_POINT('Ctrl Pts',(20.7570183053472,-17.3832435063943,
20.5492726812186));
#150529=CARTESIAN_POINT('Ctrl Pts',(20.8103455378025,-17.452012603364,20.553588801659));
#150530=CARTESIAN_POINT('Ctrl Pts',(20.8601432986902,-17.5234793777062,
20.5579049220995));
#150531=CARTESIAN_POINT('Ctrl Pts',(20.906146010203,-17.5972373970474,20.56222104254));
#150532=CARTESIAN_POINT('Ctrl Pts',(20.9506510026991,-17.6685940625427,
20.5663966422274));
#150533=CARTESIAN_POINT('Ctrl Pts',(20.9916040781895,-17.7420946349332,
20.5705722419149));
#150534=CARTESIAN_POINT('Ctrl Pts',(21.0288116000799,-17.8173459910005,
20.5747478416023));
#150535=CARTESIAN_POINT('Ctrl Pts',(21.0678973296718,-17.8963959788854,
20.5791342224193));
#150536=CARTESIAN_POINT('Ctrl Pts',(21.102849178176,-17.9773776221854,20.5835206032363));
#150537=CARTESIAN_POINT('Ctrl Pts',(21.133500670816,-18.0598136233087,20.5879069840533));
#150538=CARTESIAN_POINT('Ctrl Pts',(21.164152163456,-18.1422496244321,20.5922933648703));
#150539=CARTESIAN_POINT('Ctrl Pts',(21.190503198929,-18.2261394071235,20.5966797456872));
#150540=CARTESIAN_POINT('Ctrl Pts',(21.2124488472332,-18.310991956643,20.6010661265042));
#150541=CARTESIAN_POINT('Ctrl Pts',(21.2333845648802,-18.3919396230659,
20.6052506476905));
#150542=CARTESIAN_POINT('Ctrl Pts',(21.2503893834069,-18.4740647142243,
20.6094351688768));
#150543=CARTESIAN_POINT('Ctrl Pts',(21.26333508953,-18.556950629829,20.6136196900631));
#150544=CARTESIAN_POINT('Ctrl Pts',(21.2762623681317,-18.6397185617595,
20.617798254807));
#150545=CARTESIAN_POINT('Ctrl Pts',(21.2851419407115,-18.723244716315,20.6219768195509));
#150546=CARTESIAN_POINT('Ctrl Pts',(21.2898958840996,-18.807099242091,20.6261553842948));
#150547=CARTESIAN_POINT('Ctrl Pts',(21.2947352019821,-18.892459683515,20.6304089904986));
#150548=CARTESIAN_POINT('Ctrl Pts',(21.2952991221815,-18.9781599402376,
20.6346625967024));
#150549=CARTESIAN_POINT('Ctrl Pts',(21.291560298641,-19.0637377233313,20.6389162029062));
#150550=CARTESIAN_POINT('Ctrl Pts',(21.2878940830978,-19.1476535848683,
20.6430872040273));
#150551=CARTESIAN_POINT('Ctrl Pts',(21.2800907694638,-19.2314512062989,
20.6472582051485));
#150552=CARTESIAN_POINT('Ctrl Pts',(21.2681770980697,-19.3146933079325,
20.6514292062696));
#150553=CARTESIAN_POINT('Ctrl Pts',(21.2562674233253,-19.3979074845461,
20.6555988081554));
#150554=CARTESIAN_POINT('Ctrl Pts',(21.2402501944418,-19.4805660564329,
20.6597684100413));
#150555=CARTESIAN_POINT('Ctrl Pts',(21.2202039195678,-19.5622377162434,
20.6639380119271));
#150556=CARTESIAN_POINT('Ctrl Pts',(21.2001583553194,-19.6439064808536,
20.6681074660036));
#150557=CARTESIAN_POINT('Ctrl Pts',(21.176084139551,-19.7245879563522,20.6722769200801));
#150558=CARTESIAN_POINT('Ctrl Pts',(21.1481104108277,-19.8038632075242,
20.6764463741566));
#150559=CARTESIAN_POINT('Ctrl Pts',(21.1191514853751,-19.8859304253638,
20.6807626707424));
#150560=CARTESIAN_POINT('Ctrl Pts',(21.0860134227954,-19.9664900212755,
20.6850789673281));
#150561=CARTESIAN_POINT('Ctrl Pts',(21.0488942544677,-20.045098618896,20.6893952639139));
#150562=CARTESIAN_POINT('Ctrl Pts',(21.0129862928853,-20.1211422004356,
20.6935707187789));
#150563=CARTESIAN_POINT('Ctrl Pts',(20.9733533017232,-20.1953597550482,
20.697746173644));
#150564=CARTESIAN_POINT('Ctrl Pts',(20.930221018763,-20.2673757017459,20.701921628509));
#150565=CARTESIAN_POINT('Ctrl Pts',(20.8849064017289,-20.3430353891307,
20.7063083459551));
#150566=CARTESIAN_POINT('Ctrl Pts',(20.8357293771905,-20.4162643215318,
20.7106950634012));
#150567=CARTESIAN_POINT('Ctrl Pts',(20.7830012667822,-20.4866640703179,
20.7150817808473));
#150568=CARTESIAN_POINT('Ctrl Pts',(20.730273156374,-20.557063819104,20.7194684982935));
#150569=CARTESIAN_POINT('Ctrl Pts',(20.6739943901059,-20.624633986963,20.7238552157396));
#150570=CARTESIAN_POINT('Ctrl Pts',(20.6145211534102,-20.689020492561,20.7282419331857));
#150571=CARTESIAN_POINT('Ctrl Pts',(20.5577980726924,-20.7504296432493,
20.7324258004444));
#150572=CARTESIAN_POINT('Ctrl Pts',(20.4979583003737,-20.8091716397172,
20.7366096677032));
#150573=CARTESIAN_POINT('Ctrl Pts',(20.4352825899291,-20.8649133668842,
20.7407935349619));
#150574=CARTESIAN_POINT('Ctrl Pts',(20.3895046482308,-20.905626771141,20.7438494050922));
#150575=CARTESIAN_POINT('Ctrl Pts',(20.3422147320298,-20.9447401724555,
20.7469052752225));
#150576=CARTESIAN_POINT('Ctrl Pts',(20.293535746825,-20.9821350335323,20.7499611453528));
#150577=CARTESIAN_POINT('Ctrl Pts',(20.2935357468249,-20.9821350335323,
19.9498236325831));
#150578=CARTESIAN_POINT('Ctrl Pts',(20.2269624064254,-21.0332762149925,
19.9540083599342));
#150579=CARTESIAN_POINT('Ctrl Pts',(20.1579647892918,-21.0810672001043,
19.9581930872852));
#150580=CARTESIAN_POINT('Ctrl Pts',(20.0869226462412,-21.1252925052297,
19.9623778146363));
#150581=CARTESIAN_POINT('Ctrl Pts',(20.0710253809767,-21.1351889044203,
19.9633142407899));
#150582=CARTESIAN_POINT('Ctrl Pts',(20.0550258276038,-21.1449069419241,
19.9642506669435));
#150583=CARTESIAN_POINT('Ctrl Pts',(20.0389283877474,-21.1544445288931,
19.965187093097));
#150584=CARTESIAN_POINT('Ctrl Pts',(19.9669932812531,-21.1970654264043,
19.9693717283983));
#150585=CARTESIAN_POINT('Ctrl Pts',(19.89283401806,-21.2362376726233,19.9735563636995));
#150586=CARTESIAN_POINT('Ctrl Pts',(19.8168151370648,-21.2717222633202,
19.9777409990007));
#150587=CARTESIAN_POINT('Ctrl Pts',(19.7409044598142,-21.3071563459651,
19.9819196779762));
#150588=CARTESIAN_POINT('Ctrl Pts',(19.6631398357117,-21.3389130062059,
19.9860983569518));
#150589=CARTESIAN_POINT('Ctrl Pts',(19.5839125153235,-21.3667978624093,
19.9902770359274));
#150590=CARTESIAN_POINT('Ctrl Pts',(19.5032651236308,-21.3951825270617,
19.9945306135879));
#150591=CARTESIAN_POINT('Ctrl Pts',(19.4211024978226,-21.419554974605,19.9987841912483));
#150592=CARTESIAN_POINT('Ctrl Pts',(19.3378610660991,-21.4397604010133,
20.0030377689088));
#150593=CARTESIAN_POINT('Ctrl Pts',(19.2562334111025,-21.4595741108662,
20.007208883732));
#150594=CARTESIAN_POINT('Ctrl Pts',(19.1735688735353,-21.4753808138571,
20.0113799985552));
#150595=CARTESIAN_POINT('Ctrl Pts',(19.0902949413618,-21.4870845971604,
20.0155511133785));
#150596=CARTESIAN_POINT('Ctrl Pts',(19.0070489529336,-21.4987844530938,
20.0197208285252));
#150597=CARTESIAN_POINT('Ctrl Pts',(18.9231944311978,-21.5063840596987,
20.0238905436719));
#150598=CARTESIAN_POINT('Ctrl Pts',(18.8391675225314,-21.509838890979,20.0280602588185));
#150599=CARTESIAN_POINT('Ctrl Pts',(18.7551436043038,-21.513293599305,20.032229825569));
#150600=CARTESIAN_POINT('Ctrl Pts',(18.670947771023,-21.5126038075443,20.0363993923194));
#150601=CARTESIAN_POINT('Ctrl Pts',(18.5870183641846,-21.5077770635822,
20.0405689590698));
#150602=CARTESIAN_POINT('Ctrl Pts',(18.5001381401371,-21.5027806193961,
20.0448851207956));
#150603=CARTESIAN_POINT('Ctrl Pts',(18.4135439525319,-21.4933509339464,
20.0492012825213));
#150604=CARTESIAN_POINT('Ctrl Pts',(18.3277166966688,-21.4795549207553,
20.053517444247));
#150605=CARTESIAN_POINT('Ctrl Pts',(18.2446852202507,-21.4662083057154,
20.0576930091878));
#150606=CARTESIAN_POINT('Ctrl Pts',(18.1623719289166,-21.4487756010914,
20.0618685741286));
#150607=CARTESIAN_POINT('Ctrl Pts',(18.0812003839157,-21.4273691969563,
20.0660441390694));
#150608=CARTESIAN_POINT('Ctrl Pts',(17.9959291092672,-21.4048816199831,
20.0704305991875));
#150609=CARTESIAN_POINT('Ctrl Pts',(17.9119185059158,-21.3780085540391,
20.0748170593057));
#150610=CARTESIAN_POINT('Ctrl Pts',(17.8296377675495,-21.3469381938825,
20.0792035194239));
#150611=CARTESIAN_POINT('Ctrl Pts',(17.7473570291832,-21.315867833726,20.0835899795421));
#150612=CARTESIAN_POINT('Ctrl Pts',(17.6668066567987,-21.2806004817434,
20.0879764396603));
#150613=CARTESIAN_POINT('Ctrl Pts',(17.5884257348681,-21.2413797419973,
20.0923628997785));
#150614=CARTESIAN_POINT('Ctrl Pts',(17.5136510990602,-21.2039635384314,
20.0965475399912));
#150615=CARTESIAN_POINT('Ctrl Pts',(17.4405723466444,-21.1628104733658,
20.100732180204));
#150616=CARTESIAN_POINT('Ctrl Pts',(17.3695877608619,-21.1180976990178,
20.1049168204167));
#150617=CARTESIAN_POINT('Ctrl Pts',(17.2987042121431,-21.0734485673238,
20.1090955043538));
#150618=CARTESIAN_POINT('Ctrl Pts',(17.2299092952355,-21.0252500336355,
20.1132741882909));
#150619=CARTESIAN_POINT('Ctrl Pts',(17.1635782312554,-20.9737258637741,
20.117452872228));
#150620=CARTESIAN_POINT('Ctrl Pts',(17.0960583483627,-20.9212782516533,
20.1217064486544));
#150621=CARTESIAN_POINT('Ctrl Pts',(17.0310919385808,-20.8653848344035,
20.1259600250807));
#150622=CARTESIAN_POINT('Ctrl Pts',(16.9690453966424,-20.8063287864041,
20.130213601507));
#150623=CARTESIAN_POINT('Ctrl Pts',(16.9082016411681,-20.748417553457,20.1343847213775));
#150624=CARTESIAN_POINT('Ctrl Pts',(16.8501659076099,-20.6874655440672,
20.138555841248));
#150625=CARTESIAN_POINT('Ctrl Pts',(16.7952502349276,-20.6237802931102,
20.1427269611185));
#150626=CARTESIAN_POINT('Ctrl Pts',(16.7403529896792,-20.5601164122958,
20.1468966813333));
#150627=CARTESIAN_POINT('Ctrl Pts',(16.6885740261885,-20.4937214595179,
20.151066401548));
#150628=CARTESIAN_POINT('Ctrl Pts',(16.6401868618211,-20.4249380646821,
20.1552361217628));
#150629=CARTESIAN_POINT('Ctrl Pts',(16.5918014193429,-20.3561571175489,
20.1594056935953));
#150630=CARTESIAN_POINT('Ctrl Pts',(16.5468077999962,-20.2849882740964,
20.1635752654278));
#150631=CARTESIAN_POINT('Ctrl Pts',(16.5054369234077,-20.2118041965518,
20.1677448372603));
#150632=CARTESIAN_POINT('Ctrl Pts',(16.4626116274946,-20.136047286488,20.1720609930269));
#150633=CARTESIAN_POINT('Ctrl Pts',(16.4236688015119,-20.0581312666225,
20.1763771487935));
#150634=CARTESIAN_POINT('Ctrl Pts',(16.3888124800457,-19.978496710297,20.1806933045602));
#150635=CARTESIAN_POINT('Ctrl Pts',(16.3550914981633,-19.9014560095544,
20.1848688745654));
#150636=CARTESIAN_POINT('Ctrl Pts',(16.3251950198264,-19.8228074630063,
20.1890444445707));
#150637=CARTESIAN_POINT('Ctrl Pts',(16.2992578088289,-19.7429680540524,
20.193220014576));
#150638=CARTESIAN_POINT('Ctrl Pts',(16.2720106919199,-19.6590965186773,
20.1976064632233));
#150639=CARTESIAN_POINT('Ctrl Pts',(16.2491334314107,-19.5739112339791,
20.2019929118706));
#150640=CARTESIAN_POINT('Ctrl Pts',(16.2307217504163,-19.4879085791077,
20.2063793605179));
#150641=CARTESIAN_POINT('Ctrl Pts',(16.2123100694219,-19.4019059242363,
20.2107658091652));
#150642=CARTESIAN_POINT('Ctrl Pts',(16.1983639848637,-19.3150864841139,
20.2151522578125));
#150643=CARTESIAN_POINT('Ctrl Pts',(16.1889163328206,-19.2279513128369,
20.2195387064599));
#150644=CARTESIAN_POINT('Ctrl Pts',(16.1790436177049,-19.1368958083959,
20.2241225075637));
#150645=CARTESIAN_POINT('Ctrl Pts',(16.1740562221029,-19.0453011470167,
20.2287063086676));
#150646=CARTESIAN_POINT('Ctrl Pts',(16.17400047263,-18.9535555916975,20.2332901097715));
#150647=CARTESIAN_POINT('',(16.1742339566945,-18.9509923323772,20.1667099326003));
#150648=CARTESIAN_POINT('Ctrl Pts',(20.2935357468249,-20.9821350335323,
19.8833624910577));
#150649=CARTESIAN_POINT('Ctrl Pts',(20.2268945255956,-21.0333283605784,
19.8875327680454));
#150650=CARTESIAN_POINT('Ctrl Pts',(20.1576922012557,-21.0812658913437,
19.891703045033));
#150651=CARTESIAN_POINT('Ctrl Pts',(20.0862835351796,-21.1256902356321,
19.8958733220206));
#150652=CARTESIAN_POINT('Ctrl Pts',(20.0148884140487,-21.1701061534178,
19.9000428079814));
#150653=CARTESIAN_POINT('Ctrl Pts',(19.9412881731929,-21.2110099658142,
19.9042122939422));
#150654=CARTESIAN_POINT('Ctrl Pts',(19.865865744466,-21.248188131775,19.9083817799029));
#150655=CARTESIAN_POINT('Ctrl Pts',(19.7904349973461,-21.2853703981421,
19.9125517257192));
#150656=CARTESIAN_POINT('Ctrl Pts',(19.7131820765029,-21.3188259999574,
19.9167216715355));
#150657=CARTESIAN_POINT('Ctrl Pts',(19.6345124063599,-21.3483884088336,
19.9208916173519));
#150658=CARTESIAN_POINT('Ctrl Pts',(19.5557587928649,-21.3779823618574,
19.9250660126495));
#150659=CARTESIAN_POINT('Ctrl Pts',(19.4755858434494,-21.4036746662349,
19.9292404079472));
#150660=CARTESIAN_POINT('Ctrl Pts',(19.3944162755987,-21.4253480027938,
19.9334148032449));
#150661=CARTESIAN_POINT('Ctrl Pts',(19.3132003061911,-21.4470337291756,
19.9375915848857));
#150662=CARTESIAN_POINT('Ctrl Pts',(19.2309870338681,-21.4646958169869,
19.9417683665265));
#150663=CARTESIAN_POINT('Ctrl Pts',(19.1482091842432,-21.478268147226,19.9459451481673));
#150664=CARTESIAN_POINT('Ctrl Pts',(19.0652902818818,-21.4918636045978,
19.9501290470077));
#150665=CARTESIAN_POINT('Ctrl Pts',(18.9818053382874,-21.5013553363726,
19.9543129458482));
#150666=CARTESIAN_POINT('Ctrl Pts',(18.898191710259,-21.5067291602599,19.9584968446886));
#150667=CARTESIAN_POINT('Ctrl Pts',(18.8442012325137,-21.5101991127764,
19.9611984461208));
#150668=CARTESIAN_POINT('Ctrl Pts',(18.7901571303858,-21.5119531845074,
19.963900047553));
#150669=CARTESIAN_POINT('Ctrl Pts',(18.7361763184532,-21.5119990749291,
19.9666016489852));
#150670=CARTESIAN_POINT('Ctrl Pts',(18.6525629441398,-21.5120701567241,
19.9707862842974));
#150671=CARTESIAN_POINT('Ctrl Pts',(18.5687904831801,-21.5080406575016,
19.9749709196097));
#150672=CARTESIAN_POINT('Ctrl Pts',(18.4852943717975,-21.4998904039421,
19.9791555549219));
#150673=CARTESIAN_POINT('Ctrl Pts',(18.401917106683,-21.4917517512489,19.9833342339293));
#150674=CARTESIAN_POINT('Ctrl Pts',(18.3188158637712,-21.479504039016,19.9875129129367));
#150675=CARTESIAN_POINT('Ctrl Pts',(18.2364263585064,-21.4631790998037,
19.9916915919441));
#150676=CARTESIAN_POINT('Ctrl Pts',(18.1525601036474,-21.4465615523608,
19.9959451695992));
#150677=CARTESIAN_POINT('Ctrl Pts',(18.0694318349346,-21.4257191735617,
20.0001987472543));
#150678=CARTESIAN_POINT('Ctrl Pts',(17.9874960097627,-21.4007408585965,
20.0044523249094));
#150679=CARTESIAN_POINT('Ctrl Pts',(17.9071486482337,-21.3762467902365,
20.0086234398147));
#150680=CARTESIAN_POINT('Ctrl Pts',(17.8279483680941,-21.3477758591386,
20.0127945547199));
#150681=CARTESIAN_POINT('Ctrl Pts',(17.7503119553381,-21.3154631012117,
20.0169656696251));
#150682=CARTESIAN_POINT('Ctrl Pts',(17.6727015942355,-21.283161186145,20.0211353848722));
#150683=CARTESIAN_POINT('Ctrl Pts',(17.5966544826745,-21.2470201811682,
20.0253051001192));
#150684=CARTESIAN_POINT('Ctrl Pts',(17.5225687032627,-21.2072237612453,
20.0294748153662));
#150685=CARTESIAN_POINT('Ctrl Pts',(17.4484855601723,-21.1674287574667,
20.0336443822352));
#150686=CARTESIAN_POINT('Ctrl Pts',(17.3763640153247,-21.1239788158135,
20.0378139491041));
#150687=CARTESIAN_POINT('Ctrl Pts',(17.306577534865,-21.0771035518365,20.041983515973));
#150688=CARTESIAN_POINT('Ctrl Pts',(17.2343374822408,-21.0285802345095,
20.0462996776141));
#150689=CARTESIAN_POINT('Ctrl Pts',(17.1646001862987,-20.9763865421866,
20.0506158392553));
#150690=CARTESIAN_POINT('Ctrl Pts',(17.0977455243704,-20.9208248502551,
20.0549320008964));
#150691=CARTESIAN_POINT('Ctrl Pts',(17.0330686154626,-20.8670730491965,
20.059107565999));
#150692=CARTESIAN_POINT('Ctrl Pts',(16.9710897386264,-20.8101696543991,
20.0632831311016));
#150693=CARTESIAN_POINT('Ctrl Pts',(16.9121162723824,-20.7504270024225,
20.0674586962043));
#150694=CARTESIAN_POINT('Ctrl Pts',(16.8501642397595,-20.6876669348877,
20.0718451561147));
#150695=CARTESIAN_POINT('Ctrl Pts',(16.7915295867437,-20.6217736911658,
20.0762316160251));
#150696=CARTESIAN_POINT('Ctrl Pts',(16.7365203854165,-20.5531480847578,
20.0806180759355));
#150697=CARTESIAN_POINT('Ctrl Pts',(16.6815111840894,-20.4845224783498,
20.0850045358459));
#150698=CARTESIAN_POINT('Ctrl Pts',(16.6301277117734,-20.4131650245491,
20.0893909957563));
#150699=CARTESIAN_POINT('Ctrl Pts',(16.5826239199876,-20.339508905323,20.0937774556667));
#150700=CARTESIAN_POINT('Ctrl Pts',(16.5362791661252,-20.2676499107529,
20.0980568909966));
#150701=CARTESIAN_POINT('Ctrl Pts',(16.4934601213991,-20.1933453656254,
20.1023363263266));
#150702=CARTESIAN_POINT('Ctrl Pts',(16.4544271376053,-20.1169667656347,
20.1066157616565));
#150703=CARTESIAN_POINT('Ctrl Pts',(16.4154575008855,-20.0407121213442,
20.1108882518421));
#150704=CARTESIAN_POINT('Ctrl Pts',(16.3802619051423,-19.9623904954392,
20.1151607420277));
#150705=CARTESIAN_POINT('Ctrl Pts',(16.3490570393213,-19.882401566158,20.1194332322133));
#150706=CARTESIAN_POINT('Ctrl Pts',(16.3179055660145,-19.8025495004692,
20.1236984120328));
#150707=CARTESIAN_POINT('Ctrl Pts',(16.2907313869642,-19.7210362103122,
20.1279635918524));
#150708=CARTESIAN_POINT('Ctrl Pts',(16.2677042874668,-19.6382838030585,
20.1322287716719));
#150709=CARTESIAN_POINT('Ctrl Pts',(16.2447004012897,-19.5556148174328,
20.136489651819));
#150710=CARTESIAN_POINT('Ctrl Pts',(16.2258353999309,-19.4717096122622,
20.1407505319661));
#150711=CARTESIAN_POINT('Ctrl Pts',(16.2112300227482,-19.3870076342743,
20.1450114121132));
#150712=CARTESIAN_POINT('Ctrl Pts',(16.1966372356338,-19.3023786707434,
20.1492686193135));
#150713=CARTESIAN_POINT('Ctrl Pts',(16.1862968405519,-19.2169547258213,
20.1535258265139));
#150714=CARTESIAN_POINT('Ctrl Pts',(16.1802787590759,-19.1311865610278,
20.1577830337143));
#150715=CARTESIAN_POINT('Ctrl Pts',(16.1760723590192,-19.0712380185088,
20.1607586525524));
#150716=CARTESIAN_POINT('Ctrl Pts',(16.1739765481552,-19.0111215762638,
20.1637342713904));
#150717=CARTESIAN_POINT('Ctrl Pts',(16.1740001980189,-18.950993095359,20.1667098902285));
#150718=CARTESIAN_POINT('Ctrl Pts',(16.1778405451444,-18.9509805605723,
20.166710586341));
#150719=CARTESIAN_POINT('Ctrl Pts',(16.17655678384,-18.5861666074448,20.1847914783433));
#150720=CARTESIAN_POINT('Ctrl Pts',(16.4202751438729,-17.3676607662538,
20.2452643059062));
#150721=CARTESIAN_POINT('Ctrl Pts',(18.2938122673756,-15.9570836117056,
20.3481290690295));
#150722=CARTESIAN_POINT('Ctrl Pts',(21.0139857521136,-16.9607793310482,
20.4753048757109));
#150723=CARTESIAN_POINT('Ctrl Pts',(21.565931935867,-19.4468145759116,20.5870029228023));
#150724=CARTESIAN_POINT('Ctrl Pts',(20.719740355667,-20.6463213593665,20.6563090343332));
#150725=CARTESIAN_POINT('Ctrl Pts',(20.2916962225613,-20.979776477136,20.6832232103036));
#150726=CARTESIAN_POINT('Origin',(18.734,-18.952,-1.76670989022851));
#150727=CARTESIAN_POINT('',(20.2910035915388,-20.9788220864065,21.5499225011608));
#150728=CARTESIAN_POINT('',(20.2957383325669,-20.9849679853861,21.4832513385096));
#150729=CARTESIAN_POINT('',(20.2935357468249,-20.9821350335323,-1.76670989022851));
#150730=CARTESIAN_POINT('',(16.1741052595683,-18.953341674122,21.0332900820446));
#150731=CARTESIAN_POINT('Ctrl Pts',(16.1775161375017,-18.9533393271451,
21.0332901097715));
#150732=CARTESIAN_POINT('Ctrl Pts',(16.179969922226,-18.4391275102653,21.0587831909243));
#150733=CARTESIAN_POINT('Ctrl Pts',(16.5801691895444,-17.06634175119,21.1266682076376));
#150734=CARTESIAN_POINT('Ctrl Pts',(18.8208064652996,-15.9262793346745,
21.2369451599114));
#150735=CARTESIAN_POINT('Ctrl Pts',(21.325440014071,-17.3869837941583,21.3641209665928));
#150736=CARTESIAN_POINT('Ctrl Pts',(21.4293000734299,-19.7637664899637,
21.4684467470093));
#150737=CARTESIAN_POINT('Ctrl Pts',(20.6042288430632,-20.7393377755163,
21.5303805918653));
#150738=CARTESIAN_POINT('Ctrl Pts',(20.2910035915388,-20.9788220864065,
21.5499225011608));
#150739=CARTESIAN_POINT('Ctrl Pts',(20.293535746825,-20.9821350335323,20.7499611453528));
#150740=CARTESIAN_POINT('Ctrl Pts',(20.223540407456,-21.0359049710261,20.7543551701242));
#150741=CARTESIAN_POINT('Ctrl Pts',(20.1506714756736,-21.0861194930542,
20.7587491948957));
#150742=CARTESIAN_POINT('Ctrl Pts',(20.075331422459,-21.1324655500888,20.7631432196671));
#150743=CARTESIAN_POINT('Ctrl Pts',(20.003802857654,-21.1764669384953,20.7673149486772));
#150744=CARTESIAN_POINT('Ctrl Pts',(19.9300475503307,-21.2169814550763,
20.7714866776873));
#150745=CARTESIAN_POINT('Ctrl Pts',(19.8544414350538,-21.2537843058407,
20.7756584066974));
#150746=CARTESIAN_POINT('Ctrl Pts',(19.7788660533636,-21.2905721963919,
20.7798284399162));
#150747=CARTESIAN_POINT('Ctrl Pts',(19.7014417708356,-21.3236512161474,
20.7839984731349));
#150748=CARTESIAN_POINT('Ctrl Pts',(19.6225688837902,-21.352842630986,20.7881685063537));
#150749=CARTESIAN_POINT('Ctrl Pts',(19.5437044012148,-21.3820309352706,
20.7923380952256));
#150750=CARTESIAN_POINT('Ctrl Pts',(19.4633920523903,-21.4073322986088,
20.7965076840975));
#150751=CARTESIAN_POINT('Ctrl Pts',(19.3820505778548,-21.4286167342853,
20.8006772729694));
#150752=CARTESIAN_POINT('Ctrl Pts',(19.3006933737931,-21.4499052858706,
20.8048476681416));
#150753=CARTESIAN_POINT('Ctrl Pts',(19.2183070941476,-21.4671752522082,
20.8090180633139));
#150754=CARTESIAN_POINT('Ctrl Pts',(19.1353227109471,-21.4803473024247,
20.8131884584861));
#150755=CARTESIAN_POINT('Ctrl Pts',(19.0522458578645,-21.4935340303177,
20.817363500749));
#150756=CARTESIAN_POINT('Ctrl Pts',(18.9685700262187,-21.5026136576386,
20.8215385430118));
#150757=CARTESIAN_POINT('Ctrl Pts',(18.884732829483,-21.5075585718422,20.8257135852747));
#150758=CARTESIAN_POINT('Ctrl Pts',(18.8008414639323,-21.5125066810493,
20.8298913251122));
#150759=CARTESIAN_POINT('Ctrl Pts',(18.7167889853071,-21.5133147558977,
20.8340690649496));
#150760=CARTESIAN_POINT('Ctrl Pts',(18.633012146745,-21.5100073208447,20.8382468047871));
#150761=CARTESIAN_POINT('Ctrl Pts',(18.5490995412421,-21.5066945258336,
20.8424313149797));
#150762=CARTESIAN_POINT('Ctrl Pts',(18.4654639244527,-21.4992529521216,
20.8466158251724));
#150763=CARTESIAN_POINT('Ctrl Pts',(18.3825355774442,-21.4877588133885,
20.8508003353651));
#150764=CARTESIAN_POINT('Ctrl Pts',(18.3520331048177,-21.4835310714315,
20.8523394701991));
#150765=CARTESIAN_POINT('Ctrl Pts',(18.3216262005314,-21.47875555542,20.8538786050331));
#150766=CARTESIAN_POINT('Ctrl Pts',(18.2913357986938,-21.4734377654192,
20.8554177398671));
#150767=CARTESIAN_POINT('Ctrl Pts',(18.208977638002,-21.458978947548,20.8596025742139));
#150768=CARTESIAN_POINT('Ctrl Pts',(18.1271754851468,-21.4404538825132,
20.8637874085606));
#150769=CARTESIAN_POINT('Ctrl Pts',(18.0463616913993,-21.4179184002202,
20.8679722429073));
#150770=CARTESIAN_POINT('Ctrl Pts',(17.9656628842856,-21.3954149827411,
20.8721511228248));
#150771=CARTESIAN_POINT('Ctrl Pts',(17.8859500822175,-21.3689126049628,
20.8763300027422));
#150772=CARTESIAN_POINT('Ctrl Pts',(17.8076468707951,-21.3385183594543,
20.8805088826597));
#150773=CARTESIAN_POINT('Ctrl Pts',(17.7279449213762,-21.3075811785374,
20.8847624103218));
#150774=CARTESIAN_POINT('Ctrl Pts',(17.6497038924681,-21.2726118027868,
20.8890159379838));
#150775=CARTESIAN_POINT('Ctrl Pts',(17.5733558319313,-21.2337767452422,
20.8932694656458));
#150776=CARTESIAN_POINT('Ctrl Pts',(17.4984833648361,-21.1956922602179,
20.8974407845723));
#150777=CARTESIAN_POINT('Ctrl Pts',(17.4254317742295,-21.1538904079626,
20.9016121034987));
#150778=CARTESIAN_POINT('Ctrl Pts',(17.3545880671759,-21.108576620383,20.9057834224251));
#150779=CARTESIAN_POINT('Ctrl Pts',(17.2837681192032,-21.0632780298334,
20.909953342403));
#150780=CARTESIAN_POINT('Ctrl Pts',(17.2151549713756,-21.0144700907621,
20.9141232623808));
#150781=CARTESIAN_POINT('Ctrl Pts',(17.149108758861,-20.9624028834442,20.9182931823587));
#150782=CARTESIAN_POINT('Ctrl Pts',(17.0830648895668,-20.9103375233926,
20.922462954394));
#150783=CARTESIAN_POINT('Ctrl Pts',(17.0195881352142,-20.8550134104489,
20.9266327264293));
#150784=CARTESIAN_POINT('Ctrl Pts',(16.9590064055076,-20.7967215886173,
20.9308024984647));
#150785=CARTESIAN_POINT('Ctrl Pts',(16.8963013133658,-20.7363866645938,
20.9351184191383));
#150786=CARTESIAN_POINT('Ctrl Pts',(16.8366983362714,-20.6728724968329,
20.939434339812));
#150787=CARTESIAN_POINT('Ctrl Pts',(16.7805189580978,-20.6065427824413,
20.9437502604856));
#150788=CARTESIAN_POINT('Ctrl Pts',(16.7261638999386,-20.542367001209,20.9479260297243));
#150789=CARTESIAN_POINT('Ctrl Pts',(16.6750137422496,-20.475556136878,20.952101798963));
#150790=CARTESIAN_POINT('Ctrl Pts',(16.6273169433956,-20.4064712094146,
20.9562775682017));
#150791=CARTESIAN_POINT('Ctrl Pts',(16.5772188714757,-20.3339082335378,
20.9606635645929));
#150792=CARTESIAN_POINT('Ctrl Pts',(16.5309313063379,-20.2588367080555,
20.965049560984));
#150793=CARTESIAN_POINT('Ctrl Pts',(16.488687917131,-20.1817047005368,20.9694355573751));
#150794=CARTESIAN_POINT('Ctrl Pts',(16.4464445279241,-20.1045726930181,
20.9738215537662));
#150795=CARTESIAN_POINT('Ctrl Pts',(16.408245498097,-20.0253807586022,20.9782075501574));
#150796=CARTESIAN_POINT('Ctrl Pts',(16.374265613089,-19.9445994273774,20.9825935465485));
#150797=CARTESIAN_POINT('Ctrl Pts',(16.3382155102257,-19.8588965093302,
20.9872467589128));
#150798=CARTESIAN_POINT('Ctrl Pts',(16.30679887472,-19.7711342279521,20.9918999712772));
#150799=CARTESIAN_POINT('Ctrl Pts',(16.2802296059439,-19.6818019274115,
20.9965531836415));
#150800=CARTESIAN_POINT('Ctrl Pts',(16.2537435506638,-19.5927494107485,
21.0011918223993));
#150801=CARTESIAN_POINT('Ctrl Pts',(16.2320746955043,-19.5021369352023,
21.0058304611572));
#150802=CARTESIAN_POINT('Ctrl Pts',(16.2153886011344,-19.4104720509521,
21.010469099915));
#150803=CARTESIAN_POINT('Ctrl Pts',(16.1987928068799,-19.3193032294376,
21.0150826357574));
#150804=CARTESIAN_POINT('Ctrl Pts',(16.1871261077823,-19.2270936177058,
21.0196961715999));
#150805=CARTESIAN_POINT('Ctrl Pts',(16.1805035115345,-19.1343614087313,
21.0243097074423));
#150806=CARTESIAN_POINT('Ctrl Pts',(16.1762064899349,-19.0741928147187,
21.0273031653588));
#150807=CARTESIAN_POINT('Ctrl Pts',(16.1740320413834,-19.0138045835855,
21.0302966232753));
#150808=CARTESIAN_POINT('Ctrl Pts',(16.1740003516178,-18.9533417463077,
21.0332900811918));
#150809=CARTESIAN_POINT('',(16.1715628046961,-18.9501455684938,20.9667098902285));
#150810=CARTESIAN_POINT('Ctrl Pts',(20.2916962225613,-20.979776477136,20.6832232103036));
#150811=CARTESIAN_POINT('Ctrl Pts',(20.0455373138351,-21.1715392921144,
20.6987009698937));
#150812=CARTESIAN_POINT('Ctrl Pts',(19.0022218507969,-21.7248575169448,
20.7565706650442));
#150813=CARTESIAN_POINT('Ctrl Pts',(16.8944629917136,-21.2791319918735,
20.8510662250192));
#150814=CARTESIAN_POINT('Ctrl Pts',(16.1775450733739,-19.6845343053476,
20.9300840254041));
#150815=CARTESIAN_POINT('Ctrl Pts',(16.1715628046961,-18.9501455684938,
20.9667098902285));
#150816=CARTESIAN_POINT('Ctrl Pts',(16.1715628046961,-18.9501455684938,
20.9667098902285));
#150817=CARTESIAN_POINT('Ctrl Pts',(16.1706210062014,-18.8345295298074,
20.9724759609646));
#150818=CARTESIAN_POINT('Ctrl Pts',(16.2303035994096,-17.8698877850362,
21.0206339672611));
#150819=CARTESIAN_POINT('Ctrl Pts',(17.4553333973082,-16.2082456258976,
21.1111839091181));
#150820=CARTESIAN_POINT('Ctrl Pts',(20.3489604080877,-16.3916498602743,
21.2383597157995));
#150821=CARTESIAN_POINT('Ctrl Pts',(21.7259567090655,-18.8613631150646,
21.3623821922634));
#150822=CARTESIAN_POINT('Ctrl Pts',(20.9160603918706,-20.5025267532674,
21.4440127331667));
#150823=CARTESIAN_POINT('Ctrl Pts',(20.2957383325669,-20.9849679853861,
21.4832513385096));
#150824=CARTESIAN_POINT('Origin',(-18.734,-18.952,-1.76670989022851));
#150825=CARTESIAN_POINT('',(-17.1724222076957,-20.9847558846529,0.749817803349287));
#150826=CARTESIAN_POINT('',(-17.1763092872519,-20.979697823649,0.683386607315289));
#150827=CARTESIAN_POINT('',(-17.1744641402401,-20.9821349467765,-1.76670989022851));
#150828=CARTESIAN_POINT('',(-21.2939992553243,-18.9500473764188,0.233290109771496));
#150829=CARTESIAN_POINT('Ctrl Pts',(-21.2960080607363,-18.9500458442149,
0.233290109771496));
#150830=CARTESIAN_POINT('Ctrl Pts',(-21.2971423972504,-18.8187089636245,
0.239839092339242));
#150831=CARTESIAN_POINT('Ctrl Pts',(-21.2281784586555,-17.8383740905167,
0.288780010467466));
#150832=CARTESIAN_POINT('Ctrl Pts',(-19.9618261937418,-16.1848209595297,
0.380112864156168));
#150833=CARTESIAN_POINT('Ctrl Pts',(-17.072091960026,-16.4220625707093,
0.507288670837601));
#150834=CARTESIAN_POINT('Ctrl Pts',(-15.7493320347114,-18.9005846102407,
0.630523650568644));
#150835=CARTESIAN_POINT('Ctrl Pts',(-16.5648621130939,-20.5111939119585,
0.711366694739205));
#150836=CARTESIAN_POINT('Ctrl Pts',(-17.1724222076957,-20.9847558846529,
0.749817803349287));
#150837=CARTESIAN_POINT('',(-18.0722323438033,-21.4249867709335,1.75387482315159E-11));
#150838=CARTESIAN_POINT('Ctrl Pts',(-18.0722323438033,-21.4249867709335,
1.75386372092134E-11));
#150839=CARTESIAN_POINT('Ctrl Pts',(-18.1529469590682,-21.4465858843588,
0.00418159276979397));
#150840=CARTESIAN_POINT('Ctrl Pts',(-18.2348713083479,-21.4642696834585,
0.00836318552204881));
#150841=CARTESIAN_POINT('Ctrl Pts',(-18.3175904330397,-21.4779063863382,
0.0125447782743042));
#150842=CARTESIAN_POINT('Ctrl Pts',(-18.4001917640921,-21.4915236702882,
0.0167204163572968));
#150843=CARTESIAN_POINT('Ctrl Pts',(-18.4835851718186,-21.5011052307699,
0.0208960544402894));
#150844=CARTESIAN_POINT('Ctrl Pts',(-18.5673419980694,-21.5065694569521,
0.0250716925232821));
#150845=CARTESIAN_POINT('Ctrl Pts',(-18.6514951828609,-21.5120595412382,
0.029267090784533));
#150846=CARTESIAN_POINT('Ctrl Pts',(-18.7360147805748,-21.5133930942776,
0.0334624890457846));
#150847=CARTESIAN_POINT('Ctrl Pts',(-18.8204570723939,-21.5105396566466,
0.0376578873070355));
#150848=CARTESIAN_POINT('Ctrl Pts',(-18.9043499961557,-21.5077047830247,
0.0418259909775979));
#150849=CARTESIAN_POINT('Ctrl Pts',(-18.988166150782,-21.5007372505448,
0.0459940946481601));
#150850=CARTESIAN_POINT('Ctrl Pts',(-19.0714685200797,-21.4896593541993,
0.0501621983187226));
#150851=CARTESIAN_POINT('Ctrl Pts',(-19.154742806599,-21.4785851924188,
0.0543288968439996));
#150852=CARTESIAN_POINT('Ctrl Pts',(-19.2375031954148,-21.4634034794687,
0.058495595369277));
#150853=CARTESIAN_POINT('Ctrl Pts',(-19.3193181247988,-21.4441883341317,
0.062662293894554));
#150854=CARTESIAN_POINT('Ctrl Pts',(-19.4011301114167,-21.424973879936,
0.0668288425496423));
#150855=CARTESIAN_POINT('Ctrl Pts',(-19.4819962578846,-21.4017263881227,
0.0709953912047298));
#150856=CARTESIAN_POINT('Ctrl Pts',(-19.5614968770273,-21.3745707251823,
0.0751619398598182));
#150857=CARTESIAN_POINT('Ctrl Pts',(-19.6419526867075,-21.347088790163,
0.0793785491042754));
#150858=CARTESIAN_POINT('Ctrl Pts',(-19.7210094734801,-21.3156042817862,
0.0835951583487334));
#150859=CARTESIAN_POINT('Ctrl Pts',(-19.7982514704291,-21.280297405335,
0.0878117675931906));
#150860=CARTESIAN_POINT('Ctrl Pts',(-19.8746836538426,-21.2453606900341,
0.0919841694456302));
#150861=CARTESIAN_POINT('Ctrl Pts',(-19.94933853646,-21.2066816487831,0.0961565712980696));
#150862=CARTESIAN_POINT('Ctrl Pts',(-20.0218382563897,-21.1644811016999,
0.100328973150509));
#150863=CARTESIAN_POINT('Ctrl Pts',(-20.0954901988233,-21.1216098703703,
0.104567686090975));
#150864=CARTESIAN_POINT('Ctrl Pts',(-20.1669174627927,-21.0751044941557,
0.108806399031441));
#150865=CARTESIAN_POINT('Ctrl Pts',(-20.2357562486613,-21.0252409820392,
0.113045111971908));
#150866=CARTESIAN_POINT('Ctrl Pts',(-20.3045950345299,-20.9753774699226,
0.117283824912374));
#150867=CARTESIAN_POINT('Ctrl Pts',(-20.3708449996543,-20.922156180229,
0.12152253785284));
#150868=CARTESIAN_POINT('Ctrl Pts',(-20.4341804646243,-20.8658929927532,
0.125761250793306));
#150869=CARTESIAN_POINT('Ctrl Pts',(-20.4958618762422,-20.8110991607781,
0.129889266554068));
#150870=CARTESIAN_POINT('Ctrl Pts',(-20.5550187782048,-20.7532072778741,
0.134017282314829));
#150871=CARTESIAN_POINT('Ctrl Pts',(-20.6113174681947,-20.6924824399031,
0.13814529807559));
#150872=CARTESIAN_POINT('Ctrl Pts',(-20.6675250873048,-20.6318558327154,
0.142266636202701));
#150873=CARTESIAN_POINT('Ctrl Pts',(-20.7208833621661,-20.5684057202645,
0.146387974329813));
#150874=CARTESIAN_POINT('Ctrl Pts',(-20.7710928145057,-20.5024363466744,
0.150509312456924));
#150875=CARTESIAN_POINT('Ctrl Pts',(-20.8212566402015,-20.4365269211813,
0.154626905416172));
#150876=CARTESIAN_POINT('Ctrl Pts',(-20.8682770342032,-20.3681031504801,
0.15874449837542));
#150877=CARTESIAN_POINT('Ctrl Pts',(-20.9118931740675,-20.2975041145794,
0.162862091334668));
#150878=CARTESIAN_POINT('Ctrl Pts',(-20.9554836015079,-20.2269466979588,
0.16697725690589));
#150879=CARTESIAN_POINT('Ctrl Pts',(-20.9956735091388,-20.1542169629418,
0.171092422477113));
#150880=CARTESIAN_POINT('Ctrl Pts',(-21.0322449112854,-20.0796836115467,
0.175207588048335));
#150881=CARTESIAN_POINT('Ctrl Pts',(-21.0688064249755,-20.0051704130512,
0.179321640929506));
#150882=CARTESIAN_POINT('Ctrl Pts',(-21.1017511684254,-19.928854991947,
0.183435693810676));
#150883=CARTESIAN_POINT('Ctrl Pts',(-21.1309074516109,-19.8511299507926,
0.187549746691847));
#150884=CARTESIAN_POINT('Ctrl Pts',(-21.1600799699192,-19.7733616299242,
0.191666090405279));
#150885=CARTESIAN_POINT('Ctrl Pts',(-21.1854596434762,-19.6941825637462,
0.195782434118711));
#150886=CARTESIAN_POINT('Ctrl Pts',(-21.2069235785594,-19.6140037572439,
0.199898777832143));
#150887=CARTESIAN_POINT('Ctrl Pts',(-21.2283934303839,-19.5338028486779,
0.204016256255544));
#150888=CARTESIAN_POINT('Ctrl Pts',(-21.2459452901289,-19.4526021135391,
0.208133734678947));
#150889=CARTESIAN_POINT('Ctrl Pts',(-21.25950720014,-19.3708238078728,0.212251213102348));
#150890=CARTESIAN_POINT('Ctrl Pts',(-21.2730871839159,-19.2889365174201,
0.216374178830764));
#150891=CARTESIAN_POINT('Ctrl Pts',(-21.2826665420701,-19.2064705900185,
0.22049714455918));
#150892=CARTESIAN_POINT('Ctrl Pts',(-21.2882251767647,-19.1238538518089,
0.224620110287596));
#150893=CARTESIAN_POINT('Ctrl Pts',(-21.2921215111921,-19.065943508881,
0.227510110115563));
#150894=CARTESIAN_POINT('Ctrl Pts',(-21.2940434271759,-19.0079591563185,
0.230400109943529));
#150895=CARTESIAN_POINT('Ctrl Pts',(-21.2939992553243,-18.9500473764188,
0.233290109771496));
#150896=CARTESIAN_POINT('',(-19.3957372685685,-21.4249949024184,0.));
#150897=CARTESIAN_POINT('Origin',(-18.734,-18.952,0.));
#150898=CARTESIAN_POINT('',(-21.2914666238416,-18.9551442278135,0.166709890228505));
#150899=CARTESIAN_POINT('Ctrl Pts',(-19.3957372685684,-21.4249949024184,
-8.32667268468867E-16));
#150900=CARTESIAN_POINT('Ctrl Pts',(-20.2191097516036,-21.2046724677036,
0.0423919355604773));
#150901=CARTESIAN_POINT('Ctrl Pts',(-21.1334435320312,-20.3367930039316,
0.0979618989699793));
#150902=CARTESIAN_POINT('Ctrl Pts',(-21.2935045362274,-19.2205935412502,
0.153531862379481));
#150903=CARTESIAN_POINT('Ctrl Pts',(-21.2914666238416,-18.9551442278135,
0.166709890228505));
#150904=CARTESIAN_POINT('Ctrl Pts',(-21.2914666238416,-18.9551442278135,
0.166709890228505));
#150905=CARTESIAN_POINT('Ctrl Pts',(-21.2869488473544,-18.3666789556461,
0.195923797939959));
#150906=CARTESIAN_POINT('Ctrl Pts',(-20.7940986851072,-16.9152596074165,
0.267529641211892));
#150907=CARTESIAN_POINT('Ctrl Pts',(-18.3819425606837,-15.9462796184213,
0.381527420044302));
#150908=CARTESIAN_POINT('Ctrl Pts',(-16.0159518620258,-17.6196571530585,
0.508703226725737));
#150909=CARTESIAN_POINT('Ctrl Pts',(-16.1161224269361,-19.9120072834025,
0.609322955816067));
#150910=CARTESIAN_POINT('Ctrl Pts',(-16.9218454647275,-20.7868241350996,
0.667550749345919));
#150911=CARTESIAN_POINT('Ctrl Pts',(-17.176309287252,-20.9796978236491,
0.683386607315295));
#150912=CARTESIAN_POINT('Origin',(-18.734,-18.952,-1.76670989022851));
#150913=CARTESIAN_POINT('',(-17.1739275047339,-20.9828452456382,1.55000082236256));
#150914=CARTESIAN_POINT('',(-17.1744641402401,-20.9821349467765,1.48324949998987));
#150915=CARTESIAN_POINT('',(-17.1744641402401,-20.9821349467765,-1.76670989022851));
#150916=CARTESIAN_POINT('',(-21.2964370736898,-18.9538544369521,1.0332901097715));
#150917=CARTESIAN_POINT('Ctrl Pts',(-21.2964370736898,-18.9538544369521,
1.0332901097715));
#150918=CARTESIAN_POINT('Ctrl Pts',(-21.2904548055299,-18.219465735772,
1.06991597459592));
#150919=CARTESIAN_POINT('Ctrl Pts',(-20.5735369171316,-16.6248681111266,
1.14893377498083));
#150920=CARTESIAN_POINT('Ctrl Pts',(-17.865447416609,-16.0521913171216,
1.27034351092621));
#150921=CARTESIAN_POINT('Ctrl Pts',(-15.8255862006271,-18.112700872363,
1.39751931760764));
#150922=CARTESIAN_POINT('Ctrl Pts',(-16.2862202722418,-20.1874548438184,
1.49073842141976));
#150923=CARTESIAN_POINT('Ctrl Pts',(-17.0385457522606,-20.8810080370261,
1.54156558967141));
#150924=CARTESIAN_POINT('Ctrl Pts',(-17.173927504734,-20.9828452456383,
1.55000082236257));
#150925=CARTESIAN_POINT('Ctrl Pts',(-17.1724222076957,-20.9847558846529,
0.749817803349287));
#150926=CARTESIAN_POINT('Ctrl Pts',(-17.2346906124658,-21.033290916597,
0.75375863029968));
#150927=CARTESIAN_POINT('Ctrl Pts',(-17.9939164669478,-21.567801595126,
0.800091392810553));
#150928=CARTESIAN_POINT('Ctrl Pts',(-20.0126665309401,-21.6957542121544,
0.888816090881905));
#150929=CARTESIAN_POINT('Ctrl Pts',(-21.2376962809792,-20.0341121664399,
0.979366032738912));
#150930=CARTESIAN_POINT('Ctrl Pts',(-21.2973788721029,-19.0694704700222,
1.02752403903544));
#150931=CARTESIAN_POINT('Ctrl Pts',(-21.2964370736898,-18.9538544369521,
1.0332901097715));
#150932=CARTESIAN_POINT('',(-21.2939288367578,-18.9506582997167,0.966709918232303));
#150933=CARTESIAN_POINT('Ctrl Pts',(-17.176309287252,-20.9796978236491,
0.683386607315295));
#150934=CARTESIAN_POINT('Ctrl Pts',(-17.6030345728764,-21.3031390068366,
0.709942684906398));
#150935=CARTESIAN_POINT('Ctrl Pts',(-18.9689508247891,-21.8140068744739,
0.778890698057982));
#150936=CARTESIAN_POINT('Ctrl Pts',(-20.8878308446456,-20.8376582577765,
0.873331792362382));
#150937=CARTESIAN_POINT('Ctrl Pts',(-21.2880301148004,-19.4648724899129,
0.941216809075682));
#150938=CARTESIAN_POINT('Ctrl Pts',(-21.2904838985449,-18.9506606701336,
0.966709890228504));
#150939=CARTESIAN_POINT('Ctrl Pts',(-21.2939996483808,-18.9506582509922,
0.966709918807928));
#150940=CARTESIAN_POINT('Ctrl Pts',(-21.2939507847444,-18.8574285254183,
0.971325634427595));
#150941=CARTESIAN_POINT('Ctrl Pts',(-21.2888049399727,-18.7643768813754,
0.975941350047264));
#150942=CARTESIAN_POINT('Ctrl Pts',(-21.2786450004472,-18.6720324631339,
0.980557065666932));
#150943=CARTESIAN_POINT('Ctrl Pts',(-21.2684492555577,-18.5793626073736,
0.98518904785764));
#150944=CARTESIAN_POINT('Ctrl Pts',(-21.2532041411694,-18.4874052362913,
0.989821030048348));
#150945=CARTESIAN_POINT('Ctrl Pts',(-21.2330434185021,-18.3966784783199,
0.994453012239056));
#150946=CARTESIAN_POINT('Ctrl Pts',(-21.2127838652416,-18.3055069654919,
0.999107701033865));
#150947=CARTESIAN_POINT('Ctrl Pts',(-21.1875605220101,-18.2155784195034,
1.00376238982867));
#150948=CARTESIAN_POINT('Ctrl Pts',(-21.1575575881288,-18.1273979038206,
1.00841707862348));
#150949=CARTESIAN_POINT('Ctrl Pts',(-21.1382431842027,-18.0706316520587,
1.01141353689948));
#150950=CARTESIAN_POINT('Ctrl Pts',(-21.1169490236919,-18.0145893782908,
1.01440999517548));
#150951=CARTESIAN_POINT('Ctrl Pts',(-21.0937343882856,-17.9594005758905,
1.01740645345148));
#150952=CARTESIAN_POINT('Ctrl Pts',(-21.0613129620801,-17.8823242120765,
1.02159128983477));
#150953=CARTESIAN_POINT('Ctrl Pts',(-21.0250509387666,-17.8066946664276,
1.02577612621805));
#150954=CARTESIAN_POINT('Ctrl Pts',(-20.9850989461096,-17.7329210301116,
1.02996096260134));
#150955=CARTESIAN_POINT('Ctrl Pts',(-20.9452038038475,-17.6592523712966,
1.03413984409765));
#150956=CARTESIAN_POINT('Ctrl Pts',(-20.9016293390032,-17.5874347771646,
1.03831872559397));
#150957=CARTESIAN_POINT('Ctrl Pts',(-20.8545742066751,-17.5178573871528,
1.04249760709029));
#150958=CARTESIAN_POINT('Ctrl Pts',(-20.8066785470568,-17.447037163635,
1.0467511343004));
#150959=CARTESIAN_POINT('Ctrl Pts',(-20.7551768351364,-17.3785384082051,
1.05100466151051));
#150960=CARTESIAN_POINT('Ctrl Pts',(-20.7003275395571,-17.3127452891087,
1.05525818872062));
#150961=CARTESIAN_POINT('Ctrl Pts',(-20.6465383152431,-17.2482237523413,
1.05942950809333));
#150962=CARTESIAN_POINT('Ctrl Pts',(-20.5895300617653,-17.1863045680918,
1.06360082746604));
#150963=CARTESIAN_POINT('Ctrl Pts',(-20.5295891698327,-17.1273193339164,
1.06777214683875));
#150964=CARTESIAN_POINT('Ctrl Pts',(-20.4696683865407,-17.0683538877827,
1.0719420668402));
#150965=CARTESIAN_POINT('Ctrl Pts',(-20.4068172462801,-17.0123207593134,
1.07611198684165));
#150966=CARTESIAN_POINT('Ctrl Pts',(-20.3413596900249,-16.9595154136398,
1.08028190684309));
#150967=CARTESIAN_POINT('Ctrl Pts',(-20.2759044627329,-16.9067119467669,
1.08445167847984));
#150968=CARTESIAN_POINT('Ctrl Pts',(-20.2078433623746,-16.8571363224976,
1.08862145011658));
#150969=CARTESIAN_POINT('Ctrl Pts',(-20.1375330967626,-16.8110434739837,
1.09279122175333));
#150970=CARTESIAN_POINT('Ctrl Pts',(-20.0647584945778,-16.763335096196,
1.0971071416183));
#150971=CARTESIAN_POINT('Ctrl Pts',(-19.9895745735351,-16.7193584596411,
1.10142306148326));
#150972=CARTESIAN_POINT('Ctrl Pts',(-19.912407443714,-16.6793460675678,
1.10573898134822));
#150973=CARTESIAN_POINT('Ctrl Pts',(-19.8377461836545,-16.640633009079,
1.10991474914186));
#150974=CARTESIAN_POINT('Ctrl Pts',(-19.7612289942279,-16.6056308240552,
1.11409051693549));
#150975=CARTESIAN_POINT('Ctrl Pts',(-19.6832631274217,-16.5745014164215,
1.11826628472913));
#150976=CARTESIAN_POINT('Ctrl Pts',(-19.6013720862765,-16.5418048056382,
1.12265228062976));
#150977=CARTESIAN_POINT('Ctrl Pts',(-19.5178832247939,-16.513381343314,
1.12703827653039));
#150978=CARTESIAN_POINT('Ctrl Pts',(-19.4332853705763,-16.4893591470744,
1.13142427243102));
#150979=CARTESIAN_POINT('Ctrl Pts',(-19.3486875163586,-16.4653369508349,
1.13581026833165));
#150980=CARTESIAN_POINT('Ctrl Pts',(-19.262981251447,-16.4457160760172,
1.14019626423228));
#150981=CARTESIAN_POINT('Ctrl Pts',(-19.1766642016327,-16.4305622346382,
1.14458226013291));
#150982=CARTESIAN_POINT('Ctrl Pts',(-19.094308163638,-16.4161037894172,
1.14876698662453));
#150983=CARTESIAN_POINT('Ctrl Pts',(-19.0110898349947,-16.4056576058547,
1.15295171311615));
#150984=CARTESIAN_POINT('Ctrl Pts',(-18.9274347085164,-16.3993184660947,
1.15713643960778));
#150985=CARTESIAN_POINT('Ctrl Pts',(-18.8438986079916,-16.3929883457718,
1.16131521199853));
#150986=CARTESIAN_POINT('Ctrl Pts',(-18.7599273988698,-16.3907536965201,
1.16549398438929));
#150987=CARTESIAN_POINT('Ctrl Pts',(-18.6759557948522,-16.3926581177481,
1.16967275678004));
#150988=CARTESIAN_POINT('Ctrl Pts',(-18.5904814574488,-16.3945966199894,
1.1739263113648));
#150989=CARTESIAN_POINT('Ctrl Pts',(-18.5050071857135,-16.4008238803847,
1.17817986594957));
#150990=CARTESIAN_POINT('Ctrl Pts',(-18.4199959336435,-16.4113305121855,
1.18243342053433));
#150991=CARTESIAN_POINT('Ctrl Pts',(-18.3366303540414,-16.4216337535614,
1.18660463357606));
#150992=CARTESIAN_POINT('Ctrl Pts',(-18.253710504808,-16.4360521008819,
1.19077584661778));
#150993=CARTESIAN_POINT('Ctrl Pts',(-18.1716702063162,-16.4545242337241,
1.19494705965951));
#150994=CARTESIAN_POINT('Ctrl Pts',(-18.0896574058363,-16.4729901751342,
1.19911687460703));
#150995=CARTESIAN_POINT('Ctrl Pts',(-18.0085240190108,-16.4955071026302,
1.20328668955455));
#150996=CARTESIAN_POINT('Ctrl Pts',(-17.928693809361,-16.5219625642146,
1.20745650450207));
#150997=CARTESIAN_POINT('Ctrl Pts',(-17.8488664128646,-16.5484170935294,
1.2116261725086));
#150998=CARTESIAN_POINT('Ctrl Pts',(-17.7703425386245,-16.5788097354628,
1.21579584051513));
#150999=CARTESIAN_POINT('Ctrl Pts',(-17.6935296044675,-16.6129785473364,
1.21996550852166));
#151000=CARTESIAN_POINT('Ctrl Pts',(-17.6140201094723,-16.6483468743828,
1.22428155504605));
#151001=CARTESIAN_POINT('Ctrl Pts',(-17.5363443994794,-16.6877612214625,
1.22859760157044));
#151002=CARTESIAN_POINT('Ctrl Pts',(-17.4609286630762,-16.7309891105393,
1.23291364809483));
#151003=CARTESIAN_POINT('Ctrl Pts',(-17.3879657937454,-16.7728110295788,
1.23708931690885));
#151004=CARTESIAN_POINT('Ctrl Pts',(-17.3171185130706,-16.8182019314128,
1.24126498572286));
#151005=CARTESIAN_POINT('Ctrl Pts',(-17.2487433707402,-16.8669070176034,
1.24544065453688));
#151006=CARTESIAN_POINT('Ctrl Pts',(-17.1769202732361,-16.9180681565082,
1.24982688991646));
#151007=CARTESIAN_POINT('Ctrl Pts',(-17.107825650743,-16.972886152708,1.25421312529603));
#151008=CARTESIAN_POINT('Ctrl Pts',(-17.0418318787045,-17.0310192480737,
1.25859936067561));
#151009=CARTESIAN_POINT('Ctrl Pts',(-16.9758381066661,-17.0891523434394,
1.26298559605519));
#151010=CARTESIAN_POINT('Ctrl Pts',(-16.9129455467798,-17.150600078281,
1.26737183143476));
#151011=CARTESIAN_POINT('Ctrl Pts',(-16.8534788456906,-17.2149795084125,
1.27175806681434));
#151012=CARTESIAN_POINT('Ctrl Pts',(-16.7967468035303,-17.2763983609397,
1.2759425950616));
#151013=CARTESIAN_POINT('Ctrl Pts',(-16.7429212561054,-17.3407138418484,
1.28012712330885));
#151014=CARTESIAN_POINT('Ctrl Pts',(-16.6923122163234,-17.4076195436403,
1.28431165155611));
#151015=CARTESIAN_POINT('Ctrl Pts',(-16.6417752336978,-17.4744299850868,
1.2884902218716));
#151016=CARTESIAN_POINT('Ctrl Pts',(-16.5944459372434,-17.5438229582135,
1.29266879218708));
#151017=CARTESIAN_POINT('Ctrl Pts',(-16.550596298851,-17.615456593369,1.29684736250257));
#151018=CARTESIAN_POINT('Ctrl Pts',(-16.5059592554184,-17.6883765489466,
1.30110096712729));
#151019=CARTESIAN_POINT('Ctrl Pts',(-16.4649284015663,-17.7636180793202,
1.30535457175201));
#151020=CARTESIAN_POINT('Ctrl Pts',(-16.4277464893493,-17.840786814058,
1.30960817637672));
#151021=CARTESIAN_POINT('Ctrl Pts',(-16.3912866203068,-17.9164569933187,
1.31377917938137));
#151022=CARTESIAN_POINT('Ctrl Pts',(-16.3585277513987,-17.9939797629346,
1.31795018238601));
#151023=CARTESIAN_POINT('Ctrl Pts',(-16.3296531528721,-18.072957203143,
1.32212118539066));
#151024=CARTESIAN_POINT('Ctrl Pts',(-16.3007882503651,-18.1519081229201,
1.32629078778269));
#151025=CARTESIAN_POINT('Ctrl Pts',(-16.2758051856693,-18.2323123114455,
1.33046039017472));
#151026=CARTESIAN_POINT('Ctrl Pts',(-16.2548387934267,-18.3137526249001,
1.33462999256676));
#151027=CARTESIAN_POINT('Ctrl Pts',(-16.2338731513477,-18.3951900244743,
1.33879944577318));
#151028=CARTESIAN_POINT('Ctrl Pts',(-16.2169240098584,-18.477663029525,
1.3429688989796));
#151029=CARTESIAN_POINT('Ctrl Pts',(-16.2040757430117,-18.5607414487807,
1.34713835218602));
#151030=CARTESIAN_POINT('Ctrl Pts',(-16.1907749845688,-18.6467457324343,
1.3514546456285));
#151031=CARTESIAN_POINT('Ctrl Pts',(-16.181869424783,-18.7333983482173,
1.35577093907098));
#151032=CARTESIAN_POINT('Ctrl Pts',(-16.1773942991259,-18.8202149846984,
1.36008723251346));
#151033=CARTESIAN_POINT('Ctrl Pts',(-16.1730651991088,-18.90419874991,1.36426268309241));
#151034=CARTESIAN_POINT('Ctrl Pts',(-16.1728817996142,-18.9883355251162,
1.36843813367136));
#151035=CARTESIAN_POINT('Ctrl Pts',(-16.1768228581885,-19.0721876258056,
1.37261358425031));
#151036=CARTESIAN_POINT('Ctrl Pts',(-16.1809633215807,-19.1602823716003,
1.37700029912456));
#151037=CARTESIAN_POINT('Ctrl Pts',(-16.1896565615449,-19.2480622945844,
1.3813870139988));
#151038=CARTESIAN_POINT('Ctrl Pts',(-16.2028167371298,-19.3350290978058,
1.38577372887305));
#151039=CARTESIAN_POINT('Ctrl Pts',(-16.2159769127148,-19.4219959010273,
1.39016044374729));
#151040=CARTESIAN_POINT('Ctrl Pts',(-16.2336038329925,-19.5081490310293,
1.39454715862153));
#151041=CARTESIAN_POINT('Ctrl Pts',(-16.2555511525982,-19.593008042705,
1.39893387349578));
#151042=CARTESIAN_POINT('Ctrl Pts',(-16.2764836526239,-19.6739432683273,
1.4031177515669));
#151043=CARTESIAN_POINT('Ctrl Pts',(-16.3014237438776,-19.7540026391425,
1.40730162963803));
#151044=CARTESIAN_POINT('Ctrl Pts',(-16.3302816128663,-19.8327598511259,
1.41148550770915));
#151045=CARTESIAN_POINT('Ctrl Pts',(-16.3591010961105,-19.9114123029754,
1.4156638205296));
#151046=CARTESIAN_POINT('Ctrl Pts',(-16.391827853758,-19.9887656069921,
1.41984213335005));
#151047=CARTESIAN_POINT('Ctrl Pts',(-16.42832166062,-20.0644061287649,1.42402044617049));
#151048=CARTESIAN_POINT('Ctrl Pts',(-16.4647778765757,-20.1399687360639,
1.4281944550671));
#151049=CARTESIAN_POINT('Ctrl Pts',(-16.5049932362158,-20.2138216531577,
1.43236846396371));
#151050=CARTESIAN_POINT('Ctrl Pts',(-16.5487790194524,-20.2855701204566,
1.43654247286032));
#151051=CARTESIAN_POINT('Ctrl Pts',(-16.5925359561236,-20.3572713190599,
1.44071373187301));
#151052=CARTESIAN_POINT('Ctrl Pts',(-16.6398584066156,-20.4268704292796,
1.44488499088571));
#151053=CARTESIAN_POINT('Ctrl Pts',(-16.6905118002526,-20.4939973986662,
1.4490562498984));
#151054=CARTESIAN_POINT('Ctrl Pts',(-16.7411445970495,-20.5610970726761,
1.45322581278081));
#151055=CARTESIAN_POINT('Ctrl Pts',(-16.7951053669189,-20.6257262378605,
1.45739537566322));
#151056=CARTESIAN_POINT('Ctrl Pts',(-16.8521171387588,-20.6875451295102,
1.46156493854563));
#151057=CARTESIAN_POINT('Ctrl Pts',(-16.9091416027605,-20.7493777834998,
1.46573542967084));
#151058=CARTESIAN_POINT('Ctrl Pts',(-16.9692181178399,-20.808398571774,
1.46990592079606));
#151059=CARTESIAN_POINT('Ctrl Pts',(-17.0320310972619,-20.8643027621463,
1.47407641192128));
#151060=CARTESIAN_POINT('Ctrl Pts',(-17.0780839460982,-20.9052902658792,
1.47713410794414));
#151061=CARTESIAN_POINT('Ctrl Pts',(-17.1256069408164,-20.9446031784427,
1.480191803967));
#151062=CARTESIAN_POINT('Ctrl Pts',(-17.1744641402401,-20.9821349467765,
1.48324949998987));
#151063=CARTESIAN_POINT('Origin',(-18.734,-18.952,-1.76670989022851));
#151064=CARTESIAN_POINT('',(-17.1744641402401,-20.9821349467765,2.34989188578132));
#151065=CARTESIAN_POINT('',(-17.1744641402401,-20.9821349467765,2.28327544915889));
#151066=CARTESIAN_POINT('',(-17.1744641402401,-20.9821349467765,-1.76670989022851));
#151067=CARTESIAN_POINT('',(-21.2937660511389,-18.9530076677181,1.83329006740113));
#151068=CARTESIAN_POINT('Ctrl Pts',(-21.293999801981,-18.9530069047618,
1.83329010977149));
#151069=CARTESIAN_POINT('Ctrl Pts',(-21.2940336318731,-18.8669962707737,
1.83754657623943));
#151070=CARTESIAN_POINT('Ctrl Pts',(-21.2897284501564,-18.7810104793984,
1.84180304270736));
#151071=CARTESIAN_POINT('Ctrl Pts',(-21.2811180404876,-18.6955049945465,
1.8460595091753));
#151072=CARTESIAN_POINT('Ctrl Pts',(-21.272502628509,-18.6099498343665,
1.85031844848306));
#151073=CARTESIAN_POINT('Ctrl Pts',(-21.2595770560965,-18.5248759662227,
1.85457738779083));
#151074=CARTESIAN_POINT('Ctrl Pts',(-21.2424267247842,-18.4407316102198,
1.8588363270986));
#151075=CARTESIAN_POINT('Ctrl Pts',(-21.2252479656664,-18.3564477793963,
1.8631023258792));
#151076=CARTESIAN_POINT('Ctrl Pts',(-21.2038305496871,-18.273096962458,
1.8673683246598));
#151077=CARTESIAN_POINT('Ctrl Pts',(-21.1783105998859,-18.191115191842,
1.87163432344041));
#151078=CARTESIAN_POINT('Ctrl Pts',(-21.1527682035212,-18.1090613125802,
1.87590407446243));
#151079=CARTESIAN_POINT('Ctrl Pts',(-21.1231162337396,-18.0283792845701,
1.88017382548446));
#151080=CARTESIAN_POINT('Ctrl Pts',(-21.0895392521437,-17.949485744934,
1.88444357650648));
#151081=CARTESIAN_POINT('Ctrl Pts',(-21.0558918636089,-17.8704267749242,
1.88872228068881));
#151082=CARTESIAN_POINT('Ctrl Pts',(-21.0183032087881,-17.7931641756621,
1.89300098487114));
#151083=CARTESIAN_POINT('Ctrl Pts',(-20.9770042486984,-17.7180907892714,
1.89727968905346));
#151084=CARTESIAN_POINT('Ctrl Pts',(-20.9482314701846,-17.6657875372232,
1.90026064081344));
#151085=CARTESIAN_POINT('Ctrl Pts',(-20.917658721245,-17.614546342522,1.90324159257341));
#151086=CARTESIAN_POINT('Ctrl Pts',(-20.8853760799725,-17.5644910946152,
1.90622254433338));
#151087=CARTESIAN_POINT('Ctrl Pts',(-20.8400579766697,-17.4942239539453,
1.91040717961954));
#151088=CARTESIAN_POINT('Ctrl Pts',(-20.7912093745918,-17.4260486192458,
1.9145918149057));
#151089=CARTESIAN_POINT('Ctrl Pts',(-20.7390496453448,-17.3603417704474,
1.91877645019186));
#151090=CARTESIAN_POINT('Ctrl Pts',(-20.6869641588708,-17.294728447032,
1.92295512917932));
#151091=CARTESIAN_POINT('Ctrl Pts',(-20.6315771902452,-17.2315769876738,
1.92713380816678));
#151092=CARTESIAN_POINT('Ctrl Pts',(-20.5731519433967,-17.1712360827161,
1.93131248715424));
#151093=CARTESIAN_POINT('Ctrl Pts',(-20.5136794819871,-17.1098136269271,
1.9355660648151));
#151094=CARTESIAN_POINT('Ctrl Pts',(-20.4510590117389,-17.05130387858,1.93981964247596));
#151095=CARTESIAN_POINT('Ctrl Pts',(-20.3856118360818,-16.9960403013062,
1.94407322013681));
#151096=CARTESIAN_POINT('Ctrl Pts',(-20.321433464053,-16.9418481014699,
1.94824433503721));
#151097=CARTESIAN_POINT('Ctrl Pts',(-20.2545373771256,-16.8907776413735,
1.9524154499376));
#151098=CARTESIAN_POINT('Ctrl Pts',(-20.1852631886002,-16.8431057026456,
1.956586564838));
#151099=CARTESIAN_POINT('Ctrl Pts',(-20.1160122456088,-16.7954497606359,
1.96075628008586));
#151100=CARTESIAN_POINT('Ctrl Pts',(-20.0443851644975,-16.751190335713,
1.96492599533372));
#151101=CARTESIAN_POINT('Ctrl Pts',(-19.9707522609747,-16.7105621032529,
1.96909571058158));
#151102=CARTESIAN_POINT('Ctrl Pts',(-19.8971219775584,-16.6699353164821,
1.97326527745694));
#151103=CARTESIAN_POINT('Ctrl Pts',(-19.8214864168391,-16.6329396867698,
1.9774348443323));
#151104=CARTESIAN_POINT('Ctrl Pts',(-19.7442411213497,-16.5997642812137,
1.98160441120766));
#151105=CARTESIAN_POINT('Ctrl Pts',(-19.6642800145858,-16.5654224856545,
1.98592057285826));
#151106=CARTESIAN_POINT('Ctrl Pts',(-19.5825943566344,-16.5351747549185,
1.99023673450886));
#151107=CARTESIAN_POINT('Ctrl Pts',(-19.4996442818955,-16.5091760534986,
1.99455289615945));
#151108=CARTESIAN_POINT('Ctrl Pts',(-19.4193962589829,-16.4840242450908,
1.99872846128247));
#151109=CARTESIAN_POINT('Ctrl Pts',(-19.3379653976299,-16.4628489695091,
2.0029040264055));
#151110=CARTESIAN_POINT('Ctrl Pts',(-19.2557808529989,-16.4457388920059,
2.00707959152852));
#151111=CARTESIAN_POINT('Ctrl Pts',(-19.1694454229471,-16.4277646377701,
2.0114660514429));
#151112=CARTESIAN_POINT('Ctrl Pts',(-19.0822787497951,-16.414277123413,
2.01585251135729));
#151113=CARTESIAN_POINT('Ctrl Pts',(-18.9947846786655,-16.4053175794039,
2.02023897127167));
#151114=CARTESIAN_POINT('Ctrl Pts',(-18.9072906075359,-16.3963580353947,
2.02462543118605));
#151115=CARTESIAN_POINT('Ctrl Pts',(-18.8194697217397,-16.3919264150073,
2.02901189110044));
#151116=CARTESIAN_POINT('Ctrl Pts',(-18.7318236815548,-16.3920009250709,
2.03339835101482));
#151117=CARTESIAN_POINT('Ctrl Pts',(-18.6482103252817,-16.3920720068503,
2.03758298542414));
#151118=CARTESIAN_POINT('Ctrl Pts',(-18.5644448542372,-16.3962439324394,
2.04176761983347));
#151119=CARTESIAN_POINT('Ctrl Pts',(-18.4809627381507,-16.4045361348754,
2.04595225424279));
#151120=CARTESIAN_POINT('Ctrl Pts',(-18.3975994484666,-16.4128165343932,
2.05013093234583));
#151121=CARTESIAN_POINT('Ctrl Pts',(-18.3145191664838,-16.4252055165336,
2.05430961044886));
#151122=CARTESIAN_POINT('Ctrl Pts',(-18.2321575527427,-16.4416705080546,
2.0584882885519));
#151123=CARTESIAN_POINT('Ctrl Pts',(-18.1483196667378,-16.4584306226215,
2.06274186643291));
#151124=CARTESIAN_POINT('Ctrl Pts',(-18.0652269487778,-16.4794143083259,
2.06699544431393));
#151125=CARTESIAN_POINT('Ctrl Pts',(-17.983333704675,-16.5045318974371,
2.07124902219494));
#151126=CARTESIAN_POINT('Ctrl Pts',(-17.9030281203276,-16.5291625332492,
2.07542013619884));
#151127=CARTESIAN_POINT('Ctrl Pts',(-17.823876376669,-16.5577680742283,
2.07959125020274));
#151128=CARTESIAN_POINT('Ctrl Pts',(-17.7462950293603,-16.5902127761008,
2.08376236420664));
#151129=CARTESIAN_POINT('Ctrl Pts',(-17.6687397151752,-16.6226465908598,
2.08793207855547));
#151130=CARTESIAN_POINT('Ctrl Pts',(-17.5927541748485,-16.6589168306539,
2.0921017929043));
#151131=CARTESIAN_POINT('Ctrl Pts',(-17.5187361779858,-16.6988391440238,
2.09627150725313));
#151132=CARTESIAN_POINT('Ctrl Pts',(-17.444720814957,-16.7387600368103,
2.10044107322811));
#151133=CARTESIAN_POINT('Ctrl Pts',(-17.3726732606788,-16.7823325256568,
2.1046106392031));
#151134=CARTESIAN_POINT('Ctrl Pts',(-17.3029665902195,-16.8293263604378,
2.10878020517808));
#151135=CARTESIAN_POINT('Ctrl Pts',(-17.230809120241,-16.877972439788,2.11309636788793));
#151136=CARTESIAN_POINT('Ctrl Pts',(-17.161160645027,-16.9302846355734,
2.11741253059778));
#151137=CARTESIAN_POINT('Ctrl Pts',(-17.0944005276118,-16.9859599266179,
2.12172869330762));
#151138=CARTESIAN_POINT('Ctrl Pts',(-17.0298151129941,-17.039821601751,
2.12590425753617));
#151139=CARTESIAN_POINT('Ctrl Pts',(-16.9679330839857,-17.0968302774655,
2.13007982176472));
#151140=CARTESIAN_POINT('Ctrl Pts',(-16.9090612874562,-17.1566730950997,
2.13425538599327));
#151141=CARTESIAN_POINT('Ctrl Pts',(-16.8472160178593,-17.2195384297455,
2.13864184794376));
#151142=CARTESIAN_POINT('Ctrl Pts',(-16.7886934534027,-17.2855312985657,
2.14302830989426));
#151143=CARTESIAN_POINT('Ctrl Pts',(-16.7338009846514,-17.3542503641063,
2.14741477184476));
#151144=CARTESIAN_POINT('Ctrl Pts',(-16.6789085159001,-17.4229694296469,
2.15180123379525));
#151145=CARTESIAN_POINT('Ctrl Pts',(-16.6276464193007,-17.4944141761415,
2.15618769574575));
#151146=CARTESIAN_POINT('Ctrl Pts',(-16.5802679097402,-17.5681509896722,
2.16057415769625));
#151147=CARTESIAN_POINT('Ctrl Pts',(-16.5350693576943,-17.6384950599053,
2.16475879183957));
#151148=CARTESIAN_POINT('Ctrl Pts',(-16.4932366288049,-17.7111867434462,
2.1689434259829));
#151149=CARTESIAN_POINT('Ctrl Pts',(-16.4550217747165,-17.7858703979901,
2.17312806012623));
#151150=CARTESIAN_POINT('Ctrl Pts',(-16.4168613147861,-17.8604477495111,
2.17730673795607));
#151151=CARTESIAN_POINT('Ctrl Pts',(-16.3823087086902,-17.9370110341542,
2.18148541578591));
#151152=CARTESIAN_POINT('Ctrl Pts',(-16.3515723823109,-18.0151762991511,
2.18566409361575));
#151153=CARTESIAN_POINT('Ctrl Pts',(-16.3202851270053,-18.0947426263631,
2.18991767156417));
#151154=CARTESIAN_POINT('Ctrl Pts',(-16.2929525719636,-18.1759685244401,
2.19417124951258));
#151155=CARTESIAN_POINT('Ctrl Pts',(-16.2697452280172,-18.2584234586145,
2.19842482746099));
#151156=CARTESIAN_POINT('Ctrl Pts',(-16.2469878054908,-18.3392798366961,
2.2025959411759));
#151157=CARTESIAN_POINT('Ctrl Pts',(-16.2281972006543,-18.4213175582044,
2.2067670548908));
#151158=CARTESIAN_POINT('Ctrl Pts',(-16.2134847477736,-18.5041128900115,
2.2109381686057));
#151159=CARTESIAN_POINT('Ctrl Pts',(-16.1987772318085,-18.5868804389886,
2.21510788266025));
#151160=CARTESIAN_POINT('Ctrl Pts',(-16.1881452304224,-18.670404640811,
2.2192775967148));
#151161=CARTESIAN_POINT('Ctrl Pts',(-16.1816490383963,-18.7542512482959,
2.22344731076935));
#151162=CARTESIAN_POINT('Ctrl Pts',(-16.1751530775363,-18.8380948721097,
2.22761687644514));
#151163=CARTESIAN_POINT('Ctrl Pts',(-16.1727926681059,-18.9222604200508,
2.23178644212092));
#151164=CARTESIAN_POINT('Ctrl Pts',(-16.1745761446872,-19.0063095650504,
2.23595600779671));
#151165=CARTESIAN_POINT('Ctrl Pts',(-16.1764223263562,-19.0933137861385,
2.24027217084513));
#151166=CARTESIAN_POINT('Ctrl Pts',(-16.1827092038591,-19.1801927391925,
2.24458833389354));
#151167=CARTESIAN_POINT('Ctrl Pts',(-16.1933873263743,-19.2664634201503,
2.24890449694196));
#151168=CARTESIAN_POINT('Ctrl Pts',(-16.2037176087591,-19.3499238313371,
2.25308006086205));
#151169=CARTESIAN_POINT('Ctrl Pts',(-16.218157311486,-19.4328145349867,
2.25725562478214));
#151170=CARTESIAN_POINT('Ctrl Pts',(-16.2366094603544,-19.5147081770231,
2.26143118870224));
#151171=CARTESIAN_POINT('Ctrl Pts',(-16.2559935873087,-19.6007380895988,
2.26581765131481));
#151172=CARTESIAN_POINT('Ctrl Pts',(-16.2798059943325,-19.6856670076961,
2.27020411392739));
#151173=CARTESIAN_POINT('Ctrl Pts',(-16.3078756047366,-19.7690192278691,
2.27459057653996));
#151174=CARTESIAN_POINT('Ctrl Pts',(-16.3359452151407,-19.8523714480422,
2.27897703915253));
#151175=CARTESIAN_POINT('Ctrl Pts',(-16.3682717448823,-19.9341464586679,
2.28336350176511));
#151176=CARTESIAN_POINT('Ctrl Pts',(-16.4046276535555,-20.0138966388589,
2.28774996437768));
#151177=CARTESIAN_POINT('Ctrl Pts',(-16.4393112999405,-20.0899785509834,
2.29193466292291));
#151178=CARTESIAN_POINT('Ctrl Pts',(-16.4777908907529,-20.1645010086698,
2.29611936146814));
#151179=CARTESIAN_POINT('Ctrl Pts',(-16.5199038099267,-20.2370595554693,
2.30030406001337));
#151180=CARTESIAN_POINT('Ctrl Pts',(-16.5619476212891,-20.309499032813,
2.30448189141751));
#151181=CARTESIAN_POINT('Ctrl Pts',(-16.6076126789554,-20.3799806118441,
2.30865972282164));
#151182=CARTESIAN_POINT('Ctrl Pts',(-16.6566890879459,-20.448121443821,
2.31283755422578));
#151183=CARTESIAN_POINT('Ctrl Pts',(-16.7057182446913,-20.516196667752,
2.31701136308798));
#151184=CARTESIAN_POINT('Ctrl Pts',(-16.7581519651898,-20.5819352475649,
2.32118517195017));
#151185=CARTESIAN_POINT('Ctrl Pts',(-16.8137358429733,-20.6449812660625,
2.32535898081237));
#151186=CARTESIAN_POINT('Ctrl Pts',(-16.869286579699,-20.7079896943122,
2.32953030110331));
#151187=CARTESIAN_POINT('Ctrl Pts',(-16.9279834437401,-20.768308402384,
2.33370162139425));
#151188=CARTESIAN_POINT('Ctrl Pts',(-16.9895311180585,-20.8256137061672,
2.33787294168519));
#151189=CARTESIAN_POINT('Ctrl Pts',(-17.0486441410571,-20.8806521747689,
2.3418792563839));
#151190=CARTESIAN_POINT('Ctrl Pts',(-17.1103863961487,-20.9329108595394,
2.34588557108261));
#151191=CARTESIAN_POINT('Ctrl Pts',(-17.1744641402401,-20.9821349467765,
2.34989188578132));
#151192=CARTESIAN_POINT('Ctrl Pts',(-17.173927504734,-20.9828452456383,
1.55000082236257));
#151193=CARTESIAN_POINT('Ctrl Pts',(-17.7189175614377,-21.3927990620285,
1.58395752523188));
#151194=CARTESIAN_POINT('Ctrl Pts',(-19.3278236148535,-21.8312445050739,
1.66030616366168));
#151195=CARTESIAN_POINT('Ctrl Pts',(-21.0477247446925,-20.5363391578402,
1.75473569408639));
#151196=CARTESIAN_POINT('Ctrl Pts',(-21.2914430930582,-19.3178333754147,
1.81520852164178));
#151197=CARTESIAN_POINT('Ctrl Pts',(-21.2901593318677,-18.9530194399495,
1.8332894136367));
#151198=CARTESIAN_POINT('',(-21.2939995273704,-18.9504444089713,1.76670989019937));
#151199=CARTESIAN_POINT('Ctrl Pts',(-17.1744641402401,-20.9821349467765,
1.48324949998987));
#151200=CARTESIAN_POINT('Ctrl Pts',(-17.2411721150464,-21.0333795593612,
1.48742437517027));
#151201=CARTESIAN_POINT('Ctrl Pts',(-17.3103682156612,-21.0813018765702,
1.49159925035068));
#151202=CARTESIAN_POINT('Ctrl Pts',(-17.3816812909535,-21.1256683530757,
1.49577412553108));
#151203=CARTESIAN_POINT('Ctrl Pts',(-17.4530395002482,-21.1700629090974,
1.49995164298747));
#151204=CARTESIAN_POINT('Ctrl Pts',(-17.5265169491212,-21.2108969219799,
1.50412916044385));
#151205=CARTESIAN_POINT('Ctrl Pts',(-17.601718291717,-21.2479830428572,
1.50830667790024));
#151206=CARTESIAN_POINT('Ctrl Pts',(-17.677042648538,-21.2851298291464,
1.51249102893241));
#151207=CARTESIAN_POINT('Ctrl Pts',(-17.7540961057752,-21.3185163049187,
1.51667537996458));
#151208=CARTESIAN_POINT('Ctrl Pts',(-17.8324642291364,-21.348003600551,
1.52085973099674));
#151209=CARTESIAN_POINT('Ctrl Pts',(-17.8652394163241,-21.3603358039081,
1.5226097140569));
#151210=CARTESIAN_POINT('Ctrl Pts',(-17.8982443822024,-21.3719866124526,
1.52435969711706));
#151211=CARTESIAN_POINT('Ctrl Pts',(-17.9314482087024,-21.3829485025983,
1.52610968017722));
#151212=CARTESIAN_POINT('Ctrl Pts',(-18.01084679095,-21.4091611000027,1.53029432359276));
#151213=CARTESIAN_POINT('Ctrl Pts',(-18.0916786888191,-21.4315284615327,
1.53447896700831));
#151214=CARTESIAN_POINT('Ctrl Pts',(-18.1735366063454,-21.4498952708977,
1.53866361042385));
#151215=CARTESIAN_POINT('Ctrl Pts',(-18.2552780145749,-21.4682359385759,
1.54284229778925));
#151216=CARTESIAN_POINT('Ctrl Pts',(-18.3380420967243,-21.4825872643746,
1.54702098515466));
#151217=CARTESIAN_POINT('Ctrl Pts',(-18.4214050302511,-21.4928432428797,
1.55119967252006));
#151218=CARTESIAN_POINT('Ctrl Pts',(-18.5062619503251,-21.5032830236249,
1.5554532481175));
#151219=CARTESIAN_POINT('Ctrl Pts',(-18.5917389405056,-21.5094790670787,
1.55970682371494));
#151220=CARTESIAN_POINT('Ctrl Pts',(-18.6773765369535,-21.5113737092173,
1.56396039931238));
#151221=CARTESIAN_POINT('Ctrl Pts',(-18.7613541250249,-21.513231625409,
1.56813152314313));
#151222=CARTESIAN_POINT('Ctrl Pts',(-18.8454856674055,-21.510953399411,
1.57230264697389));
#151223=CARTESIAN_POINT('Ctrl Pts',(-18.9293330517837,-21.5045369730683,
1.57647377080464));
#151224=CARTESIAN_POINT('Ctrl Pts',(-19.0131523042948,-21.4981226995185,
1.58064349517013));
#151225=CARTESIAN_POINT('Ctrl Pts',(-19.0966871298398,-21.4875730181186,
1.58481321953563));
#151226=CARTESIAN_POINT('Ctrl Pts',(-19.179501972955,-21.4729379191272,
1.58898294390113));
#151227=CARTESIAN_POINT('Ctrl Pts',(-19.2623138727389,-21.4583033402833,
1.59315252007));
#151228=CARTESIAN_POINT('Ctrl Pts',(-19.3444053881076,-21.4395837134394,
1.59732209623888));
#151229=CARTESIAN_POINT('Ctrl Pts',(-19.4253499807632,-21.4168803630397,
1.60149167240775));
#151230=CARTESIAN_POINT('Ctrl Pts',(-19.5091400560411,-21.3933789112856,
1.60580782361199));
#151231=CARTESIAN_POINT('Ctrl Pts',(-19.5917005611986,-21.3656085745896,
1.61012397481624));
#151232=CARTESIAN_POINT('Ctrl Pts',(-19.6725761234496,-21.3337377816398,
1.61444012602048));
#151233=CARTESIAN_POINT('Ctrl Pts',(-19.7508175799528,-21.3029050159575,
1.61861570078383));
#151234=CARTESIAN_POINT('Ctrl Pts',(-19.8274817556368,-21.2682350333859,
1.62279127554719));
#151235=CARTESIAN_POINT('Ctrl Pts',(-19.9021790201189,-21.2299283959234,
1.62696685031055));
#151236=CARTESIAN_POINT('Ctrl Pts',(-19.9806484631081,-21.1896872903713,
1.63135328973523));
#151237=CARTESIAN_POINT('Ctrl Pts',(-20.0569466040008,-21.1454328549357,
1.63573972915991));
#151238=CARTESIAN_POINT('Ctrl Pts',(-20.1306554964563,-21.0974494690434,
1.6401261685846));
#151239=CARTESIAN_POINT('Ctrl Pts',(-20.2043643889117,-21.049466083151,
1.64451260800928));
#151240=CARTESIAN_POINT('Ctrl Pts',(-20.2754836084046,-20.9977541495255,
1.64889904743396));
#151241=CARTESIAN_POINT('Ctrl Pts',(-20.34363649293,-20.9426457144927,1.65328548685865));
#151242=CARTESIAN_POINT('Ctrl Pts',(-20.4078056269716,-20.8907585408379,
1.65741552510087));
#151243=CARTESIAN_POINT('Ctrl Pts',(-20.469597781961,-20.8356563927705,
1.6615455633431));
#151244=CARTESIAN_POINT('Ctrl Pts',(-20.5286666481821,-20.7775880208587,
1.66567560158532));
#151245=CARTESIAN_POINT('Ctrl Pts',(-20.5888757444006,-20.7183987318922,
1.66988536361091));
#151246=CARTESIAN_POINT('Ctrl Pts',(-20.6462548721938,-20.6561277358796,
1.67409512563649));
#151247=CARTESIAN_POINT('Ctrl Pts',(-20.70047016696,-20.5910836105752,1.67830488766208));
#151248=CARTESIAN_POINT('Ctrl Pts',(-20.7535207637169,-20.5274368172154,
1.68242421208196));
#151249=CARTESIAN_POINT('Ctrl Pts',(-20.8035417749399,-20.4611352293305,
1.68654353650185));
#151250=CARTESIAN_POINT('Ctrl Pts',(-20.8502568537434,-20.3925057892921,
1.69066286092173));
#151251=CARTESIAN_POINT('Ctrl Pts',(-20.8969436352055,-20.3239179210705,
1.69477969008884));
#151252=CARTESIAN_POINT('Ctrl Pts',(-20.940328192166,-20.2530053887166,
1.69889651925596));
#151253=CARTESIAN_POINT('Ctrl Pts',(-20.9801755792367,-20.1801267309364,
1.70301334842307));
#151254=CARTESIAN_POINT('Ctrl Pts',(-21.0200115219931,-20.1072690041715,
1.70712899522189));
#151255=CARTESIAN_POINT('Ctrl Pts',(-21.0563120854056,-20.0324466882332,
1.71124464202071));
#151256=CARTESIAN_POINT('Ctrl Pts',(-21.0888874490411,-19.9560443726991,
1.71536028881953));
#151257=CARTESIAN_POINT('Ctrl Pts',(-21.122756810271,-19.8766071129166,
1.71963942226786));
#151258=CARTESIAN_POINT('Ctrl Pts',(-21.1525985823987,-19.7954621912662,
1.72391855571618));
#151259=CARTESIAN_POINT('Ctrl Pts',(-21.1782545829907,-19.7130647367531,
1.7281976891645));
#151260=CARTESIAN_POINT('Ctrl Pts',(-21.2029529666689,-19.6337427887209,
1.73231710284076));
#151261=CARTESIAN_POINT('Ctrl Pts',(-21.2237724306601,-19.5532606399815,
1.73643651651702));
#151262=CARTESIAN_POINT('Ctrl Pts',(-21.2406233757609,-19.4720377410235,
1.74055593019328));
#151263=CARTESIAN_POINT('Ctrl Pts',(-21.257483616485,-19.3907700364207,
1.74467761629503));
#151264=CARTESIAN_POINT('Ctrl Pts',(-21.2703709111432,-19.3087612356736,
1.74879930239678));
#151265=CARTESIAN_POINT('Ctrl Pts',(-21.2792473404998,-19.2264375624415,
1.75292098849853));
#151266=CARTESIAN_POINT('Ctrl Pts',(-21.2881358445687,-19.1440019033387,
1.75704828137884));
#151267=CARTESIAN_POINT('Ctrl Pts',(-21.2930025792327,-19.061250988371,
1.76117557425916));
#151268=CARTESIAN_POINT('Ctrl Pts',(-21.2938616786583,-18.9786117668865,
1.76530286713947));
#151269=CARTESIAN_POINT('Ctrl Pts',(-21.293959302996,-18.969221003687,1.76577187482611));
#151270=CARTESIAN_POINT('Ctrl Pts',(-21.2940052315708,-18.95983167724,1.76624088251274));
#151271=CARTESIAN_POINT('Ctrl Pts',(-21.2939995273704,-18.9504444089713,
1.76670989019937));
#151272=CARTESIAN_POINT('Ctrl Pts',(-21.29399952737,-18.9504444083884,1.7667098902285));
#151273=CARTESIAN_POINT('Ctrl Pts',(-21.2939437779003,-18.8586988530854,
1.77129369133236));
#151274=CARTESIAN_POINT('Ctrl Pts',(-21.2889563823031,-18.7671041917188,
1.77587749243622));
#151275=CARTESIAN_POINT('Ctrl Pts',(-21.2790836671927,-18.6760486872856,
1.78046129354008));
#151276=CARTESIAN_POINT('Ctrl Pts',(-21.2700706759119,-18.5929223680962,
1.78464593362342));
#151277=CARTESIAN_POINT('Ctrl Pts',(-21.2569640808322,-18.5100833893621,
1.78883057370677));
#151278=CARTESIAN_POINT('Ctrl Pts',(-21.2397911341478,-18.4279668025532,
1.79301521379011));
#151279=CARTESIAN_POINT('Ctrl Pts',(-21.2226426307479,-18.3459670972049,
1.79719389762437));
#151280=CARTESIAN_POINT('Ctrl Pts',(-21.2014393656626,-18.2646881878446,
1.80137258145863));
#151281=CARTESIAN_POINT('Ctrl Pts',(-21.1762603194833,-18.1845597535461,
1.80555126529289));
#151282=CARTESIAN_POINT('Ctrl Pts',(-21.1506300008844,-18.1029952143143,
1.80980484174825));
#151283=CARTESIAN_POINT('Ctrl Pts',(-21.1208800336003,-18.0226232755941,
1.81405841820361));
#151284=CARTESIAN_POINT('Ctrl Pts',(-21.0871481586077,-17.9438860463016,
1.81831199465897));
#151285=CARTESIAN_POINT('Ctrl Pts',(-21.0540701842775,-17.866675157493,
1.82248311449243));
#151286=CARTESIAN_POINT('Ctrl Pts',(-21.0171634947162,-17.7910366074843,
1.82665423432589));
#151287=CARTESIAN_POINT('Ctrl Pts',(-20.9766076064455,-17.7173700459194,
1.83082535415935));
#151288=CARTESIAN_POINT('Ctrl Pts',(-20.9360653268187,-17.6437282033794,
1.83499507436165));
#151289=CARTESIAN_POINT('Ctrl Pts',(-20.8918765020354,-17.5720574377846,
1.83916479456395));
#151290=CARTESIAN_POINT('Ctrl Pts',(-20.8442669678557,-17.5027335219578,
1.84333451476625));
#151291=CARTESIAN_POINT('Ctrl Pts',(-20.7966591276122,-17.4334120726597,
1.84750408661088));
#151292=CARTESIAN_POINT('Ctrl Pts',(-20.7456310810944,-17.3664376858416,
1.8516736584555));
#151293=CARTESIAN_POINT('Ctrl Pts',(-20.6914516584179,-17.3021566726028,
1.85584323030013));
#151294=CARTESIAN_POINT('Ctrl Pts',(-20.6353675232618,-17.2356158189659,
1.86015938612691));
#151295=CARTESIAN_POINT('Ctrl Pts',(-20.5759066443104,-17.1719616467127,
1.8644755419537));
#151296=CARTESIAN_POINT('Ctrl Pts',(-20.5134108747745,-17.111538933111,
1.86879169778048));
#151297=CARTESIAN_POINT('Ctrl Pts',(-20.4529507162969,-17.0530843070278,
1.87296726785888));
#151298=CARTESIAN_POINT('Ctrl Pts',(-20.3896507223166,-16.9976541361553,
1.87714283793729));
#151299=CARTESIAN_POINT('Ctrl Pts',(-20.3238547745764,-16.9455200485037,
1.88131840801569));
#151300=CARTESIAN_POINT('Ctrl Pts',(-20.2547359371302,-16.8907530354344,
1.88570485671667));
#151301=CARTESIAN_POINT('Ctrl Pts',(-20.182862878563,-16.8396241326094,
1.89009130541764));
#151302=CARTESIAN_POINT('Ctrl Pts',(-20.1086675044515,-16.7923960427418,
1.89447775411861));
#151303=CARTESIAN_POINT('Ctrl Pts',(-20.03447213034,-16.7451679528743,1.89886420281958));
#151304=CARTESIAN_POINT('Ctrl Pts',(-19.9579549830438,-16.7018408956605,
1.90325065152055));
#151305=CARTESIAN_POINT('Ctrl Pts',(-19.8795742651273,-16.6626202580004,
1.90763710022152));
#151306=CARTESIAN_POINT('Ctrl Pts',(-19.8047997208725,-16.6252041002467,
1.91182173531074));
#151307=CARTESIAN_POINT('Ctrl Pts',(-19.7280509965214,-16.5913855369158,
1.91600637039996));
#151308=CARTESIAN_POINT('Ctrl Pts',(-19.649708651428,-16.5613771385474,
1.92019100548918));
#151309=CARTESIAN_POINT('Ctrl Pts',(-19.5714778164139,-16.5314114532082,
1.92436968429779));
#151310=CARTESIAN_POINT('Ctrl Pts',(-19.4916582921575,-16.5052453236535,
1.9285483631064));
#151311=CARTESIAN_POINT('Ctrl Pts',(-19.4106541203679,-16.4830449170977,
1.93272704191501));
#151312=CARTESIAN_POINT('Ctrl Pts',(-19.3281980247582,-16.4604465890721,
1.93698061962285));
#151313=CARTESIAN_POINT('Ctrl Pts',(-19.2445148259725,-16.4419577675855,
1.94123419733068));
#151314=CARTESIAN_POINT('Ctrl Pts',(-19.1600508251799,-16.4277019402686,
1.94548777503851));
#151315=CARTESIAN_POINT('Ctrl Pts',(-19.0772243047194,-16.4137224867517,
1.94965888980624));
#151316=CARTESIAN_POINT('Ctrl Pts',(-18.9936474609864,-16.4038134443357,
1.95383000457398));
#151317=CARTESIAN_POINT('Ctrl Pts',(-18.9097535040447,-16.3980401910335,
1.95800111934171));
#151318=CARTESIAN_POINT('Ctrl Pts',(-18.8258876980693,-16.3922688749706,
1.96217083447453));
#151319=CARTESIAN_POINT('Ctrl Pts',(-18.7417054487799,-16.3906306234224,
1.96634054960734));
#151320=CARTESIAN_POINT('Ctrl Pts',(-18.6576449613787,-16.3931389431864,
1.97051026474016));
#151321=CARTESIAN_POINT('Ctrl Pts',(-18.5735874647729,-16.3956471737067,
1.97467983151832));
#151322=CARTESIAN_POINT('Ctrl Pts',(-18.4896521812446,-16.4023016676361,
1.97884939829647));
#151323=CARTESIAN_POINT('Ctrl Pts',(-18.4062758154027,-16.4130638332502,
1.98301896507463));
#151324=CARTESIAN_POINT('Ctrl Pts',(-18.319968075054,-16.4242043787278,
1.98733512689366));
#151325=CARTESIAN_POINT('Ctrl Pts',(-18.2342598093425,-16.439746750557,
1.99165128871269));
#151326=CARTESIAN_POINT('Ctrl Pts',(-18.1496259627856,-16.4595901250738,
1.99596745053171));
#151327=CARTESIAN_POINT('Ctrl Pts',(-18.0677490201717,-16.4787871118902,
2.00014301560344));
#151328=CARTESIAN_POINT('Ctrl Pts',(-17.9868780138239,-16.502009022233,
2.00431858067517));
#151329=CARTESIAN_POINT('Ctrl Pts',(-17.9074274756712,-16.5291137331635,
2.0084941457469));
#151330=CARTESIAN_POINT('Ctrl Pts',(-17.8239641319306,-16.5575874207934,
2.01288060593958));
#151331=CARTESIAN_POINT('Ctrl Pts',(-17.7420690633719,-16.590346235575,
2.01726706613225));
#151332=CARTESIAN_POINT('Ctrl Pts',(-17.6621969477419,-16.6271692067657,
2.02165352632493));
#151333=CARTESIAN_POINT('Ctrl Pts',(-17.5823248321119,-16.6639921779565,
2.0260399865176));
#151334=CARTESIAN_POINT('Ctrl Pts',(-17.504476147719,-16.7048789684268,
2.03042644671028));
#151335=CARTESIAN_POINT('Ctrl Pts',(-17.4290716122241,-16.7495554711238,
2.03481290690295));
#151336=CARTESIAN_POINT('Ctrl Pts',(-17.357136554413,-16.7921763397919,
2.03899753937201));
#151337=CARTESIAN_POINT('Ctrl Pts',(-17.2871579127874,-16.8384044871301,
2.04318217184106));
#151338=CARTESIAN_POINT('Ctrl Pts',(-17.2195204149456,-16.8880349841983,
2.04736680431012));
#151339=CARTESIAN_POINT('Ctrl Pts',(-17.1519791912745,-16.9375948379828,
2.05154548043789));
#151340=CARTESIAN_POINT('Ctrl Pts',(-17.086772860019,-16.9905471522445,
2.05572415656566));
#151341=CARTESIAN_POINT('Ctrl Pts',(-17.0242598415601,-17.0466421358133,
2.05990283269343));
#151342=CARTESIAN_POINT('Ctrl Pts',(-16.9606262851279,-17.1037426148895,
2.06415641106388));
#151343=CARTESIAN_POINT('Ctrl Pts',(-16.8997839645222,-17.1640992941634,
2.06840998943434));
#151344=CARTESIAN_POINT('Ctrl Pts',(-16.8420782884877,-17.2274037465225,
2.07266356780479));
#151345=CARTESIAN_POINT('Ctrl Pts',(-16.785491383458,-17.2894808813865,
2.07683467976165));
#151346=CARTESIAN_POINT('Ctrl Pts',(-16.731920908933,-17.3543921535987,
2.08100579171851));
#151347=CARTESIAN_POINT('Ctrl Pts',(-16.6816563258902,-17.4218086906071,
2.08517690367537));
#151348=CARTESIAN_POINT('Ctrl Pts',(-16.6314086098611,-17.4892026050136,
2.08934661595479));
#151349=CARTESIAN_POINT('Ctrl Pts',(-16.5844648568947,-17.5590997461159,
2.09351632823422));
#151350=CARTESIAN_POINT('Ctrl Pts',(-16.5410736162982,-17.6311389642871,
2.09768604051365));
#151351=CARTESIAN_POINT('Ctrl Pts',(-16.4976839199281,-17.7031756186953,
2.10185560439955));
#151352=CARTESIAN_POINT('Ctrl Pts',(-16.4578467211853,-17.7773538040915,
2.10602516828545));
#151353=CARTESIAN_POINT('Ctrl Pts',(-16.4217659505504,-17.8532854326233,
2.11019473217135));
#151354=CARTESIAN_POINT('Ctrl Pts',(-16.3844165855094,-17.9318868056618,
2.1145108972891));
#151355=CARTESIAN_POINT('Ctrl Pts',(-16.3510929501845,-18.0123667456603,
2.11882706240685));
#151356=CARTESIAN_POINT('Ctrl Pts',(-16.3219673471267,-18.094271324093,
2.1231432275246));
#151357=CARTESIAN_POINT('Ctrl Pts',(-16.2937905370921,-18.1735077863526,
2.12731878963606));
#151358=CARTESIAN_POINT('Ctrl Pts',(-16.2695425399181,-18.2540770297308,
2.13149435174752));
#151359=CARTESIAN_POINT('Ctrl Pts',(-16.2493282310178,-18.3355535705167,
2.13566991385898));
#151360=CARTESIAN_POINT('Ctrl Pts',(-16.2280929125411,-18.421145430248,
2.14005638047988));
#151361=CARTESIAN_POINT('Ctrl Pts',(-16.2113095992892,-18.5077380811988,
2.14444284710078));
#151362=CARTESIAN_POINT('Ctrl Pts',(-16.1990385986542,-18.5948296013288,
2.14882931372168));
#151363=CARTESIAN_POINT('Ctrl Pts',(-16.1867675980192,-18.6819211214589,
2.15321578034258));
#151364=CARTESIAN_POINT('Ctrl Pts',(-16.1790088854275,-18.7695109260976,
2.15760224696348));
#151365=CARTESIAN_POINT('Ctrl Pts',(-16.1757597065435,-18.8570968865864,
2.16198871358438));
#151366=CARTESIAN_POINT('Ctrl Pts',(-16.1726599323311,-18.9406554444202,
2.16617348044408));
#151367=CARTESIAN_POINT('Ctrl Pts',(-16.1736525434599,-19.0245215348921,
2.17035824730378));
#151368=CARTESIAN_POINT('Ctrl Pts',(-16.1787734749095,-19.1082606971499,
2.17454301416348));
#151369=CARTESIAN_POINT('Ctrl Pts',(-16.1838870737151,-19.1918799535929,
2.17872178887008));
#151370=CARTESIAN_POINT('Ctrl Pts',(-16.1931172227911,-19.2753721875309,
2.18290056357669));
#151371=CARTESIAN_POINT('Ctrl Pts',(-16.2064478895621,-19.3583007863897,
2.18707933828329));
#151372=CARTESIAN_POINT('Ctrl Pts',(-16.2197626541988,-19.4411304598357,
2.19125312813524));
#151373=CARTESIAN_POINT('Ctrl Pts',(-16.2371681396007,-19.5233973830479,
2.19542691798718));
#151374=CARTESIAN_POINT('Ctrl Pts',(-16.2585964580771,-19.604669368544,
2.19960070783913));
#151375=CARTESIAN_POINT('Ctrl Pts',(-16.2800107743008,-19.685888247172,
2.20377177034406));
#151376=CARTESIAN_POINT('Ctrl Pts',(-16.3054425872083,-19.7661130354452,
2.20794283284899));
#151377=CARTESIAN_POINT('Ctrl Pts',(-16.3347730134509,-19.8449220945941,
2.21211389535393));
#151378=CARTESIAN_POINT('Ctrl Pts',(-16.3640930724252,-19.9237032975281,
2.2162834835358));
#151379=CARTESIAN_POINT('Ctrl Pts',(-16.39730884696,-20.0010693347075,2.22045307171766));
#151380=CARTESIAN_POINT('Ctrl Pts',(-16.4342521400316,-20.0766153922879,
2.22462265989953));
#151381=CARTESIAN_POINT('Ctrl Pts',(-16.4711934569176,-20.152157408728,
2.22879202504011));
#151382=CARTESIAN_POINT('Ctrl Pts',(-16.5118616925174,-20.2258792266091,
2.23296139018068));
#151383=CARTESIAN_POINT('Ctrl Pts',(-16.5560418075785,-20.2973988672747,
2.23713075532125));
#151384=CARTESIAN_POINT('Ctrl Pts',(-16.6002584549483,-20.3689776471614,
2.2413035680883));
#151385=CARTESIAN_POINT('Ctrl Pts',(-16.6479925397301,-20.4383502207137,
2.24547638085536));
#151386=CARTESIAN_POINT('Ctrl Pts',(-16.6989849376185,-20.5051624821249,
2.24964919362241));
#151387=CARTESIAN_POINT('Ctrl Pts',(-16.7499993048254,-20.5720035286083,
2.25382380418396));
#151388=CARTESIAN_POINT('Ctrl Pts',(-16.8042744856599,-20.6362817129064,
2.25799841474552));
#151389=CARTESIAN_POINT('Ctrl Pts',(-16.8615116635141,-20.697676782719,
2.26217302530707));
#151390=CARTESIAN_POINT('Ctrl Pts',(-16.9188352988078,-20.7591645905165,
2.26635394166764));
#151391=CARTESIAN_POINT('Ctrl Pts',(-16.9791295379422,-20.8177602638219,
2.27053485802822));
#151392=CARTESIAN_POINT('Ctrl Pts',(-17.042059662408,-20.8731813797841,
2.27471577438879));
#151393=CARTESIAN_POINT('Ctrl Pts',(-17.0850057020011,-20.9110029709633,
2.27756899931215));
#151394=CARTESIAN_POINT('Ctrl Pts',(-17.1291786179257,-20.9473469165081,
2.28042222423552));
#151395=CARTESIAN_POINT('Ctrl Pts',(-17.1744641402401,-20.9821349467765,
2.28327544915889));
#151396=CARTESIAN_POINT('Origin',(-18.734,-18.952,-1.76670989022851));
#151397=CARTESIAN_POINT('',(-17.1744641402401,-20.9821349467765,3.14981136057519));
#151398=CARTESIAN_POINT('',(-17.1746506047673,-20.9818836121459,3.08342410085253));
#151399=CARTESIAN_POINT('',(-17.1744641402401,-20.9821349467765,-1.76670989022851));
#151400=CARTESIAN_POINT('',(-21.2939989850553,-18.9497204131755,2.63329010980608));
#151401=CARTESIAN_POINT('Ctrl Pts',(-21.2939989850553,-18.9497204131756,
2.63329010980608));
#151402=CARTESIAN_POINT('Ctrl Pts',(-21.2939071256071,-18.8465613267959,
2.63841342883209));
#151403=CARTESIAN_POINT('Ctrl Pts',(-21.287576105512,-18.7436786900576,
2.6435367478581));
#151404=CARTESIAN_POINT('Ctrl Pts',(-21.275128076311,-18.6417289897787,
2.64866006688411));
#151405=CARTESIAN_POINT('Ctrl Pts',(-21.262474961387,-18.538099631808,2.65386779441926));
#151406=CARTESIAN_POINT('Ctrl Pts',(-21.243501668497,-18.4354341184935,
2.65907552195442));
#151407=CARTESIAN_POINT('Ctrl Pts',(-21.2183850428296,-18.3343990293364,
2.66428324948958));
#151408=CARTESIAN_POINT('Ctrl Pts',(-21.2103562166424,-18.3021019691982,
2.66594796113372));
#151409=CARTESIAN_POINT('Ctrl Pts',(-21.2017000060005,-18.2699713447231,
2.66761267277785));
#151410=CARTESIAN_POINT('Ctrl Pts',(-21.1924232051049,-18.2380284707345,
2.66927738442199));
#151411=CARTESIAN_POINT('Ctrl Pts',(-21.1691038390101,-18.1577327328991,
2.67346201883518));
#151412=CARTESIAN_POINT('Ctrl Pts',(-21.1418030734485,-18.078431236944,
2.67764665324838));
#151413=CARTESIAN_POINT('Ctrl Pts',(-21.1106233366666,-18.0005476808522,
2.68183128766158));
#151414=CARTESIAN_POINT('Ctrl Pts',(-21.0794879803785,-17.922774982357,
2.68600996576595));
#151415=CARTESIAN_POINT('Ctrl Pts',(-21.0444847892945,-17.8464166382493,
2.69018864387031));
#151416=CARTESIAN_POINT('Ctrl Pts',(-21.0057661997858,-17.7718820679648,
2.69436732197468));
#151417=CARTESIAN_POINT('Ctrl Pts',(-20.9663536076263,-17.6960115195363,
2.69862089985504));
#151418=CARTESIAN_POINT('Ctrl Pts',(-20.923091244402,-17.6220312333053,
2.70287447773541));
#151419=CARTESIAN_POINT('Ctrl Pts',(-20.876191573922,-17.5503526618234,
2.70712805561577));
#151420=CARTESIAN_POINT('Ctrl Pts',(-20.8302011447859,-17.4800637188824,
2.71129916961465));
#151421=CARTESIAN_POINT('Ctrl Pts',(-20.780713445874,-17.411988443355,2.71547028361353));
#151422=CARTESIAN_POINT('Ctrl Pts',(-20.7279747026929,-17.3464892136704,
2.71964139761241));
#151423=CARTESIAN_POINT('Ctrl Pts',(-20.6752536565045,-17.2810119628825,
2.72381111195386));
#151424=CARTESIAN_POINT('Ctrl Pts',(-20.6192840209004,-17.2181093992113,
2.7279808262953));
#151425=CARTESIAN_POINT('Ctrl Pts',(-20.560353487424,-17.1581123393662,
2.73215054063675));
#151426=CARTESIAN_POINT('Ctrl Pts',(-20.5014250509472,-17.0981174144723,
2.73632010660198));
#151427=CARTESIAN_POINT('Ctrl Pts',(-20.4395362490537,-17.0410281154374,
2.74048967256721));
#151428=CARTESIAN_POINT('Ctrl Pts',(-20.3750119946107,-16.987138774991,
2.74465923853245));
#151429=CARTESIAN_POINT('Ctrl Pts',(-20.3082191477021,-16.9313547524167,
2.74897540124669));
#151430=CARTESIAN_POINT('Ctrl Pts',(-20.2386024799445,-16.879000234265,
2.75329156396094));
#151431=CARTESIAN_POINT('Ctrl Pts',(-20.1665585535975,-16.8303553571546,
2.75760772667519));
#151432=CARTESIAN_POINT('Ctrl Pts',(-20.0968614498203,-16.7832950812909,
2.76178329088814));
#151433=CARTESIAN_POINT('Ctrl Pts',(-20.0248932222052,-16.739706678548,
2.76595885510108));
#151434=CARTESIAN_POINT('Ctrl Pts',(-19.9510397172924,-16.6997978939418,
2.77013441931403));
#151435=CARTESIAN_POINT('Ctrl Pts',(-19.8734560486543,-16.6578734121683,
2.77452088127893));
#151436=CARTESIAN_POINT('Ctrl Pts',(-19.7937921742853,-16.6200102829178,
2.77890734324383));
#151437=CARTESIAN_POINT('Ctrl Pts',(-19.7125190809675,-16.5863921694029,
2.78329380520873));
#151438=CARTESIAN_POINT('Ctrl Pts',(-19.6312459876497,-16.552774055888,
2.78768026717362));
#151439=CARTESIAN_POINT('Ctrl Pts',(-19.5483642476804,-16.5234010802283,
2.79206672913852));
#151440=CARTESIAN_POINT('Ctrl Pts',(-19.464360786173,-16.4983958913426,
2.79645319110342));
#151441=CARTESIAN_POINT('Ctrl Pts',(-19.3842224476364,-16.4745412280211,
2.80063782549363));
#151442=CARTESIAN_POINT('Ctrl Pts',(-19.3027650531602,-16.454572455802,
2.80482245988384));
#151443=CARTESIAN_POINT('Ctrl Pts',(-19.2204003081582,-16.4386327884243,
2.80900709427406));
#151444=CARTESIAN_POINT('Ctrl Pts',(-19.138152799176,-16.4227158091903,
2.81318577235517));
#151445=CARTESIAN_POINT('Ctrl Pts',(-19.0550009527856,-16.4108166300768,
2.81736445043628));
#151446=CARTESIAN_POINT('Ctrl Pts',(-18.9713715368519,-16.403028687197,
2.8215431285174));
#151447=CARTESIAN_POINT('Ctrl Pts',(-18.8862431236693,-16.3951011510316,
2.82579670640354));
#151448=CARTESIAN_POINT('Ctrl Pts',(-18.8006203137754,-16.3914338261787,
2.83005028428969));
#151449=CARTESIAN_POINT('Ctrl Pts',(-18.7149640762876,-16.3920707756642,
2.83430386217583));
#151450=CARTESIAN_POINT('Ctrl Pts',(-18.630968452178,-16.3926953766405,
2.83847497615099));
#151451=CARTESIAN_POINT('Ctrl Pts',(-18.546941166232,-16.3974588441842,
2.84264609012615));
#151452=CARTESIAN_POINT('Ctrl Pts',(-18.4633201985532,-16.4063502901835,
2.84681720410131));
#151453=CARTESIAN_POINT('Ctrl Pts',(-18.3797272906974,-16.4152387525723,
2.85098691841891));
#151454=CARTESIAN_POINT('Ctrl Pts',(-18.296540887401,-16.4282523938205,
2.85515663273652));
#151455=CARTESIAN_POINT('Ctrl Pts',(-18.2141948751358,-16.4453283756812,
2.85932634705412));
#151456=CARTESIAN_POINT('Ctrl Pts',(-18.1318517930947,-16.4624037499053,
2.86349591299542));
#151457=CARTESIAN_POINT('Ctrl Pts',(-18.0503494929033,-16.4835410830848,
2.86766547893671));
#151458=CARTESIAN_POINT('Ctrl Pts',(-17.970111330977,-16.5086264916435,
2.87183504487801));
#151459=CARTESIAN_POINT('Ctrl Pts',(-17.8870520941434,-16.534593872258,
2.87615120762025));
#151460=CARTESIAN_POINT('Ctrl Pts',(-17.8053480471385,-16.5647919650888,
2.88046737036249));
#151461=CARTESIAN_POINT('Ctrl Pts',(-17.7254493921686,-16.5990389566669,
2.88478353310472));
#151462=CARTESIAN_POINT('Ctrl Pts',(-17.6481534275891,-16.6321703560501,
2.88895909729375));
#151463=CARTESIAN_POINT('Ctrl Pts',(-17.5725474425878,-16.6690906702012,
2.89313466148277));
#151464=CARTESIAN_POINT('Ctrl Pts',(-17.4990149692573,-16.7095879116805,
2.8973102256718));
#151465=CARTESIAN_POINT('Ctrl Pts',(-17.4217685453457,-16.752130572642,
2.90169668769064));
#151466=CARTESIAN_POINT('Ctrl Pts',(-17.346811100329,-16.7986206906176,
2.90608314970948));
#151467=CARTESIAN_POINT('Ctrl Pts',(-17.2745520021333,-16.8487616536581,
2.91046961172832));
#151468=CARTESIAN_POINT('Ctrl Pts',(-17.2022929039376,-16.8989026166987,
2.91485607374717));
#151469=CARTESIAN_POINT('Ctrl Pts',(-17.1327325650199,-16.9526940096935,
2.91924253576601));
#151470=CARTESIAN_POINT('Ctrl Pts',(-17.0662376770538,-17.0097927931961,
2.92362899778485));
#151471=CARTESIAN_POINT('Ctrl Pts',(-17.0028023176014,-17.0642643769008,
2.92781363217407));
#151472=CARTESIAN_POINT('Ctrl Pts',(-16.9419203976444,-17.1219484370566,
2.93199826656328));
#151473=CARTESIAN_POINT('Ctrl Pts',(-16.8839351856056,-17.1825763134456,
2.9361829009525));
#151474=CARTESIAN_POINT('Ctrl Pts',(-16.8260325083402,-17.2431178935555,
2.94036157903253));
#151475=CARTESIAN_POINT('Ctrl Pts',(-16.7710186644549,-17.3065946373125,
2.94454025711256));
#151476=CARTESIAN_POINT('Ctrl Pts',(-16.7192032202856,-17.3726982756761,
2.9487189351926));
#151477=CARTESIAN_POINT('Ctrl Pts',(-16.6664590214574,-17.4399867743277,
2.952972513079));
#151478=CARTESIAN_POINT('Ctrl Pts',(-16.6170293785859,-17.5099969539576,
2.95722609096541));
#151479=CARTESIAN_POINT('Ctrl Pts',(-16.5712008555433,-17.5823650629685,
2.96147966885181));
#151480=CARTESIAN_POINT('Ctrl Pts',(-16.5262608079009,-17.6533301748861,
2.96565078282569));
#151481=CARTESIAN_POINT('Ctrl Pts',(-16.4847837540971,-17.7265621993711,
2.96982189679957));
#151482=CARTESIAN_POINT('Ctrl Pts',(-16.4469976092765,-17.8016869709401,
2.97399301077346));
#151483=CARTESIAN_POINT('Ctrl Pts',(-16.4092241439622,-17.8767865336655,
2.97816272508971));
#151484=CARTESIAN_POINT('Ctrl Pts',(-16.3751393344499,-17.9537771714644,
2.98233243940597));
#151485=CARTESIAN_POINT('Ctrl Pts',(-16.3449251982367,-18.0322600413271,
2.98650215372222));
#151486=CARTESIAN_POINT('Ctrl Pts',(-16.3147121371724,-18.1107401184316,
2.9906717196621));
#151487=CARTESIAN_POINT('Ctrl Pts',(-16.2883696400365,-18.1907118923997,
2.99484128560198));
#151488=CARTESIAN_POINT('Ctrl Pts',(-16.2660311035624,-18.2717577444641,
2.99901085154186));
#151489=CARTESIAN_POINT('Ctrl Pts',(-16.2429071716547,-18.355653068883,
3.00332701428556));
#151490=CARTESIAN_POINT('Ctrl Pts',(-16.2240741377505,-18.4406988974033,
3.00764317702926));
#151491=CARTESIAN_POINT('Ctrl Pts',(-16.2096228114113,-18.5264182690326,
3.01195933977297));
#151492=CARTESIAN_POINT('Ctrl Pts',(-16.1956422355373,-18.6093453409713,
3.01613490396041));
#151493=CARTESIAN_POINT('Ctrl Pts',(-16.185762291265,-18.6929022752325,
3.02031046814786));
#151494=CARTESIAN_POINT('Ctrl Pts',(-16.1800123293529,-18.7766518372414,
3.0244860323353));
#151495=CARTESIAN_POINT('Ctrl Pts',(-16.173971950515,-18.8646313908073,
3.02887249435713));
#151496=CARTESIAN_POINT('Ctrl Pts',(-16.172489739197,-18.9528229589758,
3.03325895637896));
#151497=CARTESIAN_POINT('Ctrl Pts',(-16.1755378747839,-19.0407217776812,
3.0376454184008));
#151498=CARTESIAN_POINT('Ctrl Pts',(-16.1785860103708,-19.1286205963865,
3.04203188042263));
#151499=CARTESIAN_POINT('Ctrl Pts',(-16.1861643670755,-19.216226094126,
3.04641834244446));
#151500=CARTESIAN_POINT('Ctrl Pts',(-16.1981829862586,-19.3030442604849,
3.05080480446629));
#151501=CARTESIAN_POINT('Ctrl Pts',(-16.2096452990137,-19.3858438700305,
3.05498823010089));
#151502=CARTESIAN_POINT('Ctrl Pts',(-16.2251885633093,-19.4682355295088,
3.05917165573549));
#151503=CARTESIAN_POINT('Ctrl Pts',(-16.2447727253556,-19.5497855595166,
3.06335508137009));
#151504=CARTESIAN_POINT('Ctrl Pts',(-16.2643314314963,-19.6312295890802,
3.06753306930006));
#151505=CARTESIAN_POINT('Ctrl Pts',(-16.2879205024951,-19.7118337178596,
3.07171105723003));
#151506=CARTESIAN_POINT('Ctrl Pts',(-16.3154483597632,-19.7911709977758,
3.07588904515999));
#151507=CARTESIAN_POINT('Ctrl Pts',(-16.3429486961575,-19.8704289605388,
3.08006285616193));
#151508=CARTESIAN_POINT('Ctrl Pts',(-16.3743798496445,-19.9484221573035,
3.08423666716387));
#151509=CARTESIAN_POINT('Ctrl Pts',(-16.4095998941543,-20.0247367561263,
3.08841047816581));
#151510=CARTESIAN_POINT('Ctrl Pts',(-16.444795294454,-20.1009979560103,
3.09258136866391));
#151511=CARTESIAN_POINT('Ctrl Pts',(-16.4837741268821,-20.1755824748352,
3.09675225916201));
#151512=CARTESIAN_POINT('Ctrl Pts',(-16.5263461035702,-20.2480957810201,
3.10092314966012));
#151513=CARTESIAN_POINT('Ctrl Pts',(-16.5689128842207,-20.3206002367383,
3.10509353108851));
#151514=CARTESIAN_POINT('Ctrl Pts',(-16.6150717177107,-20.3910335782552,
3.10926391251691));
#151515=CARTESIAN_POINT('Ctrl Pts',(-16.6645865127533,-20.4590261506693,
3.1134342939453));
#151516=CARTESIAN_POINT('Ctrl Pts',(-16.7140950873081,-20.5270101812535,
3.1176041514534));
#151517=CARTESIAN_POINT('Ctrl Pts',(-16.7669585097174,-20.5925536836102,
3.12177400896149));
#151518=CARTESIAN_POINT('Ctrl Pts',(-16.8228985547658,-20.6553177231579,
3.12594386646958));
#151519=CARTESIAN_POINT('Ctrl Pts',(-16.8788810408548,-20.7181293810289,
3.13011688759851));
#151520=CARTESIAN_POINT('Ctrl Pts',(-16.9379445036831,-20.7781570213184,
3.13428990872743));
#151521=CARTESIAN_POINT('Ctrl Pts',(-16.9997721932451,-20.8350968945538,
3.13846292985636));
#151522=CARTESIAN_POINT('Ctrl Pts',(-17.0558184987732,-20.886712433719,
3.14224574009597));
#151523=CARTESIAN_POINT('Ctrl Pts',(-17.1141355856602,-20.935790961425,
3.14602855033558));
#151524=CARTESIAN_POINT('Ctrl Pts',(-17.1744641402401,-20.9821349467765,
3.14981136057519));
#151525=CARTESIAN_POINT('Ctrl Pts',(-17.1744641402401,-20.9821349467765,
2.34989188578132));
#151526=CARTESIAN_POINT('Ctrl Pts',(-17.2411525456397,-21.0333645262761,
2.35406142611977));
#151527=CARTESIAN_POINT('Ctrl Pts',(-17.3103704829791,-21.0813066702107,
2.35823096645821));
#151528=CARTESIAN_POINT('Ctrl Pts',(-17.3817556000124,-21.1257145817016,
2.36240050679666));
#151529=CARTESIAN_POINT('Ctrl Pts',(-17.4566943588888,-21.1723331754607,
2.36677761215186));
#151530=CARTESIAN_POINT('Ctrl Pts',(-17.5340212076732,-21.2150562104906,
2.37115471750707));
#151531=CARTESIAN_POINT('Ctrl Pts',(-17.6132860090178,-21.2536516136064,
2.37553182286227));
#151532=CARTESIAN_POINT('Ctrl Pts',(-17.6888991971082,-21.290468983053,
2.37970728138738));
#151533=CARTESIAN_POINT('Ctrl Pts',(-17.7662752668567,-21.3235304882983,
2.38388273991248));
#151534=CARTESIAN_POINT('Ctrl Pts',(-17.8450031383188,-21.3526841899594,
2.38805819843759));
#151535=CARTESIAN_POINT('Ctrl Pts',(-17.9237867046597,-21.3818585159795,
2.39223661082962));
#151536=CARTESIAN_POINT('Ctrl Pts',(-18.003923537627,-21.4071193998067,
2.39641502322166));
#151537=CARTESIAN_POINT('Ctrl Pts',(-18.0849885035953,-21.4283650937482,
2.4005934356137));
#151538=CARTESIAN_POINT('Ctrl Pts',(-18.1661797209869,-21.4496438759549,
2.40477835550876));
#151539=CARTESIAN_POINT('Ctrl Pts',(-18.2483015058921,-21.4668949022888,
2.40896327540382));
#151540=CARTESIAN_POINT('Ctrl Pts',(-18.330920338965,-21.4800677971249,
2.41314819529888));
#151541=CARTESIAN_POINT('Ctrl Pts',(-18.3426179929777,-21.4819328920483,
2.41374072055229));
#151542=CARTESIAN_POINT('Ctrl Pts',(-18.3543256072978,-21.4837163198092,
2.41433324580571));
#151543=CARTESIAN_POINT('Ctrl Pts',(-18.3660419494156,-21.4854180217663,
2.41492577105912));
#151544=CARTESIAN_POINT('Ctrl Pts',(-18.4487871282886,-21.4974360758149,
2.41911040544306));
#151545=CARTESIAN_POINT('Ctrl Pts',(-18.5322757027619,-21.5054183621378,
2.42329503982701));
#151546=CARTESIAN_POINT('Ctrl Pts',(-18.6160795877488,-21.5092826938715,
2.42747967421096));
#151547=CARTESIAN_POINT('Ctrl Pts',(-18.6997641882828,-21.5131415252074,
2.43165835228604));
#151548=CARTESIAN_POINT('Ctrl Pts',(-18.7837627522474,-21.5128940235268,
2.43583703036112));
#151549=CARTESIAN_POINT('Ctrl Pts',(-18.8676394869462,-21.5085094342734,
2.4400157084362));
#151550=CARTESIAN_POINT('Ctrl Pts',(-18.9530196520595,-21.5040462543969,
2.44426928632388));
#151551=CARTESIAN_POINT('Ctrl Pts',(-19.0382731002349,-21.4952961442204,
2.44852286421156));
#151552=CARTESIAN_POINT('Ctrl Pts',(-19.1229373349518,-21.4822821481962,
2.45277644209924));
#151553=CARTESIAN_POINT('Ctrl Pts',(-19.2059601880618,-21.4695204539118,
2.45694755606894));
#151554=CARTESIAN_POINT('Ctrl Pts',(-19.2884159943141,-21.4526587990524,
2.46111867003864));
#151555=CARTESIAN_POINT('Ctrl Pts',(-19.369872949231,-21.4317712782505,
2.46528978400833));
#151556=CARTESIAN_POINT('Ctrl Pts',(-19.4513025704848,-21.4108907664568,
2.4694594983207));
#151557=CARTESIAN_POINT('Ctrl Pts',(-19.5317335608195,-21.3859871858364,
2.47362921263307));
#151558=CARTESIAN_POINT('Ctrl Pts',(-19.6107456770647,-21.3571854435258,
2.47779892694543));
#151559=CARTESIAN_POINT('Ctrl Pts',(-19.6897549817247,-21.3283847261029,
2.48196849288174));
#151560=CARTESIAN_POINT('Ctrl Pts',(-19.7673450807606,-21.2956862811391,
2.48613805881804));
#151561=CARTESIAN_POINT('Ctrl Pts',(-19.8431135302999,-21.2592640024292,
2.49030762475434));
#151562=CARTESIAN_POINT('Ctrl Pts',(-19.9215459053805,-21.2215611611749,
2.49462378750319));
#151563=CARTESIAN_POINT('Ctrl Pts',(-19.9980256738095,-21.179867982504,
2.49893995025204));
#151564=CARTESIAN_POINT('Ctrl Pts',(-20.0721336489206,-21.1344294576518,
2.50325611300089));
#151565=CARTESIAN_POINT('Ctrl Pts',(-20.1438275642521,-21.0904710881423,
2.50743167718557));
#151566=CARTESIAN_POINT('Ctrl Pts',(-20.2133014733427,-21.0430079392832,
2.51160724137025));
#151567=CARTESIAN_POINT('Ctrl Pts',(-20.2802065215959,-20.9923052204448,
2.51578280555493));
#151568=CARTESIAN_POINT('Ctrl Pts',(-20.3504907851974,-20.9390416274994,
2.52016926758587));
#151569=CARTESIAN_POINT('Ctrl Pts',(-20.4179394151666,-20.8822029788409,
2.5245557296168));
#151570=CARTESIAN_POINT('Ctrl Pts',(-20.4821902270813,-20.8221419544883,
2.52894219164774));
#151571=CARTESIAN_POINT('Ctrl Pts',(-20.546441038996,-20.7620809301358,
2.53332865367868));
#151572=CARTESIAN_POINT('Ctrl Pts',(-20.6074936847469,-20.6987980004695,
2.53771511570962));
#151573=CARTESIAN_POINT('Ctrl Pts',(-20.6650349200516,-20.6326856153193,
2.54210157774055));
#151574=CARTESIAN_POINT('Ctrl Pts',(-20.7194682477086,-20.5701440813393,
2.54625111891256));
#151575=CARTESIAN_POINT('Ctrl Pts',(-20.7709705307815,-20.5048282635486,
2.55040066008456));
#151576=CARTESIAN_POINT('Ctrl Pts',(-20.8192426277936,-20.4370465256121,
2.55455020125656));
#151577=CARTESIAN_POINT('Ctrl Pts',(-20.8674506257188,-20.3693547930364,
2.55869423237583));
#151578=CARTESIAN_POINT('Ctrl Pts',(-20.9124366796727,-20.2992040148273,
2.5628382634951));
#151579=CARTESIAN_POINT('Ctrl Pts',(-20.9539402798274,-20.226937313753,
2.56698229461437));
#151580=CARTESIAN_POINT('Ctrl Pts',(-20.9954017278076,-20.1547440086875,
2.57112211694398));
#151581=CARTESIAN_POINT('Ctrl Pts',(-21.0333875106771,-20.0804394498645,
2.57526193927359));
#151582=CARTESIAN_POINT('Ctrl Pts',(-21.0676798966755,-20.0043963796272,
2.5794017616032));
#151583=CARTESIAN_POINT('Ctrl Pts',(-21.1019481578627,-19.9284068059507,
2.5835386715536));
#151584=CARTESIAN_POINT('Ctrl Pts',(-21.1325279904582,-19.8506815753028,
2.58767558150399));
#151585=CARTESIAN_POINT('Ctrl Pts',(-21.1592478841602,-19.771617410977,
2.59181249145439));
#151586=CARTESIAN_POINT('Ctrl Pts',(-21.185962767488,-19.6925680723481,
2.59594862567316));
#151587=CARTESIAN_POINT('Ctrl Pts',(-21.2088189905539,-19.6121807387845,
2.60008475989194));
#151588=CARTESIAN_POINT('Ctrl Pts',(-21.2276938748169,-19.5308703297809,
2.60422089411071));
#151589=CARTESIAN_POINT('Ctrl Pts',(-21.2465668271854,-19.4495682431134,
2.60835660498518));
#151590=CARTESIAN_POINT('Ctrl Pts',(-21.2614591515706,-19.3673437264561,
2.61249231585964));
#151591=CARTESIAN_POINT('Ctrl Pts',(-21.2722989879432,-19.2846232821176,
2.61662802673411));
#151592=CARTESIAN_POINT('Ctrl Pts',(-21.2831447249165,-19.2018578093952,
2.62076598885829));
#151593=CARTESIAN_POINT('Ctrl Pts',(-21.2899335186421,-19.1185963356274,
2.62490395098247));
#151594=CARTESIAN_POINT('Ctrl Pts',(-21.2926453380223,-19.0352708485401,
2.62904191310665));
#151595=CARTESIAN_POINT('Ctrl Pts',(-21.2935733586036,-19.0067557610229,
2.6304579786616));
#151596=CARTESIAN_POINT('Ctrl Pts',(-21.2940243746442,-18.9782331861905,
2.63187404421655));
#151597=CARTESIAN_POINT('Ctrl Pts',(-21.2939989850559,-18.9497204138719,
2.6332901097715));
#151598=CARTESIAN_POINT('',(-21.2939990581247,-18.9541959965425,2.56670989022851));
#151599=CARTESIAN_POINT('Ctrl Pts',(-17.1744641402401,-20.9821349467765,
2.28327544915889));
#151600=CARTESIAN_POINT('Ctrl Pts',(-17.2056206582372,-21.0060691720155,
2.2852384728612));
#151601=CARTESIAN_POINT('Ctrl Pts',(-17.2373036935225,-21.0292671064051,
2.28720149656351));
#151602=CARTESIAN_POINT('Ctrl Pts',(-17.2694745299266,-21.0517059669168,
2.28916452026582));
#151603=CARTESIAN_POINT('Ctrl Pts',(-17.3380540324737,-21.0995395349439,
2.29334915467512));
#151604=CARTESIAN_POINT('Ctrl Pts',(-17.4091070955212,-21.1440987240518,
2.29753378908443));
#151605=CARTESIAN_POINT('Ctrl Pts',(-17.4822878905415,-21.1851181775792,
2.30171842349373));
#151606=CARTESIAN_POINT('Ctrl Pts',(-17.5553645218077,-21.2260792450197,
2.30589710159675));
#151607=CARTESIAN_POINT('Ctrl Pts',(-17.6305624715103,-21.2635103616649,
2.31007577969977));
#151608=CARTESIAN_POINT('Ctrl Pts',(-17.7075059666942,-21.2971886916808,
2.31425445780279));
#151609=CARTESIAN_POINT('Ctrl Pts',(-17.7858286182921,-21.331470681366,
2.31850803568381));
#151610=CARTESIAN_POINT('Ctrl Pts',(-17.8659596132195,-21.3618637479389,
2.32276161356483));
#151611=CARTESIAN_POINT('Ctrl Pts',(-17.947475192358,-21.3881811769579,
2.32701519144585));
#151612=CARTESIAN_POINT('Ctrl Pts',(-18.0274104335102,-21.4139883914482,
2.33118630544973));
#151613=CARTESIAN_POINT('Ctrl Pts',(-18.1086765942978,-21.4358764386359,
2.33535741945361));
#151614=CARTESIAN_POINT('Ctrl Pts',(-18.190854468218,-21.453717995959,2.33952853345749));
#151615=CARTESIAN_POINT('Ctrl Pts',(-18.2730047666085,-21.471553566386,
2.3436982478063));
#151616=CARTESIAN_POINT('Ctrl Pts',(-18.3560657213573,-21.4853452461106,
2.3478679621551));
#151617=CARTESIAN_POINT('Ctrl Pts',(-18.4396056840042,-21.4950163166424,
2.35203767650391));
#151618=CARTESIAN_POINT('Ctrl Pts',(-18.5231426739906,-21.5046870430418,
2.35620724247887));
#151619=CARTESIAN_POINT('Ctrl Pts',(-18.6071581809067,-21.5102373997233,
2.36037680845383));
#151620=CARTESIAN_POINT('Ctrl Pts',(-18.6912145089614,-21.5116424363095,
2.3645463744288));
#151621=CARTESIAN_POINT('Ctrl Pts',(-18.778226152585,-21.5130968722283,
2.36886253713867));
#151622=CARTESIAN_POINT('Ctrl Pts',(-18.8652810139473,-21.5101090568401,
2.37317869984854));
#151623=CARTESIAN_POINT('Ctrl Pts',(-18.9518945613345,-21.5027100893949,
2.37749486255841));
#151624=CARTESIAN_POINT('Ctrl Pts',(-19.0356866828292,-21.4955521424246,
2.38167042678694));
#151625=CARTESIAN_POINT('Ctrl Pts',(-19.1190653399572,-21.4842661264592,
2.38584599101547));
#151626=CARTESIAN_POINT('Ctrl Pts',(-19.2015998086144,-21.4689327402582,
2.390021555244));
#151627=CARTESIAN_POINT('Ctrl Pts',(-19.2883028950858,-21.4528249015418,
2.39440801719454));
#151628=CARTESIAN_POINT('Ctrl Pts',(-19.3740737042372,-21.4322502184737,
2.39879447914509));
#151629=CARTESIAN_POINT('Ctrl Pts',(-19.4584303876454,-21.4073616054374,
2.40318094109563));
#151630=CARTESIAN_POINT('Ctrl Pts',(-19.5427870710536,-21.3824729924011,
2.40756740304617));
#151631=CARTESIAN_POINT('Ctrl Pts',(-19.6257291066931,-21.3532707138335,
2.41195386499671));
#151632=CARTESIAN_POINT('Ctrl Pts',(-19.7068005673137,-21.3199651720906,
2.41634032694725));
#151633=CARTESIAN_POINT('Ctrl Pts',(-19.7841418063303,-21.2881920691418,
2.42052496109048));
#151634=CARTESIAN_POINT('Ctrl Pts',(-19.8600687027268,-21.2525667345391,
2.4247095952337));
#151635=CARTESIAN_POINT('Ctrl Pts',(-19.9341709431478,-21.2132363227278,
2.42889422937693));
#151636=CARTESIAN_POINT('Ctrl Pts',(-20.0081677081176,-21.1739618929342,
2.43307290720666));
#151637=CARTESIAN_POINT('Ctrl Pts',(-20.0803445730473,-21.1309930750319,
2.4372515850364));
#151638=CARTESIAN_POINT('Ctrl Pts',(-20.1503107695072,-21.0845252177121,
2.44143026286614));
#151639=CARTESIAN_POINT('Ctrl Pts',(-20.2215310651425,-21.0372244538674,
2.44568384081458));
#151640=CARTESIAN_POINT('Ctrl Pts',(-20.2904602140006,-20.9862981588784,
2.44993741876302));
#151641=CARTESIAN_POINT('Ctrl Pts',(-20.3567118459237,-20.932001582095,
2.45419099671146));
#151642=CARTESIAN_POINT('Ctrl Pts',(-20.4216790556215,-20.8787576545515,
2.45836211042625));
#151643=CARTESIAN_POINT('Ctrl Pts',(-20.4840712679219,-20.8222732635721,
2.46253322414104));
#151644=CARTESIAN_POINT('Ctrl Pts',(-20.5435545161742,-20.7628319781232,
2.46670433785583));
#151645=CARTESIAN_POINT('Ctrl Pts',(-20.6030178042074,-20.7034106388123,
2.47087405191028));
#151646=CARTESIAN_POINT('Ctrl Pts',(-20.6595737416717,-20.6410347004966,
2.47504376596472));
#151647=CARTESIAN_POINT('Ctrl Pts',(-20.7129241773316,-20.5760255848885,
2.47921348001916));
#151648=CARTESIAN_POINT('Ctrl Pts',(-20.7662727145228,-20.5110187826217,
2.48338304569485));
#151649=CARTESIAN_POINT('Ctrl Pts',(-20.8164156855257,-20.4433793455188,
2.48755261137053));
#151650=CARTESIAN_POINT('Ctrl Pts',(-20.8630951945853,-20.3734618012432,
2.49172217704622));
#151651=CARTESIAN_POINT('Ctrl Pts',(-20.9114159041743,-20.3010860325135,
2.49603834009476));
#151652=CARTESIAN_POINT('Ctrl Pts',(-20.9560247758173,-20.226269417489,
2.5003545031433));
#151653=CARTESIAN_POINT('Ctrl Pts',(-20.9966856911225,-20.1494362042253,
2.50467066619184));
#151654=CARTESIAN_POINT('Ctrl Pts',(-21.036022076007,-20.0751058349709,
2.50884623011182));
#151655=CARTESIAN_POINT('Ctrl Pts',(-21.0716636082435,-19.9988886784647,
2.5130217940318));
#151656=CARTESIAN_POINT('Ctrl Pts',(-21.1034449999269,-19.9211905861704,
2.51719735795179));
#151657=CARTESIAN_POINT('Ctrl Pts',(-21.1368316008925,-19.839568131463,
2.52158382056461));
#151658=CARTESIAN_POINT('Ctrl Pts',(-21.1659576672678,-19.756311755636,
2.52597028317742));
#151659=CARTESIAN_POINT('Ctrl Pts',(-21.1906909603509,-19.6719093868885,
2.53035674579024));
#151660=CARTESIAN_POINT('Ctrl Pts',(-21.215424253434,-19.5875070181411,
2.53474320840306));
#151661=CARTESIAN_POINT('Ctrl Pts',(-21.2357647130118,-19.5019592385496,
2.53912967101588));
#151662=CARTESIAN_POINT('Ctrl Pts',(-21.2516424693651,-19.4157632978678,
2.54351613362869));
#151663=CARTESIAN_POINT('Ctrl Pts',(-21.2744558895146,-19.2919155598001,
2.54981867489014));
#151664=CARTESIAN_POINT('Ctrl Pts',(-21.2881358177162,-19.1663368452798,
2.55612121615159));
#151665=CARTESIAN_POINT('Ctrl Pts',(-21.2924829866165,-19.0401181433864,
2.56242375741304));
#151666=CARTESIAN_POINT('Ctrl Pts',(-21.2934684379609,-19.0115058689788,
2.56385246835153));
#151667=CARTESIAN_POINT('Ctrl Pts',(-21.2939744691011,-18.982860830915,
2.56528117929002));
#151668=CARTESIAN_POINT('Ctrl Pts',(-21.2939990581247,-18.9541959965425,
2.56670989022851));
#151669=CARTESIAN_POINT('Ctrl Pts',(-21.2953147714723,-18.9541844553181,
2.56671052139392));
#151670=CARTESIAN_POINT('Ctrl Pts',(-21.288986792687,-18.2584132339351,
2.60137099436598));
#151671=CARTESIAN_POINT('Ctrl Pts',(-20.6359183782719,-16.7012242333178,
2.67842340289853));
#151672=CARTESIAN_POINT('Ctrl Pts',(-18.0006016698944,-16.0150938498363,
2.79786774699156));
#151673=CARTESIAN_POINT('Ctrl Pts',(-15.8675520976762,-17.9789803420861,
2.92504355367299));
#151674=CARTESIAN_POINT('Ctrl Pts',(-16.2393388133108,-20.1169975231494,
3.02022900495998));
#151675=CARTESIAN_POINT('Ctrl Pts',(-17.007518734373,-20.85614290823,3.0730225206865));
#151676=CARTESIAN_POINT('Ctrl Pts',(-17.1746506047676,-20.9818836121461,
3.08342410085255));
#151677=CARTESIAN_POINT('Origin',(-18.734,-18.952,-1.76670989022851));
#151678=CARTESIAN_POINT('',(-17.1744641402401,-20.9821349467765,3.94993168147533));
#151679=CARTESIAN_POINT('',(-17.1744641402401,-20.9821349467765,3.88329344502913));
#151680=CARTESIAN_POINT('',(-17.1744641402401,-20.9821349467765,-1.76670989022851));
#151681=CARTESIAN_POINT('',(-21.2939999971965,-18.9521198080496,3.43329010980363));
#151682=CARTESIAN_POINT('Ctrl Pts',(-21.2939999971965,-18.9521198080496,
3.43329010980363));
#151683=CARTESIAN_POINT('Ctrl Pts',(-21.294003905102,-18.8686175883755,
3.43746913841141));
#151684=CARTESIAN_POINT('Ctrl Pts',(-21.2899179933662,-18.784957797327,
3.44164816701919));
#151685=CARTESIAN_POINT('Ctrl Pts',(-21.2817219740999,-18.7015748760837,
3.44582719562697));
#151686=CARTESIAN_POINT('Ctrl Pts',(-21.2735376207105,-18.6183106386626,
3.45000027597723));
#151687=CARTESIAN_POINT('Ctrl Pts',(-21.2612548239782,-18.5353229435677,
3.45417335632749));
#151688=CARTESIAN_POINT('Ctrl Pts',(-21.2449053023278,-18.4530465324881,
3.45834643667775));
#151689=CARTESIAN_POINT('Ctrl Pts',(-21.228391285294,-18.3699423241145,
3.46256150311585));
#151690=CARTESIAN_POINT('Ctrl Pts',(-21.2077282378307,-18.287564271427,
3.46677656955394));
#151691=CARTESIAN_POINT('Ctrl Pts',(-21.1830026840864,-18.2063554108441,
3.47099163599204));
#151692=CARTESIAN_POINT('Ctrl Pts',(-21.1585674190593,-18.1260999774808,
3.47515721572331));
#151693=CARTESIAN_POINT('Ctrl Pts',(-21.1301646741428,-18.0469868800103,
3.47932279545459));
#151694=CARTESIAN_POINT('Ctrl Pts',(-21.0979289771719,-17.9694320426113,
3.48348837518587));
#151695=CARTESIAN_POINT('Ctrl Pts',(-21.0657039544922,-17.8919028861496,
3.48765257555777));
#151696=CARTESIAN_POINT('Ctrl Pts',(-21.0296486772609,-17.815931390789,
3.49181677592968));
#151697=CARTESIAN_POINT('Ctrl Pts',(-20.9899463178963,-17.7419147919381,
3.49598097630159));
#151698=CARTESIAN_POINT('Ctrl Pts',(-20.9502451090693,-17.6679003380199,
3.50014505599882));
#151699=CARTESIAN_POINT('Ctrl Pts',(-20.9068972472216,-17.5958410741357,
3.50430913569606));
#151700=CARTESIAN_POINT('Ctrl Pts',(-20.8601318431732,-17.5261096166098,
3.50847321539329));
#151701=CARTESIAN_POINT('Ctrl Pts',(-20.8123689128482,-17.4548907569624,
3.51272611670985));
#151702=CARTESIAN_POINT('Ctrl Pts',(-20.7610412266544,-17.3861005826242,
3.51697901802641));
#151703=CARTESIAN_POINT('Ctrl Pts',(-20.7064383509254,-17.3201032655836,
3.52123191934298));
#151704=CARTESIAN_POINT('Ctrl Pts',(-20.6528987388226,-17.2553910923328,
3.52540200532764));
#151705=CARTESIAN_POINT('Ctrl Pts',(-20.5962107113946,-17.1933642853479,
3.52957209131231));
#151706=CARTESIAN_POINT('Ctrl Pts',(-20.5366855500211,-17.1343298407728,
3.53374217729697));
#151707=CARTESIAN_POINT('Ctrl Pts',(-20.4753871892412,-17.0735368147901,
3.53803648627948));
#151708=CARTESIAN_POINT('Ctrl Pts',(-20.4110803806519,-17.0159176096093,
3.54233079526199));
#151709=CARTESIAN_POINT('Ctrl Pts',(-20.344141220394,-16.9617625140732,
3.5466251042445));
#151710=CARTESIAN_POINT('Ctrl Pts',(-20.277202060136,-16.9076074185371,
3.55091941322701));
#151711=CARTESIAN_POINT('Ctrl Pts',(-20.2076310154015,-16.8569166856669,
3.55521372220952));
#151712=CARTESIAN_POINT('Ctrl Pts',(-20.1358342086541,-16.8099307080659,
3.55950803119203));
#151713=CARTESIAN_POINT('Ctrl Pts',(-20.065871057879,-16.7641447297733,
3.56369266558497));
#151714=CARTESIAN_POINT('Ctrl Pts',(-19.9935321931096,-16.7217048000893,
3.56787729997791));
#151715=CARTESIAN_POINT('Ctrl Pts',(-19.9191711337668,-16.6828659396841,
3.57206193437085));
#151716=CARTESIAN_POINT('Ctrl Pts',(-19.844915918188,-16.6440823615894,
3.57624061245468));
#151717=CARTESIAN_POINT('Ctrl Pts',(-19.7686446296087,-16.6088898827212,
3.58041929053851));
#151718=CARTESIAN_POINT('Ctrl Pts',(-19.6907394622033,-16.5775001365629,
3.58459796862235));
#151719=CARTESIAN_POINT('Ctrl Pts',(-19.6114379006591,-16.545547751763,
3.58885154650781));
#151720=CARTESIAN_POINT('Ctrl Pts',(-19.5304437130242,-16.5175360325718,
3.59310512439327));
#151721=CARTESIAN_POINT('Ctrl Pts',(-19.4481859912091,-16.4936390887503,
3.59735870227873));
#151722=CARTESIAN_POINT('Ctrl Pts',(-19.3675229958469,-16.4702054338166,
3.60152981625657));
#151723=CARTESIAN_POINT('Ctrl Pts',(-19.2856454833717,-16.4507285663624,
3.60570093023441));
#151724=CARTESIAN_POINT('Ctrl Pts',(-19.202976239882,-16.4353233647474,
3.60987204421224));
#151725=CARTESIAN_POINT('Ctrl Pts',(-19.1203347368553,-16.4199233324967,
3.6140417585325));
#151726=CARTESIAN_POINT('Ctrl Pts',(-19.0369024823163,-16.408592336823,
3.61821147285276));
#151727=CARTESIAN_POINT('Ctrl Pts',(-18.9531132034112,-16.4013943064262,
3.62238118717302));
#151728=CARTESIAN_POINT('Ctrl Pts',(-18.8693269060884,-16.3941965321663,
3.62655075311695));
#151729=CARTESIAN_POINT('Ctrl Pts',(-18.785184068077,-16.3911314692988,
3.63072031906087));
#151730=CARTESIAN_POINT('Ctrl Pts',(-18.7011229313377,-16.3922111223079,
3.6348898850048));
#151731=CARTESIAN_POINT('Ctrl Pts',(-18.6141063087261,-16.393328734585,
3.63920604774385));
#151732=CARTESIAN_POINT('Ctrl Pts',(-18.5271777668962,-16.3988879352091,
3.6435222104829));
#151733=CARTESIAN_POINT('Ctrl Pts',(-18.4408207068908,-16.4088433193977,
3.64783837322196));
#151734=CARTESIAN_POINT('Ctrl Pts',(-18.3572767190368,-16.418474407993,
3.65201393741352));
#151735=CARTESIAN_POINT('Ctrl Pts',(-18.274268009732,-16.4322195436239,
3.65618950160509));
#151736=CARTESIAN_POINT('Ctrl Pts',(-18.1922227301015,-16.4499853338117,
3.66036506579665));
#151737=CARTESIAN_POINT('Ctrl Pts',(-18.1060335384336,-16.4686484318293,
3.66475152780945));
#151738=CARTESIAN_POINT('Ctrl Pts',(-18.0209082233737,-16.4917488722623,
3.66913798982225));
#151739=CARTESIAN_POINT('Ctrl Pts',(-17.9373239039192,-16.5191195676866,
3.67352445183505));
#151740=CARTESIAN_POINT('Ctrl Pts',(-17.8537395844646,-16.5464902631109,
3.67791091384785));
#151741=CARTESIAN_POINT('Ctrl Pts',(-17.7716967745984,-16.578130933778,
3.68229737586065));
#151742=CARTESIAN_POINT('Ctrl Pts',(-17.6916449845523,-16.6138177954293,
3.68668383787346));
#151743=CARTESIAN_POINT('Ctrl Pts',(-17.6152764960369,-16.647862651673,
3.69086847226646));
#151744=CARTESIAN_POINT('Ctrl Pts',(-17.5404355759515,-16.6857162600702,
3.69505310665946));
#151745=CARTESIAN_POINT('Ctrl Pts',(-17.4675280096795,-16.7272194045853,
3.69923774105246));
#151746=CARTESIAN_POINT('Ctrl Pts',(-17.394724218304,-16.7686634745113,
3.70341641913635));
#151747=CARTESIAN_POINT('Ctrl Pts',(-17.3238487109969,-16.813746536681,
3.70759509722024));
#151748=CARTESIAN_POINT('Ctrl Pts',(-17.2552863124839,-16.8622617794679,
3.71177377530414));
#151749=CARTESIAN_POINT('Ctrl Pts',(-17.1854949822514,-16.9116466231152,
3.71602735318959));
#151750=CARTESIAN_POINT('Ctrl Pts',(-17.1181009417722,-16.9645877049941,
3.72028093107504));
#151751=CARTESIAN_POINT('Ctrl Pts',(-17.0534828491147,-17.0208184690246,
3.72453450896048));
#151752=CARTESIAN_POINT('Ctrl Pts',(-16.9901175042762,-17.0759590899683,
3.72870562293838));
#151753=CARTESIAN_POINT('Ctrl Pts',(-16.9294217964547,-17.1342626616187,
3.73287673691628));
#151754=CARTESIAN_POINT('Ctrl Pts',(-16.8717211662673,-17.1954358692518,
3.73704785089418));
#151755=CARTESIAN_POINT('Ctrl Pts',(-16.8140398980835,-17.2565885496243,
3.7412175652145));
#151756=CARTESIAN_POINT('Ctrl Pts',(-16.7593520269263,-17.3206086192035,
3.74538727953482));
#151757=CARTESIAN_POINT('Ctrl Pts',(-16.7079460749934,-17.3871659854907,
3.74955699385514));
#151758=CARTESIAN_POINT('Ctrl Pts',(-16.6565419523049,-17.4537209833811,
3.75372655979912));
#151759=CARTESIAN_POINT('Ctrl Pts',(-16.6084197971694,-17.5228127338604,
3.75789612574311));
#151760=CARTESIAN_POINT('Ctrl Pts',(-16.5638269155198,-17.5940792425927,
3.76206569168709));
#151761=CARTESIAN_POINT('Ctrl Pts',(-16.5176662031612,-17.6678513938575,
3.76638185442608));
#151762=CARTESIAN_POINT('Ctrl Pts',(-16.4752878401623,-17.7439536306547,
3.77069801716506));
#151763=CARTESIAN_POINT('Ctrl Pts',(-16.4369153041026,-17.8219549124597,
3.77501417990404));
#151764=CARTESIAN_POINT('Ctrl Pts',(-16.39979274937,-17.8974153107121,3.77918974409566));
#151765=CARTESIAN_POINT('Ctrl Pts',(-16.3664191932587,-17.9746524800457,
3.78336530828728));
#151766=CARTESIAN_POINT('Ctrl Pts',(-16.3369478575573,-18.0532558615431,
3.78754087247891));
#151767=CARTESIAN_POINT('Ctrl Pts',(-16.3059879947497,-18.1358293129816,
3.79192733449157));
#151768=CARTESIAN_POINT('Ctrl Pts',(-16.2793350909185,-18.2199100618433,
3.79631379650423));
#151769=CARTESIAN_POINT('Ctrl Pts',(-16.2571069074461,-18.3050064853038,
3.8007002585169));
#151770=CARTESIAN_POINT('Ctrl Pts',(-16.2348787239738,-18.3901029087642,
3.80508672052956));
#151771=CARTESIAN_POINT('Ctrl Pts',(-16.2170753038452,-18.4762144232225,
3.80947318254223));
#151772=CARTESIAN_POINT('Ctrl Pts',(-16.2037517912764,-18.5628419315354,
3.81385964455489));
#151773=CARTESIAN_POINT('Ctrl Pts',(-16.1910413132713,-18.645483579777,
3.818044278948));
#151774=CARTESIAN_POINT('Ctrl Pts',(-16.182360236898,-18.7289023900138,
3.82222891334111));
#151775=CARTESIAN_POINT('Ctrl Pts',(-16.1777943305987,-18.812670980335,
3.82641354773422));
#151776=CARTESIAN_POINT('Ctrl Pts',(-16.1732349233019,-18.8963203364362,
3.83059222581821));
#151777=CARTESIAN_POINT('Ctrl Pts',(-16.1727790761929,-18.9803180282759,
3.83477090390221));
#151778=CARTESIAN_POINT('Ctrl Pts',(-16.1764611917473,-19.0642285359488,
3.83894958198621));
#151779=CARTESIAN_POINT('Ctrl Pts',(-16.1802093065766,-19.149643079165,
3.84320315987163));
#151780=CARTESIAN_POINT('Ctrl Pts',(-16.1882452624471,-19.2349668053833,
3.84745673775705));
#151781=CARTESIAN_POINT('Ctrl Pts',(-16.2005498883094,-19.3197370413416,
3.85171031564247));
#151782=CARTESIAN_POINT('Ctrl Pts',(-16.212615964989,-19.4028638408618,
3.85588142962048));
#151783=CARTESIAN_POINT('Ctrl Pts',(-16.2287866065492,-19.4854579433574,
3.86005254359849));
#151784=CARTESIAN_POINT('Ctrl Pts',(-16.2489913365583,-19.5670869390743,
3.8642236575765));
#151785=CARTESIAN_POINT('Ctrl Pts',(-16.2691892866752,-19.6486885433934,
3.86839337189693));
#151786=CARTESIAN_POINT('Ctrl Pts',(-16.293418526377,-19.7293252379216,
3.87256308621737));
#151787=CARTESIAN_POINT('Ctrl Pts',(-16.3215576717042,-19.8085757483414,
3.8767328005378));
#151788=CARTESIAN_POINT('Ctrl Pts',(-16.3496958157198,-19.887823438688,
3.8809023664819));
#151789=CARTESIAN_POINT('Ctrl Pts',(-16.3817434340021,-19.9656846097681,
3.885071932426));
#151790=CARTESIAN_POINT('Ctrl Pts',(-16.4175300086122,-20.041755375761,
3.8892414983701));
#151791=CARTESIAN_POINT('Ctrl Pts',(-16.454574795037,-20.1205006960403,
3.89355766110895));
#151792=CARTESIAN_POINT('Ctrl Pts',(-16.4956261286208,-20.1973268901832,
3.8978738238478));
#151793=CARTESIAN_POINT('Ctrl Pts',(-16.5404425366711,-20.2718127348508,
3.90218998658666));
#151794=CARTESIAN_POINT('Ctrl Pts',(-16.5837990549444,-20.3438722109649,
3.9063655507784));
#151795=CARTESIAN_POINT('Ctrl Pts',(-16.6306788183652,-20.4137411050174,
3.91054111497014));
#151796=CARTESIAN_POINT('Ctrl Pts',(-16.6808195479046,-20.4810683539769,
3.91471667916187));
#151797=CARTESIAN_POINT('Ctrl Pts',(-16.7334927664925,-20.5517961422228,
3.91910314117428));
#151798=CARTESIAN_POINT('Ctrl Pts',(-16.7897646588838,-20.619718331068,
3.92348960318669));
#151799=CARTESIAN_POINT('Ctrl Pts',(-16.849285590087,-20.6844697957155,
3.9278760651991));
#151800=CARTESIAN_POINT('Ctrl Pts',(-16.9088065212902,-20.749221260363,
3.93226252721151));
#151801=CARTESIAN_POINT('Ctrl Pts',(-16.9715760238563,-20.8108016487771,
3.93664898922392));
#151802=CARTESIAN_POINT('Ctrl Pts',(-17.0372042845901,-20.8688944415816,
3.94103545123633));
#151803=CARTESIAN_POINT('Ctrl Pts',(-17.0815714090152,-20.9081673118016,
3.944000861316));
#151804=CARTESIAN_POINT('Ctrl Pts',(-17.1273611506995,-20.945950750545,
3.94696627139566));
#151805=CARTESIAN_POINT('Ctrl Pts',(-17.1744641402401,-20.9821349467765,
3.94993168147533));
#151806=CARTESIAN_POINT('Ctrl Pts',(-17.1744641402401,-20.9821349467765,
3.14981136057519));
#151807=CARTESIAN_POINT('Ctrl Pts',(-17.2410960571067,-21.0333211321692,
3.15398941355794));
#151808=CARTESIAN_POINT('Ctrl Pts',(-17.3101818003053,-21.081170625289,
3.15816746654069));
#151809=CARTESIAN_POINT('Ctrl Pts',(-17.3813457473345,-21.1254595631725,
3.16234551952344));
#151810=CARTESIAN_POINT('Ctrl Pts',(-17.4526225822357,-21.169818756911,
3.16653020018116));
#151811=CARTESIAN_POINT('Ctrl Pts',(-17.5259837968862,-21.2106059047489,
3.17071488083887));
#151812=CARTESIAN_POINT('Ctrl Pts',(-17.6010303509287,-21.2476436514153,
3.17489956149659));
#151813=CARTESIAN_POINT('Ctrl Pts',(-17.619448495431,-21.2567335633885,
3.17592657804697));
#151814=CARTESIAN_POINT('Ctrl Pts',(-17.6379680672954,-21.2655978709631,
3.17695359459734));
#151815=CARTESIAN_POINT('Ctrl Pts',(-17.6565830150582,-21.2742344068933,
3.17798061114772));
#151816=CARTESIAN_POINT('Ctrl Pts',(-17.7324306249074,-21.3094244389056,
3.18216524554016));
#151817=CARTESIAN_POINT('Ctrl Pts',(-17.8101452346756,-21.3409601078314,
3.1863498799326));
#151818=CARTESIAN_POINT('Ctrl Pts',(-17.8893401694871,-21.3686401823023,
3.19053451432505));
#151819=CARTESIAN_POINT('Ctrl Pts',(-17.9684223801111,-21.3962808576132,
3.19471319240838));
#151820=CARTESIAN_POINT('Ctrl Pts',(-18.0489802999385,-21.4200766888001,
3.19889187049172));
#151821=CARTESIAN_POINT('Ctrl Pts',(-18.1306051532973,-21.4398735214984,
3.20307054857505));
#151822=CARTESIAN_POINT('Ctrl Pts',(-18.2136930735049,-21.4600251981987,
3.20732412646064));
#151823=CARTESIAN_POINT('Ctrl Pts',(-18.2978861156728,-21.4760328992745,
3.21157770434623));
#151824=CARTESIAN_POINT('Ctrl Pts',(-18.3827345240936,-21.4877863800873,
3.21583128223182));
#151825=CARTESIAN_POINT('Ctrl Pts',(-18.4659379805339,-21.4993119967375,
3.22000239620916));
#151826=CARTESIAN_POINT('Ctrl Pts',(-18.5497711422166,-21.5067468078098,
3.2241735101865));
#151827=CARTESIAN_POINT('Ctrl Pts',(-18.633799056368,-21.5100382661124,
3.22834462416384));
#151828=CARTESIAN_POINT('Ctrl Pts',(-18.7177987741413,-21.5133286199344,
3.2325143384836));
#151829=CARTESIAN_POINT('Ctrl Pts',(-18.8019926552973,-21.5124783642369,
3.23668405280337));
#151830=CARTESIAN_POINT('Ctrl Pts',(-18.8859422870026,-21.5074869480043,
3.24085376712313));
#151831=CARTESIAN_POINT('Ctrl Pts',(-18.9698889314197,-21.5024957093878,
3.24502333306657));
#151832=CARTESIAN_POINT('Ctrl Pts',(-19.0535908844956,-21.493363631381,
3.24919289901));
#151833=CARTESIAN_POINT('Ctrl Pts',(-19.136612772952,-21.4801421943902,
3.25336246495344));
#151834=CARTESIAN_POINT('Ctrl Pts',(-19.2225536086148,-21.4664559079808,
3.25767862769308));
#151835=CARTESIAN_POINT('Ctrl Pts',(-19.3077651468766,-21.4483874314134,
3.26199479043273));
#151836=CARTESIAN_POINT('Ctrl Pts',(-19.3917756297608,-21.4260515800793,
3.26631095317237));
#151837=CARTESIAN_POINT('Ctrl Pts',(-19.473049479976,-21.4044433167598,
3.27048651736345));
#151838=CARTESIAN_POINT('Ctrl Pts',(-19.5531988875818,-21.3788416169569,
3.27466208155453));
#151839=CARTESIAN_POINT('Ctrl Pts',(-19.6318137018706,-21.3494007918438,
3.27883764574561));
#151840=CARTESIAN_POINT('Ctrl Pts',(-19.7143991635781,-21.3184729806291,
3.28322410775954));
#151841=CARTESIAN_POINT('Ctrl Pts',(-19.7952903977544,-21.2833082561225,
3.28761056977346));
#151842=CARTESIAN_POINT('Ctrl Pts',(-19.8740394547189,-21.2441409297171,
3.29199703178738));
#151843=CARTESIAN_POINT('Ctrl Pts',(-19.9527885116833,-21.2049736033117,
3.29638349380131));
#151844=CARTESIAN_POINT('Ctrl Pts',(-20.0293949232976,-21.161804026126,
3.30076995581523));
#151845=CARTESIAN_POINT('Ctrl Pts',(-20.103446255522,-21.1149186191895,
3.30515641782916));
#151846=CARTESIAN_POINT('Ctrl Pts',(-20.1740903761505,-21.070190479346,
3.30934105222176));
#151847=CARTESIAN_POINT('Ctrl Pts',(-20.2426723273843,-21.0219144506012,
3.31352568661436));
#151848=CARTESIAN_POINT('Ctrl Pts',(-20.3088136057118,-20.97030674261,3.31771032100697));
#151849=CARTESIAN_POINT('Ctrl Pts',(-20.374860740116,-20.9187724918035,
3.32188899909045));
#151850=CARTESIAN_POINT('Ctrl Pts',(-20.4384737424745,-20.8639162618918,
3.32606767717394));
#151851=CARTESIAN_POINT('Ctrl Pts',(-20.4993017308436,-20.8059983276909,
3.33024635525743));
#151852=CARTESIAN_POINT('Ctrl Pts',(-20.5612200171964,-20.7470422561363,
3.33449993314298));
#151853=CARTESIAN_POINT('Ctrl Pts',(-20.6202520574043,-20.6849138964936,
3.33875351102852));
#151854=CARTESIAN_POINT('Ctrl Pts',(-20.6760617089388,-20.6199317488056,
3.34300708891407));
#151855=CARTESIAN_POINT('Ctrl Pts',(-20.7307893814671,-20.5562094068616,
3.34717820289155));
#151856=CARTESIAN_POINT('Ctrl Pts',(-20.7824181813927,-20.4897433069906,
3.35134931686903));
#151857=CARTESIAN_POINT('Ctrl Pts',(-20.8306684931562,-20.4208707328441,
3.3555204308465));
#151858=CARTESIAN_POINT('Ctrl Pts',(-20.8789026140616,-20.352021269555,
3.3596901451664));
#151859=CARTESIAN_POINT('Ctrl Pts',(-20.923760234583,-20.2807673121879,
3.36385985948629));
#151860=CARTESIAN_POINT('Ctrl Pts',(-20.965003586852,-20.2074771983009,
3.36802957380619));
#151861=CARTESIAN_POINT('Ctrl Pts',(-21.0062454715054,-20.1341896923909,
3.37219913974974));
#151862=CARTESIAN_POINT('Ctrl Pts',(-21.0438731187515,-20.0588665753507,
3.3763687056933));
#151863=CARTESIAN_POINT('Ctrl Pts',(-21.0776941561667,-19.9819017925755,
3.38053827163685));
#151864=CARTESIAN_POINT('Ctrl Pts',(-21.1127042995432,-19.9022310229647,
3.38485443437633));
#151865=CARTESIAN_POINT('Ctrl Pts',(-21.1436349596428,-19.8208014806364,
3.38917059711581));
#151866=CARTESIAN_POINT('Ctrl Pts',(-21.1703273243944,-19.7380719867856,
3.39348675985529));
#151867=CARTESIAN_POINT('Ctrl Pts',(-21.1961501881654,-19.6580373975152,
3.39766232404647));
#151868=CARTESIAN_POINT('Ctrl Pts',(-21.2180065643708,-19.5767867151054,
3.40183788823765));
#151869=CARTESIAN_POINT('Ctrl Pts',(-21.2358041974883,-19.4947483371046,
3.40601345242883));
#151870=CARTESIAN_POINT('Ctrl Pts',(-21.2545007467516,-19.4085663956271,
3.41039991444246));
#151871=CARTESIAN_POINT('Ctrl Pts',(-21.2687176692139,-19.3215156705805,
3.41478637645609));
#151872=CARTESIAN_POINT('Ctrl Pts',(-21.2784095170101,-19.2340996450695,
3.41917283846971));
#151873=CARTESIAN_POINT('Ctrl Pts',(-21.2881013648063,-19.1466836195585,
3.42355930048334));
#151874=CARTESIAN_POINT('Ctrl Pts',(-21.293268179777,-19.0589028772671,
3.42794576249697));
#151875=CARTESIAN_POINT('Ctrl Pts',(-21.2939275539577,-18.9712592442245,
3.43233222451059));
#151876=CARTESIAN_POINT('Ctrl Pts',(-21.2939755504833,-18.9648795739236,
3.43265151959756));
#151877=CARTESIAN_POINT('Ctrl Pts',(-21.2939996986147,-18.958499723977,
3.43297081468453));
#151878=CARTESIAN_POINT('Ctrl Pts',(-21.2939999971965,-18.9521198086916,
3.4332901097715));
#151879=CARTESIAN_POINT('',(-21.2936055506457,-18.9523823947329,3.36670986511492));
#151880=CARTESIAN_POINT('Ctrl Pts',(-17.1746506047676,-20.9818836121461,
3.08342410085255));
#151881=CARTESIAN_POINT('Ctrl Pts',(-17.6886694217464,-21.3686027203593,
3.11541445624699));
#151882=CARTESIAN_POINT('Ctrl Pts',(-19.2309396521922,-21.8303673584937,
3.1897967472019));
#151883=CARTESIAN_POINT('Ctrl Pts',(-21.0089153287167,-20.6164715882702,
3.28422525530708));
#151884=CARTESIAN_POINT('Ctrl Pts',(-21.2903730986671,-19.3569817773889,
3.34666340801782));
#151885=CARTESIAN_POINT('Ctrl Pts',(-21.2898370719784,-18.9523866753572,
3.36670962516808));
#151886=CARTESIAN_POINT('Ctrl Pts',(-21.2939999715072,-18.9523819467093,
3.36670989022851));
#151887=CARTESIAN_POINT('Ctrl Pts',(-21.2940130064034,-18.8650154810554,
3.3710315430356));
#151888=CARTESIAN_POINT('Ctrl Pts',(-21.2895493128086,-18.777713537132,
3.37535319584269));
#151889=CARTESIAN_POINT('Ctrl Pts',(-21.2806546261691,-18.690944038544,
3.37967484864978));
#151890=CARTESIAN_POINT('Ctrl Pts',(-21.2713805337795,-18.6004733587877,
3.3841808429622));
#151891=CARTESIAN_POINT('Ctrl Pts',(-21.2572890869443,-18.5105820575898,
3.38868683727461));
#151892=CARTESIAN_POINT('Ctrl Pts',(-21.2384911684206,-18.4217887333304,
3.39319283158702));
#151893=CARTESIAN_POINT('Ctrl Pts',(-21.2204017935412,-18.3363422660907,
3.39752898296562));
#151894=CARTESIAN_POINT('Ctrl Pts',(-21.1979545494933,-18.2519128648075,
3.40186513434422));
#151895=CARTESIAN_POINT('Ctrl Pts',(-21.1712990035407,-18.1689459997295,
3.40620128572282));
#151896=CARTESIAN_POINT('Ctrl Pts',(-21.1446099328527,-18.0858747870536,
3.41054289068799));
#151897=CARTESIAN_POINT('Ctrl Pts',(-21.1137021554184,-18.0042701592823,
3.41488449565315));
#151898=CARTESIAN_POINT('Ctrl Pts',(-21.078773161122,-17.9245571437388,
3.41922610061831));
#151899=CARTESIAN_POINT('Ctrl Pts',(-21.043770395337,-17.8446757709914,
3.42357687523372));
#151900=CARTESIAN_POINT('Ctrl Pts',(-21.004729634837,-17.7666943545291,
3.42792764984912));
#151901=CARTESIAN_POINT('Ctrl Pts',(-20.9618940508663,-17.6910130460174,
3.43227842446453));
#151902=CARTESIAN_POINT('Ctrl Pts',(-20.9570751477607,-17.6824990756493,
3.4327678764426));
#151903=CARTESIAN_POINT('Ctrl Pts',(-20.9522082623988,-17.6740141830165,
3.43325732842066));
#151904=CARTESIAN_POINT('Ctrl Pts',(-20.9472937739975,-17.6655589131313,
3.43374678039873));
#151905=CARTESIAN_POINT('Ctrl Pts',(-20.9052767057114,-17.5932694654538,
3.43793141479117));
#151906=CARTESIAN_POINT('Ctrl Pts',(-20.8596361007271,-17.5229061642047,
3.44211604918361));
#151907=CARTESIAN_POINT('Ctrl Pts',(-20.8105736599317,-17.4548554395525,
3.44630068357605));
#151908=CARTESIAN_POINT('Ctrl Pts',(-20.7615810534482,-17.3869015766838,
3.45047936165939));
#151909=CARTESIAN_POINT('Ctrl Pts',(-20.7091765523541,-17.3212541220958,
3.45465803974272));
#151910=CARTESIAN_POINT('Ctrl Pts',(-20.6536069384428,-17.2582735752542,
3.45883671782606));
#151911=CARTESIAN_POINT('Ctrl Pts',(-20.5970412791291,-17.1941641473621,
3.46309029571165));
#151912=CARTESIAN_POINT('Ctrl Pts',(-20.5371961639065,-17.1328185931041,
3.46734387359723));
#151913=CARTESIAN_POINT('Ctrl Pts',(-20.4743771168501,-17.074584891095,
3.47159745148282));
#151914=CARTESIAN_POINT('Ctrl Pts',(-20.4127759396134,-17.0174801630436,
3.47576856546016));
#151915=CARTESIAN_POINT('Ctrl Pts',(-20.3483154653819,-16.9633680324697,
3.4799396794375));
#151916=CARTESIAN_POINT('Ctrl Pts',(-20.2813221318919,-16.9125407039714,
3.48411079341484));
#151917=CARTESIAN_POINT('Ctrl Pts',(-20.2143512786619,-16.8617304310739,
3.4882805077346));
#151918=CARTESIAN_POINT('Ctrl Pts',(-20.1448496203253,-16.8142030489947,
3.49245022205436));
#151919=CARTESIAN_POINT('Ctrl Pts',(-20.0731762130981,-16.7702101223371,
3.49661993637412));
#151920=CARTESIAN_POINT('Ctrl Pts',(-20.0015053563183,-16.7262187611366,
3.50078950231756));
#151921=CARTESIAN_POINT('Ctrl Pts',(-19.9276632968149,-16.6857618452166,
3.504959068261));
#151922=CARTESIAN_POINT('Ctrl Pts',(-19.8520364016659,-16.6490465474635,
3.50912863420444));
#151923=CARTESIAN_POINT('Ctrl Pts',(-19.7737505581549,-16.6110403851227,
3.51344479694408));
#151924=CARTESIAN_POINT('Ctrl Pts',(-19.6935525085947,-16.5770440773061,
3.51776095968372));
#151925=CARTESIAN_POINT('Ctrl Pts',(-19.6118947218444,-16.5472337208457,
3.52207712242337));
#151926=CARTESIAN_POINT('Ctrl Pts',(-19.5328969289333,-16.5183944336205,
3.52625268661444));
#151927=CARTESIAN_POINT('Ctrl Pts',(-19.4525335041398,-16.4934726654687,
3.53042825080552));
#151928=CARTESIAN_POINT('Ctrl Pts',(-19.3712290384547,-16.4725768508482,
3.5346038149966));
#151929=CARTESIAN_POINT('Ctrl Pts',(-19.2858180774516,-16.4506256382961,
3.53899027701053));
#151930=CARTESIAN_POINT('Ctrl Pts',(-19.1993690855434,-16.4331178853207,
3.54337673902446));
#151931=CARTESIAN_POINT('Ctrl Pts',(-19.112383460267,-16.4201180997139,
3.54776320103838));
#151932=CARTESIAN_POINT('Ctrl Pts',(-19.0253978349906,-16.4071183141071,
3.55214966305231));
#151933=CARTESIAN_POINT('Ctrl Pts',(-18.937876161197,-16.3986264761921,
3.55653612506623));
#151934=CARTESIAN_POINT('Ctrl Pts',(-18.8503205710795,-16.3946440363642,
3.56092258708016));
#151935=CARTESIAN_POINT('Ctrl Pts',(-18.7667935434872,-16.3908448344978,
3.56510722147276));
#151936=CARTESIAN_POINT('Ctrl Pts',(-18.6829247485327,-16.391135040087,
3.56929185586536));
#151937=CARTESIAN_POINT('Ctrl Pts',(-18.5991482896987,-16.3955542219267,
3.57347649025797));
#151938=CARTESIAN_POINT('Ctrl Pts',(-18.5154910762845,-16.3999671136081,
3.57765516834146));
#151939=CARTESIAN_POINT('Ctrl Pts',(-18.4319263933964,-16.4084972837709,
3.58183384642495));
#151940=CARTESIAN_POINT('Ctrl Pts',(-18.3488909423387,-16.4211323595045,
3.58601252450844));
#151941=CARTESIAN_POINT('Ctrl Pts',(-18.2643671404859,-16.4339939098917,
3.59026610239399));
#151942=CARTESIAN_POINT('Ctrl Pts',(-18.1803922116832,-16.4511089960901,
3.59451968027954));
#151943=CARTESIAN_POINT('Ctrl Pts',(-18.0974241252638,-16.4724090749271,
3.59877325816509));
#151944=CARTESIAN_POINT('Ctrl Pts',(-18.0160645371101,-16.4932962101692,
3.60294437214256));
#151945=CARTESIAN_POINT('Ctrl Pts',(-17.9356735666137,-16.5182073979463,
3.60711548612003));
#151946=CARTESIAN_POINT('Ctrl Pts',(-17.8566736061544,-16.5470263205885,
3.61128660009751));
#151947=CARTESIAN_POINT('Ctrl Pts',(-17.7777001548948,-16.575835572763,
3.6154563144174));
#151948=CARTESIAN_POINT('Ctrl Pts',(-17.7001172184807,-16.6085497980589,
3.6196260287373));
#151949=CARTESIAN_POINT('Ctrl Pts',(-17.6243306732527,-16.6450032541687,
3.6237957430572));
#151950=CARTESIAN_POINT('Ctrl Pts',(-17.5485468248353,-16.6814554131081,
3.62796530900076));
#151951=CARTESIAN_POINT('Ctrl Pts',(-17.4745596547067,-16.7216463381322,
3.63213487494432));
#151952=CARTESIAN_POINT('Ctrl Pts',(-17.4027524956497,-16.7653632944266,
3.63630444088788));
#151953=CARTESIAN_POINT('Ctrl Pts',(-17.3284206854457,-16.8106172849846,
3.64062060362735));
#151954=CARTESIAN_POINT('Ctrl Pts',(-17.2564254874565,-16.8596495964178,
3.64493676636683));
#151955=CARTESIAN_POINT('Ctrl Pts',(-17.1871598840616,-16.9121750918955,
3.64925292910631));
#151956=CARTESIAN_POINT('Ctrl Pts',(-17.1201506004283,-16.9629895748702,
3.65342849329749));
#151957=CARTESIAN_POINT('Ctrl Pts',(-17.0556961397385,-17.0170728169151,
3.65760405748868));
#151958=CARTESIAN_POINT('Ctrl Pts',(-16.9941175012612,-17.0741264977155,
3.66177962167986));
#151959=CARTESIAN_POINT('Ctrl Pts',(-16.92942867212,-17.1340618243228,3.66616608369348));
#151960=CARTESIAN_POINT('Ctrl Pts',(-16.8679142228486,-17.1972751310411,
3.67055254570711));
#151961=CARTESIAN_POINT('Ctrl Pts',(-16.8098997912682,-17.263379738734,
3.67493900772073));
#151962=CARTESIAN_POINT('Ctrl Pts',(-16.7518853596878,-17.3294843464269,
3.67932546973435));
#151963=CARTESIAN_POINT('Ctrl Pts',(-16.6973712458221,-17.3984797526768,
3.68371193174797));
#151964=CARTESIAN_POINT('Ctrl Pts',(-16.6466304638567,-17.4699445288448,
3.6880983937616));
#151965=CARTESIAN_POINT('Ctrl Pts',(-16.5982243404926,-17.538121104715,
3.69228302815506));
#151966=CARTESIAN_POINT('Ctrl Pts',(-16.5530717694469,-17.6087985715454,
3.69646766254852));
#151967=CARTESIAN_POINT('Ctrl Pts',(-16.5114409937959,-17.6816333348434,
3.70065229694198));
#151968=CARTESIAN_POINT('Ctrl Pts',(-16.4698694744012,-17.754364426871,
3.70483097502633));
#151969=CARTESIAN_POINT('Ctrl Pts',(-16.4318100196567,-17.8292463201214,
3.70900965311068));
#151970=CARTESIAN_POINT('Ctrl Pts',(-16.3974886040357,-17.905905120685,
3.71318833119504));
#151971=CARTESIAN_POINT('Ctrl Pts',(-16.3625520017104,-17.9839379751455,
3.71744190908037));
#151972=CARTESIAN_POINT('Ctrl Pts',(-16.3314890444374,-18.0638116724909,
3.7216954869657));
#151973=CARTESIAN_POINT('Ctrl Pts',(-16.3044899883695,-18.1451040318682,
3.72594906485104));
#151974=CARTESIAN_POINT('Ctrl Pts',(-16.2780143616845,-18.2248203802401,
3.73012017882942));
#151975=CARTESIAN_POINT('Ctrl Pts',(-16.2554466207297,-18.3059004177641,
3.73429129280781));
#151976=CARTESIAN_POINT('Ctrl Pts',(-16.2369175937363,-18.3879260187454,
3.73846240678619));
#151977=CARTESIAN_POINT('Ctrl Pts',(-16.2183947843369,-18.4699240952442,
3.742632121107));
#151978=CARTESIAN_POINT('Ctrl Pts',(-16.2039080986716,-18.5528666566984,
3.74680183542782));
#151979=CARTESIAN_POINT('Ctrl Pts',(-16.1935378668542,-18.6363227121694,
3.75097154974863));
#151980=CARTESIAN_POINT('Ctrl Pts',(-16.1831680040541,-18.7197757979158,
3.75514111569312));
#151981=CARTESIAN_POINT('Ctrl Pts',(-16.1769143597415,-18.8037418847219,
3.75931068163761));
#151982=CARTESIAN_POINT('Ctrl Pts',(-16.174805548368,-18.8877835010606,
3.76348024758209));
#151983=CARTESIAN_POINT('Ctrl Pts',(-16.1726225937887,-18.9747799169337,
3.7677964103205));
#151984=CARTESIAN_POINT('Ctrl Pts',(-16.1748813730051,-19.0618567451386,
3.77211257305891));
#151985=CARTESIAN_POINT('Ctrl Pts',(-16.1815548449752,-19.1485292105273,
3.77642873579733));
#151986=CARTESIAN_POINT('Ctrl Pts',(-16.1880109292993,-19.2323783294909,
3.78060429998945));
#151987=CARTESIAN_POINT('Ctrl Pts',(-16.1985983999138,-19.3158485639561,
3.78477986418157));
#151988=CARTESIAN_POINT('Ctrl Pts',(-16.2132401674605,-19.3985085292081,
3.78895542837369));
#151989=CARTESIAN_POINT('Ctrl Pts',(-16.2286214558734,-19.485343452771,
3.79334189038525));
#151990=CARTESIAN_POINT('Ctrl Pts',(-16.2484772384201,-19.5712835336828,
3.7977283523968));
#151991=CARTESIAN_POINT('Ctrl Pts',(-16.272658640717,-19.6558456599874,
3.80211481440836));
#151992=CARTESIAN_POINT('Ctrl Pts',(-16.2968400430139,-19.7404077862919,
3.80650127641991));
#151993=CARTESIAN_POINT('Ctrl Pts',(-16.3253468050044,-19.8235914337677,
3.81088773843147));
#151994=CARTESIAN_POINT('Ctrl Pts',(-16.3579723492966,-19.9049389293615,
3.81527420044303));
#151995=CARTESIAN_POINT('Ctrl Pts',(-16.3890953380463,-19.9825400007035,
3.81945864581547));
#151996=CARTESIAN_POINT('Ctrl Pts',(-16.4240819170418,-20.0587591592382,
3.82364309118791));
#151997=CARTESIAN_POINT('Ctrl Pts',(-16.4627883931821,-20.1331849292367,
3.82782753656036));
#151998=CARTESIAN_POINT('Ctrl Pts',(-16.5014420743038,-20.2075091836669,
3.83200627441578));
#151999=CARTESIAN_POINT('Ctrl Pts',(-16.5438053667044,-20.2800445024167,
3.8361850122712));
#152000=CARTESIAN_POINT('Ctrl Pts',(-16.5896861940544,-20.3503984774131,
3.84036375012661));
#152001=CARTESIAN_POINT('Ctrl Pts',(-16.6355124170914,-20.4206687217817,
3.84453751472581));
#152002=CARTESIAN_POINT('Ctrl Pts',(-16.6848476028014,-20.4887624000661,
3.84871127932502));
#152003=CARTESIAN_POINT('Ctrl Pts',(-16.7374540925185,-20.5543122165542,
3.85288504392422));
#152004=CARTESIAN_POINT('Ctrl Pts',(-16.7900243343999,-20.6198168667711,
3.85705593264376));
#152005=CARTESIAN_POINT('Ctrl Pts',(-16.8458611159082,-20.6827807792016,
3.86122682136329));
#152006=CARTESIAN_POINT('Ctrl Pts',(-16.9046845019153,-20.7428670549394,
3.86539771008283));
#152007=CARTESIAN_POINT('Ctrl Pts',(-16.9634896683972,-20.8029347199936,
3.86956730694181));
#152008=CARTESIAN_POINT('Ctrl Pts',(-17.0252792822203,-20.8601261886928,
3.87373690380078));
#152009=CARTESIAN_POINT('Ctrl Pts',(-17.0897351511593,-20.9141399305011,
3.87790650065976));
#152010=CARTESIAN_POINT('Ctrl Pts',(-17.117493244807,-20.9374010939616,
3.87970214878288));
#152011=CARTESIAN_POINT('Ctrl Pts',(-17.1457453692821,-20.9600733822345,
3.88149779690601));
#152012=CARTESIAN_POINT('Ctrl Pts',(-17.1744641402401,-20.9821349467765,
3.88329344502913));
#152013=CARTESIAN_POINT('Origin',(-18.734,-18.952,-1.76670989022851));
#152014=CARTESIAN_POINT('',(-17.1762220465436,-20.9798104602808,4.7499734600764));
#152015=CARTESIAN_POINT('',(-17.1735447294248,-20.9833104140832,4.68319929961578));
#152016=CARTESIAN_POINT('',(-17.1744641402401,-20.9821349467765,-1.76670989022851));
#152017=CARTESIAN_POINT('',(-21.2939990418858,-18.954214846262,4.23329008725046));
#152018=CARTESIAN_POINT('Ctrl Pts',(-21.2923872764654,-18.9542129983989,
4.2332901097715));
#152019=CARTESIAN_POINT('Ctrl Pts',(-21.2874612769029,-18.3551143891762,
4.26304769694121));
#152020=CARTESIAN_POINT('Ctrl Pts',(-20.7784813193811,-16.8950156348367,
4.3351972196714));
#152021=CARTESIAN_POINT('Ctrl Pts',(-18.3440265497682,-15.950131970293,
4.44973867796207));
#152022=CARTESIAN_POINT('Ctrl Pts',(-15.9988188107527,-17.6550517274584,
4.5769144846435));
#152023=CARTESIAN_POINT('Ctrl Pts',(-16.1279940901006,-19.9330437902871,
4.67699274534828));
#152024=CARTESIAN_POINT('Ctrl Pts',(-16.9304195254802,-20.7936897644837,
4.73467907049259));
#152025=CARTESIAN_POINT('Ctrl Pts',(-17.1762220465438,-20.9798104602809,
4.74997346007641));
#152026=CARTESIAN_POINT('Ctrl Pts',(-17.1744641402401,-20.9821349467765,
3.94993168147533));
#152027=CARTESIAN_POINT('Ctrl Pts',(-17.2408641401809,-21.033142975164,
3.95411195179436));
#152028=CARTESIAN_POINT('Ctrl Pts',(-17.309875151081,-21.0809712817735,
3.95829222211338));
#152029=CARTESIAN_POINT('Ctrl Pts',(-17.381159192972,-21.1253434498118,
3.96247249243241));
#152030=CARTESIAN_POINT('Ctrl Pts',(-17.4523585054123,-21.1696628763203,
3.9666477940095));
#152031=CARTESIAN_POINT('Ctrl Pts',(-17.5258250930132,-21.2105340841302,
3.9708230955866));
#152032=CARTESIAN_POINT('Ctrl Pts',(-17.6011898523106,-21.2477223632861,
3.9749983971637));
#152033=CARTESIAN_POINT('Ctrl Pts',(-17.6764914717807,-21.2848794864807,
3.97917020071568));
#152034=CARTESIAN_POINT('Ctrl Pts',(-17.7536876917253,-21.3183596094561,
3.98334200426766));
#152035=CARTESIAN_POINT('Ctrl Pts',(-17.8323836483386,-21.3479732791533,
3.98751380781964));
#152036=CARTESIAN_POINT('Ctrl Pts',(-17.911045866078,-21.3775742527489,
3.9916838228178));
#152037=CARTESIAN_POINT('Ctrl Pts',(-17.9912061137305,-21.4033119028792,
3.99585383781596));
#152038=CARTESIAN_POINT('Ctrl Pts',(-18.0724494594724,-21.4250448605571,
4.00002385281411));
#152039=CARTESIAN_POINT('Ctrl Pts',(-18.1536823453448,-21.4467750201731,
4.00419333093369));
#152040=CARTESIAN_POINT('Ctrl Pts',(-18.2359976077846,-21.4645013933133,
4.00836280905326));
#152041=CARTESIAN_POINT('Ctrl Pts',(-18.3189663842219,-21.4781328345465,
4.01253228717283));
#152042=CARTESIAN_POINT('Ctrl Pts',(-18.401949366933,-21.4917666098143,
4.01670247920854));
#152043=CARTESIAN_POINT('Ctrl Pts',(-18.4855856317187,-21.5013039876535,
4.02087267124424));
#152044=CARTESIAN_POINT('Ctrl Pts',(-18.5694387459347,-21.5067053829474,
4.02504286327995));
#152045=CARTESIAN_POINT('Ctrl Pts',(-18.6533842887412,-21.5121127320256,
4.02921765198419));
#152046=CARTESIAN_POINT('Ctrl Pts',(-18.7375466982335,-21.5133749703138,
4.03339244068844));
#152047=CARTESIAN_POINT('Ctrl Pts',(-18.8214876223156,-21.51050462496,4.03756722939268));
#152048=CARTESIAN_POINT('Ctrl Pts',(-18.9054811188542,-21.5076324819001,
4.04174463277981));
#152049=CARTESIAN_POINT('Ctrl Pts',(-18.9892523957867,-21.5006226419762,
4.04592203616693));
#152050=CARTESIAN_POINT('Ctrl Pts',(-19.0723687017023,-21.4895394818029,
4.05009943955406));
#152051=CARTESIAN_POINT('Ctrl Pts',(-19.155621576138,-21.4784381108733,
4.05428370683862));
#152052=CARTESIAN_POINT('Ctrl Pts',(-19.2382168797992,-21.46325014424,4.05846797412318));
#152053=CARTESIAN_POINT('Ctrl Pts',(-19.3197329580376,-21.4440908695047,
4.06265224140774));
#152054=CARTESIAN_POINT('Ctrl Pts',(-19.3558324065943,-21.4356061721586,
4.06450524691108));
#152055=CARTESIAN_POINT('Ctrl Pts',(-19.3917204150806,-21.4263432877792,
4.06635825241442));
#152056=CARTESIAN_POINT('Ctrl Pts',(-19.4273615317731,-21.4163152773656,
4.06821125791777));
#152057=CARTESIAN_POINT('Ctrl Pts',(-19.5078497129731,-21.3936690643915,
4.07239589231081));
#152058=CARTESIAN_POINT('Ctrl Pts',(-19.5873770243866,-21.3670332665356,
4.07658052670385));
#152059=CARTESIAN_POINT('Ctrl Pts',(-19.6655189252301,-21.336506760724,
4.08076516109689));
#152060=CARTESIAN_POINT('Ctrl Pts',(-19.7435496007498,-21.3060237056149,
4.08494383918084));
#152061=CARTESIAN_POINT('Ctrl Pts',(-19.820198357802,-21.2716611086064,
4.08912251726478));
#152062=CARTESIAN_POINT('Ctrl Pts',(-19.8950545149195,-21.2335679725542,
4.09330119534872));
#152063=CARTESIAN_POINT('Ctrl Pts',(-19.9712524148552,-21.1947920444153,
4.09755477323416));
#152064=CARTESIAN_POINT('Ctrl Pts',(-20.0455923539257,-21.152150652534,
4.10180835111959));
#152065=CARTESIAN_POINT('Ctrl Pts',(-20.1176611149874,-21.1058528080795,
4.10606192900503));
#152066=CARTESIAN_POINT('Ctrl Pts',(-20.1883326824852,-21.0604525376826,
4.11023304298298));
#152067=CARTESIAN_POINT('Ctrl Pts',(-20.2568199436825,-21.0115365845692,
4.11440415696092));
#152068=CARTESIAN_POINT('Ctrl Pts',(-20.3227584711504,-20.9593481313285,
4.11857527093886));
#152069=CARTESIAN_POINT('Ctrl Pts',(-20.3886748723086,-20.9071771904272,
4.12274498525923));
#152070=CARTESIAN_POINT('Ctrl Pts',(-20.4520438778608,-20.8517362155432,
4.1269146995796));
#152071=CARTESIAN_POINT('Ctrl Pts',(-20.512532273786,-20.7933101181229,
4.13108441389997));
#152072=CARTESIAN_POINT('Ctrl Pts',(-20.5730185172742,-20.7348860997541,
4.13525397984399));
#152073=CARTESIAN_POINT('Ctrl Pts',(-20.6306240246485,-20.6734774902644,
4.13942354578802));
#152074=CARTESIAN_POINT('Ctrl Pts',(-20.6850517529254,-20.6094067266084,
4.14359311173205));
#152075=CARTESIAN_POINT('Ctrl Pts',(-20.7413930929849,-20.5430833139418,
4.14790927447098));
#152076=CARTESIAN_POINT('Ctrl Pts',(-20.7943286933419,-20.47390746331,4.1522254372099));
#152077=CARTESIAN_POINT('Ctrl Pts',(-20.8435751066795,-20.4022733774286,
4.15654159994883));
#152078=CARTESIAN_POINT('Ctrl Pts',(-20.8912173232822,-20.3329727643606,
4.16071716414051));
#152079=CARTESIAN_POINT('Ctrl Pts',(-20.9354068051746,-20.261372036261,
4.16489272833218));
#152080=CARTESIAN_POINT('Ctrl Pts',(-20.9759325838393,-20.1878552866415,
4.16906829252385));
#152081=CARTESIAN_POINT('Ctrl Pts',(-21.0185052232437,-20.1106253807678,
4.17345475453641));
#152082=CARTESIAN_POINT('Ctrl Pts',(-21.0570340704736,-20.0312813353546,
4.17784121654897));
#152083=CARTESIAN_POINT('Ctrl Pts',(-21.0913315250628,-19.9502925828359,
4.18222767856152));
#152084=CARTESIAN_POINT('Ctrl Pts',(-21.125628979652,-19.8693038303172,
4.18661414057408));
#152085=CARTESIAN_POINT('Ctrl Pts',(-21.1556949146933,-19.7866709419479,
4.19100060258664));
#152086=CARTESIAN_POINT('Ctrl Pts',(-21.1814026084241,-19.7028797988221,
4.19538706459919));
#152087=CARTESIAN_POINT('Ctrl Pts',(-21.2113658472603,-19.6052182170354,
4.20049964335886));
#152088=CARTESIAN_POINT('Ctrl Pts',(-21.235501378659,-19.5056900725396,
4.20561222211854));
#152089=CARTESIAN_POINT('Ctrl Pts',(-21.253614967081,-19.4049242957285,
4.2107248008782));
#152090=CARTESIAN_POINT('Ctrl Pts',(-21.2714816855059,-19.3055318551366,
4.21576770033001));
#152091=CARTESIAN_POINT('Ctrl Pts',(-21.283489454374,-19.2049352741372,
4.22081059978182));
#152092=CARTESIAN_POINT('Ctrl Pts',(-21.2894978367355,-19.1037590407195,
4.22585349923363));
#152093=CARTESIAN_POINT('Ctrl Pts',(-21.2924512874039,-19.0540253526423,
4.22833236190591));
#152094=CARTESIAN_POINT('Ctrl Pts',(-21.2939558375883,-19.0041519285412,
4.23081122457819));
#152095=CARTESIAN_POINT('Ctrl Pts',(-21.2939990418858,-18.954214846262,
4.23329008725046));
#152096=CARTESIAN_POINT('',(-21.2939989159607,-18.9496440968075,4.16670989022851));
#152097=CARTESIAN_POINT('Ctrl Pts',(-17.1744641402401,-20.9821349467765,
3.88329344502913));
#152098=CARTESIAN_POINT('Ctrl Pts',(-17.2411550934206,-21.033366483464,
3.88746331306014));
#152099=CARTESIAN_POINT('Ctrl Pts',(-17.3103644275838,-21.0813016244736,
3.89163318109116));
#152100=CARTESIAN_POINT('Ctrl Pts',(-17.381727523325,-21.1256971152457,
3.89580304912217));
#152101=CARTESIAN_POINT('Ctrl Pts',(-17.4531658161136,-21.1701393866372,
3.89997731104559));
#152102=CARTESIAN_POINT('Ctrl Pts',(-17.5267620105389,-21.2110343169657,
3.904151572969));
#152103=CARTESIAN_POINT('Ctrl Pts',(-17.6021247933809,-21.2481834675481,
3.90832583489242));
#152104=CARTESIAN_POINT('Ctrl Pts',(-17.6775291402241,-21.2853531065901,
3.91250239900029));
#152105=CARTESIAN_POINT('Ctrl Pts',(-17.7547015931812,-21.3187726695461,
3.91667896310817));
#152106=CARTESIAN_POINT('Ctrl Pts',(-17.8332308997776,-21.3482919329841,
3.92085552721604));
#152107=CARTESIAN_POINT('Ctrl Pts',(-17.9118958332387,-21.3778621787281,
3.92503930460925));
#152108=CARTESIAN_POINT('Ctrl Pts',(-17.9919218622461,-21.4035185308936,
3.92922308200245));
#152109=CARTESIAN_POINT('Ctrl Pts',(-18.0728828643972,-21.4251607576161,
3.93340685939566));
#152110=CARTESIAN_POINT('Ctrl Pts',(-18.1312147045753,-21.440753831772,
3.93642124197193));
#152111=CARTESIAN_POINT('Ctrl Pts',(-18.1900316123881,-21.4542641966054,
3.9394356245482));
#152112=CARTESIAN_POINT('Ctrl Pts',(-18.249172131343,-21.4656710082613,
3.94245000712447));
#152113=CARTESIAN_POINT('Ctrl Pts',(-18.3312723437007,-21.4815062034173,
3.94663464151747));
#152114=CARTESIAN_POINT('Ctrl Pts',(-18.4143019582716,-21.4933443659487,
3.95081927591047));
#152115=CARTESIAN_POINT('Ctrl Pts',(-18.4978371529755,-21.5010835823263,
3.95500391030347));
#152116=CARTESIAN_POINT('Ctrl Pts',(-18.5812534456693,-21.5088117828872,
3.95918258838737));
#152117=CARTESIAN_POINT('Ctrl Pts',(-18.6651734349298,-21.5124525840588,
3.96336126647127));
#152118=CARTESIAN_POINT('Ctrl Pts',(-18.7491632186831,-21.511955092731,
3.96753994455517));
#152119=CARTESIAN_POINT('Ctrl Pts',(-18.8346584589489,-21.5114486842286,
3.97179352244062));
#152120=CARTESIAN_POINT('Ctrl Pts',(-18.9202255470372,-21.5066540748902,
3.97604710032607));
#152121=CARTESIAN_POINT('Ctrl Pts',(-19.0054014154827,-21.4975728769128,
3.98030067821151));
#152122=CARTESIAN_POINT('Ctrl Pts',(-19.0889259835101,-21.4886677356788,
3.98447179218942));
#152123=CARTESIAN_POINT('Ctrl Pts',(-19.1720738871336,-21.4756407813847,
3.98864290616732));
#152124=CARTESIAN_POINT('Ctrl Pts',(-19.254410355074,-21.4585460423323,
3.99281402014522));
#152125=CARTESIAN_POINT('Ctrl Pts',(-19.3367191942173,-21.4414570395848,
3.99698373446554));
#152126=CARTESIAN_POINT('Ctrl Pts',(-19.4182166883876,-21.4203030563999,
4.00115344878586));
#152127=CARTESIAN_POINT('Ctrl Pts',(-19.4984772632651,-21.3951894142597,
4.00532316310618));
#152128=CARTESIAN_POINT('Ctrl Pts',(-19.5787349821269,-21.3700766657707,
4.00949272905017));
#152129=CARTESIAN_POINT('Ctrl Pts',(-19.6577554304214,-21.3410046766651,
4.01366229499415));
#152130=CARTESIAN_POINT('Ctrl Pts',(-19.7351285466055,-21.3081285264543,
4.01783186093814));
#152131=CARTESIAN_POINT('Ctrl Pts',(-19.8152220061068,-21.2740964913582,
4.02214802367712));
#152132=CARTESIAN_POINT('Ctrl Pts',(-19.8935496523619,-21.235988015554,
4.0264641864161));
#152133=CARTESIAN_POINT('Ctrl Pts',(-19.9696814081004,-21.1940284248142,
4.03078034915508));
#152134=CARTESIAN_POINT('Ctrl Pts',(-20.0433331799013,-21.1534356633306,
4.0349559133467));
#152135=CARTESIAN_POINT('Ctrl Pts',(-20.1149295504521,-21.1092391216319,
4.03913147753832));
#152136=CARTESIAN_POINT('Ctrl Pts',(-20.1841097633276,-21.0616875774157,
4.04330704172994));
#152137=CARTESIAN_POINT('Ctrl Pts',(-20.2567841042981,-21.0117343177421,
4.0476935037426));
#152138=CARTESIAN_POINT('Ctrl Pts',(-20.3267913293727,-20.9580785813376,
4.05207996575526));
#152139=CARTESIAN_POINT('Ctrl Pts',(-20.3937533178436,-20.9010559057932,
4.05646642776792));
#152140=CARTESIAN_POINT('Ctrl Pts',(-20.4607153063145,-20.8440332302488,
4.06085288978057));
#152141=CARTESIAN_POINT('Ctrl Pts',(-20.5246316886731,-20.7836440693277,
4.06523935179323));
#152142=CARTESIAN_POINT('Ctrl Pts',(-20.5851713910718,-20.7202659530956,
4.06962581380589));
#152143=CARTESIAN_POINT('Ctrl Pts',(-20.6421808499863,-20.66058359639,4.07375648865202));
#152144=CARTESIAN_POINT('Ctrl Pts',(-20.6964202744403,-20.5980163329693,
4.07788716349815));
#152145=CARTESIAN_POINT('Ctrl Pts',(-20.747578131795,-20.5328551822216,
4.08201783834428));
#152146=CARTESIAN_POINT('Ctrl Pts',(-20.7986699217385,-20.467778183328,
4.08614317866296));
#152147=CARTESIAN_POINT('Ctrl Pts',(-20.8466877493678,-20.4001143092104,
4.09026851898165));
#152148=CARTESIAN_POINT('Ctrl Pts',(-20.8913569516645,-20.3301911997632,
4.09439385930034));
#152149=CARTESIAN_POINT('Ctrl Pts',(-20.9359826817961,-20.2603361396387,
4.09851518482882));
#152150=CARTESIAN_POINT('Ctrl Pts',(-20.9772659998208,-20.188226602647,
4.10263651035731));
#152151=CARTESIAN_POINT('Ctrl Pts',(-21.0149735460513,-20.1142218730579,
4.10675783588579));
#152152=CARTESIAN_POINT('Ctrl Pts',(-21.0526563884391,-20.0402656271644,
4.11087646135587));
#152153=CARTESIAN_POINT('Ctrl Pts',(-21.0867678956212,-19.9644170734847,
4.11499508682595));
#152154=CARTESIAN_POINT('Ctrl Pts',(-21.1171197545789,-19.8870616211436,
4.11911371229603));
#152155=CARTESIAN_POINT('Ctrl Pts',(-21.1474714047475,-19.8097067009274,
4.12323230943426));
#152156=CARTESIAN_POINT('Ctrl Pts',(-21.1740632676919,-19.730845335542,
4.12735090657249));
#152157=CARTESIAN_POINT('Ctrl Pts',(-21.1967549321189,-19.6508834983916,
4.13146950371072));
#152158=CARTESIAN_POINT('Ctrl Pts',(-21.2194452848828,-19.5709262833344,
4.13558786277862));
#152159=CARTESIAN_POINT('Ctrl Pts',(-21.238235765403,-19.4898691801177,
4.13970622184653));
#152160=CARTESIAN_POINT('Ctrl Pts',(-21.2530362470693,-19.4081319830388,
4.14382458091443));
#152161=CARTESIAN_POINT('Ctrl Pts',(-21.2678499327185,-19.3263218655936,
4.14794661410211));
#152162=CARTESIAN_POINT('Ctrl Pts',(-21.2786664327327,-19.2438309098082,
4.15206864728979));
#152163=CARTESIAN_POINT('Ctrl Pts',(-21.2854471635996,-19.1610869947161,
4.15619068047747));
#152164=CARTESIAN_POINT('Ctrl Pts',(-21.2912151852698,-19.090700969273,
4.15969708372782));
#152165=CARTESIAN_POINT('Ctrl Pts',(-21.2940637843831,-19.0201321760509,
4.16320348697816));
#152166=CARTESIAN_POINT('Ctrl Pts',(-21.2939989159607,-18.9496440968075,
4.16670989022851));
#152167=CARTESIAN_POINT('Ctrl Pts',(-21.2939116738757,-18.9496434105868,
4.1667099283594));
#152168=CARTESIAN_POINT('Ctrl Pts',(-21.2957663705073,-18.7480072535544,
4.17674049240205));
#152169=CARTESIAN_POINT('Ctrl Pts',(-21.1817725642886,-17.6962740222633,
4.22916299200517));
#152170=CARTESIAN_POINT('Ctrl Pts',(-19.7309870059684,-16.0937999128286,
4.32397742716877));
#152171=CARTESIAN_POINT('Ctrl Pts',(-16.8703562036358,-16.5666022074633,
4.4511532338502));
#152172=CARTESIAN_POINT('Ctrl Pts',(-15.7867861847936,-19.0722717083388,
4.57089385799921));
#152173=CARTESIAN_POINT('Ctrl Pts',(-16.6213792802803,-20.5504282248243,
4.64824254658773));
#152174=CARTESIAN_POINT('Ctrl Pts',(-17.1735447294247,-20.9833104140831,
4.68319929961578));
#152175=CARTESIAN_POINT('Origin',(-18.734,-18.952,-1.76670989022851));
#152176=CARTESIAN_POINT('',(-17.1744641402401,-20.9821349467765,5.54983330998614));
#152177=CARTESIAN_POINT('',(-17.1744641402401,-20.9821349467765,5.48336964453106));
#152178=CARTESIAN_POINT('',(-17.1744641402401,-20.9821349467765,-1.76670989022851));
#152179=CARTESIAN_POINT('',(-21.2938494922829,-18.9508032548851,5.03329016024732));
#152180=CARTESIAN_POINT('Ctrl Pts',(-21.2939997202205,-18.9508031412445,
5.03329016239894));
#152181=CARTESIAN_POINT('Ctrl Pts',(-21.2939564765218,-18.8583078019835,
5.03786858507833));
#152182=CARTESIAN_POINT('Ctrl Pts',(-21.2888961385929,-18.7659792628466,
5.04244700775773));
#152183=CARTESIAN_POINT('Ctrl Pts',(-21.2788976615006,-18.6743385289801,
5.04702543043713));
#152184=CARTESIAN_POINT('Ctrl Pts',(-21.2688681118673,-18.5824130006966,
5.05161808160601));
#152185=CARTESIAN_POINT('Ctrl Pts',(-21.2538698091559,-18.4911798450256,
5.05621073277489));
#152186=CARTESIAN_POINT('Ctrl Pts',(-21.2340326305246,-18.40114897993,5.06080338394377));
#152187=CARTESIAN_POINT('Ctrl Pts',(-21.2141037578095,-18.3107019620212,
5.06541726388461));
#152188=CARTESIAN_POINT('Ctrl Pts',(-21.1892913049386,-18.2214686542029,
5.07003114382545));
#152189=CARTESIAN_POINT('Ctrl Pts',(-21.1597755903596,-18.1339457321084,
5.0746450237663));
#152190=CARTESIAN_POINT('Ctrl Pts',(-21.1363775884172,-18.0645636578345,
5.07830258630061));
#152191=CARTESIAN_POINT('Ctrl Pts',(-21.1100249393917,-17.9962560714796,
5.08196014883493));
#152192=CARTESIAN_POINT('Ctrl Pts',(-21.0808281256644,-17.9292596866307,
5.08561771136924));
#152193=CARTESIAN_POINT('Ctrl Pts',(-21.0474239145964,-17.8526088095457,
5.08980234576229));
#152194=CARTESIAN_POINT('Ctrl Pts',(-21.0101982941979,-17.7774535557438,
5.09398698015533));
#152195=CARTESIAN_POINT('Ctrl Pts',(-20.9693070771845,-17.7042010295369,
5.09817161454838));
#152196=CARTESIAN_POINT('Ctrl Pts',(-20.9284740637572,-17.6310527692342,
5.10235029263232));
#152197=CARTESIAN_POINT('Ctrl Pts',(-20.8839860396696,-17.5598022552459,
5.10652897071627));
#152198=CARTESIAN_POINT('Ctrl Pts',(-20.8360465870686,-17.4908360304904,
5.11070764880022));
#152199=CARTESIAN_POINT('Ctrl Pts',(-20.7872478542333,-17.4206336357213,
5.11496122668565));
#152200=CARTESIAN_POINT('Ctrl Pts',(-20.7348729347517,-17.352798669429,
5.11921480457109));
#152201=CARTESIAN_POINT('Ctrl Pts',(-20.6791852047646,-17.2877120083456,
5.12346838245653));
#152202=CARTESIAN_POINT('Ctrl Pts',(-20.6245770900889,-17.2238871791935,
5.12763949643448));
#152203=CARTESIAN_POINT('Ctrl Pts',(-20.5667837820755,-17.1627054093254,
5.13181061041243));
#152204=CARTESIAN_POINT('Ctrl Pts',(-20.5060958601737,-17.1044945839443,
5.13598172439038));
#152205=CARTESIAN_POINT('Ctrl Pts',(-20.4454283026902,-17.0463032917677,
5.14015143871076));
#152206=CARTESIAN_POINT('Ctrl Pts',(-20.3818683920876,-16.9910812823424,
5.14432115303113));
#152207=CARTESIAN_POINT('Ctrl Pts',(-20.3157437934271,-16.9391198316952,
5.1484908673515));
#152208=CARTESIAN_POINT('Ctrl Pts',(-20.2496215477636,-16.8871602300594,
5.15266043329554));
#152209=CARTESIAN_POINT('Ctrl Pts',(-20.1809351577375,-16.8384612400848,
5.15682999923958));
#152210=CARTESIAN_POINT('Ctrl Pts',(-20.1100445342429,-16.7932731901002,
5.16099956518362));
#152211=CARTESIAN_POINT('Ctrl Pts',(-20.0366614838791,-16.7464963840235,
5.16531572792255));
#152212=CARTESIAN_POINT('Ctrl Pts',(-19.9609167591474,-16.703482284346,
5.16963189066146));
#152213=CARTESIAN_POINT('Ctrl Pts',(-19.8832395142303,-16.6644579700185,
5.17394805340038));
#152214=CARTESIAN_POINT('Ctrl Pts',(-19.8080925973962,-16.6267048686257,
5.17812361759207));
#152215=CARTESIAN_POINT('Ctrl Pts',(-19.731137580502,-16.5926857570977,
5.18229918178375));
#152216=CARTESIAN_POINT('Ctrl Pts',(-19.6527837251095,-16.5625572895602,
5.18647474597543));
#152217=CARTESIAN_POINT('Ctrl Pts',(-19.5704724027498,-16.530907104751,
5.19086120798797));
#152218=CARTESIAN_POINT('Ctrl Pts',(-19.4866177726054,-16.5035511069691,
5.19524767000051));
#152219=CARTESIAN_POINT('Ctrl Pts',(-19.4017104542219,-16.4806111699446,
5.19963413201305));
#152220=CARTESIAN_POINT('Ctrl Pts',(-19.3168031358384,-16.45767123292,5.20402059402559));
#152221=CARTESIAN_POINT('Ctrl Pts',(-19.2308437124363,-16.439147404523,
5.20840705603813));
#152222=CARTESIAN_POINT('Ctrl Pts',(-19.1443308019265,-16.4250990060965,
5.21279351805067));
#152223=CARTESIAN_POINT('Ctrl Pts',(-19.0617984786721,-16.4116969953064,
5.21697815244371));
#152224=CARTESIAN_POINT('Ctrl Pts',(-18.9784552815195,-16.4023177375285,
5.22116278683676));
#152225=CARTESIAN_POINT('Ctrl Pts',(-18.894727859237,-16.3970505767697,
5.22534742122981));
#152226=CARTESIAN_POINT('Ctrl Pts',(-18.8111196125767,-16.3917909131622,
5.22952609931376));
#152227=CARTESIAN_POINT('Ctrl Pts',(-18.7271286822944,-16.3906317491884,
5.2337047773977));
#152228=CARTESIAN_POINT('Ctrl Pts',(-18.6431902849674,-16.3936111328307,
5.23788345548164));
#152229=CARTESIAN_POINT('Ctrl Pts',(-18.5577473521939,-16.3966439197836,
5.24213703336708));
#152230=CARTESIAN_POINT('Ctrl Pts',(-18.4723593301118,-16.4039651578947,
5.24639061125252));
#152231=CARTESIAN_POINT('Ctrl Pts',(-18.3874890362874,-16.4155595508613,
5.25064418913795));
#152232=CARTESIAN_POINT('Ctrl Pts',(-18.3042641187195,-16.4269291638956,
5.2548153031159));
#152233=CARTESIAN_POINT('Ctrl Pts',(-18.2215375109946,-16.44240765832,5.25898641709385));
#152234=CARTESIAN_POINT('Ctrl Pts',(-18.1397421978239,-16.4619281808444,
5.26315753107181));
#152235=CARTESIAN_POINT('Ctrl Pts',(-18.0579743318605,-16.4814421530689,
5.26732724539218));
#152236=CARTESIAN_POINT('Ctrl Pts',(-17.9771375869061,-16.5049953529781,
5.27149695971255));
#152237=CARTESIAN_POINT('Ctrl Pts',(-17.8976542388869,-16.5324699282984,
5.27566667403293));
#152238=CARTESIAN_POINT('Ctrl Pts',(-17.8181737192263,-16.5599435259556,
5.27983623997697));
#152239=CARTESIAN_POINT('Ctrl Pts',(-17.7400469352591,-16.5913380704868,
5.28400580592101));
#152240=CARTESIAN_POINT('Ctrl Pts',(-17.6636791864353,-16.6264864317639,
5.28817537186506));
#152241=CARTESIAN_POINT('Ctrl Pts',(-17.5846264417726,-16.6628705660634,
5.29249153460398));
#152242=CARTESIAN_POINT('Ctrl Pts',(-17.5074592081877,-16.7032771763716,
5.2968076973429));
#152243=CARTESIAN_POINT('Ctrl Pts',(-17.4326007161618,-16.7474683254656,
5.30112386008182));
#152244=CARTESIAN_POINT('Ctrl Pts',(-17.36018073164,-16.7902199525259,5.3052994242735));
#152245=CARTESIAN_POINT('Ctrl Pts',(-17.2899217514086,-16.8365130434918,
5.30947498846518));
#152246=CARTESIAN_POINT('Ctrl Pts',(-17.2221770223174,-16.886088268064,
5.31365055265686));
#152247=CARTESIAN_POINT('Ctrl Pts',(-17.1510106680076,-16.9381674193753,
5.3180370146694));
#152248=CARTESIAN_POINT('Ctrl Pts',(-17.0826196821852,-16.9938686102921,
5.32242347668194));
#152249=CARTESIAN_POINT('Ctrl Pts',(-17.0173721044249,-17.0528452753571,
5.32680993869448));
#152250=CARTESIAN_POINT('Ctrl Pts',(-16.9521245266647,-17.1118219404221,
5.33119640070702));
#152251=CARTESIAN_POINT('Ctrl Pts',(-16.890020712904,-17.1740736151505,
5.33558286271956));
#152252=CARTESIAN_POINT('Ctrl Pts',(-16.8313804354228,-17.239213150305,
5.3399693247321));
#152253=CARTESIAN_POINT('Ctrl Pts',(-16.7754382840343,-17.3013555188871,
5.34415395912515));
#152254=CARTESIAN_POINT('Ctrl Pts',(-16.7224397206528,-17.3663571440021,
5.34833859351819));
#152255=CARTESIAN_POINT('Ctrl Pts',(-16.6726908063355,-17.4339076417707,
5.35252322791124));
#152256=CARTESIAN_POINT('Ctrl Pts',(-16.6230127034401,-17.5013619897667,
5.35670190599519));
#152257=CARTESIAN_POINT('Ctrl Pts',(-16.576575332432,-17.5713576368075,
5.36088058407914));
#152258=CARTESIAN_POINT('Ctrl Pts',(-16.533646260122,-17.6435492292772,
5.36505926216308));
#152259=CARTESIAN_POINT('Ctrl Pts',(-16.4899477150435,-17.7170348041588,
5.36931284004852));
#152260=CARTESIAN_POINT('Ctrl Pts',(-16.4498848008428,-17.7927954651137,
5.37356641793395));
#152261=CARTESIAN_POINT('Ctrl Pts',(-16.4136951701205,-17.8704337762126,
5.37781999581938));
#152262=CARTESIAN_POINT('Ctrl Pts',(-16.378207146008,-17.9465669171521,
5.38199110979734));
#152263=CARTESIAN_POINT('Ctrl Pts',(-16.3464437665668,-18.0245051179384,
5.38616222377529));
#152264=CARTESIAN_POINT('Ctrl Pts',(-16.3185831851716,-18.1038481205324,
5.39033333775324));
#152265=CARTESIAN_POINT('Ctrl Pts',(-16.2907319526636,-18.1831644988157,
5.39450305207362));
#152266=CARTESIAN_POINT('Ctrl Pts',(-16.2667810695588,-18.2638843090191,
5.39867276639399));
#152267=CARTESIAN_POINT('Ctrl Pts',(-16.2468600106956,-18.3455886927151,
5.40284248071436));
#152268=CARTESIAN_POINT('Ctrl Pts',(-16.2269396607092,-18.4272901690185,
5.40701204665841));
#152269=CARTESIAN_POINT('Ctrl Pts',(-16.2110489579957,-18.5099757020134,
5.41118161260245));
#152270=CARTESIAN_POINT('Ctrl Pts',(-16.1992667534716,-18.5932140346339,
5.4153511785465));
#152271=CARTESIAN_POINT('Ctrl Pts',(-16.1870703011713,-18.6793789243438,
5.41966734128542));
#152272=CARTESIAN_POINT('Ctrl Pts',(-16.1792767060087,-18.7661356875971,
5.42398350402433));
#152273=CARTESIAN_POINT('Ctrl Pts',(-16.1759149870658,-18.8529996636308,
5.42829966676326));
#152274=CARTESIAN_POINT('Ctrl Pts',(-16.1726627757638,-18.9370340547817,
5.43247523095494));
#152275=CARTESIAN_POINT('Ctrl Pts',(-16.1735580857934,-19.0211683105535,
5.43665079514662));
#152276=CARTESIAN_POINT('Ctrl Pts',(-16.1785740672325,-19.1049650356758,
5.4408263593383));
#152277=CARTESIAN_POINT('Ctrl Pts',(-16.1838433939698,-19.1929941341762,
5.44521282135084));
#152278=CARTESIAN_POINT('Ctrl Pts',(-16.1936605371381,-19.2806501283313,
5.44959928336338));
#152279=CARTESIAN_POINT('Ctrl Pts',(-16.2079333028747,-19.3674359657934,
5.45398574537592));
#152280=CARTESIAN_POINT('Ctrl Pts',(-16.2222060686114,-19.4542218032555,
5.45837220738846));
#152281=CARTESIAN_POINT('Ctrl Pts',(-16.2409342590202,-19.5401369333207,
5.462758669401));
#152282=CARTESIAN_POINT('Ctrl Pts',(-16.2639654295305,-19.6247029215675,
5.46714513141354));
#152283=CARTESIAN_POINT('Ctrl Pts',(-16.2859330287312,-19.7053636823823,
5.47132902816154));
#152284=CARTESIAN_POINT('Ctrl Pts',(-16.3118967078507,-19.7850973400462,
5.47551292490953));
#152285=CARTESIAN_POINT('Ctrl Pts',(-16.3417612031338,-19.8634787648475,
5.47969682165753));
#152286=CARTESIAN_POINT('Ctrl Pts',(-16.3715858706222,-19.9417556588589,
5.48387513869027));
#152287=CARTESIAN_POINT('Ctrl Pts',(-16.4053008633503,-20.018683474586,
5.488053455723));
#152288=CARTESIAN_POINT('Ctrl Pts',(-16.4427606711044,-20.0938504007627,
5.49223177275574));
#152289=CARTESIAN_POINT('Ctrl Pts',(-16.4801817643412,-20.1689396423106,
5.49640577151947));
#152290=CARTESIAN_POINT('Ctrl Pts',(-16.5213397815898,-20.242271199406,
5.5005797702832));
#152291=CARTESIAN_POINT('Ctrl Pts',(-16.5660409635171,-20.31345275942,5.50475376904693));
#152292=CARTESIAN_POINT('Ctrl Pts',(-16.6107117825595,-20.384585969985,
5.50892493265869));
#152293=CARTESIAN_POINT('Ctrl Pts',(-16.6589207423439,-20.4535716954381,
5.51309609627045));
#152294=CARTESIAN_POINT('Ctrl Pts',(-16.7104285670038,-20.5200429380478,
5.51726725988221));
#152295=CARTESIAN_POINT('Ctrl Pts',(-16.7619153763091,-20.5864870601814,
5.52143672164609));
#152296=CARTESIAN_POINT('Ctrl Pts',(-16.8166980925858,-20.6504183762542,
5.52560618340997));
#152297=CARTESIAN_POINT('Ctrl Pts',(-16.8744954343627,-20.7115007162187,
5.52977564517385));
#152298=CARTESIAN_POINT('Ctrl Pts',(-16.9323025068466,-20.7725933399494,
5.53394580890445));
#152299=CARTESIAN_POINT('Ctrl Pts',(-16.9931249059,-20.8308356918097,5.53811597263505));
#152300=CARTESIAN_POINT('Ctrl Pts',(-17.0566432414223,-20.8859271714451,
5.54228613636565));
#152301=CARTESIAN_POINT('Ctrl Pts',(-17.0949617933418,-20.9191620744912,
5.54480186090581));
#152302=CARTESIAN_POINT('Ctrl Pts',(-17.134260768482,-20.9512509900032,
5.54731758544598));
#152303=CARTESIAN_POINT('Ctrl Pts',(-17.1744641402401,-20.9821349467765,
5.54983330998614));
#152304=CARTESIAN_POINT('Ctrl Pts',(-17.1762220465438,-20.9798104602809,
4.74997346007641));
#152305=CARTESIAN_POINT('Ctrl Pts',(-17.6117180223192,-21.3095662889742,
4.77707100605307));
#152306=CARTESIAN_POINT('Ctrl Pts',(-18.9946005733993,-21.8166035361695,
4.8465604875902));
#152307=CARTESIAN_POINT('Ctrl Pts',(-20.9008594909828,-20.8156360190963,
4.94099937082189));
#152308=CARTESIAN_POINT('Ctrl Pts',(-21.288210216193,-19.4541225063383,
5.00834070807693));
#152309=CARTESIAN_POINT('Ctrl Pts',(-21.2903252254699,-18.9508059208324,
5.0332901097715));
#152310=CARTESIAN_POINT('',(-21.2942629789487,-18.9528355653121,4.96670989022851));
#152311=CARTESIAN_POINT('Ctrl Pts',(-17.1735447294247,-20.9833104140831,
4.68319929961578));
#152312=CARTESIAN_POINT('Ctrl Pts',(-17.2909884433531,-21.0753829841412,
4.69063448214821));
#152313=CARTESIAN_POINT('Ctrl Pts',(-18.1310916369067,-21.6211178664512,
4.74046160024112));
#152314=CARTESIAN_POINT('Ctrl Pts',(-20.2331955554845,-21.5817725214897,
4.83268065389451));
#152315=CARTESIAN_POINT('Ctrl Pts',(-21.2762380205877,-19.8928505327429,
4.91974900156632));
#152316=CARTESIAN_POINT('Ctrl Pts',(-21.298094862478,-18.9985742441059,
4.96442541367765));
#152317=CARTESIAN_POINT('Ctrl Pts',(-21.2979001547653,-18.9528367523378,
4.96670989022851));
#152318=CARTESIAN_POINT('Ctrl Pts',(-21.2939998636668,-18.952835479442,
4.96670989022851));
#152319=CARTESIAN_POINT('Ctrl Pts',(-21.2940269378476,-18.8698772454869,
4.97085977152528));
#152320=CARTESIAN_POINT('Ctrl Pts',(-21.2900172964774,-18.7867551328103,
4.97500965282205));
#152321=CARTESIAN_POINT('Ctrl Pts',(-21.2819493183893,-18.7038986680417,
4.97915953411883));
#152322=CARTESIAN_POINT('Ctrl Pts',(-21.273892503302,-18.6211568449806,
4.98330367356456));
#152323=CARTESIAN_POINT('Ctrl Pts',(-21.2617885455565,-18.5386804021309,
4.98744781301029));
#152324=CARTESIAN_POINT('Ctrl Pts',(-21.2456678375727,-18.456899329729,
4.99159195245603));
#152325=CARTESIAN_POINT('Ctrl Pts',(-21.2295645603719,-18.3752066844683,
4.99573161098224));
#152326=CARTESIAN_POINT('Ctrl Pts',(-21.2094532518122,-18.294208373011,
4.99987126950845));
#152327=CARTESIAN_POINT('Ctrl Pts',(-21.1854159920051,-18.2143282341436,
5.00401092803467));
#152328=CARTESIAN_POINT('Ctrl Pts',(-21.1613926712713,-18.1344944173246,
5.00814818599592));
#152329=CARTESIAN_POINT('Ctrl Pts',(-21.1334480518403,-18.0557779336931,
5.01228544395717));
#152330=CARTESIAN_POINT('Ctrl Pts',(-21.1017147974227,-17.9785902003445,
5.01642270191842));
#152331=CARTESIAN_POINT('Ctrl Pts',(-21.069990038471,-17.9014231313041,
5.02055885227397));
#152332=CARTESIAN_POINT('Ctrl Pts',(-21.0344788364885,-17.8257844328049,
5.02469500262952));
#152333=CARTESIAN_POINT('Ctrl Pts',(-20.9953624823967,-17.7520667838548,
5.02883115298507));
#152334=CARTESIAN_POINT('Ctrl Pts',(-20.9562443890682,-17.678345857185,
5.03296748724695));
#152335=CARTESIAN_POINT('Ctrl Pts',(-20.9135210465752,-17.6065465624556,
5.03710382150882));
#152336=CARTESIAN_POINT('Ctrl Pts',(-20.8674196102011,-17.5370368319954,
5.0412401557707));
#152337=CARTESIAN_POINT('Ctrl Pts',(-20.8212714994527,-17.4674567279542,
5.04538067777222));
#152338=CARTESIAN_POINT('Ctrl Pts',(-20.7717387262313,-17.4001712070023,
5.04952119977375));
#152339=CARTESIAN_POINT('Ctrl Pts',(-20.7190913321281,-17.3355185113618,
5.05366172177528));
#152340=CARTESIAN_POINT('Ctrl Pts',(-20.6664157771983,-17.2708312333193,
5.05780445852121));
#152341=CARTESIAN_POINT('Ctrl Pts',(-20.6106225991452,-17.208779931402,
5.06194719526715));
#152342=CARTESIAN_POINT('Ctrl Pts',(-20.5520199344772,-17.1496672011409,
5.06608993201309));
#152343=CARTESIAN_POINT('Ctrl Pts',(-20.493317306161,-17.0904536371683,
5.07023973538444));
#152344=CARTESIAN_POINT('Ctrl Pts',(-20.4317959684771,-17.034188968823,
5.07438953875579));
#152345=CARTESIAN_POINT('Ctrl Pts',(-20.3677981562822,-16.9811363353776,
5.07853934212713));
#152346=CARTESIAN_POINT('Ctrl Pts',(-20.324139169833,-16.9449440949673,
5.08137031717055));
#152347=CARTESIAN_POINT('Ctrl Pts',(-20.2793283343474,-16.9102458437321,
5.08420129221396));
#152348=CARTESIAN_POINT('Ctrl Pts',(-20.2334815623284,-16.8771132454428,
5.08703226725737));
#152349=CARTESIAN_POINT('Ctrl Pts',(-20.1657126925719,-16.8281379601764,
5.09121690165042));
#152350=CARTESIAN_POINT('Ctrl Pts',(-20.0954157767523,-16.7823951726099,
5.09540153604348));
#152351=CARTESIAN_POINT('Ctrl Pts',(-20.0229321512533,-16.7401559934151,
5.09958617043653));
#152352=CARTESIAN_POINT('Ctrl Pts',(-19.9505516972234,-16.6979769364637,
5.10376484852047));
#152353=CARTESIAN_POINT('Ctrl Pts',(-19.8759911100091,-16.6592918118668,
5.10794352660442));
#152354=CARTESIAN_POINT('Ctrl Pts',(-19.799622378274,-16.6243297168797,
5.11212220468837));
#152355=CARTESIAN_POINT('Ctrl Pts',(-19.7218847919079,-16.5887409514667,
5.1163757825738));
#152356=CARTESIAN_POINT('Ctrl Pts',(-19.6422739922292,-16.5570102814913,
5.12062936045924));
#152357=CARTESIAN_POINT('Ctrl Pts',(-19.5612105522305,-16.5293314914585,
5.12488293834467));
#152358=CARTESIAN_POINT('Ctrl Pts',(-19.4817186851985,-16.5021893087812,
5.12905405232263));
#152359=CARTESIAN_POINT('Ctrl Pts',(-19.4008304551545,-16.478943456341,
5.13322516630058));
#152360=CARTESIAN_POINT('Ctrl Pts',(-19.3189628776791,-16.4597282588495,
5.13739628027853));
#152361=CARTESIAN_POINT('Ctrl Pts',(-19.2371227716601,-16.4405195092031,
5.1415659945989));
#152362=CARTESIAN_POINT('Ctrl Pts',(-19.1543044183625,-16.4253388333996,
5.14573570891927));
#152363=CARTESIAN_POINT('Ctrl Pts',(-19.0709381209925,-16.4142701675273,
5.14990542323965));
#152364=CARTESIAN_POINT('Ctrl Pts',(-18.987574790153,-16.4032018955255,
5.1540749891837));
#152365=CARTESIAN_POINT('Ctrl Pts',(-18.9036640101517,-16.3962454022305,
5.15824455512774));
#152366=CARTESIAN_POINT('Ctrl Pts',(-18.8196429975839,-16.3934329641448,
5.16241412107179));
#152367=CARTESIAN_POINT('Ctrl Pts',(-18.7326679098655,-16.3905216442056,
5.16673028381071));
#152368=CARTESIAN_POINT('Ctrl Pts',(-18.6455752209302,-16.3920512290413,
5.17104644654963));
#152369=CARTESIAN_POINT('Ctrl Pts',(-18.5588499153532,-16.3979987376964,
5.17536260928855));
#152370=CARTESIAN_POINT('Ctrl Pts',(-18.4749496774836,-16.4037525068827,
5.17953817348022));
#152371=CARTESIAN_POINT('Ctrl Pts',(-18.3913937177405,-16.413640690019,
5.1837137376719));
#152372=CARTESIAN_POINT('Ctrl Pts',(-18.3086140512034,-16.4275898125371,
5.18788930186358));
#152373=CARTESIAN_POINT('Ctrl Pts',(-18.2216533804996,-16.4422434720727,
5.19227576387612));
#152374=CARTESIAN_POINT('Ctrl Pts',(-18.1355500550634,-16.461378961618,
5.19666222588866));
#152375=CARTESIAN_POINT('Ctrl Pts',(-18.0507884164764,-16.4848514572205,
5.2010486879012));
#152376=CARTESIAN_POINT('Ctrl Pts',(-17.9660267778894,-16.508323952823,
5.20543514991373));
#152377=CARTESIAN_POINT('Ctrl Pts',(-17.8826073525323,-16.5361331988247,
5.20982161192627));
#152378=CARTESIAN_POINT('Ctrl Pts',(-17.8009895271363,-16.5680764572817,
5.21420807393881));
#152379=CARTESIAN_POINT('Ctrl Pts',(-17.7231270588734,-16.5985499590658,
5.21839270833186));
#152380=CARTESIAN_POINT('Ctrl Pts',(-17.6466142262364,-16.6328988372128,
5.2225773427249));
#152381=CARTESIAN_POINT('Ctrl Pts',(-17.5718637493067,-16.6709828289062,
5.22676197711795));
#152382=CARTESIAN_POINT('Ctrl Pts',(-17.4972196704287,-16.7090126127514,
5.23094065520189));
#152383=CARTESIAN_POINT('Ctrl Pts',(-17.4243333709909,-16.7507667429069,
5.23511933328583));
#152384=CARTESIAN_POINT('Ctrl Pts',(-17.3535988359376,-16.7960564417742,
5.23929801136977));
#152385=CARTESIAN_POINT('Ctrl Pts',(-17.2815964351795,-16.8421579259446,
5.24355158925521));
#152386=CARTESIAN_POINT('Ctrl Pts',(-17.2118241472897,-16.8919227999544,
5.24780516714065));
#152387=CARTESIAN_POINT('Ctrl Pts',(-17.144672562554,-16.9451023203508,
5.25205874502608));
#152388=CARTESIAN_POINT('Ctrl Pts',(-17.078822842324,-16.997250851973,5.25622985900404));
#152389=CARTESIAN_POINT('Ctrl Pts',(-17.0154934944014,-17.0526825135667,
5.26040097298199));
#152390=CARTESIAN_POINT('Ctrl Pts',(-16.955023187236,-17.1111193684413,
5.26457208695994));
#152391=CARTESIAN_POINT('Ctrl Pts',(-16.8945731714661,-17.1695366142649,
5.26874180128032));
#152392=CARTESIAN_POINT('Ctrl Pts',(-16.8369806216437,-17.2309567312115,
5.27291151560069));
#152393=CARTESIAN_POINT('Ctrl Pts',(-16.7825490296999,-17.2950633353943,
5.27708122992106));
#152394=CARTESIAN_POINT('Ctrl Pts',(-16.7281193746657,-17.3591676583889,
5.28125079586511));
#152395=CARTESIAN_POINT('Ctrl Pts',(-16.6768507509727,-17.4259579273207,
5.28542036180915));
#152396=CARTESIAN_POINT('Ctrl Pts',(-16.6290069551022,-17.495083982883,
5.28958992775319));
#152397=CARTESIAN_POINT('Ctrl Pts',(-16.5794810303907,-17.5666404252826,
5.29390609049211));
#152398=CARTESIAN_POINT('Ctrl Pts',(-16.5336255484983,-17.6406995292211,
5.29822225323103));
#152399=CARTESIAN_POINT('Ctrl Pts',(-16.4916836990302,-17.7168410602658,
5.30253841596995));
#152400=CARTESIAN_POINT('Ctrl Pts',(-16.4511081008972,-17.7905022889454,
5.30671398016163));
#152401=CARTESIAN_POINT('Ctrl Pts',(-16.414195241831,-17.8661119140595,
5.31088954435331));
#152402=CARTESIAN_POINT('Ctrl Pts',(-16.3811171829163,-17.9432669089039,
5.31506510854499));
#152403=CARTESIAN_POINT('Ctrl Pts',(-16.3463684298814,-18.0243188191194,
5.31945157055753));
#152404=CARTESIAN_POINT('Ctrl Pts',(-16.3158522513522,-18.1070757672222,
5.32383803257007));
#152405=CARTESIAN_POINT('Ctrl Pts',(-16.2897090382153,-18.1910521081324,
5.32822449458261));
#152406=CARTESIAN_POINT('Ctrl Pts',(-16.2635658250785,-18.2750284490425,
5.33261095659515));
#152407=CARTESIAN_POINT('Ctrl Pts',(-16.2417956472861,-18.3602236017744,
5.3369974186077));
#152408=CARTESIAN_POINT('Ctrl Pts',(-16.2244766916358,-18.4461415565825,
5.34138388062024));
#152409=CARTESIAN_POINT('Ctrl Pts',(-16.2079546068079,-18.5281062989289,
5.34556851501329));
#152410=CARTESIAN_POINT('Ctrl Pts',(-16.1954216323759,-18.6110338790213,
5.34975314940633));
#152411=CARTESIAN_POINT('Ctrl Pts',(-16.1869832270606,-18.6945013429833,
5.35393778379938));
#152412=CARTESIAN_POINT('Ctrl Pts',(-16.1785568327709,-18.7778500013415,
5.35811646188332));
#152413=CARTESIAN_POINT('Ctrl Pts',(-16.1742134770096,-18.8617365633852,
5.36229513996725));
#152414=CARTESIAN_POINT('Ctrl Pts',(-16.174007684269,-18.9457275683919,
5.36647381805119));
#152415=CARTESIAN_POINT('Ctrl Pts',(-16.1737982028414,-19.0312240518001,
5.37072739593663));
#152416=CARTESIAN_POINT('Ctrl Pts',(-16.1778761703229,-19.1168282866475,
5.37498097382206));
#152417=CARTESIAN_POINT('Ctrl Pts',(-16.1862438519479,-19.2020772082027,
5.3792345517075));
#152418=CARTESIAN_POINT('Ctrl Pts',(-16.1944493097363,-19.285673413064,
5.38340566568545));
#152419=CARTESIAN_POINT('Ctrl Pts',(-16.2067795899915,-19.3689274796563,
5.3875767796634));
#152420=CARTESIAN_POINT('Ctrl Pts',(-16.2231843067497,-19.4514041995498,
5.39174789364135));
#152421=CARTESIAN_POINT('Ctrl Pts',(-16.2395835187468,-19.5338532435834,
5.39591760796172));
#152422=CARTESIAN_POINT('Ctrl Pts',(-16.2600543622648,-19.615525008144,
5.4000873222821));
#152423=CARTESIAN_POINT('Ctrl Pts',(-16.28449508295,-19.6959930519487,5.40425703660247));
#152424=CARTESIAN_POINT('Ctrl Pts',(-16.3089349339295,-19.7764582323553,
5.40842660254652));
#152425=CARTESIAN_POINT('Ctrl Pts',(-16.3373442466933,-19.8557193372408,
5.41259616849057));
#152426=CARTESIAN_POINT('Ctrl Pts',(-16.3695713807105,-19.9333650209197,
5.41676573443462));
#152427=CARTESIAN_POINT('Ctrl Pts',(-16.4029315810032,-20.0137406310502,
5.42108189717354));
#152428=CARTESIAN_POINT('Ctrl Pts',(-16.4403828646777,-20.0923846228543,
5.42539805991246));
#152429=CARTESIAN_POINT('Ctrl Pts',(-16.4817035150009,-20.1688650474316,
5.42971422265138));
#152430=CARTESIAN_POINT('Ctrl Pts',(-16.5216781494859,-20.2428541302225,
5.43388978684306));
#152431=CARTESIAN_POINT('Ctrl Pts',(-16.5652736482195,-20.3148180591348,
5.43806535103474));
#152432=CARTESIAN_POINT('Ctrl Pts',(-16.6122442629255,-20.3843940073149,
5.44224091522642));
#152433=CARTESIAN_POINT('Ctrl Pts',(-16.6615872517183,-20.4574840712365,
5.44662737723896));
#152434=CARTESIAN_POINT('Ctrl Pts',(-16.714654919849,-20.527938114488,5.45101383925151));
#152435=CARTESIAN_POINT('Ctrl Pts',(-16.7711149075847,-20.5953752200803,
5.45540030126405));
#152436=CARTESIAN_POINT('Ctrl Pts',(-16.8275748953204,-20.6628123256726,
5.45978676327659));
#152437=CARTESIAN_POINT('Ctrl Pts',(-16.8874267520077,-20.7272321203105,
5.46417322528914));
#152438=CARTESIAN_POINT('Ctrl Pts',(-16.9502957329767,-20.788300380603,
5.46855968730168));
#152439=CARTESIAN_POINT('Ctrl Pts',(-17.0102748276393,-20.8465615279686,
5.47274451766204));
#152440=CARTESIAN_POINT('Ctrl Pts',(-17.073223024649,-20.9019893649773,
5.4769293480224));
#152441=CARTESIAN_POINT('Ctrl Pts',(-17.1388417266606,-20.9542662367919,
5.48111417838276));
#152442=CARTESIAN_POINT('Ctrl Pts',(-17.1506303973543,-20.963657992615,
5.48186600043219));
#152443=CARTESIAN_POINT('Ctrl Pts',(-17.1625051568043,-20.9729481370306,
5.48261782248163));
#152444=CARTESIAN_POINT('Ctrl Pts',(-17.1744641402401,-20.9821349467765,
5.48336964453106));
#152445=CARTESIAN_POINT('Origin',(-18.734,-18.952,-1.76670989022851));
#152446=CARTESIAN_POINT('',(-17.1721129507126,-20.9851649608899,6.34984101818205));
#152447=CARTESIAN_POINT('',(-17.1744641402401,-20.9821349467765,6.28334279287586));
#152448=CARTESIAN_POINT('',(-17.1744641402401,-20.9821349467765,-1.76670989022851));
#152449=CARTESIAN_POINT('',(-21.2939994369002,-18.9503020392335,5.8332901097715));
#152450=CARTESIAN_POINT('Ctrl Pts',(-21.2967673690372,-18.950300203358,
5.8332901097715));
#152451=CARTESIAN_POINT('Ctrl Pts',(-21.2975539709192,-18.8475231740461,
5.83841759033362));
#152452=CARTESIAN_POINT('Ctrl Pts',(-21.2452320420947,-17.8958349639979,
5.88593700645621));
#152453=CARTESIAN_POINT('Ctrl Pts',(-20.0538051353946,-16.2277743551153,
5.97584835813928));
#152454=CARTESIAN_POINT('Ctrl Pts',(-17.1577428384119,-16.3676810722738,
6.10302416482072));
#152455=CARTESIAN_POINT('Ctrl Pts',(-15.736433506265,-18.8289532162803,
6.22768838483497));
#152456=CARTESIAN_POINT('Ctrl Pts',(-16.5413044417107,-20.4955798434453,
6.30996066928875));
#152457=CARTESIAN_POINT('Ctrl Pts',(-17.1721129507126,-20.9851649608899,
6.34984101818205));
#152458=CARTESIAN_POINT('Ctrl Pts',(-17.1744641402401,-20.9821349467765,
5.54983330998614));
#152459=CARTESIAN_POINT('Ctrl Pts',(-17.2411773822525,-21.0333836055931,
5.55400788870292));
#152460=CARTESIAN_POINT('Ctrl Pts',(-17.3103822987326,-21.0813118661074,
5.5581824674197));
#152461=CARTESIAN_POINT('Ctrl Pts',(-17.3817082756447,-21.1256851410083,
5.56235704613648));
#152462=CARTESIAN_POINT('Ctrl Pts',(-17.4530769014014,-21.1700849485833,
5.56653412101197));
#152463=CARTESIAN_POINT('Ctrl Pts',(-17.5265687102689,-21.2109253156985,
5.57071119588746));
#152464=CARTESIAN_POINT('Ctrl Pts',(-17.6017887254332,-21.2480177764434,
5.57488827076295));
#152465=CARTESIAN_POINT('Ctrl Pts',(-17.6771346879595,-21.2851723442958,
5.57907233967534));
#152466=CARTESIAN_POINT('Ctrl Pts',(-17.7542142119762,-21.318566294549,
5.58325640858772));
#152467=CARTESIAN_POINT('Ctrl Pts',(-17.8326129636017,-21.3480595590705,
5.58744047750011));
#152468=CARTESIAN_POINT('Ctrl Pts',(-17.8755870423865,-21.364226217938,
5.58973396436506));
#152469=CARTESIAN_POINT('Ctrl Pts',(-17.9189572378514,-21.3792217334331,
5.59202745123002));
#152470=CARTESIAN_POINT('Ctrl Pts',(-17.9626538344086,-21.393029514944,
5.59432093809498));
#152471=CARTESIAN_POINT('Ctrl Pts',(-18.042381468173,-21.4182228213826,
5.59850557248802));
#152472=CARTESIAN_POINT('Ctrl Pts',(-18.123493045634,-21.4395528703719,
5.60269020688107));
#152473=CARTESIAN_POINT('Ctrl Pts',(-18.2055793173495,-21.4568695738795,
5.60687484127412));
#152474=CARTESIAN_POINT('Ctrl Pts',(-18.2875487494174,-21.474161629203,
5.61105351935806));
#152475=CARTESIAN_POINT('Ctrl Pts',(-18.3704896737371,-21.4874515917234,
5.615232197442));
#152476=CARTESIAN_POINT('Ctrl Pts',(-18.4539769469565,-21.4966388918203,
5.61941087552594));
#152477=CARTESIAN_POINT('Ctrl Pts',(-18.5389606695473,-21.5059908676685,
5.62366445341137));
#152478=CARTESIAN_POINT('Ctrl Pts',(-18.624510060566,-21.511091508697,5.62791803129681));
#152479=CARTESIAN_POINT('Ctrl Pts',(-18.7101649534091,-21.5118890387191,
5.63217160918224));
#152480=CARTESIAN_POINT('Ctrl Pts',(-18.7941592590127,-21.5126711070654,
5.63634272316019));
#152481=CARTESIAN_POINT('Ctrl Pts',(-18.87825453103,-21.5093154194064,5.64051383713815));
#152482=CARTESIAN_POINT('Ctrl Pts',(-18.9620126684401,-21.5018255279589,
5.6446849511161));
#152483=CARTESIAN_POINT('Ctrl Pts',(-19.0457426999983,-21.4943381498168,
5.64885466543647));
#152484=CARTESIAN_POINT('Ctrl Pts',(-19.1291353638018,-21.4827193639704,
5.65302437975684));
#152485=CARTESIAN_POINT('Ctrl Pts',(-19.2117557819361,-21.4670247340387,
5.65719409407721));
#152486=CARTESIAN_POINT('Ctrl Pts',(-19.2943732600814,-21.4513306625894,
5.66136366002126));
#152487=CARTESIAN_POINT('Ctrl Pts',(-19.3762180954026,-21.4315611221138,
5.66553322596531));
#152488=CARTESIAN_POINT('Ctrl Pts',(-19.4568650837658,-21.4078228907379,
5.66970279190935));
#152489=CARTESIAN_POINT('Ctrl Pts',(-19.5403475207509,-21.3832500524311,
5.67401895464827));
#152490=CARTESIAN_POINT('Ctrl Pts',(-19.6225458049915,-21.354424401291,
5.6783351173872));
#152491=CARTESIAN_POINT('Ctrl Pts',(-19.7030067527823,-21.3215201862534,
5.68265128012612));
#152492=CARTESIAN_POINT('Ctrl Pts',(-19.7808466936618,-21.2896878225597,
5.6868268443178));
#152493=CARTESIAN_POINT('Ctrl Pts',(-19.8570603406959,-21.2540387751658,
5.69100240850948));
#152494=CARTESIAN_POINT('Ctrl Pts',(-19.9312606656524,-21.2147785791989,
5.69517797270115));
#152495=CARTESIAN_POINT('Ctrl Pts',(-20.009208672628,-21.173535444066,5.6995644347137));
#152496=CARTESIAN_POINT('Ctrl Pts',(-20.0849341253746,-21.1283070744553,
5.70395089672624));
#152497=CARTESIAN_POINT('Ctrl Pts',(-20.1580227463385,-21.0793831854912,
5.70833735873878));
#152498=CARTESIAN_POINT('Ctrl Pts',(-20.2311113673024,-21.0304592965271,
5.71272382075132));
#152499=CARTESIAN_POINT('Ctrl Pts',(-20.3015627371329,-20.977840296355,
5.71711028276386));
#152500=CARTESIAN_POINT('Ctrl Pts',(-20.3690044710744,-20.9218630357379,
5.72149674477641));
#152501=CARTESIAN_POINT('Ctrl Pts',(-20.4324580482223,-20.8691959820087,
5.72562381401755));
#152502=CARTESIAN_POINT('Ctrl Pts',(-20.493497997814,-20.8133485129555,
5.72975088325869));
#152503=CARTESIAN_POINT('Ctrl Pts',(-20.5517814829091,-20.7545732940418,
5.73387795249983));
#152504=CARTESIAN_POINT('Ctrl Pts',(-20.6102782700971,-20.6955829734199,
5.73802012571948));
#152505=CARTESIAN_POINT('Ctrl Pts',(-20.6659979620833,-20.6336436795686,
5.74216229893913));
#152506=CARTESIAN_POINT('Ctrl Pts',(-20.7186255971236,-20.5690532580103,
5.74630447215879));
#152507=CARTESIAN_POINT('Ctrl Pts',(-20.7709257203661,-20.5048647949491,
5.75042086784546));
#152508=CARTESIAN_POINT('Ctrl Pts',(-20.8201718394842,-20.4380584608902,
5.75453726353214));
#152509=CARTESIAN_POINT('Ctrl Pts',(-20.8660914253506,-20.368963709467,
5.75865365921881));
#152510=CARTESIAN_POINT('Ctrl Pts',(-20.9119829684086,-20.299911153783,
5.76276754104798));
#152511=CARTESIAN_POINT('Ctrl Pts',(-20.9545517475122,-20.228573347296,
5.76688142287715));
#152512=CARTESIAN_POINT('Ctrl Pts',(-20.993566969393,-20.1553108953334,
5.77099530470633));
#152513=CARTESIAN_POINT('Ctrl Pts',(-21.0325708263852,-20.0820697842621,
5.77510798818761));
#152514=CARTESIAN_POINT('Ctrl Pts',(-21.0680229592545,-20.006905559054,
5.7792206716689));
#152515=CARTESIAN_POINT('Ctrl Pts',(-21.0997379788823,-19.9302043831808,
5.78333335515018));
#152516=CARTESIAN_POINT('Ctrl Pts',(-21.1318415000294,-19.8525636359715,
5.78749641803529));
#152517=CARTESIAN_POINT('Ctrl Pts',(-21.1601155043872,-19.7733484709675,
5.7916594809204));
#152518=CARTESIAN_POINT('Ctrl Pts',(-21.1844181339265,-19.6929797358392,
5.79582254380551));
#152519=CARTESIAN_POINT('Ctrl Pts',(-21.2084475698834,-19.6135144512045,
5.79993880837766));
#152520=CARTESIAN_POINT('Ctrl Pts',(-21.2285944016387,-19.5329218806182,
5.80405507294981));
#152521=CARTESIAN_POINT('Ctrl Pts',(-21.2447724368935,-19.45162162697,5.80817133752195));
#152522=CARTESIAN_POINT('Ctrl Pts',(-21.2612263672263,-19.3689349046021,
5.81235779956354));
#152523=CARTESIAN_POINT('Ctrl Pts',(-21.2735747867911,-19.2855166404038,
5.81654426160514));
#152524=CARTESIAN_POINT('Ctrl Pts',(-21.281781944964,-19.2018142528271,
5.82073072364673));
#152525=CARTESIAN_POINT('Ctrl Pts',(-21.2899891031369,-19.1181118652504,
5.82491718568832));
#152526=CARTESIAN_POINT('Ctrl Pts',(-21.2940550344004,-19.0341258661346,
5.82910364772991));
#152527=CARTESIAN_POINT('Ctrl Pts',(-21.2939994369002,-18.9503020392335,
5.8332901097715));
#152528=CARTESIAN_POINT('',(-21.2939992944986,-18.9539005700933,5.76670989019962));
#152529=CARTESIAN_POINT('Ctrl Pts',(-17.1744641402401,-20.9821349467765,
5.48336964453106));
#152530=CARTESIAN_POINT('Ctrl Pts',(-17.2409182958941,-21.0331845772146,
5.48754739925117));
#152531=CARTESIAN_POINT('Ctrl Pts',(-17.3099759681969,-21.0810402668187,
5.49172515397129));
#152532=CARTESIAN_POINT('Ctrl Pts',(-17.381296149795,-21.12542869532,5.4959029086914));
#152533=CARTESIAN_POINT('Ctrl Pts',(-17.4525395227181,-21.169769319451,
5.50007616415482));
#152534=CARTESIAN_POINT('Ctrl Pts',(-17.5260401732958,-21.2106498622978,
5.50424941961824));
#152535=CARTESIAN_POINT('Ctrl Pts',(-17.6014265224653,-21.2478391315563,
5.50842267508166));
#152536=CARTESIAN_POINT('Ctrl Pts',(-17.6767685965176,-21.2850065592045,
5.5125934795526));
#152537=CARTESIAN_POINT('Ctrl Pts',(-17.7539937588198,-21.3184868143506,
5.51676428402354));
#152538=CARTESIAN_POINT('Ctrl Pts',(-17.8327051091542,-21.3480942217983,
5.52093508849448));
#152539=CARTESIAN_POINT('Ctrl Pts',(-17.9113938433813,-21.3776931221591,
5.52510469456949));
#152540=CARTESIAN_POINT('Ctrl Pts',(-17.9915674871628,-21.4034212231907,
5.5292743006445));
#152541=CARTESIAN_POINT('Ctrl Pts',(-18.0728096721884,-21.425141190957,
5.53344390671952));
#152542=CARTESIAN_POINT('Ctrl Pts',(-18.154052884509,-21.446861433369,5.53761356551856));
#152543=CARTESIAN_POINT('Ctrl Pts',(-18.2363642201357,-21.4645733243011,
5.5417832243176));
#152544=CARTESIAN_POINT('Ctrl Pts',(-18.3193140098708,-21.4781899234995,
5.54595288311664));
#152545=CARTESIAN_POINT('Ctrl Pts',(-18.4023474046234,-21.4918202468558,
5.55012674451098));
#152546=CARTESIAN_POINT('Ctrl Pts',(-18.4860200839174,-21.5013469583618,
5.55430060590533));
#152547=CARTESIAN_POINT('Ctrl Pts',(-18.5698945442935,-21.5067347023531,
5.55847446729967));
#152548=CARTESIAN_POINT('Ctrl Pts',(-18.6538096081786,-21.5121250545438,
5.56265034925448));
#152549=CARTESIAN_POINT('Ctrl Pts',(-18.7379261871862,-21.5133724408922,
5.56682623120928));
#152550=CARTESIAN_POINT('Ctrl Pts',(-18.8218065112355,-21.5104937007123,
5.57100211316409));
#152551=CARTESIAN_POINT('Ctrl Pts',(-18.9058383997968,-21.5076097588972,
5.57518554057747));
#152552=CARTESIAN_POINT('Ctrl Pts',(-18.9896327207643,-21.5005848307498,
5.57936896799085));
#152553=CARTESIAN_POINT('Ctrl Pts',(-19.0727566144665,-21.4894877253211,
5.58355239540423));
#152554=CARTESIAN_POINT('Ctrl Pts',(-19.1534485520546,-21.4787152879535,
5.58761342826386));
#152555=CARTESIAN_POINT('Ctrl Pts',(-19.2335083856589,-21.4641058242612,
5.59167446112349));
#152556=CARTESIAN_POINT('Ctrl Pts',(-19.3125527301388,-21.4457675790757,
5.59573549398311));
#152557=CARTESIAN_POINT('Ctrl Pts',(-19.394002867067,-21.4268711913428,
5.59992012837616));
#152558=CARTESIAN_POINT('Ctrl Pts',(-19.4746778298126,-21.4039450190917,
5.60410476276921));
#152559=CARTESIAN_POINT('Ctrl Pts',(-19.55414895591,-21.3770681825713,5.60828939716226));
#152560=CARTESIAN_POINT('Ctrl Pts',(-19.6335069646958,-21.3502296019011,
5.61246807524619));
#152561=CARTESIAN_POINT('Ctrl Pts',(-19.7116641083501,-21.3194516726888,
5.61664675333013));
#152562=CARTESIAN_POINT('Ctrl Pts',(-19.7882032486923,-21.2848642288926,
5.62082543141407));
#152563=CARTESIAN_POINT('Ctrl Pts',(-19.8661142981176,-21.2496568300239,
5.62507900929951));
#152564=CARTESIAN_POINT('Ctrl Pts',(-19.9423482986083,-21.2105021111286,
5.62933258718494));
#152565=CARTESIAN_POINT('Ctrl Pts',(-20.0164828014232,-21.1675897327921,
5.63358616507038));
#152566=CARTESIAN_POINT('Ctrl Pts',(-20.0891800622393,-21.1255092946463,
5.63775727904833));
#152567=CARTESIAN_POINT('Ctrl Pts',(-20.1598580881698,-21.0798158370632,
5.64192839302628));
#152568=CARTESIAN_POINT('Ctrl Pts',(-20.2281415862033,-21.0307354137499,
5.64609950700423));
#152569=CARTESIAN_POINT('Ctrl Pts',(-20.2964021710496,-20.9816714598466,
5.6502692213246));
#152570=CARTESIAN_POINT('Ctrl Pts',(-20.3622694505379,-20.929223065652,
5.65443893564497));
#152571=CARTESIAN_POINT('Ctrl Pts',(-20.4253973801082,-20.8736594137784,
5.65860864996535));
#152572=CARTESIAN_POINT('Ctrl Pts',(-20.4885230633159,-20.8180977390979,
5.66277821590939));
#152573=CARTESIAN_POINT('Ctrl Pts',(-20.5489092456568,-20.7594213317294,
5.66694778185343));
#152574=CARTESIAN_POINT('Ctrl Pts',(-20.6062442778982,-20.69793853382,5.67111734779748));
#152575=CARTESIAN_POINT('Ctrl Pts',(-20.6655951391428,-20.6342940765833,
5.6754335105364));
#152576=CARTESIAN_POINT('Ctrl Pts',(-20.721675941672,-20.5676425973541,
5.67974967327532));
#152577=CARTESIAN_POINT('Ctrl Pts',(-20.7741852955293,-20.4983647564226,
5.68406583601424));
#152578=CARTESIAN_POINT('Ctrl Pts',(-20.8249841627078,-20.4313436338727,
5.68824140020592));
#152579=CARTESIAN_POINT('Ctrl Pts',(-20.8724404611871,-20.3618650450199,
5.69241696439761));
#152580=CARTESIAN_POINT('Ctrl Pts',(-20.9163256700509,-20.2903029066086,
5.69659252858929));
#152581=CARTESIAN_POINT('Ctrl Pts',(-20.9624274164872,-20.2151263347089,
5.70097899060183));
#152582=CARTESIAN_POINT('Ctrl Pts',(-21.0045875620258,-20.1376507144178,
5.70536545261437));
#152583=CARTESIAN_POINT('Ctrl Pts',(-21.0425969786766,-20.0583362915702,
5.70975191462691));
#152584=CARTESIAN_POINT('Ctrl Pts',(-21.0806063953274,-19.9790218687226,
5.71413837663946));
#152585=CARTESIAN_POINT('Ctrl Pts',(-21.1144649298774,-19.897869208087,
5.718524838652));
#152586=CARTESIAN_POINT('Ctrl Pts',(-21.144023506431,-19.8153578044185,
5.72291130066454));
#152587=CARTESIAN_POINT('Ctrl Pts',(-21.1768030234138,-19.7238552940413,
5.72777574688623));
#152588=CARTESIAN_POINT('Ctrl Pts',(-21.2043967060823,-19.6304025057852,
5.73264019310792));
#152589=CARTESIAN_POINT('Ctrl Pts',(-21.2266026211961,-19.5355513454757,
5.7375046393296));
#152590=CARTESIAN_POINT('Ctrl Pts',(-21.2488226674987,-19.4406398246877,
5.74237218114127));
#152591=CARTESIAN_POINT('Ctrl Pts',(-21.2656479288596,-19.3443282665163,
5.74723972295294));
#152592=CARTESIAN_POINT('Ctrl Pts',(-21.2769239065511,-19.2471914725919,
5.75210726476461));
#152593=CARTESIAN_POINT('Ctrl Pts',(-21.2881998842426,-19.1500546786674,
5.75697480657628));
#152594=CARTESIAN_POINT('Ctrl Pts',(-21.2939263955806,-19.0520927805187,
5.76184234838795));
#152595=CARTESIAN_POINT('Ctrl Pts',(-21.2939992944986,-18.9539005700933,
5.76670989019962));
#152596=CARTESIAN_POINT('Ctrl Pts',(-21.293999294499,-18.9539005695104,
5.76670989022851));
#152597=CARTESIAN_POINT('Ctrl Pts',(-21.2940618231948,-18.8696766480678,
5.77088500205647));
#152598=CARTESIAN_POINT('Ctrl Pts',(-21.2899635861128,-18.7854119279347,
5.77506011388444));
#152599=CARTESIAN_POINT('Ctrl Pts',(-21.2817191504239,-18.7015461508316,
5.7792352257124));
#152600=CARTESIAN_POINT('Ctrl Pts',(-21.2734754980237,-18.6176883416611,
5.78340994087069));
#152601=CARTESIAN_POINT('Ctrl Pts',(-21.2610864747303,-18.5342298557722,
5.78758465602898));
#152602=CARTESIAN_POINT('Ctrl Pts',(-21.2446185572459,-18.4516056954637,
5.79175937118727));
#152603=CARTESIAN_POINT('Ctrl Pts',(-21.2281473245846,-18.3689649019827,
5.79593492676267));
#152604=CARTESIAN_POINT('Ctrl Pts',(-21.2075956572652,-18.2871592164316,
5.80011048233806));
#152605=CARTESIAN_POINT('Ctrl Pts',(-21.1830809475489,-18.2066125085882,
5.80428603791345));
#152606=CARTESIAN_POINT('Ctrl Pts',(-21.1585369190254,-18.1259694694636,
5.8084665873195));
#152607=CARTESIAN_POINT('Ctrl Pts',(-21.1300205198882,-18.0465888526481,
5.81264713672554));
#152608=CARTESIAN_POINT('Ctrl Pts',(-21.0976986239761,-17.9688780263805,
5.81682768613158));
#152609=CARTESIAN_POINT('Ctrl Pts',(-21.065355928357,-17.8911171918331,
5.8210109257945));
#152610=CARTESIAN_POINT('Ctrl Pts',(-21.0292030575735,-17.8150287001824,
5.82519416545742));
#152611=CARTESIAN_POINT('Ctrl Pts',(-20.9894534545794,-17.740996402059,
5.82937740512034));
#152612=CARTESIAN_POINT('Ctrl Pts',(-20.949632004209,-17.6668302906149,
5.83356820598567));
#152613=CARTESIAN_POINT('Ctrl Pts',(-20.9062010761476,-17.5947281861657,
5.83775900685099));
#152614=CARTESIAN_POINT('Ctrl Pts',(-20.859418003607,-17.5250457926257,
5.84194980771632));
#152615=CARTESIAN_POINT('Ctrl Pts',(-20.8291383592866,-17.4799449051208,
5.84466224092621));
#152616=CARTESIAN_POINT('Ctrl Pts',(-20.7974553185201,-17.435857034571,
5.84737467413609));
#152617=CARTESIAN_POINT('Ctrl Pts',(-20.7644472985012,-17.392870830236,
5.85008710734598));
#152618=CARTESIAN_POINT('Ctrl Pts',(-20.7135238341689,-17.3265534188316,
5.85427174173903));
#152619=CARTESIAN_POINT('Ctrl Pts',(-20.6592531496868,-17.262610070515,
5.85845637613208));
#152620=CARTESIAN_POINT('Ctrl Pts',(-20.6018847443059,-17.2013982228989,
5.86264101052513));
#152621=CARTESIAN_POINT('Ctrl Pts',(-20.5445979957492,-17.1402735027715,
5.86681968860907));
#152622=CARTESIAN_POINT('Ctrl Pts',(-20.4842225962896,-17.0818728934348,
5.87099836669301));
#152623=CARTESIAN_POINT('Ctrl Pts',(-20.4210494366143,-17.0265223453856,
5.87517704477696));
#152624=CARTESIAN_POINT('Ctrl Pts',(-20.3567439434536,-16.9701796785424,
5.87943062266239));
#152625=CARTESIAN_POINT('Ctrl Pts',(-20.2895396974699,-16.9169978755988,
5.88368420054783));
#152626=CARTESIAN_POINT('Ctrl Pts',(-20.2197842460678,-16.867282951061,
5.88793777843326));
#152627=CARTESIAN_POINT('Ctrl Pts',(-20.1513811402077,-16.8185318473461,
5.89210889241121));
#152628=CARTESIAN_POINT('Ctrl Pts',(-20.0805252582504,-16.7731146765032,
5.89628000638917));
#152629=CARTESIAN_POINT('Ctrl Pts',(-20.0075777510545,-16.7312794610715,
5.90045112036712));
#152630=CARTESIAN_POINT('Ctrl Pts',(-19.9346547220991,-16.6894582838504,
5.90462083468749));
#152631=CARTESIAN_POINT('Ctrl Pts',(-19.8596418605523,-16.6512169036013,
5.90879054900787));
#152632=CARTESIAN_POINT('Ctrl Pts',(-19.7829274662086,-16.6167588624227,
5.91296026332824));
#152633=CARTESIAN_POINT('Ctrl Pts',(-19.7062158016923,-16.5823020474091,
5.91712982927229));
#152634=CARTESIAN_POINT('Ctrl Pts',(-19.6278031447566,-16.5516284915072,
5.92129939521634));
#152635=CARTESIAN_POINT('Ctrl Pts',(-19.5480992,-16.5248942147983,5.92546896116038));
#152636=CARTESIAN_POINT('Ctrl Pts',(-19.4655929628713,-16.4972199939008,
5.9297851238993));
#152637=CARTESIAN_POINT('Ctrl Pts',(-19.3817034451241,-16.4737673840696,
5.93410128663822));
#152638=CARTESIAN_POINT('Ctrl Pts',(-19.2969019322694,-16.4546531248848,
5.93841744937714));
#152639=CARTESIAN_POINT('Ctrl Pts',(-19.2148628197764,-16.4361615106825,
5.94259301356882));
#152640=CARTESIAN_POINT('Ctrl Pts',(-19.1319706883696,-16.4217299783601,
5.9467685777605));
#152641=CARTESIAN_POINT('Ctrl Pts',(-19.0486605152116,-16.411411729507,
5.95094414195218));
#152642=CARTESIAN_POINT('Ctrl Pts',(-18.9611425432585,-16.4005723304336,
5.95533060396472));
#152643=CARTESIAN_POINT('Ctrl Pts',(-18.873163771528,-16.3942727005953,
5.95971706597726));
#152644=CARTESIAN_POINT('Ctrl Pts',(-18.7852297301449,-16.3925126461048,
5.9641035279898));
#152645=CARTESIAN_POINT('Ctrl Pts',(-18.6972956887618,-16.3907525916143,
5.96848999000234));
#152646=CARTESIAN_POINT('Ctrl Pts',(-18.609406955249,-16.3935320181048,
5.97287645201488));
#152647=CARTESIAN_POINT('Ctrl Pts',(-18.5220617179687,-16.4007880988421,
5.97726291402742));
#152648=CARTESIAN_POINT('Ctrl Pts',(-18.4387353645322,-16.4077103165486,
5.98144754842047));
#152649=CARTESIAN_POINT('Ctrl Pts',(-18.3555934356669,-16.4187320520138,
5.98563218281352));
#152650=CARTESIAN_POINT('Ctrl Pts',(-18.2730715290517,-16.4338369900522,
5.98981681720658));
#152651=CARTESIAN_POINT('Ctrl Pts',(-18.1906670821564,-16.4489204280809,
5.99399549529053));
#152652=CARTESIAN_POINT('Ctrl Pts',(-18.1088813531835,-16.4680754422336,
5.99817417337448));
#152653=CARTESIAN_POINT('Ctrl Pts',(-18.0281458685296,-16.4912338702985,
6.00235285145843));
#152654=CARTESIAN_POINT('Ctrl Pts',(-17.9459632583371,-16.5148073965427,
6.00660642934386));
#152655=CARTESIAN_POINT('Ctrl Pts',(-17.8648693945427,-16.5425292308518,
6.0108600072293));
#152656=CARTESIAN_POINT('Ctrl Pts',(-17.7853097077367,-16.5742727807073,
6.01511358511473));
#152657=CARTESIAN_POINT('Ctrl Pts',(-17.7072924407073,-16.6054009199064,
6.01928469909268));
#152658=CARTESIAN_POINT('Ctrl Pts',(-17.6307508424361,-16.6403960502736,
6.02345581307064));
#152659=CARTESIAN_POINT('Ctrl Pts',(-17.5560889447382,-16.6790887509865,
6.02762692704859));
#152660=CARTESIAN_POINT('Ctrl Pts',(-17.4814521005611,-16.7177684679901,
6.03179664136896));
#152661=CARTESIAN_POINT('Ctrl Pts',(-17.4086941123775,-16.7601430796846,
6.03596635568934));
#152662=CARTESIAN_POINT('Ctrl Pts',(-17.3381963061949,-16.80599626087,6.04013607000971));
#152663=CARTESIAN_POINT('Ctrl Pts',(-17.2677010086269,-16.8518478104023,
6.04430563595375));
#152664=CARTESIAN_POINT('Ctrl Pts',(-17.1994661183233,-16.9011774317735,
6.04847520189779));
#152665=CARTESIAN_POINT('Ctrl Pts',(-17.1338445888104,-16.9537250789642,
6.05264476784183));
#152666=CARTESIAN_POINT('Ctrl Pts',(-17.0659158872728,-17.0081202366055,
6.05696093058075));
#152667=CARTESIAN_POINT('Ctrl Pts',(-17.0007881489948,-17.0659635923392,
6.06127709331967));
#152668=CARTESIAN_POINT('Ctrl Pts',(-16.9388146313972,-17.1269220585535,
6.06559325605858));
#152669=CARTESIAN_POINT('Ctrl Pts',(-16.8788598946168,-17.1858948091426,
6.06976882025026));
#152670=CARTESIAN_POINT('Ctrl Pts',(-16.8218573212163,-17.2477824589611,
6.07394438444195));
#152671=CARTESIAN_POINT('Ctrl Pts',(-16.7680870902011,-17.3122480580631,
6.07811994863363));
#152672=CARTESIAN_POINT('Ctrl Pts',(-16.7116010526439,-17.3799696613233,
6.08250641064616));
#152673=CARTESIAN_POINT('Ctrl Pts',(-16.6586828203997,-17.4505360152566,
6.0868928726587));
#152674=CARTESIAN_POINT('Ctrl Pts',(-16.6096058643082,-17.5235219440824,
6.09127933467124));
#152675=CARTESIAN_POINT('Ctrl Pts',(-16.5605289082167,-17.5965078729081,
6.09566579668377));
#152676=CARTESIAN_POINT('Ctrl Pts',(-16.5152934615326,-17.671912839942,
6.10005225869631));
#152677=CARTESIAN_POINT('Ctrl Pts',(-16.4741163568267,-17.7492839406919,
6.10443872070885));
#152678=CARTESIAN_POINT('Ctrl Pts',(-16.4348338717473,-17.8230950824048,
6.10862335510189));
#152679=CARTESIAN_POINT('Ctrl Pts',(-16.3990982578627,-17.8989701434485,
6.11280798949494));
#152680=CARTESIAN_POINT('Ctrl Pts',(-16.3671315774458,-17.9765340240092,
6.11699262388799));
#152681=CARTESIAN_POINT('Ctrl Pts',(-16.3352103976416,-18.0539875019866,
6.12117130197194));
#152682=CARTESIAN_POINT('Ctrl Pts',(-16.3070476692933,-18.1331246030379,
6.12534998005589));
#152683=CARTESIAN_POINT('Ctrl Pts',(-16.2828196558216,-18.2135455868414,
6.12952865813984));
#152684=CARTESIAN_POINT('Ctrl Pts',(-16.2581573726208,-18.295408058982,
6.13378223602527));
#152685=CARTESIAN_POINT('Ctrl Pts',(-16.2375724777942,-18.3786004681764,
6.13803581391071));
#152686=CARTESIAN_POINT('Ctrl Pts',(-16.2211996301977,-18.4626797556595,
6.14228939179614));
#152687=CARTESIAN_POINT('Ctrl Pts',(-16.2051442022008,-18.5451290020876,
6.14646050577409));
#152688=CARTESIAN_POINT('Ctrl Pts',(-16.1931390533221,-18.6284305735957,
6.15063161975204));
#152689=CARTESIAN_POINT('Ctrl Pts',(-16.1852604222201,-18.712153039089,
6.15480273372999));
#152690=CARTESIAN_POINT('Ctrl Pts',(-16.1773844348688,-18.7958474107003,
6.15897244805036));
#152691=CARTESIAN_POINT('Ctrl Pts',(-16.1736322583368,-18.8799619381736,
6.16314216237073));
#152692=CARTESIAN_POINT('Ctrl Pts',(-16.1740284019004,-18.9640588939546,
6.1673118766911));
#152693=CARTESIAN_POINT('Ctrl Pts',(-16.1744245313676,-19.0481528572052,
6.17148144263515));
#152694=CARTESIAN_POINT('Ctrl Pts',(-16.1789686844146,-19.1322287899831,
6.1756510085792));
#152695=CARTESIAN_POINT('Ctrl Pts',(-16.1876332505419,-19.2158491562507,
6.17982057452325));
#152696=CARTESIAN_POINT('Ctrl Pts',(-16.1966024521254,-19.3024095114393,
6.18413673726217));
#152697=CARTESIAN_POINT('Ctrl Pts',(-16.2099871509033,-19.3884811440158,
6.18845290000109));
#152698=CARTESIAN_POINT('Ctrl Pts',(-16.2276984844482,-19.4735867263867,
6.19276906274001));
#152699=CARTESIAN_POINT('Ctrl Pts',(-16.2448328731658,-19.5559200033635,
6.19694462693169));
#152700=CARTESIAN_POINT('Ctrl Pts',(-16.2660161808878,-19.6373487577952,
6.20112019112337));
#152701=CARTESIAN_POINT('Ctrl Pts',(-16.2911167416149,-19.7174550188626,
6.20529575531506));
#152702=CARTESIAN_POINT('Ctrl Pts',(-16.3174850719935,-19.8016072567419,
6.2096822173276));
#152703=CARTESIAN_POINT('Ctrl Pts',(-16.3481765728436,-19.8842993445549,
6.21406867934013));
#152704=CARTESIAN_POINT('Ctrl Pts',(-16.3829817631982,-19.965071197017,
6.21845514135267));
#152705=CARTESIAN_POINT('Ctrl Pts',(-16.4177869535528,-20.045843049479,
6.22284160336521));
#152706=CARTESIAN_POINT('Ctrl Pts',(-16.4567055084016,-20.1246941799628,
6.22722806537775));
#152707=CARTESIAN_POINT('Ctrl Pts',(-16.4994739740983,-20.2011971179794,
6.23161452739029));
#152708=CARTESIAN_POINT('Ctrl Pts',(-16.5415036429151,-20.27637851848,6.23592521618075));
#152709=CARTESIAN_POINT('Ctrl Pts',(-16.5874123872811,-20.3495805439044,
6.24023590497122));
#152710=CARTESIAN_POINT('Ctrl Pts',(-16.6369860440941,-20.4203774953111,
6.24454659376168));
#152711=CARTESIAN_POINT('Ctrl Pts',(-16.6850336766682,-20.4889951065029,
6.24872458676161));
#152712=CARTESIAN_POINT('Ctrl Pts',(-16.7365236132887,-20.5553531244434,
6.25290257976153));
#152713=CARTESIAN_POINT('Ctrl Pts',(-16.7912139159174,-20.619087949538,
6.25708057276145));
#152714=CARTESIAN_POINT('Ctrl Pts',(-16.8485097182233,-20.6858591642344,
6.26145760944719));
#152715=CARTESIAN_POINT('Ctrl Pts',(-16.9093181745504,-20.7497505671933,
6.26583464613292));
#152716=CARTESIAN_POINT('Ctrl Pts',(-16.973310673513,-20.8103791581899,
6.27021168281866));
#152717=CARTESIAN_POINT('Ctrl Pts',(-17.0373031724756,-20.8710077491866,
6.27458871950439));
#152718=CARTESIAN_POINT('Ctrl Pts',(-17.1044793276203,-20.9283730896681,
6.27896575619013));
#152719=CARTESIAN_POINT('Ctrl Pts',(-17.1744641402401,-20.9821349467765,
6.28334279287586));
#152720=CARTESIAN_POINT('Origin',(-18.734,-18.952,-1.76670989022851));
#152721=CARTESIAN_POINT('',(-17.1744641402401,-20.9821349467765,7.14996297217343));
#152722=CARTESIAN_POINT('',(-17.1744641402401,-20.9821349467765,7.08324141939143));
#152723=CARTESIAN_POINT('',(-17.1744641402401,-20.9821349467765,-1.76670989022851));
#152724=CARTESIAN_POINT('',(-21.2939991231355,-18.954118854712,6.6332901097715));
#152725=CARTESIAN_POINT('Ctrl Pts',(-21.2939991231355,-18.954118854712,
6.6332901097715));
#152726=CARTESIAN_POINT('Ctrl Pts',(-21.2940674480299,-18.8715687540988,
6.63740642252224));
#152727=CARTESIAN_POINT('Ctrl Pts',(-21.2901386830331,-18.788875859184,
6.64152273527298));
#152728=CARTESIAN_POINT('Ctrl Pts',(-21.2821979940262,-18.7064659224447,
6.64563904802373));
#152729=CARTESIAN_POINT('Ctrl Pts',(-21.2742662779566,-18.6241491085059,
6.64975070936244));
#152730=CARTESIAN_POINT('Ctrl Pts',(-21.2623316869624,-18.5421150878493,
6.65386237070115));
#152731=CARTESIAN_POINT('Ctrl Pts',(-21.2464314307689,-18.4607889397778,
6.65797403203986));
#152732=CARTESIAN_POINT('Ctrl Pts',(-21.2305407999848,-18.3795120234587,
6.66208320433541));
#152733=CARTESIAN_POINT('Ctrl Pts',(-21.2106893569247,-18.2989425946371,
6.66619237663095));
#152734=CARTESIAN_POINT('Ctrl Pts',(-21.1869659077107,-18.2194986309849,
6.6703015489265));
#152735=CARTESIAN_POINT('Ctrl Pts',(-21.1632492097462,-18.1400772755973,
6.67440955182855));
#152736=CARTESIAN_POINT('Ctrl Pts',(-21.1356628286737,-18.0617812045221,
6.67851755473059));
#152737=CARTESIAN_POINT('Ctrl Pts',(-21.1043458531986,-17.9850147176796,
6.68262555763264));
#152738=CARTESIAN_POINT('Ctrl Pts',(-21.0730277445932,-17.9082454532244,
6.686733709173));
#152739=CARTESIAN_POINT('Ctrl Pts',(-21.0379789552763,-17.8330063217982,
6.69084186071337));
#152740=CARTESIAN_POINT('Ctrl Pts',(-20.9993866849094,-17.7596815996408,
6.69495001225373));
#152741=CARTESIAN_POINT('Ctrl Pts',(-20.9607561733792,-17.6862842198592,
6.69906223457025));
#152742=CARTESIAN_POINT('Ctrl Pts',(-20.9185753946451,-17.6148054564872,
6.70317445688677));
#152743=CARTESIAN_POINT('Ctrl Pts',(-20.8730771242598,-17.5456042319217,
6.70728667920329));
#152744=CARTESIAN_POINT('Ctrl Pts',(-20.8275541489319,-17.4763654320317,
6.71140113440064));
#152745=CARTESIAN_POINT('Ctrl Pts',(-20.7787103793543,-17.4094070139061,
6.715515589598));
#152746=CARTESIAN_POINT('Ctrl Pts',(-20.7268199445207,-17.3450561090317,
6.71963004479535));
#152747=CARTESIAN_POINT('Ctrl Pts',(-20.6748438133914,-17.2805989295771,
6.72375129495541));
#152748=CARTESIAN_POINT('Ctrl Pts',(-20.6198112918954,-17.2187582108668,
6.72787254511546));
#152749=CARTESIAN_POINT('Ctrl Pts',(-20.5620341095491,-17.1598249822283,
6.73199379527552));
#152750=CARTESIAN_POINT('Ctrl Pts',(-20.529745700387,-17.1268905239828,
6.73429692959298));
#152751=CARTESIAN_POINT('Ctrl Pts',(-20.4966007367167,-17.0948633881749,
6.73660006391043));
#152752=CARTESIAN_POINT('Ctrl Pts',(-20.4626578964191,-17.0637887096122,
6.73890319822789));
#152753=CARTESIAN_POINT('Ctrl Pts',(-20.400986123379,-17.0073281863674,
6.74308783262094));
#152754=CARTESIAN_POINT('Ctrl Pts',(-20.3364305466714,-16.9537872066972,
6.74727246701399));
#152755=CARTESIAN_POINT('Ctrl Pts',(-20.2692989765721,-16.9034744198481,
6.75145710140703));
#152756=CARTESIAN_POINT('Ctrl Pts',(-20.2022629599536,-16.8532332470236,
6.75563577949098));
#152757=CARTESIAN_POINT('Ctrl Pts',(-20.1326585979523,-16.8062114135715,
6.75981445757492));
#152758=CARTESIAN_POINT('Ctrl Pts',(-20.0608289916761,-16.7626793686516,
6.76399313565886));
#152759=CARTESIAN_POINT('Ctrl Pts',(-19.9877118913304,-16.7183670431124,
6.7682467135443));
#152760=CARTESIAN_POINT('Ctrl Pts',(-19.9122893426568,-16.6776711711576,
6.77250029142973));
#152761=CARTESIAN_POINT('Ctrl Pts',(-19.8349567777298,-16.6408327248832,
6.77675386931517));
#152762=CARTESIAN_POINT('Ctrl Pts',(-19.7591234554761,-16.6047084637741,
6.78092498329312));
#152763=CARTESIAN_POINT('Ctrl Pts',(-19.6814539493098,-16.5722936025649,
6.78509609727107));
#152764=CARTESIAN_POINT('Ctrl Pts',(-19.6023470115176,-16.5437696398416,
6.78926721124902));
#152765=CARTESIAN_POINT('Ctrl Pts',(-19.5232666188221,-16.5152552486095,
6.7934369255694));
#152766=CARTESIAN_POINT('Ctrl Pts',(-19.4427501848433,-16.4906293187766,
6.79760663988977));
#152767=CARTESIAN_POINT('Ctrl Pts',(-19.3612154692012,-16.4700248278448,
6.80177635421015));
#152768=CARTESIAN_POINT('Ctrl Pts',(-19.2796836549143,-16.4494210701093,
6.8059459201542));
#152769=CARTESIAN_POINT('Ctrl Pts',(-19.1971340772289,-16.4328385786397,
6.81011548609824));
#152770=CARTESIAN_POINT('Ctrl Pts',(-19.1139973178551,-16.4203598126071,
6.81428505204228));
#152771=CARTESIAN_POINT('Ctrl Pts',(-19.0279375725819,-16.407442308555,
6.8186012147812));
#152772=CARTESIAN_POINT('Ctrl Pts',(-18.9412491083339,-16.3989225513938,
6.82291737752012));
#152773=CARTESIAN_POINT('Ctrl Pts',(-18.8544163259003,-16.3948336173693,
6.82723354025904));
#152774=CARTESIAN_POINT('Ctrl Pts',(-18.7704121122212,-16.3908778799405,
6.83140910445072));
#152775=CARTESIAN_POINT('Ctrl Pts',(-18.6862733092299,-16.3910686822566,
6.8355846686424));
#152776=CARTESIAN_POINT('Ctrl Pts',(-18.6024375216844,-16.3953828377523,
6.83976023283408));
#152777=CARTESIAN_POINT('Ctrl Pts',(-18.5143673878107,-16.3999148909862,
6.84414669484662));
#152778=CARTESIAN_POINT('Ctrl Pts',(-18.4266322652435,-16.4089977253143,
6.84853315685916));
#152779=CARTESIAN_POINT('Ctrl Pts',(-18.3397299608672,-16.4225433120446,
6.8529196188717));
#152780=CARTESIAN_POINT('Ctrl Pts',(-18.252827656491,-16.4360888987749,
6.85730608088424));
#152781=CARTESIAN_POINT('Ctrl Pts',(-18.1667587226473,-16.4540970446291,
6.86169254289678));
#152782=CARTESIAN_POINT('Ctrl Pts',(-18.0820028534405,-16.4764193164273,
6.86607900490932));
#152783=CARTESIAN_POINT('Ctrl Pts',(-18.0011467274143,-16.4977145074105,
6.87026363930236));
#152784=CARTESIAN_POINT('Ctrl Pts',(-17.921184527277,-16.5230148144695,
6.87444827369541));
#152785=CARTESIAN_POINT('Ctrl Pts',(-17.8425423900642,-16.5522284838578,
6.87863290808845));
#152786=CARTESIAN_POINT('Ctrl Pts',(-17.7640121901998,-16.5814005712036,
6.88281158617239));
#152787=CARTESIAN_POINT('Ctrl Pts',(-17.6867987486329,-16.6144747979096,
6.88699026425634));
#152788=CARTESIAN_POINT('Ctrl Pts',(-17.6113151844297,-16.6513090592416,
6.89116894234028));
#152789=CARTESIAN_POINT('Ctrl Pts',(-17.5344786315872,-16.6888035482357,
6.89542252022572));
#152790=CARTESIAN_POINT('Ctrl Pts',(-17.4594350484393,-16.7301940721622,
6.89967609811116));
#152791=CARTESIAN_POINT('Ctrl Pts',(-17.3866010942662,-16.7752785688501,
6.90392967599659));
#152792=CARTESIAN_POINT('Ctrl Pts',(-17.3151791684184,-16.8194890145946,
6.90810078997454));
#152793=CARTESIAN_POINT('Ctrl Pts',(-17.2458823693353,-16.8672512282385,
6.9122719039525));
#152794=CARTESIAN_POINT('Ctrl Pts',(-17.1790791456547,-16.9183281639551,
6.91644301793045));
#152795=CARTESIAN_POINT('Ctrl Pts',(-17.112298338441,-16.9693879603127,
6.92061273225082));
#152796=CARTESIAN_POINT('Ctrl Pts',(-17.0480098099917,-17.0237599905361,
6.9247824465712));
#152797=CARTESIAN_POINT('Ctrl Pts',(-16.9865514987007,-17.0811649630962,
6.92895216089157));
#152798=CARTESIAN_POINT('Ctrl Pts',(-16.92509537436,-17.1385678929411,6.93312172683562));
#152799=CARTESIAN_POINT('Ctrl Pts',(-16.8664696025457,-17.1990032359,6.93729129277967));
#152800=CARTESIAN_POINT('Ctrl Pts',(-16.8109765840841,-17.2621535744811,
6.94146085872371));
#152801=CARTESIAN_POINT('Ctrl Pts',(-16.7535324995514,-17.3275242010623,
6.94577702146263));
#152802=CARTESIAN_POINT('Ctrl Pts',(-16.699445910539,-17.3958038977866,
6.95009318420155));
#152803=CARTESIAN_POINT('Ctrl Pts',(-16.6490068258948,-17.4666032637929,
6.95440934694047));
#152804=CARTESIAN_POINT('Ctrl Pts',(-16.6002107891277,-17.5350963478982,
6.95858491113215));
#152805=CARTESIAN_POINT('Ctrl Pts',(-16.5548284854398,-17.6059470436345,
6.96276047532383));
#152806=CARTESIAN_POINT('Ctrl Pts',(-16.5130772857549,-17.6787748442046,
6.96693603951551));
#152807=CARTESIAN_POINT('Ctrl Pts',(-16.469217332228,-17.7552810038499,
6.97132250152805));
#152808=CARTESIAN_POINT('Ctrl Pts',(-16.4293652006908,-17.833968723497,
6.97570896354059));
#152809=CARTESIAN_POINT('Ctrl Pts',(-16.3937163263691,-17.9143717780744,
6.98009542555314));
#152810=CARTESIAN_POINT('Ctrl Pts',(-16.3580674520473,-17.9947748326518,
6.98448188756568));
#152811=CARTESIAN_POINT('Ctrl Pts',(-16.3266219713967,-18.0768926531097,
6.98886834957822));
#152812=CARTESIAN_POINT('Ctrl Pts',(-16.2995147249234,-18.1602415485545,
6.99325481159076));
#152813=CARTESIAN_POINT('Ctrl Pts',(-16.273654723043,-18.2397554377671,
6.99743944598381));
#152814=CARTESIAN_POINT('Ctrl Pts',(-16.251646255088,-18.3206855701428,
7.00162408037685));
#152815=CARTESIAN_POINT('Ctrl Pts',(-16.233642830573,-18.4026239673095,
7.00580871476989));
#152816=CARTESIAN_POINT('Ctrl Pts',(-16.2156650317043,-18.4844457353099,
7.00998739285384));
#152817=CARTESIAN_POINT('Ctrl Pts',(-16.2016810508027,-18.5672724719893,
7.01416607093779));
#152818=CARTESIAN_POINT('Ctrl Pts',(-16.1917950137905,-18.6506798909933,
7.01834474902174));
#152819=CARTESIAN_POINT('Ctrl Pts',(-16.1817317766699,-18.7355823280391,
7.02259832690717));
#152820=CARTESIAN_POINT('Ctrl Pts',(-16.1759149888559,-18.8210860111299,
7.02685190479261));
#152821=CARTESIAN_POINT('Ctrl Pts',(-16.1744002778054,-18.9067312233285,
7.03110548267805));
#152822=CARTESIAN_POINT('Ctrl Pts',(-16.1729149323844,-18.9907160359657,
7.035276596656));
#152823=CARTESIAN_POINT('Ctrl Pts',(-16.1755663524988,-19.0748364579018,
7.03944771063395));
#152824=CARTESIAN_POINT('Ctrl Pts',(-16.1823546543812,-19.1586543737305,
7.0436188246119));
#152825=CARTESIAN_POINT('Ctrl Pts',(-16.1891406783834,-19.2424441636481,
7.04778853893228));
#152826=CARTESIAN_POINT('Ctrl Pts',(-16.2000607901197,-19.3259311909065,
7.05195825325265));
#152827=CARTESIAN_POINT('Ctrl Pts',(-16.2150630692561,-19.408680127589,
7.05612796757302));
#152828=CARTESIAN_POINT('Ctrl Pts',(-16.2300648145471,-19.4914261197094,
7.06029753351707));
#152829=CARTESIAN_POINT('Ctrl Pts',(-16.2491483555178,-19.5734336209725,
7.06446709946112));
#152830=CARTESIAN_POINT('Ctrl Pts',(-16.2722104781218,-19.6542765480713,
7.06863666540517));
#152831=CARTESIAN_POINT('Ctrl Pts',(-16.2960834365064,-19.7379618127562,
7.07295282814409));
#152832=CARTESIAN_POINT('Ctrl Pts',(-16.3242198111562,-19.8203985795373,
7.07726899088301));
#152833=CARTESIAN_POINT('Ctrl Pts',(-16.3564491538598,-19.9011322215678,
7.08158515362193));
#152834=CARTESIAN_POINT('Ctrl Pts',(-16.3876286291149,-19.9792359737009,
7.08576071781361));
#152835=CARTESIAN_POINT('Ctrl Pts',(-16.4226382716206,-20.0557454470094,
7.08993628200529));
#152836=CARTESIAN_POINT('Ctrl Pts',(-16.4612757941355,-20.1302719058339,
7.09411184619697));
#152837=CARTESIAN_POINT('Ctrl Pts',(-16.5018648060606,-20.2085625189238,
7.0984983082095));
#152838=CARTESIAN_POINT('Ctrl Pts',(-16.5464575227366,-20.2846640250243,
7.10288477022204));
#152839=CARTESIAN_POINT('Ctrl Pts',(-16.5947677080408,-20.3581597352503,
7.10727123223458));
#152840=CARTESIAN_POINT('Ctrl Pts',(-16.6430778933451,-20.4316554454763,
7.11165769424711));
#152841=CARTESIAN_POINT('Ctrl Pts',(-16.6951051426579,-20.5025449370744,
7.11604415625965));
#152842=CARTESIAN_POINT('Ctrl Pts',(-16.7505157350918,-20.5704530178111,
7.12043061827219));
#152843=CARTESIAN_POINT('Ctrl Pts',(-16.8033793819778,-20.6352397064761,
7.12461545674303));
#152844=CARTESIAN_POINT('Ctrl Pts',(-16.8595189473533,-20.6975542088439,
7.12880029521386));
#152845=CARTESIAN_POINT('Ctrl Pts',(-16.9186744386697,-20.7570465662638,
7.1329851336847));
#152846=CARTESIAN_POINT('Ctrl Pts',(-16.9777385242717,-20.8164469974515,
7.13716350583869));
#152847=CARTESIAN_POINT('Ctrl Pts',(-17.0398089529806,-20.8730336264076,
7.14134187799268));
#152848=CARTESIAN_POINT('Ctrl Pts',(-17.1045853939782,-20.9264893116152,
7.14552025014667));
#152849=CARTESIAN_POINT('Ctrl Pts',(-17.127543594814,-20.9454351866573,
7.14700115748892));
#152850=CARTESIAN_POINT('Ctrl Pts',(-17.1508413505485,-20.9639880803871,
7.14848206483117));
#152851=CARTESIAN_POINT('Ctrl Pts',(-17.1744641402401,-20.9821349467765,
7.14996297217343));
#152852=CARTESIAN_POINT('Ctrl Pts',(-17.1721129507126,-20.9851649608899,
6.34984101818205));
#152853=CARTESIAN_POINT('Ctrl Pts',(-17.2118400414908,-21.015998077639,
6.35235260484923));
#152854=CARTESIAN_POINT('Ctrl Pts',(-17.9391679507452,-21.5446793877424,
6.39725612707689));
#152855=CARTESIAN_POINT('Ctrl Pts',(-19.9200692482785,-21.7370548823945,
6.48455158486502));
#152856=CARTESIAN_POINT('Ctrl Pts',(-21.2201491927466,-20.0919179991473,
6.57652302872766));
#152857=CARTESIAN_POINT('Ctrl Pts',(-21.2969228070761,-19.0983559330699,
6.62610253702982));
#152858=CARTESIAN_POINT('Ctrl Pts',(-21.2956373923518,-18.9541202106712,
6.6332901097715));
#152859=CARTESIAN_POINT('',(-21.293999428374,-18.9502892327451,6.5667098902584));
#152860=CARTESIAN_POINT('Ctrl Pts',(-17.1744641402401,-20.9821349467765,
6.28334279287586));
#152861=CARTESIAN_POINT('Ctrl Pts',(-17.2411328275767,-21.0333493789942,
6.28751243024914));
#152862=CARTESIAN_POINT('Ctrl Pts',(-17.3103496505638,-21.0812937513021,
6.29168206762242));
#152863=CARTESIAN_POINT('Ctrl Pts',(-17.3817564935579,-21.1257151375664,
6.2958517049957));
#152864=CARTESIAN_POINT('Ctrl Pts',(-17.4531631314398,-21.1701363962327,
6.30002133039193));
#152865=CARTESIAN_POINT('Ctrl Pts',(-17.5267593855407,-21.2110344470256,
6.30419095578816));
#152866=CARTESIAN_POINT('Ctrl Pts',(-17.6021596903972,-21.2482006692705,
6.30836058118439));
#152867=CARTESIAN_POINT('Ctrl Pts',(-17.6781541019692,-21.285659737841,
6.31256306059166));
#152868=CARTESIAN_POINT('Ctrl Pts',(-17.7559807011725,-21.319327685251,
6.31676553999894));
#152869=CARTESIAN_POINT('Ctrl Pts',(-17.8352228079875,-21.3490397491736,
6.32096801940622));
#152870=CARTESIAN_POINT('Ctrl Pts',(-17.9139612308849,-21.3785629553113,
6.32514378673608));
#152871=CARTESIAN_POINT('Ctrl Pts',(-17.9940967580289,-21.4041803383333,
6.32931955406594));
#152872=CARTESIAN_POINT('Ctrl Pts',(-18.0752056469976,-21.4257805077355,
6.33349532139579));
#152873=CARTESIAN_POINT('Ctrl Pts',(-18.1570928073895,-21.4475879391874,
6.33771115684178));
#152874=CARTESIAN_POINT('Ctrl Pts',(-18.2399716399031,-21.4653005516914,
6.34192699228777));
#152875=CARTESIAN_POINT('Ctrl Pts',(-18.3233977108253,-21.4788568934794,
6.34614282773376));
#152876=CARTESIAN_POINT('Ctrl Pts',(-18.4068237817474,-21.4924132352675,
6.35035866317974));
#152877=CARTESIAN_POINT('Ctrl Pts',(-18.4907966114,-21.5018133172571,6.35457449862573));
#152878=CARTESIAN_POINT('Ctrl Pts',(-18.5748705298082,-21.5070494734381,
6.35879033407172));
#152879=CARTESIAN_POINT('Ctrl Pts',(-18.6583222240302,-21.512246877256,
6.36297496846476));
#152880=CARTESIAN_POINT('Ctrl Pts',(-18.742184118471,-21.5133611702432,
6.36715960285781));
#152881=CARTESIAN_POINT('Ctrl Pts',(-18.8260228331339,-21.5103455197025,
6.37134423725085));
#152882=CARTESIAN_POINT('Ctrl Pts',(-18.9097422137639,-21.5073341615672,
6.3755229153348));
#152883=CARTESIAN_POINT('Ctrl Pts',(-18.993438024348,-21.5002045527773,
6.37970159341875));
#152884=CARTESIAN_POINT('Ctrl Pts',(-19.0766734176215,-21.4889617515555,
6.3838802715027));
#152885=CARTESIAN_POINT('Ctrl Pts',(-19.1614007454992,-21.4775174312018,
6.38813384938813));
#152886=CARTESIAN_POINT('Ctrl Pts',(-19.2456505065471,-21.4618109801083,
6.39238742727357));
#152887=CARTESIAN_POINT('Ctrl Pts',(-19.3289636478329,-21.4419032627308,
6.396641005159));
#152888=CARTESIAN_POINT('Ctrl Pts',(-19.4106616013027,-21.4223814953013,
6.40081211913695));
#152889=CARTESIAN_POINT('Ctrl Pts',(-19.4914584592903,-21.3988200192302,
6.4049832331149));
#152890=CARTESIAN_POINT('Ctrl Pts',(-19.5709299408016,-21.3713280625392,
6.40915434709285));
#152891=CARTESIAN_POINT('Ctrl Pts',(-19.6503747548898,-21.3438453310398,
6.41332406141322));
#152892=CARTESIAN_POINT('Ctrl Pts',(-19.7284946413759,-21.3124348885695,
6.41749377573359));
#152893=CARTESIAN_POINT('Ctrl Pts',(-19.8048810053293,-21.2772556574332,
6.42166349005396));
#152894=CARTESIAN_POINT('Ctrl Pts',(-19.8812646511281,-21.2420776781249,
6.425833055998));
#152895=CARTESIAN_POINT('Ctrl Pts',(-19.9559144795494,-21.2031313700067,
6.43000262194205));
#152896=CARTESIAN_POINT('Ctrl Pts',(-20.0284436491277,-21.1606230188135,
6.43417218788609));
#152897=CARTESIAN_POINT('Ctrl Pts',(-20.103522854834,-21.1166201264321,
6.43848835062501));
#152898=CARTESIAN_POINT('Ctrl Pts',(-20.176329047329,-21.068800314323,6.44280451336393));
#152899=CARTESIAN_POINT('Ctrl Pts',(-20.2464645244673,-21.0174420984932,
6.44712067610285));
#152900=CARTESIAN_POINT('Ctrl Pts',(-20.3143153458147,-20.9677568711422,
6.45129624029453));
#152901=CARTESIAN_POINT('Ctrl Pts',(-20.3796664407516,-20.9147605602811,
6.45547180448621));
#152902=CARTESIAN_POINT('Ctrl Pts',(-20.4421918593798,-20.8587460689742,
6.45964736867789));
#152903=CARTESIAN_POINT('Ctrl Pts',(-20.507875288263,-20.7999024188731,
6.46403383069043));
#152904=CARTESIAN_POINT('Ctrl Pts',(-20.5704396751017,-20.7377280904825,
6.46842029270298));
#152905=CARTESIAN_POINT('Ctrl Pts',(-20.6295529524491,-20.6726042556212,
6.47280675471552));
#152906=CARTESIAN_POINT('Ctrl Pts',(-20.6886662297964,-20.6074804207598,
6.47719321672807));
#152907=CARTESIAN_POINT('Ctrl Pts',(-20.7443280892574,-20.5394075767508,
6.48157967874061));
#152908=CARTESIAN_POINT('Ctrl Pts',(-20.7962584977303,-20.4688025212726,
6.48596614075316));
#152909=CARTESIAN_POINT('Ctrl Pts',(-20.8460908704135,-20.4010499743282,
6.49017538570612));
#152910=CARTESIAN_POINT('Ctrl Pts',(-20.8926734978047,-20.3307132360494,
6.49438463065908));
#152911=CARTESIAN_POINT('Ctrl Pts',(-20.9357293738869,-20.2581346654015,
6.49859387561203));
#152912=CARTESIAN_POINT('Ctrl Pts',(-20.978722858141,-20.1856612676154,
6.50279702099133));
#152913=CARTESIAN_POINT('Ctrl Pts',(-21.0181995127225,-20.1109528753409,
6.50700016637063));
#152914=CARTESIAN_POINT('Ctrl Pts',(-21.0539239335175,-20.0343829926107,
6.51120331174993));
#152915=CARTESIAN_POINT('Ctrl Pts',(-21.0896068791139,-19.9579020056841,
6.51540157737791));
#152916=CARTESIAN_POINT('Ctrl Pts',(-21.1215460556627,-19.8795642299174,
6.51959984300589));
#152917=CARTESIAN_POINT('Ctrl Pts',(-21.1495512259748,-19.7997689984256,
6.52379810863387));
#152918=CARTESIAN_POINT('Ctrl Pts',(-21.1775306085271,-19.7200472440895,
6.52799250840908));
#152919=CARTESIAN_POINT('Ctrl Pts',(-21.2015830381501,-19.6388711282236,
6.53218690818428));
#152920=CARTESIAN_POINT('Ctrl Pts',(-21.2215663308332,-19.556660028202,
6.53638130795949));
#152921=CARTESIAN_POINT('Ctrl Pts',(-21.2415389226779,-19.4744929513404,
6.54057346167872));
#152922=CARTESIAN_POINT('Ctrl Pts',(-21.2574466025637,-19.391292431292,
6.54476561539796));
#152923=CARTESIAN_POINT('Ctrl Pts',(-21.2691973211301,-19.3074919730945,
6.54895776911719));
#152924=CARTESIAN_POINT('Ctrl Pts',(-21.2809466969546,-19.2237010906845,
6.55314944380356));
#152925=CARTESIAN_POINT('Ctrl Pts',(-21.288539988214,-19.1393108539585,
6.55734111848993));
#152926=CARTESIAN_POINT('Ctrl Pts',(-21.2919366299884,-19.0547628189733,
6.5615327931763));
#152927=CARTESIAN_POINT('Ctrl Pts',(-21.2933350165072,-19.0199546642823,
6.5632584921937));
#152928=CARTESIAN_POINT('Ctrl Pts',(-21.294022704555,-18.985119821685,6.56498419121111));
#152929=CARTESIAN_POINT('Ctrl Pts',(-21.2939994283744,-18.9502892333484,
6.56670989022851));
#152930=CARTESIAN_POINT('Ctrl Pts',(-21.293999428374,-18.9502892327451,
6.5667098902584));
#152931=CARTESIAN_POINT('Ctrl Pts',(-21.2939356382109,-18.8548333601135,
6.57143929947811));
#152932=CARTESIAN_POINT('Ctrl Pts',(-21.2885288437516,-18.7595846663126,
6.57616870869782));
#152933=CARTESIAN_POINT('Ctrl Pts',(-21.2778724975473,-18.6650980721178,
6.58089811791753));
#152934=CARTESIAN_POINT('Ctrl Pts',(-21.2671635859909,-18.5701453968674,
6.5856508562461));
#152935=CARTESIAN_POINT('Ctrl Pts',(-21.2511533349016,-18.4759625571734,
6.59040359457466));
#152936=CARTESIAN_POINT('Ctrl Pts',(-21.2299860493113,-18.383094347327,
6.59515633290323));
#152937=CARTESIAN_POINT('Ctrl Pts',(-21.2086961910769,-18.2896883688573,
6.59993659274375));
#152938=CARTESIAN_POINT('Ctrl Pts',(-21.1821895164639,-18.1976124823347,
6.60471685258427));
#152939=CARTESIAN_POINT('Ctrl Pts',(-21.1506609174307,-18.1073994967067,
6.60949711242479));
#152940=CARTESIAN_POINT('Ctrl Pts',(-21.1426476472041,-18.0844710744505,
6.61071205742805));
#152941=CARTESIAN_POINT('Ctrl Pts',(-21.1343102131572,-18.061662873534,
6.61192700243132));
#152942=CARTESIAN_POINT('Ctrl Pts',(-21.1256522921827,-18.0389833992214,
6.61314194743458));
#152943=CARTESIAN_POINT('Ctrl Pts',(-21.0958318198278,-17.9608684985716,
6.61732658182763));
#152944=CARTESIAN_POINT('Ctrl Pts',(-21.062124806143,-17.8840707367778,
6.62151121622068));
#152945=CARTESIAN_POINT('Ctrl Pts',(-21.0246680532229,-17.8090039939071,
6.62569585061373));
#152946=CARTESIAN_POINT('Ctrl Pts',(-20.9872646153543,-17.7340440992535,
6.62987452869768));
#152947=CARTESIAN_POINT('Ctrl Pts',(-20.9461222434272,-17.6608107375728,
6.63405320678162));
#152948=CARTESIAN_POINT('Ctrl Pts',(-20.9014264094921,-17.5896994606784,
6.63823188486557));
#152949=CARTESIAN_POINT('Ctrl Pts',(-20.8559294348561,-17.5173135652524,
6.64248546275101));
#152950=CARTESIAN_POINT('Ctrl Pts',(-20.8067505255347,-17.4471270300727,
6.64673904063645));
#152951=CARTESIAN_POINT('Ctrl Pts',(-20.7541351457543,-17.3795325145211,
6.65099261852188));
#152952=CARTESIAN_POINT('Ctrl Pts',(-20.7025398177813,-17.3132484505532,
6.65516373249984));
#152953=CARTESIAN_POINT('Ctrl Pts',(-20.6476403712485,-17.2494571801025,
6.65933484647779));
#152954=CARTESIAN_POINT('Ctrl Pts',(-20.5897118973504,-17.188499686977,
6.66350596045574));
#152955=CARTESIAN_POINT('Ctrl Pts',(-20.5318028619112,-17.127562648727,
6.66767567477611));
#152956=CARTESIAN_POINT('Ctrl Pts',(-20.4708671343697,-17.0694578324914,
6.67184538909649));
#152957=CARTESIAN_POINT('Ctrl Pts',(-20.4072185463107,-17.0144913687206,
6.67601510341686));
#152958=CARTESIAN_POINT('Ctrl Pts',(-20.3435722231415,-16.9595268608925,
6.6801846693609));
#152959=CARTESIAN_POINT('Ctrl Pts',(-20.2772135801197,-16.9077007835214,
6.68435423530495));
#152960=CARTESIAN_POINT('Ctrl Pts',(-20.2084905554454,-16.8592798558091,
6.68852380124899));
#152961=CARTESIAN_POINT('Ctrl Pts',(-20.1373513140027,-16.8091565080122,
6.69283996398791));
#152962=CARTESIAN_POINT('Ctrl Pts',(-20.0636787652557,-16.7626825189766,
6.69715612672683));
#152963=CARTESIAN_POINT('Ctrl Pts',(-19.9878910926204,-16.7201045885062,
6.70147228946575));
#152964=CARTESIAN_POINT('Ctrl Pts',(-19.9145721954497,-16.6789136296424,
6.70564785365743));
#152965=CARTESIAN_POINT('Ctrl Pts',(-19.8392743011541,-16.6413689670526,
6.70982341784911));
#152966=CARTESIAN_POINT('Ctrl Pts',(-19.7623989816003,-16.607646030429,
6.71399898204079));
#152967=CARTESIAN_POINT('Ctrl Pts',(-19.6816408724096,-16.5722198284451,
6.71838544405333));
#152968=CARTESIAN_POINT('Ctrl Pts',(-19.5991423447411,-16.5410117758973,
6.72277190606587));
#152969=CARTESIAN_POINT('Ctrl Pts',(-19.5153878511231,-16.5141663251737,
6.72715836807841));
#152970=CARTESIAN_POINT('Ctrl Pts',(-19.4316333575051,-16.48732087445,6.73154483009095));
#152971=CARTESIAN_POINT('Ctrl Pts',(-19.3466234783172,-16.4648381003647,
6.73593129210349));
#152972=CARTESIAN_POINT('Ctrl Pts',(-19.2608535512399,-16.4468003401833,
6.74031775411602));
#152973=CARTESIAN_POINT('Ctrl Pts',(-19.1790300256488,-16.4295925240862,
6.74450238850907));
#152974=CARTESIAN_POINT('Ctrl Pts',(-19.0962102942859,-16.4163656164703,
6.74868702290212));
#152975=CARTESIAN_POINT('Ctrl Pts',(-19.0128164131692,-16.407228613854,
6.75287165729517));
#152976=CARTESIAN_POINT('Ctrl Pts',(-18.92954123292,-16.3981046166299,6.75705033537912));
#152977=CARTESIAN_POINT('Ctrl Pts',(-18.8456939795802,-16.3930590108019,
6.76122901346306));
#152978=CARTESIAN_POINT('Ctrl Pts',(-18.76170764213,-16.3921499484213,6.76540769154701));
#152979=CARTESIAN_POINT('Ctrl Pts',(-18.6762159099409,-16.3912245917508,
6.76966126943245));
#152980=CARTESIAN_POINT('Ctrl Pts',(-18.5905805302509,-16.3945856314592,
6.77391484731788));
#152981=CARTESIAN_POINT('Ctrl Pts',(-18.5052645325904,-16.4022392100534,
6.77816842520332));
#152982=CARTESIAN_POINT('Ctrl Pts',(-18.421602552025,-16.4097444090919,
6.78233953918127));
#152983=CARTESIAN_POINT('Ctrl Pts',(-18.3382481596055,-16.4213771508025,
6.78651065315922));
#152984=CARTESIAN_POINT('Ctrl Pts',(-18.2556369703987,-16.4370906950924,
6.79068176713718));
#152985=CARTESIAN_POINT('Ctrl Pts',(-18.1730535021743,-16.4527989665509,
6.79485148145755));
#152986=CARTESIAN_POINT('Ctrl Pts',(-18.0912131934259,-16.472585235142,
6.79902119577792));
#152987=CARTESIAN_POINT('Ctrl Pts',(-18.0105433225007,-16.4963513207745,
6.8031909100983));
#152988=CARTESIAN_POINT('Ctrl Pts',(-17.9298763221558,-16.5201165607077,
6.80736047604234));
#152989=CARTESIAN_POINT('Ctrl Pts',(-17.8503801178648,-16.5478612052845,
6.81153004198638));
#152990=CARTESIAN_POINT('Ctrl Pts',(-17.7724673106158,-16.579437063586,
6.81569960793043));
#152991=CARTESIAN_POINT('Ctrl Pts',(-17.6918151851798,-16.6121230901123,
6.82001577066935));
#152992=CARTESIAN_POINT('Ctrl Pts',(-17.6128603617428,-16.6489145558588,
6.82433193340827));
#152993=CARTESIAN_POINT('Ctrl Pts',(-17.5360366305501,-16.6895933686766,
6.82864809614719));
#152994=CARTESIAN_POINT('Ctrl Pts',(-17.4617154243205,-16.7289470734455,
6.83282366033887));
#152995=CARTESIAN_POINT('Ctrl Pts',(-17.3893889826095,-16.771938472629,
6.83699922453055));
#152996=CARTESIAN_POINT('Ctrl Pts',(-17.3194221772607,-16.8183248646023,
6.84117478872223));
#152997=CARTESIAN_POINT('Ctrl Pts',(-17.2459215149041,-16.867054122961,
6.84556125073476));
#152998=CARTESIAN_POINT('Ctrl Pts',(-17.1750255931742,-16.9195300021187,
6.8499477127473));
#152999=CARTESIAN_POINT('Ctrl Pts',(-17.1071180986344,-16.9754233435029,
6.85433417475984));
#153000=CARTESIAN_POINT('Ctrl Pts',(-17.0392106040947,-17.0313166848872,
6.85872063677238));
#153001=CARTESIAN_POINT('Ctrl Pts',(-16.9742919138006,-17.0906270409863,
6.86310709878492));
#153002=CARTESIAN_POINT('Ctrl Pts',(-16.9126993772538,-17.1529824788001,
6.86749356079746));
#153003=CARTESIAN_POINT('Ctrl Pts',(-16.8539408046155,-17.2124688504872,
6.8716781951905));
#153004=CARTESIAN_POINT('Ctrl Pts',(-16.7979903187279,-17.2749476638324,
6.87586282958355));
#153005=CARTESIAN_POINT('Ctrl Pts',(-16.7451680193311,-17.3401230342645,
6.8800474639766));
#153006=CARTESIAN_POINT('Ctrl Pts',(-16.6924209059394,-17.4052056356239,
6.88422614206054));
#153007=CARTESIAN_POINT('Ctrl Pts',(-16.6427934219785,-17.47297681583,6.88840482014449));
#153008=CARTESIAN_POINT('Ctrl Pts',(-16.5965688328438,-17.5431039762746,
6.89258349822843));
#153009=CARTESIAN_POINT('Ctrl Pts',(-16.5495157011698,-17.6144881156707,
6.89683707611387));
#153010=CARTESIAN_POINT('Ctrl Pts',(-16.5059889968457,-17.6883131849443,
6.9010906539993));
#153011=CARTESIAN_POINT('Ctrl Pts',(-16.4662445138507,-17.7641931743589,
6.90534423188474));
#153012=CARTESIAN_POINT('Ctrl Pts',(-16.4272705552134,-17.8386020821111,
6.90951534586269));
#153013=CARTESIAN_POINT('Ctrl Pts',(-16.3919336983951,-17.9149865174728,
6.91368645984064));
#153014=CARTESIAN_POINT('Ctrl Pts',(-16.3604304325482,-17.9929548975848,
6.9178575738186));
#153015=CARTESIAN_POINT('Ctrl Pts',(-16.3289377379263,-18.0708971146538,
6.92202728813897));
#153016=CARTESIAN_POINT('Ctrl Pts',(-16.3012762516654,-18.1504217947137,
6.92619700245934));
#153017=CARTESIAN_POINT('Ctrl Pts',(-16.277594697511,-18.2311165212713,
6.93036671677971));
#153018=CARTESIAN_POINT('Ctrl Pts',(-16.253913986048,-18.3118083763642,
6.93453628272376));
#153019=CARTESIAN_POINT('Ctrl Pts',(-16.2342130538339,-18.3936697535164,
6.9387058486678));
#153020=CARTESIAN_POINT('Ctrl Pts',(-16.2185906288469,-18.4762735076588,
6.94287541461184));
#153021=CARTESIAN_POINT('Ctrl Pts',(-16.2024189386697,-18.5617815078941,
6.94719157735076));
#153022=CARTESIAN_POINT('Ctrl Pts',(-16.190617990557,-18.6480845421363,
6.95150774008969));
#153023=CARTESIAN_POINT('Ctrl Pts',(-16.1832392059578,-18.7346998122939,
6.95582390282861));
#153024=CARTESIAN_POINT('Ctrl Pts',(-16.1761007844907,-18.8184935991364,
6.95999946702029));
#153025=CARTESIAN_POINT('Ctrl Pts',(-16.1731008165489,-18.9025791196894,
6.96417503121196));
#153026=CARTESIAN_POINT('Ctrl Pts',(-16.1742327266829,-18.9865182046884,
6.96835059540364));
#153027=CARTESIAN_POINT('Ctrl Pts',(-16.1754218069069,-19.0746968533245,
6.97273705741619));
#153028=CARTESIAN_POINT('Ctrl Pts',(-16.1811710990057,-19.1627133020808,
6.97712351942873));
#153029=CARTESIAN_POINT('Ctrl Pts',(-16.1914115149699,-19.2500667639851,
6.98150998144128));
#153030=CARTESIAN_POINT('Ctrl Pts',(-16.2016519309342,-19.3374202258893,
6.98589644345382));
#153031=CARTESIAN_POINT('Ctrl Pts',(-16.2163832985703,-19.4241101416678,
6.99028290546636));
#153032=CARTESIAN_POINT('Ctrl Pts',(-16.2354754819719,-19.5096515334977,
6.9946693674789));
#153033=CARTESIAN_POINT('Ctrl Pts',(-16.2536851821504,-19.5912390117506,
6.99885307745135));
#153034=CARTESIAN_POINT('Ctrl Pts',(-16.2759292313602,-19.6720854131194,
7.00303678742379));
#153035=CARTESIAN_POINT('Ctrl Pts',(-16.3021321571724,-19.7517617113997,
7.00722049739624));
#153036=CARTESIAN_POINT('Ctrl Pts',(-16.3283004575831,-19.8313327228186,
7.01139867887776));
#153037=CARTESIAN_POINT('Ctrl Pts',(-16.3584171062948,-19.9097362680112,
7.01557686035929));
#153038=CARTESIAN_POINT('Ctrl Pts',(-16.3923558259102,-19.9865542817808,
7.01975504184081));
#153039=CARTESIAN_POINT('Ctrl Pts',(-16.4262598829414,-20.0632938391182,
7.0239289560262));
#153040=CARTESIAN_POINT('Ctrl Pts',(-16.4639780734803,-20.1384506626445,
7.0281028702116));
#153041=CARTESIAN_POINT('Ctrl Pts',(-16.5053350197151,-20.2116239143695,
7.032276784397));
#153042=CARTESIAN_POINT('Ctrl Pts',(-16.5474166561144,-20.2860793675301,
7.0365238373132));
#153043=CARTESIAN_POINT('Ctrl Pts',(-16.5932656311566,-20.3584806089359,
7.0407708902294));
#153044=CARTESIAN_POINT('Ctrl Pts',(-16.6426471430979,-20.4284292153461,
7.0450179431456));
#153045=CARTESIAN_POINT('Ctrl Pts',(-16.6911293175254,-20.4971039157272,
7.04918764861211));
#153046=CARTESIAN_POINT('Ctrl Pts',(-16.7430161416243,-20.5634141925112,
7.05335735407862));
#153047=CARTESIAN_POINT('Ctrl Pts',(-16.7980413928969,-20.6270117228197,
7.05752705954513));
#153048=CARTESIAN_POINT('Ctrl Pts',(-16.8545977101723,-20.692378840986,
7.06181278618618));
#153049=CARTESIAN_POINT('Ctrl Pts',(-16.9144694015651,-20.7548795964524,
7.06609851282723));
#153050=CARTESIAN_POINT('Ctrl Pts',(-16.9773239709915,-20.8141732811709,
7.07038423946828));
#153051=CARTESIAN_POINT('Ctrl Pts',(-17.0401785404178,-20.8734669658894,
7.07466996610933));
#153052=CARTESIAN_POINT('Ctrl Pts',(-17.1060155888496,-20.9295532350968,
7.07895569275038));
#153053=CARTESIAN_POINT('Ctrl Pts',(-17.1744641402401,-20.9821349467765,
7.08324141939143));
#153054=CARTESIAN_POINT('Origin',(-18.734,-18.952,-1.76670989022851));
#153055=CARTESIAN_POINT('',(-17.1770150605606,-20.9788230109682,7.94987221524758));
#153056=CARTESIAN_POINT('',(-17.1718944119046,-20.9854718354472,7.88329695584275));
#153057=CARTESIAN_POINT('',(-17.1744641402401,-20.9821349467765,-1.76670989022851));
#153058=CARTESIAN_POINT('',(-21.29363549648,-18.9525601738873,7.43329008494618));
#153059=CARTESIAN_POINT('Ctrl Pts',(-21.2898970146452,-18.9525588546298,
7.4332901097715));
#153060=CARTESIAN_POINT('Ctrl Pts',(-21.288997505724,-18.4906083046144,
7.4561794192865));
#153061=CARTESIAN_POINT('Ctrl Pts',(-20.9482575273653,-17.1718695394144,
7.52146066436198));
#153062=CARTESIAN_POINT('Ctrl Pts',(-18.8327965306519,-15.9265198389028,
7.62913384499793));
#153063=CARTESIAN_POINT('Ctrl Pts',(-16.2435266653506,-17.2312927241795,
7.75630965167936));
#153064=CARTESIAN_POINT('Ctrl Pts',(-15.9876142035043,-19.6552910609173,
7.86322244176258));
#153065=CARTESIAN_POINT('Ctrl Pts',(-16.8231471588985,-20.7063099151551,
7.92774329628532));
#153066=CARTESIAN_POINT('Ctrl Pts',(-17.1770150605606,-20.9788230109682,
7.94987221524758));
#153067=CARTESIAN_POINT('Ctrl Pts',(-17.1744641402401,-20.9821349467765,
7.14996297217343));
#153068=CARTESIAN_POINT('Ctrl Pts',(-17.2410258191382,-21.0332671758395,
7.15413570876718));
#153069=CARTESIAN_POINT('Ctrl Pts',(-17.3101704637236,-21.0811728588169,
7.15830844536094));
#153070=CARTESIAN_POINT('Ctrl Pts',(-17.3815499321768,-21.1255866244631,
7.16248118195469));
#153071=CARTESIAN_POINT('Ctrl Pts',(-17.4528912216783,-21.1699766343845,
7.16665168666424));
#153072=CARTESIAN_POINT('Ctrl Pts',(-17.5264645719111,-21.2108781927614,
7.17082219137378));
#153073=CARTESIAN_POINT('Ctrl Pts',(-17.601892368295,-21.2480688818577,
7.17499269608332));
#153074=CARTESIAN_POINT('Ctrl Pts',(-17.6773024471275,-21.2852508350771,
7.17916222116552));
#153075=CARTESIAN_POINT('Ctrl Pts',(-17.7545656943623,-21.3187234472259,
7.18333174624772));
#153076=CARTESIAN_POINT('Ctrl Pts',(-17.8332805880677,-21.3483106102858,
7.18750127132992));
#153077=CARTESIAN_POINT('Ctrl Pts',(-17.9120006044927,-21.3778996988611,
7.1916710677624));
#153078=CARTESIAN_POINT('Ctrl Pts',(-17.992172023889,-21.4036026756203,
7.19584086419487));
#153079=CARTESIAN_POINT('Ctrl Pts',(-18.0733753666637,-21.4252923591499,
7.20001066062734));
#153080=CARTESIAN_POINT('Ctrl Pts',(-18.1546631662148,-21.447004601366,
7.20418479392025));
#153081=CARTESIAN_POINT('Ctrl Pts',(-18.2369845870321,-21.46469509586,7.20835892721316));
#153082=CARTESIAN_POINT('Ctrl Pts',(-18.3199075506605,-21.4782872844156,
7.21253306050607));
#153083=CARTESIAN_POINT('Ctrl Pts',(-18.4028745562677,-21.4918866920436,
7.21670941076135));
#153084=CARTESIAN_POINT('Ctrl Pts',(-18.4864432835453,-21.5013834070713,
7.22088576101664));
#153085=CARTESIAN_POINT('Ctrl Pts',(-18.5701765131517,-21.5067527992267,
7.22506211127192));
#153086=CARTESIAN_POINT('Ctrl Pts',(-18.6540563452631,-21.5121315922657,
7.22924577359927));
#153087=CARTESIAN_POINT('Ctrl Pts',(-18.7381007944719,-21.5133686209315,
7.23342943592662));
#153088=CARTESIAN_POINT('Ctrl Pts',(-18.8218728097775,-21.5104914245121,
7.23761309825396));
#153089=CARTESIAN_POINT('Ctrl Pts',(-18.8885736292776,-21.5082005477994,
7.24094420715385));
#153090=CARTESIAN_POINT('Ctrl Pts',(-18.9551017008547,-21.5033024409368,
7.24427531605374));
#153091=CARTESIAN_POINT('Ctrl Pts',(-19.0212404493959,-21.4958342957494,
7.24760642495362));
#153092=CARTESIAN_POINT('Ctrl Pts',(-19.1043258393297,-21.4864525978996,
7.25179105934667));
#153093=CARTESIAN_POINT('Ctrl Pts',(-19.1871057341708,-21.4729786230522,
7.25597569373973));
#153094=CARTESIAN_POINT('Ctrl Pts',(-19.2691452086517,-21.455441552275,
7.26016032813278));
#153095=CARTESIAN_POINT('Ctrl Pts',(-19.3510679100953,-21.4379294433474,
7.26433900621674));
#153096=CARTESIAN_POINT('Ctrl Pts',(-19.4322518385276,-21.416365821315,
7.26851768430069));
#153097=CARTESIAN_POINT('Ctrl Pts',(-19.512267670395,-21.3908315713099,
7.27269636238465));
#153098=CARTESIAN_POINT('Ctrl Pts',(-19.5937177285419,-21.3648396382247,
7.27694994027009));
#153099=CARTESIAN_POINT('Ctrl Pts',(-19.6739569228745,-21.3347333841331,
7.28120351815552));
#153100=CARTESIAN_POINT('Ctrl Pts',(-19.7525437584813,-21.3006525098573,
7.28545709604095));
#153101=CARTESIAN_POINT('Ctrl Pts',(-19.8296070349302,-21.2672323598327,
7.2896282100189));
#153102=CARTESIAN_POINT('Ctrl Pts',(-19.9050810078239,-21.2299905173575,
7.29379932399685));
#153103=CARTESIAN_POINT('Ctrl Pts',(-19.9785668286285,-21.1891082694133,
7.29797043797479));
#153104=CARTESIAN_POINT('Ctrl Pts',(-20.0520279905563,-21.1482397399023,
7.30214015229516));
#153105=CARTESIAN_POINT('Ctrl Pts',(-20.1235019236783,-21.1037334544492,
7.30630986661553));
#153106=CARTESIAN_POINT('Ctrl Pts',(-20.1926138614935,-21.055816912913,
7.3104795809359));
#153107=CARTESIAN_POINT('Ctrl Pts',(-20.2617233400095,-21.007902076453,
7.31464914687995));
#153108=CARTESIAN_POINT('Ctrl Pts',(-20.3284706127606,-20.9565774880018,
7.31881871282399));
#153109=CARTESIAN_POINT('Ctrl Pts',(-20.392510565395,-20.9021135106637,
7.32298827876804));
#153110=CARTESIAN_POINT('Ctrl Pts',(-20.4588020837621,-20.8457346470711,
7.32730444150696));
#153111=CARTESIAN_POINT('Ctrl Pts',(-20.5221919593127,-20.7859918669765,
7.33162060424587));
#153112=CARTESIAN_POINT('Ctrl Pts',(-20.5823369324964,-20.7232285521552,
7.33593676698479));
#153113=CARTESIAN_POINT('Ctrl Pts',(-20.6405226895048,-20.6625097457126,
7.34011233117647));
#153114=CARTESIAN_POINT('Ctrl Pts',(-20.6956714299406,-20.598964557046,
7.34428789536816));
#153115=CARTESIAN_POINT('Ctrl Pts',(-20.7475130548919,-20.5329380689262,
7.34846345955984));
#153116=CARTESIAN_POINT('Ctrl Pts',(-20.8019730770776,-20.4635767398546,
7.35284992157237));
#153117=CARTESIAN_POINT('Ctrl Pts',(-20.8527827827186,-20.3914773402457,
7.35723638358491));
#153118=CARTESIAN_POINT('Ctrl Pts',(-20.8996813854344,-20.3170729419277,
7.36162284559745));
#153119=CARTESIAN_POINT('Ctrl Pts',(-20.9465799881501,-20.2426685436096,
7.36600930760998));
#153120=CARTESIAN_POINT('Ctrl Pts',(-20.9895672706481,-20.1659596899256,
7.37039576962252));
#153121=CARTESIAN_POINT('Ctrl Pts',(-21.0284398795321,-20.0874054955005,
7.37478223163505));
#153122=CARTESIAN_POINT('Ctrl Pts',(-21.0682036058612,-20.0070505211677,
7.37926924910127));
#153123=CARTESIAN_POINT('Ctrl Pts',(-21.103794382086,-19.9244993534847,
7.38375626656748));
#153124=CARTESIAN_POINT('Ctrl Pts',(-21.1349820909847,-19.8401919830593,
7.38824328403369));
#153125=CARTESIAN_POINT('Ctrl Pts',(-21.1660643193882,-19.7561697500644,
7.39271512587973));
#153126=CARTESIAN_POINT('Ctrl Pts',(-21.1927730322953,-19.6704034844231,
7.39718696772577));
#153127=CARTESIAN_POINT('Ctrl Pts',(-21.2149257129941,-19.5833537887784,
7.40165880957181));
#153128=CARTESIAN_POINT('Ctrl Pts',(-21.2370311427379,-19.4964897673327,
7.40612111312314));
#153129=CARTESIAN_POINT('Ctrl Pts',(-21.2545997969947,-19.4083481090824,
7.41058341667445));
#153130=CARTESIAN_POINT('Ctrl Pts',(-21.2674980351242,-19.3194067310512,
7.41504572022578));
#153131=CARTESIAN_POINT('Ctrl Pts',(-21.2803582069864,-19.2307278436205,
7.41949485428542));
#153132=CARTESIAN_POINT('Ctrl Pts',(-21.2885753721633,-19.1412542906272,
7.42394398834506));
#153133=CARTESIAN_POINT('Ctrl Pts',(-21.292066600817,-19.0514749505384,
7.4283931224047));
#153134=CARTESIAN_POINT('Ctrl Pts',(-21.2933474798422,-19.0185362676211,
7.43002544244517));
#153135=CARTESIAN_POINT('Ctrl Pts',(-21.2939927168564,-18.9855565464178,
7.43165776248564));
#153136=CARTESIAN_POINT('Ctrl Pts',(-21.2939999386838,-18.9525603024938,
7.43329008252611));
#153137=CARTESIAN_POINT('',(-21.2941233546374,-18.9508698167174,7.36670989022851));
#153138=CARTESIAN_POINT('Ctrl Pts',(-17.1744641402401,-20.9821349467765,
7.08324141939143));
#153139=CARTESIAN_POINT('Ctrl Pts',(-17.2411540116663,-21.0333656524678,
7.08741703089603));
#153140=CARTESIAN_POINT('Ctrl Pts',(-17.3103223783338,-21.0812695113244,
7.09159264240062));
#153141=CARTESIAN_POINT('Ctrl Pts',(-17.3815967344457,-21.1256157450935,
7.09576825390522));
#153142=CARTESIAN_POINT('Ctrl Pts',(-17.4557821042021,-21.171773184163,
7.10011440728107));
#153143=CARTESIAN_POINT('Ctrl Pts',(-17.5322486915606,-21.2140758921702,
7.10446056065693));
#153144=CARTESIAN_POINT('Ctrl Pts',(-17.6105502174091,-21.2523174967809,
7.10880671403278));
#153145=CARTESIAN_POINT('Ctrl Pts',(-17.6888517432577,-21.2905591013917,
7.11315286740862));
#153146=CARTESIAN_POINT('Ctrl Pts',(-17.7689876693612,-21.3247394525465,
7.11749902078447));
#153147=CARTESIAN_POINT('Ctrl Pts',(-17.8504927560597,-21.3547099179687,
7.12184517416032));
#153148=CARTESIAN_POINT('Ctrl Pts',(-17.9289688151197,-21.3835665710906,
7.12602980855337));
#153149=CARTESIAN_POINT('Ctrl Pts',(-18.009006152961,-21.4086281659991,
7.13021444294641));
#153150=CARTESIAN_POINT('Ctrl Pts',(-18.0902029058993,-21.429725832619,
7.13439907733946));
#153151=CARTESIAN_POINT('Ctrl Pts',(-18.1712840853099,-21.4507934693218,
7.1385777554234));
#153152=CARTESIAN_POINT('Ctrl Pts',(-18.2535209603944,-21.4679082701427,
7.14275643350735));
#153153=CARTESIAN_POINT('Ctrl Pts',(-18.3364934985373,-21.4809500946628,
7.14693511159129));
#153154=CARTESIAN_POINT('Ctrl Pts',(-18.4209532597952,-21.4942256845144,
7.15118868947672));
#153155=CARTESIAN_POINT('Ctrl Pts',(-18.5061748645251,-21.5032806792605,
7.15544226736216));
#153156=CARTESIAN_POINT('Ctrl Pts',(-18.5917010358988,-21.508042058499,
7.1596958452476));
#153157=CARTESIAN_POINT('Ctrl Pts',(-18.6755691155499,-21.5127111291099,
7.16386695922555));
#153158=CARTESIAN_POINT('Ctrl Pts',(-18.7597295775161,-21.5132515520536,
7.1680380732035));
#153159=CARTESIAN_POINT('Ctrl Pts',(-18.8437446259187,-21.5096465973785,
7.17220918718145));
#153160=CARTESIAN_POINT('Ctrl Pts',(-18.9277314822606,-21.5060428523808,
7.17637890150182));
#153161=CARTESIAN_POINT('Ctrl Pts',(-19.0115725627189,-21.4982965120596,
7.1805486158222));
#153162=CARTESIAN_POINT('Ctrl Pts',(-19.0948308836174,-21.4864429513066,
7.18471833014257));
#153163=CARTESIAN_POINT('Ctrl Pts',(-19.1780862418277,-21.4745898123542,
7.18888789608662));
#153164=CARTESIAN_POINT('Ctrl Pts',(-19.2607584263887,-21.4586298092437,
7.19305746203066));
#153165=CARTESIAN_POINT('Ctrl Pts',(-19.3424177464727,-21.4386499242509,
7.19722702797471));
#153166=CARTESIAN_POINT('Ctrl Pts',(-19.4269481075131,-21.4179675711496,
7.20154319071363));
#153167=CARTESIAN_POINT('Ctrl Pts',(-19.5103925419325,-21.3929775239273,
7.20585935345255));
#153168=CARTESIAN_POINT('Ctrl Pts',(-19.5922902863026,-21.363832868264,
7.21017551619147));
#153169=CARTESIAN_POINT('Ctrl Pts',(-19.6715202202639,-21.3356375966935,
7.21435108038315));
#153170=CARTESIAN_POINT('Ctrl Pts',(-19.7493022661266,-21.3035544560161,
7.21852664457483));
#153171=CARTESIAN_POINT('Ctrl Pts',(-19.8252402968867,-21.2677708467054,
7.22270220876651));
#153172=CARTESIAN_POINT('Ctrl Pts',(-19.9050137770549,-21.2301798923559,
7.22708867077905));
#153173=CARTESIAN_POINT('Ctrl Pts',(-19.9827515495241,-21.1885050997007,
7.23147513279159));
#153174=CARTESIAN_POINT('Ctrl Pts',(-20.058026370739,-21.1430166976971,
7.23586159480413));
#153175=CARTESIAN_POINT('Ctrl Pts',(-20.133301191954,-21.0975282956936,
7.24024805681667));
#153176=CARTESIAN_POINT('Ctrl Pts',(-20.2061126241217,-21.0482266726393,
7.24463451882921));
#153177=CARTESIAN_POINT('Ctrl Pts',(-20.2760730898189,-20.9954310816997,
7.24902098084176));
#153178=CARTESIAN_POINT('Ctrl Pts',(-20.3421228419793,-20.9455867065661,
7.25316224442402));
#153179=CARTESIAN_POINT('Ctrl Pts',(-20.4058887674612,-20.892434299838,
7.25730350800628));
#153180=CARTESIAN_POINT('Ctrl Pts',(-20.4670153688586,-20.8362127616859,
7.26144477158854));
#153181=CARTESIAN_POINT('Ctrl Pts',(-20.5280546973635,-20.7800714932714,
7.26558012252323));
#153182=CARTESIAN_POINT('Ctrl Pts',(-20.5864618395735,-20.7208701082191,
7.26971547345792));
#153183=CARTESIAN_POINT('Ctrl Pts',(-20.6419120481562,-20.6588894564384,
7.27385082439262));
#153184=CARTESIAN_POINT('Ctrl Pts',(-20.6972986881794,-20.5969798597691,
7.27798143452815));
#153185=CARTESIAN_POINT('Ctrl Pts',(-20.7497348173452,-20.5322976752762,
7.28211204466369));
#153186=CARTESIAN_POINT('Ctrl Pts',(-20.7989315869957,-20.465161439182,
7.28624265479922));
#153187=CARTESIAN_POINT('Ctrl Pts',(-20.848098059321,-20.3980665482492,
7.29037072114094));
#153188=CARTESIAN_POINT('Ctrl Pts',(-20.8940288533086,-20.328520983131,
7.29449878748266));
#153189=CARTESIAN_POINT('Ctrl Pts',(-20.9364753744699,-20.2568763255013,
7.29862685382437));
#153190=CARTESIAN_POINT('Ctrl Pts',(-20.9789091334294,-20.1852532089438,
7.30275367899922));
#153191=CARTESIAN_POINT('Ctrl Pts',(-21.0178604599826,-20.11153265758,7.30688050417406));
#153192=CARTESIAN_POINT('Ctrl Pts',(-21.0531249145872,-20.0360939214574,
7.31100732934891));
#153193=CARTESIAN_POINT('Ctrl Pts',(-21.0883898804923,-19.9606540915461,
7.31513421435873));
#153194=CARTESIAN_POINT('Ctrl Pts',(-21.1199676712092,-19.8834964546654,
7.31926109936854));
#153195=CARTESIAN_POINT('Ctrl Pts',(-21.147701166054,-19.8050220870467,
7.32338798437836));
#153196=CARTESIAN_POINT('Ctrl Pts',(-21.175460263615,-19.7264752742866,
7.32751867920248));
#153197=CARTESIAN_POINT('Ctrl Pts',(-21.1993678247306,-19.6466097489538,
7.3316493740266));
#153198=CARTESIAN_POINT('Ctrl Pts',(-21.2193162430201,-19.5658429540041,
7.33578006885071));
#153199=CARTESIAN_POINT('Ctrl Pts',(-21.2392749611597,-19.4850344572076,
7.33991289645233));
#153200=CARTESIAN_POINT('Ctrl Pts',(-21.2552703785522,-19.4033242264923,
7.34404572405394));
#153201=CARTESIAN_POINT('Ctrl Pts',(-21.2672462583489,-19.3211387199431,
7.34817855165556));
#153202=CARTESIAN_POINT('Ctrl Pts',(-21.2792406903518,-19.2388258972814,
7.35231778154836));
#153203=CARTESIAN_POINT('Ctrl Pts',(-21.287203113202,-19.1560367972438,
7.35645701144116));
#153204=CARTESIAN_POINT('Ctrl Pts',(-21.291129302603,-19.0732011954116,
7.36059624133396));
#153205=CARTESIAN_POINT('Ctrl Pts',(-21.2930622985235,-19.0324184251309,
7.36263412429881));
#153206=CARTESIAN_POINT('Ctrl Pts',(-21.2940177418851,-18.9916243590029,
7.36467200726366));
#153207=CARTESIAN_POINT('Ctrl Pts',(-21.2939997505486,-18.9508698712832,
7.36670989022851));
#153208=CARTESIAN_POINT('Ctrl Pts',(-21.2976210191122,-18.9508682726504,
7.36670989022851));
#153209=CARTESIAN_POINT('Ctrl Pts',(-21.2979707979485,-18.88753758729,7.36987218932674));
#153210=CARTESIAN_POINT('Ctrl Pts',(-21.2671017039969,-17.9755793917529,
7.41542642398544));
#153211=CARTESIAN_POINT('Ctrl Pts',(-20.1784866426459,-16.2917839998255,
7.50337259420463));
#153212=CARTESIAN_POINT('Ctrl Pts',(-17.2790525549706,-16.2974908625944,
7.63054840088605));
#153213=CARTESIAN_POINT('Ctrl Pts',(-15.721016444231,-18.7282885581798,
7.7571898547655));
#153214=CARTESIAN_POINT('Ctrl Pts',(-16.5081486620308,-20.4743154612817,
7.84143937308446));
#153215=CARTESIAN_POINT('Ctrl Pts',(-17.1718944119077,-20.9854718354495,
7.88329695584294));
#153216=CARTESIAN_POINT('Origin',(-18.734,-18.952,-1.76670989022851));
#153217=CARTESIAN_POINT('',(-17.1744641402401,-20.9821349467765,8.74981198891561));
#153218=CARTESIAN_POINT('',(-17.1744641402401,-20.9821349467765,8.68337762424306));
#153219=CARTESIAN_POINT('',(-17.1744641402401,-20.9821349467765,-1.76670989022851));
#153220=CARTESIAN_POINT('',(-21.2939989173812,-18.9496456407966,8.23329012251171));
#153221=CARTESIAN_POINT('Ctrl Pts',(-21.2939989173812,-18.9496456407966,
8.23329012251171));
#153222=CARTESIAN_POINT('Ctrl Pts',(-21.2938985191548,-18.8404782076697,
8.23871812867059));
#153223=CARTESIAN_POINT('Ctrl Pts',(-21.2868114602984,-18.7316228556169,
8.24414613482947));
#153224=CARTESIAN_POINT('Ctrl Pts',(-21.272879163598,-18.6238345041783,
8.24957414098835));
#153225=CARTESIAN_POINT('Ctrl Pts',(-21.2596700733063,-18.5216412981934,
8.25472038679393));
#153226=CARTESIAN_POINT('Ctrl Pts',(-21.2403084403045,-18.4204066645113,
8.25986663259951));
#153227=CARTESIAN_POINT('Ctrl Pts',(-21.2149532278239,-18.3207543415199,
8.26501287840509));
#153228=CARTESIAN_POINT('Ctrl Pts',(-21.1943358111288,-18.2397227402535,
8.26919751279814));
#153229=CARTESIAN_POINT('Ctrl Pts',(-21.1697059337058,-18.1595514977396,
8.27338214719119));
#153230=CARTESIAN_POINT('Ctrl Pts',(-21.1411517779373,-18.0806675043514,
8.27756678158424));
#153231=CARTESIAN_POINT('Ctrl Pts',(-21.1126382654753,-18.001895792564,
8.28174545966817));
#153232=CARTESIAN_POINT('Ctrl Pts',(-21.0802117249138,-17.9244081193636,
8.28592413775211));
#153233=CARTESIAN_POINT('Ctrl Pts',(-21.0440107968602,-17.8486187792112,
8.29010281583605));
#153234=CARTESIAN_POINT('Ctrl Pts',(-21.0071609931883,-17.7714709696052,
8.29435639372149));
#153235=CARTESIAN_POINT('Ctrl Pts',(-20.9664002781983,-17.6960834444032,
8.29860997160693));
#153236=CARTESIAN_POINT('Ctrl Pts',(-20.9219272181895,-17.6228745401937,
8.30286354949236));
#153237=CARTESIAN_POINT('Ctrl Pts',(-20.8783163552311,-17.5510849334477,
8.30703466347032));
#153238=CARTESIAN_POINT('Ctrl Pts',(-20.8311360546879,-17.481390639162,
8.31120577744827));
#153239=CARTESIAN_POINT('Ctrl Pts',(-20.7806202689679,-17.4141620778997,
8.31537689142622));
#153240=CARTESIAN_POINT('Ctrl Pts',(-20.7301214343076,-17.3469560758303,
8.31954660574659));
#153241=CARTESIAN_POINT('Ctrl Pts',(-20.6762896134472,-17.282214531026,
8.32371632006697));
#153242=CARTESIAN_POINT('Ctrl Pts',(-20.6194012584855,-17.2202777086088,
8.32788603438735));
#153243=CARTESIAN_POINT('Ctrl Pts',(-20.5625149278557,-17.1583430901695,
8.33205560033139));
#153244=CARTESIAN_POINT('Ctrl Pts',(-20.5025725911954,-17.0992133339121,
8.33622516627543));
#153245=CARTESIAN_POINT('Ctrl Pts',(-20.4398891227941,-17.0431934878745,
8.34039473221948));
#153246=CARTESIAN_POINT('Ctrl Pts',(-20.3750017809722,-16.9852040531582,
8.3447108949584));
#153247=CARTESIAN_POINT('Ctrl Pts',(-20.307177357872,-16.9305476379183,
8.34902705769732));
#153248=CARTESIAN_POINT('Ctrl Pts',(-20.2368028123897,-16.8795175013831,
8.35334322043624));
#153249=CARTESIAN_POINT('Ctrl Pts',(-20.1687207103245,-16.830149666178,
8.35751878462792));
#153250=CARTESIAN_POINT('Ctrl Pts',(-20.0982524952704,-16.7841757035314,
8.3616943488196));
#153251=CARTESIAN_POINT('Ctrl Pts',(-20.0257768405865,-16.7418161628216,
8.36586991301128));
#153252=CARTESIAN_POINT('Ctrl Pts',(-19.9496406128789,-16.6973171424108,
8.37025637502383));
#153253=CARTESIAN_POINT('Ctrl Pts',(-19.8712893431907,-16.656807536765,
8.37464283703637));
#153254=CARTESIAN_POINT('Ctrl Pts',(-19.7911876038235,-16.6204866780732,
8.37902929904891));
#153255=CARTESIAN_POINT('Ctrl Pts',(-19.7110858644562,-16.5841658193814,
8.38341576106145));
#153256=CARTESIAN_POINT('Ctrl Pts',(-19.6292342232968,-16.5520338488593,
8.38780222307399));
#153257=CARTESIAN_POINT('Ctrl Pts',(-19.5461152252309,-16.524229652346,
8.39218868508653));
#153258=CARTESIAN_POINT('Ctrl Pts',(-19.466820655478,-16.49770476813,8.39637331947958));
#153259=CARTESIAN_POINT('Ctrl Pts',(-19.3860776423915,-16.4750194242752,
8.40055795387263));
#153260=CARTESIAN_POINT('Ctrl Pts',(-19.3042928646695,-16.4563305410157,
8.40474258826568));
#153261=CARTESIAN_POINT('Ctrl Pts',(-19.2226244974556,-16.4376682590682,
8.40892126634962));
#153262=CARTESIAN_POINT('Ctrl Pts',(-19.1399177555962,-16.4229912402357,
8.41309994443357));
#153263=CARTESIAN_POINT('Ctrl Pts',(-19.0565960387005,-16.4124071594417,
8.41727862251751));
#153264=CARTESIAN_POINT('Ctrl Pts',(-18.9717808399117,-16.4016333666062,
8.42153220040295));
#153265=CARTESIAN_POINT('Ctrl Pts',(-18.8863288596153,-16.3951008398354,
8.42578577828838));
#153266=CARTESIAN_POINT('Ctrl Pts',(-18.8006993328509,-16.3928690539566,
8.43003935617382));
#153267=CARTESIAN_POINT('Ctrl Pts',(-18.7167299015551,-16.3906805356019,
8.43421047015177));
#153268=CARTESIAN_POINT('Ctrl Pts',(-18.6325902275832,-16.3926275022743,
8.43838158412972));
#153269=CARTESIAN_POINT('Ctrl Pts',(-18.5487184100095,-16.3987137386477,
8.44255269810768));
#153270=CARTESIAN_POINT('Ctrl Pts',(-18.4648747364341,-16.4047979327256,
8.44672241242805));
#153271=CARTESIAN_POINT('Ctrl Pts',(-18.3812991991949,-16.4150186047169,
8.45089212674842));
#153272=CARTESIAN_POINT('Ctrl Pts',(-18.2984275456889,-16.4293274812125,
8.4550618410688));
#153273=CARTESIAN_POINT('Ctrl Pts',(-18.2155588411121,-16.443635848537,
8.45923140701284));
#153274=CARTESIAN_POINT('Ctrl Pts',(-18.1333944236484,-16.4620320520103,
8.46340097295688));
#153275=CARTESIAN_POINT('Ctrl Pts',(-18.0523612259041,-16.4844164489021,
8.46757053890092));
#153276=CARTESIAN_POINT('Ctrl Pts',(-17.9684790008923,-16.5075878535745,
8.47188670163984));
#153277=CARTESIAN_POINT('Ctrl Pts',(-17.8858095314086,-16.5350329790257,
8.47620286437876));
#153278=CARTESIAN_POINT('Ctrl Pts',(-17.8048088555659,-16.5665851897196,
8.48051902711769));
#153279=CARTESIAN_POINT('Ctrl Pts',(-17.7264467682191,-16.5971095904688,
8.48469459130937));
#153280=CARTESIAN_POINT('Ctrl Pts',(-17.6496468328973,-16.631477373477,
8.48887015550105));
#153281=CARTESIAN_POINT('Ctrl Pts',(-17.5747994654321,-16.6694895135712,
8.49304571969273));
#153282=CARTESIAN_POINT('Ctrl Pts',(-17.4961717353689,-16.7094215564963,
8.49743218170527));
#153283=CARTESIAN_POINT('Ctrl Pts',(-17.4196995115721,-16.7533754937362,
8.50181864371781));
#153284=CARTESIAN_POINT('Ctrl Pts',(-17.3458018650429,-16.8010685882387,
8.50620510573035));
#153285=CARTESIAN_POINT('Ctrl Pts',(-17.2719042185137,-16.8487616827411,
8.51059156774289));
#153286=CARTESIAN_POINT('Ctrl Pts',(-17.2005815753788,-16.9001935334405,
8.51497802975543));
#153287=CARTESIAN_POINT('Ctrl Pts',(-17.1322119090441,-16.9550335727229,
8.51936449176797));
#153288=CARTESIAN_POINT('Ctrl Pts',(-17.0669880324055,-17.0073503405056,
8.52354912616102));
#153289=CARTESIAN_POINT('Ctrl Pts',(-17.0042085866858,-17.0629632902855,
8.52773376055407));
#153290=CARTESIAN_POINT('Ctrl Pts',(-16.9442256444345,-17.1216154075823,
8.53191839494712));
#153291=CARTESIAN_POINT('Ctrl Pts',(-16.8843280804771,-17.1801840408498,
8.53609707303106));
#153292=CARTESIAN_POINT('Ctrl Pts',(-16.8272194396165,-17.2417829302056,
8.540275751115));
#153293=CARTESIAN_POINT('Ctrl Pts',(-16.7732194376016,-17.3061143459765,
8.54445442919894));
#153294=CARTESIAN_POINT('Ctrl Pts',(-16.7182515243596,-17.3715988561409,
8.54870800708438));
#153295=CARTESIAN_POINT('Ctrl Pts',(-16.6665051669308,-17.4399145156592,
8.55296158496982));
#153296=CARTESIAN_POINT('Ctrl Pts',(-16.6182789494493,-17.5107073731346,
8.55721516285525));
#153297=CARTESIAN_POINT('Ctrl Pts',(-16.5709876912994,-17.5801277729269,
8.5613862768332));
#153298=CARTESIAN_POINT('Ctrl Pts',(-16.5270815724709,-17.6519297794778,
8.56555739081116));
#153299=CARTESIAN_POINT('Ctrl Pts',(-16.4868009099952,-17.7257470693687,
8.56972850478911));
#153300=CARTESIAN_POINT('Ctrl Pts',(-16.4465337640849,-17.7995395891551,
8.57389821910948));
#153301=CARTESIAN_POINT('Ctrl Pts',(-16.409889878601,-17.8753456457563,
8.57806793342985));
#153302=CARTESIAN_POINT('Ctrl Pts',(-16.3770645250475,-17.952772715089,
8.58223764775022));
#153303=CARTESIAN_POINT('Ctrl Pts',(-16.344240339561,-18.0301970292344,
8.58640721369426));
#153304=CARTESIAN_POINT('Ctrl Pts',(-16.315234594618,-18.1092418175489,
8.59057677963831));
#153305=CARTESIAN_POINT('Ctrl Pts',(-16.2901945969736,-18.1894941625542,
8.59474634558235));
#153306=CARTESIAN_POINT('Ctrl Pts',(-16.2642742239021,-18.2725680810079,
8.59906250832127));
#153307=CARTESIAN_POINT('Ctrl Pts',(-16.2426038152403,-18.3569355479853,
8.60337867106019));
#153308=CARTESIAN_POINT('Ctrl Pts',(-16.2252901016539,-18.4421229109477,
8.60769483379911));
#153309=CARTESIAN_POINT('Ctrl Pts',(-16.2085403804665,-18.5245353045217,
8.61187039799079));
#153310=CARTESIAN_POINT('Ctrl Pts',(-16.1958678987932,-18.6077145253799,
8.61604596218247));
#153311=CARTESIAN_POINT('Ctrl Pts',(-16.1873166326445,-18.6912245670412,
8.62022152637415));
#153312=CARTESIAN_POINT('Ctrl Pts',(-16.1783334623714,-18.7789525023805,
8.62460798838669));
#153313=CARTESIAN_POINT('Ctrl Pts',(-16.1738988033979,-18.8670449731774,
8.62899445039923));
#153314=CARTESIAN_POINT('Ctrl Pts',(-16.1740017537922,-18.9549965668354,
8.63338091241177));
#153315=CARTESIAN_POINT('Ctrl Pts',(-16.1741047041864,-19.0429481604934,
8.63776737442431));
#153316=CARTESIAN_POINT('Ctrl Pts',(-16.1787451573697,-19.1307583016182,
8.64215383643685));
#153317=CARTESIAN_POINT('Ctrl Pts',(-16.1878497481281,-19.2179302444114,
8.64654029844939));
#153318=CARTESIAN_POINT('Ctrl Pts',(-16.1967810774084,-19.303443294448,
8.65084328555215));
#153319=CARTESIAN_POINT('Ctrl Pts',(-16.210042254892,-19.3886695640475,
8.65514627265491));
#153320=CARTESIAN_POINT('Ctrl Pts',(-16.2276047119207,-19.4731359322611,
8.65944925975767));
#153321=CARTESIAN_POINT('Ctrl Pts',(-16.2446561825664,-19.5551447192891,
8.66362704981018));
#153322=CARTESIAN_POINT('Ctrl Pts',(-16.2657620068644,-19.6364367189553,
8.66780483986269));
#153323=CARTESIAN_POINT('Ctrl Pts',(-16.2908434896405,-19.7165824127508,
8.67198262991519));
#153324=CARTESIAN_POINT('Ctrl Pts',(-16.3159003340244,-19.7966493767103,
8.67615631598269));
#153325=CARTESIAN_POINT('Ctrl Pts',(-16.3449249457181,-19.8755718341914,
8.68033000205019));
#153326=CARTESIAN_POINT('Ctrl Pts',(-16.3777879099992,-19.9529318592862,
8.68450368811769));
#153327=CARTESIAN_POINT('Ctrl Pts',(-16.4106284513386,-20.0302391003617,
8.68867452641044));
#153328=CARTESIAN_POINT('Ctrl Pts',(-16.4473019635812,-20.1059856045522,
8.6928453647032));
#153329=CARTESIAN_POINT('Ctrl Pts',(-16.4876301097207,-20.1797712800218,
8.69701620299595));
#153330=CARTESIAN_POINT('Ctrl Pts',(-16.5279428373367,-20.2535287452641,
8.70118544666623));
#153331=CARTESIAN_POINT('Ctrl Pts',(-16.5719072007185,-20.325326468996,
8.70535469033651));
#153332=CARTESIAN_POINT('Ctrl Pts',(-16.6192985221864,-20.3947881548353,
8.70952393400679));
#153333=CARTESIAN_POINT('Ctrl Pts',(-16.6667008411468,-20.4642659597516,
8.71369414517964));
#153334=CARTESIAN_POINT('Ctrl Pts',(-16.7175314520026,-20.5314062606125,
8.7178643563525));
#153335=CARTESIAN_POINT('Ctrl Pts',(-16.7715224002379,-20.5958618161002,
8.72203456752536));
#153336=CARTESIAN_POINT('Ctrl Pts',(-16.8255216898818,-20.6603273297408,
8.72620542298094));
#153337=CARTESIAN_POINT('Ctrl Pts',(-16.8826819840771,-20.7221069276297,
8.73037627843651));
#153338=CARTESIAN_POINT('Ctrl Pts',(-16.9426963304669,-20.780887958164,
8.73454713389209));
#153339=CARTESIAN_POINT('Ctrl Pts',(-17.0027604653468,-20.8397177540175,
8.73872144953024));
#153340=CARTESIAN_POINT('Ctrl Pts',(-17.0656830383974,-20.8955437075325,
8.74289576516841));
#153341=CARTESIAN_POINT('Ctrl Pts',(-17.1311223583306,-20.9480919983398,
8.74707008080657));
#153342=CARTESIAN_POINT('Ctrl Pts',(-17.145450343844,-20.9595974838829,
8.74798405017625));
#153343=CARTESIAN_POINT('Ctrl Pts',(-17.1598988634156,-20.970946000174,
8.74889801954593));
#153344=CARTESIAN_POINT('Ctrl Pts',(-17.1744641402401,-20.9821349467765,
8.74981198891562));
#153345=CARTESIAN_POINT('Ctrl Pts',(-17.1770150605606,-20.9788230109682,
7.94987221524758));
#153346=CARTESIAN_POINT('Ctrl Pts',(-17.501044950009,-21.2283579020811,
7.9701352318458));
#153347=CARTESIAN_POINT('Ctrl Pts',(-18.677462676132,-21.7718986662915,
8.03279018400449));
#153348=CARTESIAN_POINT('Ctrl Pts',(-20.7208249517526,-21.0909115417432,
8.12726281551247));
#153349=CARTESIAN_POINT('Ctrl Pts',(-21.2877697529773,-19.5894613481947,
8.20147243042223));
#153350=CARTESIAN_POINT('Ctrl Pts',(-21.2935816048406,-18.9496462807751,
8.23329010977151));
#153351=CARTESIAN_POINT('',(-21.2939989424941,-18.9543268925436,8.16670989022853));
#153352=CARTESIAN_POINT('Ctrl Pts',(-17.1718944119077,-20.9854718354495,
7.88329695584294));
#153353=CARTESIAN_POINT('Ctrl Pts',(-17.1803677727156,-20.9919972442953,
7.88383130864493));
#153354=CARTESIAN_POINT('Ctrl Pts',(-17.864630092765,-21.5115395255608,
7.92675759700741));
#153355=CARTESIAN_POINT('Ctrl Pts',(-19.7898862882482,-21.7889693291709,
8.01207582093036));
#153356=CARTESIAN_POINT('Ctrl Pts',(-21.1940976605954,-20.1719438373811,
8.10601244625689));
#153357=CARTESIAN_POINT('Ctrl Pts',(-21.2961551338926,-19.1382186499617,
8.15755713602294));
#153358=CARTESIAN_POINT('Ctrl Pts',(-21.2944496155086,-18.9543273021797,
8.16670989022852));
#153359=CARTESIAN_POINT('Ctrl Pts',(-21.2939989424941,-18.9543268925437,
8.16670989022852));
#153360=CARTESIAN_POINT('Ctrl Pts',(-21.2940748047761,-18.8708647825268,
8.17086478789788));
#153361=CARTESIAN_POINT('Ctrl Pts',(-21.2900646933588,-18.7872780169979,
8.17501968556725));
#153362=CARTESIAN_POINT('Ctrl Pts',(-21.2819596922617,-18.7040052286649,
8.17917458323661));
#153363=CARTESIAN_POINT('Ctrl Pts',(-21.2739328413916,-18.621535375116,
8.18328941845664));
#153364=CARTESIAN_POINT('Ctrl Pts',(-21.2618897634889,-18.539373952273,
8.18740425367668));
#153365=CARTESIAN_POINT('Ctrl Pts',(-21.2458740550218,-18.4579466307083,
8.19151908889671));
#153366=CARTESIAN_POINT('Ctrl Pts',(-21.2298653109089,-18.3765547174254,
8.19563213480031));
#153367=CARTESIAN_POINT('Ctrl Pts',(-21.2098874553344,-18.2958967363637,
8.1997451807039));
#153368=CARTESIAN_POINT('Ctrl Pts',(-21.1860355605651,-18.2163903142807,
8.20385822660749));
#153369=CARTESIAN_POINT('Ctrl Pts',(-21.1621864189584,-18.1368930694186,
8.20797079775283));
#153370=CARTESIAN_POINT('Ctrl Pts',(-21.1344642632166,-18.0585475732026,
8.21208336889816));
#153371=CARTESIAN_POINT('Ctrl Pts',(-21.1030141994635,-17.9817568744174,
8.2161959400435));
#153372=CARTESIAN_POINT('Ctrl Pts',(-21.0710029255601,-17.9035958852586,
8.22038189789764));
#153373=CARTESIAN_POINT('Ctrl Pts',(-21.035129571801,-17.8270462022335,
8.22456785575179));
#153374=CARTESIAN_POINT('Ctrl Pts',(-20.9955977974881,-17.7525103575283,
8.22875381360593));
#153375=CARTESIAN_POINT('Ctrl Pts',(-20.9567081892511,-17.6791852955855,
8.23287177349703));
#153376=CARTESIAN_POINT('Ctrl Pts',(-20.9142784405326,-17.6078095092631,
8.23698973338812));
#153377=CARTESIAN_POINT('Ctrl Pts',(-20.8685472200434,-17.5387384653204,
8.24110769327921));
#153378=CARTESIAN_POINT('Ctrl Pts',(-20.8216832918823,-17.4679566141755,
8.24532765011488));
#153379=CARTESIAN_POINT('Ctrl Pts',(-20.7713524862055,-17.399595623106,
8.24954760695055));
#153380=CARTESIAN_POINT('Ctrl Pts',(-20.7178552814754,-17.3340017854886,
8.25376756378622));
#153381=CARTESIAN_POINT('Ctrl Pts',(-20.6643580767453,-17.2684079478711,
8.25798752062189));
#153382=CARTESIAN_POINT('Ctrl Pts',(-20.6076948817587,-17.2055816046285,
8.26220747745756));
#153383=CARTESIAN_POINT('Ctrl Pts',(-20.5482046419776,-17.1458268308308,
8.26642743429323));
#153384=CARTESIAN_POINT('Ctrl Pts',(-20.4892123552949,-17.0865722243692,
8.27061206868627));
#153385=CARTESIAN_POINT('Ctrl Pts',(-20.427204219073,-17.0301005497847,
8.27479670307932));
#153386=CARTESIAN_POINT('Ctrl Pts',(-20.3624734272386,-16.9767343731088,
8.27898133747237));
#153387=CARTESIAN_POINT('Ctrl Pts',(-20.2978347716741,-16.9234441565799,
8.28316001555632));
#153388=CARTESIAN_POINT('Ctrl Pts',(-20.230481510108,-16.8732509480032,
8.28733869364026));
#153389=CARTESIAN_POINT('Ctrl Pts',(-20.1607438576395,-16.8264407877718,
8.29151737172421));
#153390=CARTESIAN_POINT('Ctrl Pts',(-20.08975620787,-16.7787915890602,8.29577094960965));
#153391=CARTESIAN_POINT('Ctrl Pts',(-20.0162981861697,-16.7346482555833,
8.30002452749508));
#153392=CARTESIAN_POINT('Ctrl Pts',(-19.9407536469187,-16.6942698045053,
8.30427810538052));
#153393=CARTESIAN_POINT('Ctrl Pts',(-19.8666736859741,-16.6546741684936,
8.30844921935847));
#153394=CARTESIAN_POINT('Ctrl Pts',(-19.7905878123475,-16.6186989652308,
8.31262033333642));
#153395=CARTESIAN_POINT('Ctrl Pts',(-19.7128859499199,-16.5865439557985,
8.31679144731437));
#153396=CARTESIAN_POINT('Ctrl Pts',(-19.6352101611027,-16.5543997362902,
8.32096116163474));
#153397=CARTESIAN_POINT('Ctrl Pts',(-19.5559198851422,-16.5260733404925,
8.32513087595511));
#153398=CARTESIAN_POINT('Ctrl Pts',(-19.4754262787741,-16.5017169401999,
8.32930059027548));
#153399=CARTESIAN_POINT('Ctrl Pts',(-19.3949355367137,-16.4773614066125,
8.33347015621953));
#153400=CARTESIAN_POINT('Ctrl Pts',(-19.3132419899457,-16.4569757200691,
8.33763972216358));
#153401=CARTESIAN_POINT('Ctrl Pts',(-19.230771941892,-16.4406621816751,
8.34180928810762));
#153402=CARTESIAN_POINT('Ctrl Pts',(-19.1454023486867,-16.4237750793961,
8.34612545084654));
#153403=CARTESIAN_POINT('Ctrl Pts',(-19.0592011520725,-16.4112519089494,
8.35044161358546));
#153404=CARTESIAN_POINT('Ctrl Pts',(-18.9726507026517,-16.4031481325656,
8.35475777632438));
#153405=CARTESIAN_POINT('Ctrl Pts',(-18.8889196250172,-16.3953083358451,
8.35893334051606));
#153406=CARTESIAN_POINT('Ctrl Pts',(-18.8048621716341,-16.3916044048151,
8.36310890470774));
#153407=CARTESIAN_POINT('Ctrl Pts',(-18.7209165514642,-16.392033433153,
8.36728446889942));
#153408=CARTESIAN_POINT('Ctrl Pts',(-18.6327310375814,-16.3924841306923,
8.37167093091196));
#153409=CARTESIAN_POINT('Ctrl Pts',(-18.544669534143,-16.3974962383813,
8.3760573929245));
#153410=CARTESIAN_POINT('Ctrl Pts',(-18.4572333890563,-16.4070048638422,
8.38044385493705));
#153411=CARTESIAN_POINT('Ctrl Pts',(-18.3697972439697,-16.4165134893032,
8.38483031694959));
#153412=CARTESIAN_POINT('Ctrl Pts',(-18.2829870179305,-16.4305184650313,
8.38921677896213));
#153413=CARTESIAN_POINT('Ctrl Pts',(-18.1972887614196,-16.4488937205182,
8.39360324097467));
#153414=CARTESIAN_POINT('Ctrl Pts',(-18.115533608726,-16.4664235032614,
8.39778787536772));
#153415=CARTESIAN_POINT('Ctrl Pts',(-18.0344860391771,-16.4879954864412,
8.40197250976076));
#153416=CARTESIAN_POINT('Ctrl Pts',(-17.9545759800698,-16.513537739239,
8.40615714415381));
#153417=CARTESIAN_POINT('Ctrl Pts',(-17.8747796630406,-16.5390436358014,
8.41033582223776));
#153418=CARTESIAN_POINT('Ctrl Pts',(-17.796118074845,-16.5685084380807,
8.4145145003217));
#153419=CARTESIAN_POINT('Ctrl Pts',(-17.7190104693569,-16.6018093156757,
8.41869317840565));
#153420=CARTESIAN_POINT('Ctrl Pts',(-17.6405207654567,-16.6357070875686,
8.42294675629108));
#153421=CARTESIAN_POINT('Ctrl Pts',(-17.5636417739317,-16.673579709668,
8.42720033417652));
#153422=CARTESIAN_POINT('Ctrl Pts',(-17.4887990603226,-16.715244622265,
8.43145391206195));
#153423=CARTESIAN_POINT('Ctrl Pts',(-17.4154073187602,-16.7561017792289,
8.43562502603991));
#153424=CARTESIAN_POINT('Ctrl Pts',(-17.3439740257042,-16.8006052628959,
8.43979614001786));
#153425=CARTESIAN_POINT('Ctrl Pts',(-17.2748782070124,-16.8485353358735,
8.44396725399581));
#153426=CARTESIAN_POINT('Ctrl Pts',(-17.20580557409,-16.8964493254522,8.44813696831618));
#153427=CARTESIAN_POINT('Ctrl Pts',(-17.1390692354551,-16.9477873587841,
8.45230668263656));
#153428=CARTESIAN_POINT('Ctrl Pts',(-17.0750196948478,-17.0022860858277,
8.45647639695693));
#153429=CARTESIAN_POINT('Ctrl Pts',(-17.010972433398,-17.0567828735727,
8.46064596290098));
#153430=CARTESIAN_POINT('Ctrl Pts',(-16.949612129695,-17.1144398326397,
8.46481552884502));
#153431=CARTESIAN_POINT('Ctrl Pts',(-16.8912555527359,-17.1749538829628,
8.46898509478907));
#153432=CARTESIAN_POINT('Ctrl Pts',(-16.8308472305215,-17.237595532643,
8.47330125752799));
#153433=CARTESIAN_POINT('Ctrl Pts',(-16.7736581532182,-17.3032985427183,
8.47761742026691));
#153434=CARTESIAN_POINT('Ctrl Pts',(-16.7199960430175,-17.3716873533194,
8.48193358300583));
#153435=CARTESIAN_POINT('Ctrl Pts',(-16.6680819704122,-17.4378484056084,
8.48610914719751));
#153436=CARTESIAN_POINT('Ctrl Pts',(-16.6194688453352,-17.5065225539072,
8.49028471138918));
#153437=CARTESIAN_POINT('Ctrl Pts',(-16.5743914182288,-17.5773397606898,
8.49446027558086));
#153438=CARTESIAN_POINT('Ctrl Pts',(-16.5270372374408,-17.6517337762351,
8.4988467375934));
#153439=CARTESIAN_POINT('Ctrl Pts',(-16.4835856052312,-17.7284925234216,
8.50323319960595));
#153440=CARTESIAN_POINT('Ctrl Pts',(-16.4442533274935,-17.8071593229862,
8.50761966161849));
#153441=CARTESIAN_POINT('Ctrl Pts',(-16.4049210497558,-17.8858261225507,
8.51200612363103));
#153442=CARTESIAN_POINT('Ctrl Pts',(-16.3697082891389,-17.9664004123698,
8.51639258564357));
#153443=CARTESIAN_POINT('Ctrl Pts',(-16.3387721302027,-18.0484052613331,
8.52077904765611));
#153444=CARTESIAN_POINT('Ctrl Pts',(-16.3092593897976,-18.1266369456353,
8.52496368204916));
#153445=CARTESIAN_POINT('Ctrl Pts',(-16.2835285016033,-18.2064616309202,
8.5291483164422));
#153446=CARTESIAN_POINT('Ctrl Pts',(-16.2617516946765,-18.2874788815808,
8.53333295083525));
#153447=CARTESIAN_POINT('Ctrl Pts',(-16.240005884339,-18.3683808142128,
8.53751162891919));
#153448=CARTESIAN_POINT('Ctrl Pts',(-16.2222030943946,-18.4504715000485,
8.54169030700313));
#153449=CARTESIAN_POINT('Ctrl Pts',(-16.2084669780844,-18.5333319271618,
8.54586898508706));
#153450=CARTESIAN_POINT('Ctrl Pts',(-16.1944846517614,-18.6176775678805,
8.5501225629725));
#153451=CARTESIAN_POINT('Ctrl Pts',(-16.1847163934876,-18.7028203654201,
8.55437614085793));
#153452=CARTESIAN_POINT('Ctrl Pts',(-16.179239049994,-18.7883036704004,
8.55862971874337));
#153453=CARTESIAN_POINT('Ctrl Pts',(-16.1738678954921,-18.8721297147068,
8.56280083272133));
#153454=CARTESIAN_POINT('Ctrl Pts',(-16.1726227957354,-18.9562827012368,
8.56697194669928));
#153455=CARTESIAN_POINT('Ctrl Pts',(-16.1755241458591,-19.0403249895433,
8.57114306067723));
#153456=CARTESIAN_POINT('Ctrl Pts',(-16.1784245224067,-19.1243390766483,
8.57531277499761));
#153457=CARTESIAN_POINT('Ctrl Pts',(-16.1854685696706,-19.2082420799255,
8.57948248931799));
#153458=CARTESIAN_POINT('Ctrl Pts',(-16.1966245729686,-19.2915967348153,
8.58365220363836));
#153459=CARTESIAN_POINT('Ctrl Pts',(-16.2077801792881,-19.3749484235886,
8.5878217695824));
#153460=CARTESIAN_POINT('Ctrl Pts',(-16.2230473888476,-19.4577513469163,
8.59199133552644));
#153461=CARTESIAN_POINT('Ctrl Pts',(-16.2423428203252,-19.5395751007105,
8.59616090147048));
#153462=CARTESIAN_POINT('Ctrl Pts',(-16.2623166553701,-19.6242756767476,
8.6004770642094));
#153463=CARTESIAN_POINT('Ctrl Pts',(-16.286607126249,-19.7079264335896,
8.60479322694832));
#153464=CARTESIAN_POINT('Ctrl Pts',(-16.3150650107314,-19.7900653421374,
8.60910938968724));
#153465=CARTESIAN_POINT('Ctrl Pts',(-16.3425958826199,-19.8695285843788,
8.61328495387892));
#153466=CARTESIAN_POINT('Ctrl Pts',(-16.3740266108363,-19.9475765433407,
8.6174605180706));
#153467=CARTESIAN_POINT('Ctrl Pts',(-16.4091731183428,-20.0238115367565,
8.62163608226228));
#153468=CARTESIAN_POINT('Ctrl Pts',(-16.4460947923907,-20.1038969784582,
8.62602254427482));
#153469=CARTESIAN_POINT('Ctrl Pts',(-16.4871172070498,-20.1819809787839,
8.63040900628736));
#153470=CARTESIAN_POINT('Ctrl Pts',(-16.5319737202489,-20.2576340464639,
8.63479546829991));
#153471=CARTESIAN_POINT('Ctrl Pts',(-16.576830233448,-20.3332871141439,
8.63918193031245));
#153472=CARTESIAN_POINT('Ctrl Pts',(-16.625520460569,-20.4065088081493,
8.64356839232499));
#153473=CARTESIAN_POINT('Ctrl Pts',(-16.677728404917,-20.4769088914603,
8.64795485433753));
#153474=CARTESIAN_POINT('Ctrl Pts',(-16.7275305669034,-20.5440648846084,
8.65213918479575));
#153475=CARTESIAN_POINT('Ctrl Pts',(-16.7807187430381,-20.6089035367426,
8.65632351525396));
#153476=CARTESIAN_POINT('Ctrl Pts',(-16.8370495093351,-20.671063360079,
8.66050784571218));
#153477=CARTESIAN_POINT('Ctrl Pts',(-16.8932939076475,-20.7331278781494,
8.6646857606321));
#153478=CARTESIAN_POINT('Ctrl Pts',(-16.9526710148719,-20.7925213917371,
8.66886367555201));
#153479=CARTESIAN_POINT('Ctrl Pts',(-17.0148956024723,-20.8489133007075,
8.67304159047192));
#153480=CARTESIAN_POINT('Ctrl Pts',(-17.0662095115363,-20.8954172535731,
8.6764869350623));
#153481=CARTESIAN_POINT('Ctrl Pts',(-17.1194590131858,-20.9398803822471,
8.67993227965268));
#153482=CARTESIAN_POINT('Ctrl Pts',(-17.1744641402401,-20.9821349467765,
8.68337762424306));
#153483=CARTESIAN_POINT('Origin',(-18.734,-18.952,-1.76670989022851));
#153484=CARTESIAN_POINT('',(-17.1725833834245,-20.9846205132764,9.54996331522893));
#153485=CARTESIAN_POINT('',(-17.1744641402401,-20.9821349467765,9.48328065029978));
#153486=CARTESIAN_POINT('',(-17.1744641402401,-20.9821349467765,-1.76670989022851));
#153487=CARTESIAN_POINT('',(-21.294330140624,-18.9526425111494,9.03329016589256));
#153488=CARTESIAN_POINT('Ctrl Pts',(-21.2980343851841,-18.9526308401995,
9.03329079542781));
#153489=CARTESIAN_POINT('Ctrl Pts',(-21.295285921847,-18.1388728971705,
9.07394170534359));
#153490=CARTESIAN_POINT('Ctrl Pts',(-20.4360628655086,-16.4715240736058,
9.15698455081984));
#153491=CARTESIAN_POINT('Ctrl Pts',(-17.5947352967179,-16.1474738554406,
9.28241933185657));
#153492=CARTESIAN_POINT('Ctrl Pts',(-15.7591749622877,-18.3919045129074,
9.40959513853801));
#153493=CARTESIAN_POINT('Ctrl Pts',(-16.3858469674303,-20.326135493453,
9.49877646632879));
#153494=CARTESIAN_POINT('Ctrl Pts',(-17.1023021555805,-20.9314719346189,
9.5455658585591));
#153495=CARTESIAN_POINT('Ctrl Pts',(-17.1725833834245,-20.9846205132764,
9.54996331522893));
#153496=CARTESIAN_POINT('Ctrl Pts',(-17.1744641402401,-20.9821349467765,
8.74981198891562));
#153497=CARTESIAN_POINT('Ctrl Pts',(-17.2411337728998,-21.0333501051849,
8.7539955003499));
#153498=CARTESIAN_POINT('Ctrl Pts',(-17.3102516250714,-21.0812183482621,
8.75817901178418));
#153499=CARTESIAN_POINT('Ctrl Pts',(-17.3814397288989,-21.1255180498535,
8.76236252321847));
#153500=CARTESIAN_POINT('Ctrl Pts',(-17.4458385782616,-21.1655928608993,
8.76614705052259));
#153501=CARTESIAN_POINT('Ctrl Pts',(-17.5119310604356,-21.202747812138,
8.76993157782671));
#153502=CARTESIAN_POINT('Ctrl Pts',(-17.5794224113972,-21.2368524223451,
8.77371610513083));
#153503=CARTESIAN_POINT('Ctrl Pts',(-17.6540490703618,-21.2745626337838,
8.77790073952388));
#153504=CARTESIAN_POINT('Ctrl Pts',(-17.7306640561251,-21.3086830520783,
8.78208537391693));
#153505=CARTESIAN_POINT('Ctrl Pts',(-17.8088876493305,-21.3389996101045,
8.78627000830998));
#153506=CARTESIAN_POINT('Ctrl Pts',(-17.8869999009332,-21.3692730162627,
8.79044868639392));
#153507=CARTESIAN_POINT('Ctrl Pts',(-17.9667157867297,-21.3957531518832,
8.79462736447786));
#153508=CARTESIAN_POINT('Ctrl Pts',(-18.0476319224909,-21.4182722603509,
8.79880604256181));
#153509=CARTESIAN_POINT('Ctrl Pts',(-18.1299984218321,-21.4411950076538,
8.80305962044724));
#153510=CARTESIAN_POINT('Ctrl Pts',(-18.213608193011,-21.4600131107992,
8.80731319833268));
#153511=CARTESIAN_POINT('Ctrl Pts',(-18.2980154243377,-21.4746013259698,
8.81156677621811));
#153512=CARTESIAN_POINT('Ctrl Pts',(-18.380786256778,-21.4889067201227,
8.81573789019606));
#153513=CARTESIAN_POINT('Ctrl Pts',(-18.4643234304655,-21.4991446900207,
8.81990900417402));
#153514=CARTESIAN_POINT('Ctrl Pts',(-18.5481939962223,-21.5052481526401,
8.82408011815197));
#153515=CARTESIAN_POINT('Ctrl Pts',(-18.6320364184008,-21.5113495671838,
8.82824983247234));
#153516=CARTESIAN_POINT('Ctrl Pts',(-18.7162115520294,-21.5133191964338,
8.83241954679272));
#153517=CARTESIAN_POINT('Ctrl Pts',(-18.8002812486104,-21.5111418085137,
8.83658926111309));
#153518=CARTESIAN_POINT('Ctrl Pts',(-18.8843479536309,-21.5089644980744,
8.84075882705713));
#153519=CARTESIAN_POINT('Ctrl Pts',(-18.9683087692068,-21.502640476632,
8.84492839300118));
#153520=CARTESIAN_POINT('Ctrl Pts',(-19.0517268423097,-21.4922066163357,
8.84909795894522));
#153521=CARTESIAN_POINT('Ctrl Pts',(-19.1380777919556,-21.481405914383,
8.85341412168414));
#153522=CARTESIAN_POINT('Ctrl Pts',(-19.2238466000237,-21.4662010579768,
8.85773028442306));
#153523=CARTESIAN_POINT('Ctrl Pts',(-19.3085579282896,-21.4466910003124,
8.86204644716198));
#153524=CARTESIAN_POINT('Ctrl Pts',(-19.3905097939472,-21.4278164807243,
8.86622201135366));
#153525=CARTESIAN_POINT('Ctrl Pts',(-19.4714715762059,-21.404913110059,
8.87039757554534));
#153526=CARTESIAN_POINT('Ctrl Pts',(-19.551028186959,-21.3781213781908,
8.87457313973702));
#153527=CARTESIAN_POINT('Ctrl Pts',(-19.6346030129934,-21.3499764596372,
8.87895960174956));
#153528=CARTESIAN_POINT('Ctrl Pts',(-19.716626443602,-21.3175402693169,
8.88334606376211));
#153529=CARTESIAN_POINT('Ctrl Pts',(-19.7966429339306,-21.2810319866776,
8.88773252577465));
#153530=CARTESIAN_POINT('Ctrl Pts',(-19.8766594242592,-21.2445237040383,
8.89211898778719));
#153531=CARTESIAN_POINT('Ctrl Pts',(-19.954668494674,-21.203943664325,8.89650544979973));
#153532=CARTESIAN_POINT('Ctrl Pts',(-20.0302483510423,-21.159564316712,
8.90089191181227));
#153533=CARTESIAN_POINT('Ctrl Pts',(-20.102350666183,-21.1172269286686,
8.90507654620531));
#153534=CARTESIAN_POINT('Ctrl Pts',(-20.1725107769709,-21.071274585504,
8.90926118059836));
#153535=CARTESIAN_POINT('Ctrl Pts',(-20.2403431519459,-21.0219107006307,
8.91344581499141));
#153536=CARTESIAN_POINT('Ctrl Pts',(-20.308078975931,-20.9726170791377,
8.91762449307535));
#153537=CARTESIAN_POINT('Ctrl Pts',(-20.3734932764658,-20.9199218296712,
8.92180317115929));
#153538=CARTESIAN_POINT('Ctrl Pts',(-20.4362266525525,-20.8640733310571,
8.92598184924322));
#153539=CARTESIAN_POINT('Ctrl Pts',(-20.50008447932,-20.807223788243,8.93023542712866));
#153540=CARTESIAN_POINT('Ctrl Pts',(-20.5611639093904,-20.7471070845338,
8.9344890050141));
#153541=CARTESIAN_POINT('Ctrl Pts',(-20.6191183231211,-20.6840302849064,
8.93874258289954));
#153542=CARTESIAN_POINT('Ctrl Pts',(-20.675949177453,-20.6221763521241,
8.94291369687749));
#153543=CARTESIAN_POINT('Ctrl Pts',(-20.7297747776525,-20.5574764280246,
8.94708481085544));
#153544=CARTESIAN_POINT('Ctrl Pts',(-20.7803043703346,-20.4902582435825,
8.95125592483339));
#153545=CARTESIAN_POINT('Ctrl Pts',(-20.8308170073239,-20.4230626148514,
8.95542563915376));
#153546=CARTESIAN_POINT('Ctrl Pts',(-20.8780355571481,-20.3533507714295,
8.95959535347413));
#153547=CARTESIAN_POINT('Ctrl Pts',(-20.9217100507378,-20.2814828821391,
8.9637650677945));
#153548=CARTESIAN_POINT('Ctrl Pts',(-20.9653829902015,-20.2096175502167,
8.96793463373855));
#153549=CARTESIAN_POINT('Ctrl Pts',(-21.005511885995,-20.1355967185424,
8.97210419968259));
#153550=CARTESIAN_POINT('Ctrl Pts',(-21.0418912815017,-20.0598076695746,
8.97627376562663));
#153551=CARTESIAN_POINT('Ctrl Pts',(-21.0795497316757,-19.9813539711409,
8.98058992836555));
#153552=CARTESIAN_POINT('Ctrl Pts',(-21.113189882732,-19.901005876374,8.98490609110447));
#153553=CARTESIAN_POINT('Ctrl Pts',(-21.1426376470827,-19.8192166309844,
8.9892222538434));
#153554=CARTESIAN_POINT('Ctrl Pts',(-21.171126153607,-19.7400916616608,
8.99339781803508));
#153555=CARTESIAN_POINT('Ctrl Pts',(-21.1956911205895,-19.6596184551168,
8.99757338222676));
#153556=CARTESIAN_POINT('Ctrl Pts',(-21.216225998462,-19.5782220792652,
9.00174894641843));
#153557=CARTESIAN_POINT('Ctrl Pts',(-21.2377980441989,-19.4927145659707,
9.00613540843098));
#153558=CARTESIAN_POINT('Ctrl Pts',(-21.254922068569,-19.4061887466987,
9.01052187044353));
#153559=CARTESIAN_POINT('Ctrl Pts',(-21.2675357890124,-19.3191463002581,
9.01490833245607));
#153560=CARTESIAN_POINT('Ctrl Pts',(-21.2801495094559,-19.2321038538175,
9.01929479446862));
#153561=CARTESIAN_POINT('Ctrl Pts',(-21.288252948244,-19.1445453649661,
9.02368125648116));
#153562=CARTESIAN_POINT('Ctrl Pts',(-21.2918468828523,-19.0569729673898,
9.02806771849371));
#153563=CARTESIAN_POINT('Ctrl Pts',(-21.2932731600888,-19.022219269613,
9.02980851558631));
#153564=CARTESIAN_POINT('Ctrl Pts',(-21.2939911726516,-18.9874363059255,
9.03154931267891));
#153565=CARTESIAN_POINT('Ctrl Pts',(-21.2939999191096,-18.9526435515772,
9.03329010977151));
#153566=CARTESIAN_POINT('',(-21.293999998394,-18.9519093211995,8.96670989026365));
#153567=CARTESIAN_POINT('Ctrl Pts',(-17.1744641402401,-20.9821349467765,
8.68337762424306));
#153568=CARTESIAN_POINT('Ctrl Pts',(-17.2410628670692,-21.0332956358081,
8.68754915470747));
#153569=CARTESIAN_POINT('Ctrl Pts',(-17.3102359477333,-21.0812173626802,
8.69172068517188));
#153570=CARTESIAN_POINT('Ctrl Pts',(-17.3816324675696,-21.1256379774995,
8.6958922156363));
#153571=CARTESIAN_POINT('Ctrl Pts',(-17.4530008754767,-21.170041101982,
8.70006210358691));
#153572=CARTESIAN_POINT('Ctrl Pts',(-17.5265905938739,-21.2109456092011,
8.70423199153752));
#153573=CARTESIAN_POINT('Ctrl Pts',(-17.6020217631817,-21.248132677214,
8.70840187948813));
#153574=CARTESIAN_POINT('Ctrl Pts',(-17.6774458595108,-21.2853162582951,
8.71257137643952));
#153575=CARTESIAN_POINT('Ctrl Pts',(-17.7547106507946,-21.3187828899485,
8.71674087339091));
#153576=CARTESIAN_POINT('Ctrl Pts',(-17.8334129450119,-21.3483603561209,
8.7209103703423));
#153577=CARTESIAN_POINT('Ctrl Pts',(-17.9121314679419,-21.3779439212794,
8.72508072705983));
#153578=CARTESIAN_POINT('Ctrl Pts',(-17.9922876513835,-21.4036365679451,
8.72925108377736));
#153579=CARTESIAN_POINT('Ctrl Pts',(-18.0734609565294,-21.4253152189017,
8.73342144049489));
#153580=CARTESIAN_POINT('Ctrl Pts',(-18.1547253310253,-21.4470181914091,
8.73759647598798));
#153581=CARTESIAN_POINT('Ctrl Pts',(-18.2370086591808,-21.4646980633853,
8.74177151148105));
#153582=CARTESIAN_POINT('Ctrl Pts',(-18.3198785149476,-21.4782825249006,
8.74594654697414));
#153583=CARTESIAN_POINT('Ctrl Pts',(-18.4028028717265,-21.4918759205077,
8.75012432826251));
#153584=CARTESIAN_POINT('Ctrl Pts',(-18.4863140672385,-21.5013684936004,
8.75430210955089));
#153585=CARTESIAN_POINT('Ctrl Pts',(-18.5699752029833,-21.506739882251,
8.75847989083926));
#153586=CARTESIAN_POINT('Ctrl Pts',(-18.6537709748597,-21.5121199150944,
8.76266439544433));
#153587=CARTESIAN_POINT('Ctrl Pts',(-18.7377167095927,-21.5133655229479,
8.76684890004941));
#153588=CARTESIAN_POINT('Ctrl Pts',(-18.8213766941403,-21.5105084157222,
8.77103340465448));
#153589=CARTESIAN_POINT('Ctrl Pts',(-18.8486819099696,-21.5095759038425,
8.77239915677598));
#153590=CARTESIAN_POINT('Ctrl Pts',(-18.8759567414457,-21.5082067564715,
8.77376490889747));
#153591=CARTESIAN_POINT('Ctrl Pts',(-18.9031862415111,-21.5064032601928,
8.77513066101897));
#153592=CARTESIAN_POINT('Ctrl Pts',(-18.9866168294529,-21.5008773873516,
8.77931529541202));
#153593=CARTESIAN_POINT('Ctrl Pts',(-19.0699316687706,-21.4912494832414,
8.78349992980506));
#153594=CARTESIAN_POINT('Ctrl Pts',(-19.1526949496533,-21.4775285662876,
8.78768456419811));
#153595=CARTESIAN_POINT('Ctrl Pts',(-19.2353404272495,-21.4638271793609,
8.79186324228203));
#153596=CARTESIAN_POINT('Ctrl Pts',(-19.3174354558603,-21.4460444262518,
8.79604192036597));
#153597=CARTESIAN_POINT('Ctrl Pts',(-19.3985474281615,-21.4242412333193,
8.8002205984499));
#153598=CARTESIAN_POINT('Ctrl Pts',(-19.4811132742725,-21.402047233823,
8.80447417633533));
#153599=CARTESIAN_POINT('Ctrl Pts',(-19.5626599937757,-21.3756872759161,
8.80872775422077));
#153600=CARTESIAN_POINT('Ctrl Pts',(-19.6427400986354,-21.3452804752331,
8.81298133210621));
#153601=CARTESIAN_POINT('Ctrl Pts',(-19.7212676943988,-21.3154631697154,
8.81715244608416));
#153602=CARTESIAN_POINT('Ctrl Pts',(-19.798384584547,-21.2817547038766,
8.82132356006211));
#153603=CARTESIAN_POINT('Ctrl Pts',(-19.8736839568159,-21.2443177089087,
8.82549467404006));
#153604=CARTESIAN_POINT('Ctrl Pts',(-19.9489580616533,-21.206893276286,
8.82966438836044));
#153605=CARTESIAN_POINT('Ctrl Pts',(-20.0224154482666,-21.1657430039572,
8.83383410268082));
#153606=CARTESIAN_POINT('Ctrl Pts',(-20.09367122156,-21.1210768011441,8.83800381700119));
#153607=CARTESIAN_POINT('Ctrl Pts',(-20.1649244592673,-21.0764121877461,
8.84217338294524));
#153608=CARTESIAN_POINT('Ctrl Pts',(-20.2339758500892,-21.0282321376739,
8.8463429488893));
#153609=CARTESIAN_POINT('Ctrl Pts',(-20.3004681352886,-20.9767907499605,
8.85051251483335));
#153610=CARTESIAN_POINT('Ctrl Pts',(-20.3692982072083,-20.9235407465149,
8.85482867757227));
#153611=CARTESIAN_POINT('Ctrl Pts',(-20.4353854517829,-20.8667961238597,
8.85914484031119));
#153612=CARTESIAN_POINT('Ctrl Pts',(-20.4983710832767,-20.8068840072891,
8.86346100305011));
#153613=CARTESIAN_POINT('Ctrl Pts',(-20.5593049644495,-20.7489235216142,
8.86763656724179));
#153614=CARTESIAN_POINT('Ctrl Pts',(-20.6173359087928,-20.6879991088312,
8.87181213143347));
#153615=CARTESIAN_POINT('Ctrl Pts',(-20.6721781340607,-20.6244429797901,
8.87598769562515));
#153616=CARTESIAN_POINT('Ctrl Pts',(-20.7297903097518,-20.5576767817615,
8.8803741576377));
#153617=CARTESIAN_POINT('Ctrl Pts',(-20.7838828183069,-20.4880064858705,
8.88476061965024));
#153618=CARTESIAN_POINT('Ctrl Pts',(-20.8341751072845,-20.4158526287652,
8.88914708166278));
#153619=CARTESIAN_POINT('Ctrl Pts',(-20.8844673962621,-20.3436987716599,
8.89353354367532));
#153620=CARTESIAN_POINT('Ctrl Pts',(-20.930959223453,-20.2690618860433,
8.89792000568786));
#153621=CARTESIAN_POINT('Ctrl Pts',(-20.9734262024012,-20.1923911818451,
8.9023064677004));
#153622=CARTESIAN_POINT('Ctrl Pts',(-21.0159038253685,-20.1157012607291,
8.90669402914565));
#153623=CARTESIAN_POINT('Ctrl Pts',(-21.0545007977188,-20.0367143701651,
8.9110815905909));
#153624=CARTESIAN_POINT('Ctrl Pts',(-21.0889748257324,-19.9558394145314,
8.91546915203614));
#153625=CARTESIAN_POINT('Ctrl Pts',(-21.1233545067051,-19.8751857940067,
8.91984470579146));
#153626=CARTESIAN_POINT('Ctrl Pts',(-21.1536335666925,-19.7926547636184,
8.92422025954678));
#153627=CARTESIAN_POINT('Ctrl Pts',(-21.1796158858339,-19.7086788876113,
8.92859581330209));
#153628=CARTESIAN_POINT('Ctrl Pts',(-21.2055560013419,-19.6248394154053,
8.9329642597524));
#153629=CARTESIAN_POINT('Ctrl Pts',(-21.227213143681,-19.5395601416149,
8.9373327062027));
#153630=CARTESIAN_POINT('Ctrl Pts',(-21.2444392039472,-19.4532933305808,
8.94170115265301));
#153631=CARTESIAN_POINT('Ctrl Pts',(-21.2616295048391,-19.3672055997974,
8.94606053069709));
#153632=CARTESIAN_POINT('Ctrl Pts',(-21.2744069696189,-19.2801348014838,
8.95041990874118));
#153633=CARTESIAN_POINT('Ctrl Pts',(-21.2826736357251,-19.1925466660746,
8.95477928678526));
#153634=CARTESIAN_POINT('Ctrl Pts',(-21.2902149496553,-19.1126438833585,
8.95875615459968));
#153635=CARTESIAN_POINT('Ctrl Pts',(-21.2940028463113,-19.0323109723971,
8.9627330224141));
#153636=CARTESIAN_POINT('Ctrl Pts',(-21.293999998394,-18.95190932191,8.96670989022851));
#153637=CARTESIAN_POINT('Ctrl Pts',(-21.293999998394,-18.9519093211995,
8.96670989026365));
#153638=CARTESIAN_POINT('Ctrl Pts',(-21.2939968622717,-18.8633718327361,
8.97108917708312));
#153639=CARTESIAN_POINT('Ctrl Pts',(-21.2893963356695,-18.7749281972304,
8.97546846390259));
#153640=CARTESIAN_POINT('Ctrl Pts',(-21.2802532223815,-18.6870575014991,
8.97984775072206));
#153641=CARTESIAN_POINT('Ctrl Pts',(-21.2710840473103,-18.5989363367038,
8.98423952038192));
#153642=CARTESIAN_POINT('Ctrl Pts',(-21.2573464424812,-18.5113917635122,
8.98863129004178));
#153643=CARTESIAN_POINT('Ctrl Pts',(-21.2391468026208,-18.4248951742595,
8.99302305970165));
#153644=CARTESIAN_POINT('Ctrl Pts',(-21.2209205771356,-18.3382722327336,
8.99742124475991));
#153645=CARTESIAN_POINT('Ctrl Pts',(-21.1982194166656,-18.2527007028949,
9.00181942981817));
#153646=CARTESIAN_POINT('Ctrl Pts',(-21.1711995861976,-18.1686366251616,
9.00621761487642));
#153647=CARTESIAN_POINT('Ctrl Pts',(-21.1441046030878,-18.0843387325816,
9.01062803299538));
#153648=CARTESIAN_POINT('Ctrl Pts',(-21.1126670698913,-18.0015570394273,
9.01503845111433));
#153649=CARTESIAN_POINT('Ctrl Pts',(-21.0770917883152,-17.9207285170577,
9.01944886923329));
#153650=CARTESIAN_POINT('Ctrl Pts',(-21.0501146625114,-17.859435362938,
9.02279333761614));
#153651=CARTESIAN_POINT('Ctrl Pts',(-21.0207591774504,-17.7992649146786,
9.02613780599899));
#153652=CARTESIAN_POINT('Ctrl Pts',(-20.9891316170539,-17.7403971815138,
9.02948227438184));
#153653=CARTESIAN_POINT('Ctrl Pts',(-20.949558877278,-17.6667412480012,
9.03366690877489));
#153654=CARTESIAN_POINT('Ctrl Pts',(-20.9063001320241,-17.5948890389388,
9.03785154316794));
#153655=CARTESIAN_POINT('Ctrl Pts',(-20.8595440286336,-17.5252335221418,
9.04203617756098));
#153656=CARTESIAN_POINT('Ctrl Pts',(-20.812854476769,-17.4556771513512,
9.04621485564493));
#153657=CARTESIAN_POINT('Ctrl Pts',(-20.7626777089518,-17.3883116408712,
9.05039353372888));
#153658=CARTESIAN_POINT('Ctrl Pts',(-20.7092482964897,-17.3235055519854,
9.05457221181283));
#153659=CARTESIAN_POINT('Ctrl Pts',(-20.6548612002084,-17.2575378605317,
9.05882578969826));
#153660=CARTESIAN_POINT('Ctrl Pts',(-20.5971039332157,-17.1942226731584,
9.06307936758369));
#153661=CARTESIAN_POINT('Ctrl Pts',(-20.5362701954422,-17.1339180044286,
9.06733294546913));
#153662=CARTESIAN_POINT('Ctrl Pts',(-20.4766158383827,-17.0747824593771,
9.07150405944708));
#153663=CARTESIAN_POINT('Ctrl Pts',(-20.4140035745828,-17.0185420838701,
9.07567517342503));
#153664=CARTESIAN_POINT('Ctrl Pts',(-20.3487498736144,-16.9654998500724,
9.07984628740299));
#153665=CARTESIAN_POINT('Ctrl Pts',(-20.2835180691556,-16.9124754151086,
9.08401600172336));
#153666=CARTESIAN_POINT('Ctrl Pts',(-20.2156469445306,-16.8626472804563,
9.08818571604373));
#153667=CARTESIAN_POINT('Ctrl Pts',(-20.1454869304126,-16.8162788933771,
9.0923554303641));
#153668=CARTESIAN_POINT('Ctrl Pts',(-20.0753294128889,-16.7699121562841,
9.09652499630815));
#153669=CARTESIAN_POINT('Ctrl Pts',(-20.0028835520724,-16.7270051749182,
9.10069456225219));
#153670=CARTESIAN_POINT('Ctrl Pts',(-19.9285285607302,-16.687777944282,
9.10486412819624));
#153671=CARTESIAN_POINT('Ctrl Pts',(-19.8515593396191,-16.6471715326087,
9.10918029093515));
#153672=CARTESIAN_POINT('Ctrl Pts',(-19.7725447065605,-16.6105086923156,
9.11349645367407));
#153673=CARTESIAN_POINT('Ctrl Pts',(-19.6919309796755,-16.577980573336,
9.11781261641299));
#153674=CARTESIAN_POINT('Ctrl Pts',(-19.6139432364648,-16.5465120544109,
9.12198818060467));
#153675=CARTESIAN_POINT('Ctrl Pts',(-19.5344594409716,-16.5189131263824,
9.12616374479635));
#153676=CARTESIAN_POINT('Ctrl Pts',(-19.4539003149004,-16.4953063812094,
9.13033930898803));
#153677=CARTESIAN_POINT('Ctrl Pts',(-19.3692723388825,-16.4705073154575,
9.13472577100056));
#153678=CARTESIAN_POINT('Ctrl Pts',(-19.2834581156085,-16.4501144565313,
9.1391122330131));
#153679=CARTESIAN_POINT('Ctrl Pts',(-19.1969566012278,-16.4342090663878,
9.14349869502564));
#153680=CARTESIAN_POINT('Ctrl Pts',(-19.1104550868471,-16.4183036762444,
9.14788515703818));
#153681=CARTESIAN_POINT('Ctrl Pts',(-19.0232668665414,-16.406885754803,
9.15227161905072));
#153682=CARTESIAN_POINT('Ctrl Pts',(-18.9358937423135,-16.3999735665917,
9.15665808106326));
#153683=CARTESIAN_POINT('Ctrl Pts',(-18.8525407850493,-16.3933794184063,
9.16084271545631));
#153684=CARTESIAN_POINT('Ctrl Pts',(-18.7687093097475,-16.3908609393394,
9.16502734984936));
#153685=CARTESIAN_POINT('Ctrl Pts',(-18.68483185138,-16.3924722128562,9.1692119842424));
#153686=CARTESIAN_POINT('Ctrl Pts',(-18.6010737821926,-16.3940811929246,
9.17339066232635));
#153687=CARTESIAN_POINT('Ctrl Pts',(-18.5172703159603,-16.3998082408783,
9.1775693404103));
#153688=CARTESIAN_POINT('Ctrl Pts',(-18.4338583233965,-16.4096556146018,
9.18174801849425));
#153689=CARTESIAN_POINT('Ctrl Pts',(-18.3489512308132,-16.4196794954222,
9.18600159637968));
#153690=CARTESIAN_POINT('Ctrl Pts',(-18.264450264908,-16.4339729066197,
9.19025517426512));
#153691=CARTESIAN_POINT('Ctrl Pts',(-18.1808154334733,-16.4524826795246,
9.19450875215055));
#153692=CARTESIAN_POINT('Ctrl Pts',(-18.0988020264459,-16.4706336043628,
9.1986798661285));
#153693=CARTESIAN_POINT('Ctrl Pts',(-18.0176219400175,-16.4928387610342,
9.20285098010646));
#153694=CARTESIAN_POINT('Ctrl Pts',(-17.9377012248092,-16.5189960417974,
9.20702209408441));
#153695=CARTESIAN_POINT('Ctrl Pts',(-17.8578073277689,-16.5451445452324,
9.21119180840478));
#153696=CARTESIAN_POINT('Ctrl Pts',(-17.7791723995178,-16.5752423959817,
9.21536152272515));
#153697=CARTESIAN_POINT('Ctrl Pts',(-17.7022076389884,-16.609137536312,
9.21953123704553));
#153698=CARTESIAN_POINT('Ctrl Pts',(-17.6252456171954,-16.6430314705078,
9.22370080298957));
#153699=CARTESIAN_POINT('Ctrl Pts',(-17.5499540656281,-16.6807222394303,
9.22787036893362));
#153700=CARTESIAN_POINT('Ctrl Pts',(-17.4767232259473,-16.7220100642766,
9.23203993487766));
#153701=CARTESIAN_POINT('Ctrl Pts',(-17.4009176802834,-16.7647495181104,
9.23635609761658));
#153702=CARTESIAN_POINT('Ctrl Pts',(-17.3273209113735,-16.811343420091,
9.2406722603555));
#153703=CARTESIAN_POINT('Ctrl Pts',(-17.2563352295956,-16.8615199531434,
9.24498842309442));
#153704=CARTESIAN_POINT('Ctrl Pts',(-17.1876618989352,-16.9100619909092,
9.2491639872861));
#153705=CARTESIAN_POINT('Ctrl Pts',(-17.1214324971171,-16.9619565080489,
9.25333955147778));
#153706=CARTESIAN_POINT('Ctrl Pts',(-17.0579778332574,-17.0169161008919,
9.25751511566946));
#153707=CARTESIAN_POINT('Ctrl Pts',(-16.9913182251753,-17.0746515721154,
9.261901577682));
#153708=CARTESIAN_POINT('Ctrl Pts',(-16.9277214465955,-17.135769485738,
9.26628803969454));
#153709=CARTESIAN_POINT('Ctrl Pts',(-16.8675259014641,-17.1998942841556,
9.27067450170708));
#153710=CARTESIAN_POINT('Ctrl Pts',(-16.8073303563327,-17.2640190825733,
9.27506096371962));
#153711=CARTESIAN_POINT('Ctrl Pts',(-16.7505363613297,-17.3311502736972,
9.27944742573217));
#153712=CARTESIAN_POINT('Ctrl Pts',(-16.6974308899392,-17.4008758076974,
9.28383388774471));
#153713=CARTESIAN_POINT('Ctrl Pts',(-16.6467688800086,-17.4673931665203,
9.28801852213775));
#153714=CARTESIAN_POINT('Ctrl Pts',(-16.5992748500801,-17.5365189656784,
9.2922031565308));
#153715=CARTESIAN_POINT('Ctrl Pts',(-16.5552283987657,-17.6079187860643,
9.29638779092385));
#153716=CARTESIAN_POINT('Ctrl Pts',(-16.5112446421229,-17.6792169776433,
9.3005664690078));
#153717=CARTESIAN_POINT('Ctrl Pts',(-16.4706989563139,-17.7527823729939,
9.30474514709174));
#153718=CARTESIAN_POINT('Ctrl Pts',(-16.4338297096935,-17.8282488551323,
9.30892382517568));
#153719=CARTESIAN_POINT('Ctrl Pts',(-16.3962996083249,-17.9050680197263,
9.31317740306112));
#153720=CARTESIAN_POINT('Ctrl Pts',(-16.3625793350038,-17.9838567118701,
9.31743098094656));
#153721=CARTESIAN_POINT('Ctrl Pts',(-16.3328731767861,-18.0641993586154,
9.32168455883199));
#153722=CARTESIAN_POINT('Ctrl Pts',(-16.3037429304123,-18.1429844063778,
9.32585567280995));
#153723=CARTESIAN_POINT('Ctrl Pts',(-16.2784727120491,-18.223263242189,
9.33002678678789));
#153724=CARTESIAN_POINT('Ctrl Pts',(-16.2572072783656,-18.3046223559168,
9.33419790076585));
#153725=CARTESIAN_POINT('Ctrl Pts',(-16.2359489805037,-18.3859541688082,
9.33836761508622));
#153726=CARTESIAN_POINT('Ctrl Pts',(-16.2186929146628,-18.4683650949799,
9.34253732940659));
#153727=CARTESIAN_POINT('Ctrl Pts',(-16.2055337985359,-18.5514270752364,
9.34670704372697));
#153728=CARTESIAN_POINT('Ctrl Pts',(-16.1923751506668,-18.6344860997912,
9.35087660967101));
#153729=CARTESIAN_POINT('Ctrl Pts',(-16.183313233791,-18.7181956778687,
9.35504617561505));
#153730=CARTESIAN_POINT('Ctrl Pts',(-16.1783912959603,-18.8021195415123,
9.3592157415591));
#153731=CARTESIAN_POINT('Ctrl Pts',(-16.1732963088673,-18.8889940646704,
9.36353190429802));
#153732=CARTESIAN_POINT('Ctrl Pts',(-16.1726378716504,-18.9760976958013,
9.36784806703694));
#153733=CARTESIAN_POINT('Ctrl Pts',(-16.1764051921424,-19.0629450261169,
9.37216422977586));
#153734=CARTESIAN_POINT('Ctrl Pts',(-16.1800497925657,-19.1469633137821,
9.37633979396754));
#153735=CARTESIAN_POINT('Ctrl Pts',(-16.1878361499306,-19.2307412775514,
9.38051535815922));
#153736=CARTESIAN_POINT('Ctrl Pts',(-16.1997016639331,-19.3138451931539,
9.3846909223509));
#153737=CARTESIAN_POINT('Ctrl Pts',(-16.2121664768403,-19.4011464899727,
9.38907738436344));
#153738=CARTESIAN_POINT('Ctrl Pts',(-16.2291332400404,-19.487703283801,
9.39346384637598));
#153739=CARTESIAN_POINT('Ctrl Pts',(-16.2504693406595,-19.5730277482654,
9.39785030838853));
#153740=CARTESIAN_POINT('Ctrl Pts',(-16.2718054412786,-19.6583522127299,
9.40223677040107));
#153741=CARTESIAN_POINT('Ctrl Pts',(-16.2975106369606,-19.7424438151944,
9.4066232324136));
#153742=CARTESIAN_POINT('Ctrl Pts',(-16.3273937923111,-19.8248382216157,
9.41100969442614));
#153743=CARTESIAN_POINT('Ctrl Pts',(-16.3558995253323,-19.9034347728948,
9.41519396859567));
#153744=CARTESIAN_POINT('Ctrl Pts',(-16.3883126378462,-19.9807796693235,
9.4193782427652));
#153745=CARTESIAN_POINT('Ctrl Pts',(-16.4245033134343,-20.0564569048823,
9.42356251693473));
#153746=CARTESIAN_POINT('Ctrl Pts',(-16.4606449440058,-20.1320315838787,
9.42774112064377));
#153747=CARTESIAN_POINT('Ctrl Pts',(-16.5005537757621,-20.2059426782427,
9.4319197243528));
#153748=CARTESIAN_POINT('Ctrl Pts',(-16.5440510006887,-20.2777916051988,
9.43609832806183));
#153749=CARTESIAN_POINT('Ctrl Pts',(-16.5874980215242,-20.3495576047938,
9.44027210886545));
#153750=CARTESIAN_POINT('Ctrl Pts',(-16.6345249665291,-20.4192657763403,
9.44444588966907));
#153751=CARTESIAN_POINT('Ctrl Pts',(-16.6849066106161,-20.48654106546,9.44861967047269));
#153752=CARTESIAN_POINT('Ctrl Pts',(-16.7352537173085,-20.5537702363309,
9.45279059008516));
#153753=CARTESIAN_POINT('Ctrl Pts',(-16.7889506803368,-20.6185694703229,
9.45696150969763));
#153754=CARTESIAN_POINT('Ctrl Pts',(-16.8457290001202,-20.6805926735391,
9.4611324293101));
#153755=CARTESIAN_POINT('Ctrl Pts',(-16.9024956626461,-20.7426031426614,
9.46530249258366));
#153756=CARTESIAN_POINT('Ctrl Pts',(-16.9623421216309,-20.8018383679809,
9.46947255585723));
#153757=CARTESIAN_POINT('Ctrl Pts',(-17.0249603575963,-20.8579862278339,
9.47364261913079));
#153758=CARTESIAN_POINT('Ctrl Pts',(-17.0732023522128,-20.9012433511144,
9.47685529618713));
#153759=CARTESIAN_POINT('Ctrl Pts',(-17.1230886546779,-20.9426686481572,
9.48006797324345));
#153760=CARTESIAN_POINT('Ctrl Pts',(-17.1744641402402,-20.9821349467765,
9.48328065029978));
#153761=CARTESIAN_POINT('Origin',(-18.734,-18.952,-1.76670989022851));
#153762=CARTESIAN_POINT('',(-17.1744641402401,-20.9821349467765,10.3499274704374));
#153763=CARTESIAN_POINT('',(-17.1744641402401,-20.9821349467765,10.2832382127855));
#153764=CARTESIAN_POINT('',(-17.1744641402401,-20.9821349467765,-1.76670989022851));
#153765=CARTESIAN_POINT('',(-21.2939992159918,-18.9540035272626,9.8332901097715));
#153766=CARTESIAN_POINT('Ctrl Pts',(-21.2939992159918,-18.9540035272626,
9.8332901097715));
#153767=CARTESIAN_POINT('Ctrl Pts',(-21.2940649620946,-18.8699966984849,
9.83745593779552));
#153768=CARTESIAN_POINT('Ctrl Pts',(-21.2899913508454,-18.7859395799201,
9.84162176581954));
#153769=CARTESIAN_POINT('Ctrl Pts',(-21.281790209728,-18.7022700514273,
9.84578759384357));
#153770=CARTESIAN_POINT('Ctrl Pts',(-21.2735905258927,-18.6186153903907,
9.84995268163077));
#153771=CARTESIAN_POINT('Ctrl Pts',(-21.2612648140692,-18.5353486407622,
9.85411776941798));
#153772=CARTESIAN_POINT('Ctrl Pts',(-21.244876840873,-18.4529033260305,
9.85828285720518));
#153773=CARTESIAN_POINT('Ctrl Pts',(-21.2284868533626,-18.3704478776001,
9.86244845694076));
#153774=CARTESIAN_POINT('Ctrl Pts',(-21.2080337038202,-18.2888145159798,
9.86661405667634));
#153775=CARTESIAN_POINT('Ctrl Pts',(-21.183632148948,-18.2084259721853,
9.87077965641192));
#153776=CARTESIAN_POINT('Ctrl Pts',(-21.1592030081949,-18.1279465493957,
9.87494996534485));
#153777=CARTESIAN_POINT('Ctrl Pts',(-21.1308166833998,-18.0487151959126,
9.87912027427778));
#153778=CARTESIAN_POINT('Ctrl Pts',(-21.0986375209737,-17.9711384427947,
9.88329058321071));
#153779=CARTESIAN_POINT('Ctrl Pts',(-21.0664396371008,-17.8935165564616,
9.88746331837886));
#153780=CARTESIAN_POINT('Ctrl Pts',(-21.0304447198543,-17.8175516031279,
9.89163605354701));
#153781=CARTESIAN_POINT('Ctrl Pts',(-20.9908638255707,-17.7436268486802,
9.89580878871516));
#153782=CARTESIAN_POINT('Ctrl Pts',(-20.951210438291,-17.6695666999462,
9.89998916630977));
#153783=CARTESIAN_POINT('Ctrl Pts',(-20.9079581930336,-17.5975546086432,
9.90416954390439));
#153784=CARTESIAN_POINT('Ctrl Pts',(-20.8613622504217,-17.5279459787351,
9.90834992149901));
#153785=CARTESIAN_POINT('Ctrl Pts',(-20.8243993123259,-17.4727278774585,
9.91166606942059));
#153786=CARTESIAN_POINT('Ctrl Pts',(-20.7853331875372,-17.4190216712153,
9.91498221734217));
#153787=CARTESIAN_POINT('Ctrl Pts',(-20.7443085775785,-17.3669891410737,
9.91829836526374));
#153788=CARTESIAN_POINT('Ctrl Pts',(-20.6925397790042,-17.3013294900759,
9.92248299965679));
#153789=CARTESIAN_POINT('Ctrl Pts',(-20.6374544461771,-17.2380865845811,
9.92666763404984));
#153790=CARTESIAN_POINT('Ctrl Pts',(-20.5793066365797,-17.1776146368404,
9.93085226844289));
#153791=CARTESIAN_POINT('Ctrl Pts',(-20.521241593192,-17.1172287634325,
9.93503094652683));
#153792=CARTESIAN_POINT('Ctrl Pts',(-20.4601230476225,-17.0596063422905,
9.93920962461077));
#153793=CARTESIAN_POINT('Ctrl Pts',(-20.3962460420502,-17.0050695709172,
9.94338830269472));
#153794=CARTESIAN_POINT('Ctrl Pts',(-20.3312240870606,-16.949555267112,
9.94764188058015));
#153795=CARTESIAN_POINT('Ctrl Pts',(-20.263344107106,-16.8972387002909,
9.95189545846559));
#153796=CARTESIAN_POINT('Ctrl Pts',(-20.1929575410584,-16.8484214078412,
9.95614903635103));
#153797=CARTESIAN_POINT('Ctrl Pts',(-20.1239355559416,-16.8005505338647,
9.96032015032898));
#153798=CARTESIAN_POINT('Ctrl Pts',(-20.0525037029719,-16.7560447387741,
9.96449126430694));
#153799=CARTESIAN_POINT('Ctrl Pts',(-19.9790262804937,-16.7151473984905,
9.96866237828489));
#153800=CARTESIAN_POINT('Ctrl Pts',(-19.9055735140743,-16.6742637817043,
9.97283209260526));
#153801=CARTESIAN_POINT('Ctrl Pts',(-19.8300769429974,-16.6369864384996,
9.97700180692563));
#153802=CARTESIAN_POINT('Ctrl Pts',(-19.7529274425305,-16.6035139202332,
9.981171521246));
#153803=CARTESIAN_POINT('Ctrl Pts',(-19.675780687374,-16.5700425930628,
9.98534108719005));
#153804=CARTESIAN_POINT('Ctrl Pts',(-19.5969815421364,-16.5403760039565,
9.9895106531341));
#153805=CARTESIAN_POINT('Ctrl Pts',(-19.5169416763858,-16.5146649119626,
9.99368021907814));
#153806=CARTESIAN_POINT('Ctrl Pts',(-19.4340877076953,-16.4880498496923,
9.99799638181706));
#153807=CARTESIAN_POINT('Ctrl Pts',(-19.3499046498554,-16.4656737716516,
10.002312544556));
#153808=CARTESIAN_POINT('Ctrl Pts',(-19.2648652451189,-16.4476473707713,
10.0066287072949));
#153809=CARTESIAN_POINT('Ctrl Pts',(-19.1825959900471,-16.4302081780036,
10.0108042714866));
#153810=CARTESIAN_POINT('Ctrl Pts',(-19.0995257948676,-16.4168396609884,
10.0149798356783));
#153811=CARTESIAN_POINT('Ctrl Pts',(-19.0160902825551,-16.4075894449818,
10.01915539987));
#153812=CARTESIAN_POINT('Ctrl Pts',(-18.9284406408648,-16.397872022555,
10.0235418618825));
#153813=CARTESIAN_POINT('Ctrl Pts',(-18.8403883907188,-16.3926998996315,
10.027928323895));
#153814=CARTESIAN_POINT('Ctrl Pts',(-18.7524390182801,-16.3920664066025,
10.0323147859076));
#153815=CARTESIAN_POINT('Ctrl Pts',(-18.6644896458415,-16.3914329135735,
10.0367012479201));
#153816=CARTESIAN_POINT('Ctrl Pts',(-18.5766437273767,-16.395337948682,
10.0410877099327));
#153817=CARTESIAN_POINT('Ctrl Pts',(-18.4893986055749,-16.403712308658,
10.0454741719452));
#153818=CARTESIAN_POINT('Ctrl Pts',(-18.4061677611554,-16.4117013519176,
10.0496588063382));
#153819=CARTESIAN_POINT('Ctrl Pts',(-18.3231738401578,-16.4237872141345,
10.0538434407313));
#153820=CARTESIAN_POINT('Ctrl Pts',(-18.2408521955264,-16.4399480015448,
10.0580280751243));
#153821=CARTESIAN_POINT('Ctrl Pts',(-18.1586477255668,-16.4560857860745,
10.0622067532083));
#153822=CARTESIAN_POINT('Ctrl Pts',(-18.0771140788203,-16.4762868870104,
10.0663854312922));
#153823=CARTESIAN_POINT('Ctrl Pts',(-17.9966818731335,-16.5004776199688,
10.0705641093762));
#153824=CARTESIAN_POINT('Ctrl Pts',(-17.9148079779654,-16.5251019544298,
10.0748176872616));
#153825=CARTESIAN_POINT('Ctrl Pts',(-17.8340758788413,-16.5538603099738,
10.079071265147));
#153826=CARTESIAN_POINT('Ctrl Pts',(-17.7549293481803,-16.5866203985945,
10.0833248430325));
#153827=CARTESIAN_POINT('Ctrl Pts',(-17.677317227458,-16.6187453689711,
10.0874959570104));
#153828=CARTESIAN_POINT('Ctrl Pts',(-17.6012301897814,-16.6547181102195,
10.0916670709884));
#153829=CARTESIAN_POINT('Ctrl Pts',(-17.5270700635694,-16.6943640398533,
10.0958381849663));
#153830=CARTESIAN_POINT('Ctrl Pts',(-17.452934822504,-16.7339966659125,
10.1000078992867));
#153831=CARTESIAN_POINT('Ctrl Pts',(-17.380725614118,-16.7772998157408,
10.1041776136071));
#153832=CARTESIAN_POINT('Ctrl Pts',(-17.3108209620502,-16.8240522971792,
10.1083473279274));
#153833=CARTESIAN_POINT('Ctrl Pts',(-17.24091879749,-16.8708031149637,10.1125168938715));
#153834=CARTESIAN_POINT('Ctrl Pts',(-17.1733214081181,-16.9210027638615,
10.1166864598155));
#153835=CARTESIAN_POINT('Ctrl Pts',(-17.1083783873652,-16.9743866979274,
10.1208560257596));
#153836=CARTESIAN_POINT('Ctrl Pts',(-17.0411520501183,-17.029647545259,
10.1251721884985));
#153837=CARTESIAN_POINT('Ctrl Pts',(-16.9767706170265,-17.088320427997,
10.1294883512374));
#153838=CARTESIAN_POINT('Ctrl Pts',(-16.9155830497419,-17.1500677607041,
10.1338045139763));
#153839=CARTESIAN_POINT('Ctrl Pts',(-16.8563886610259,-17.2098036805428,
10.137980078168));
#153840=CARTESIAN_POINT('Ctrl Pts',(-16.8001835327301,-17.2724164438389,
10.1421556423597));
#153841=CARTESIAN_POINT('Ctrl Pts',(-16.7472435046119,-17.3375655392575,
10.1463312065513));
#153842=CARTESIAN_POINT('Ctrl Pts',(-16.6916296015263,-17.4060051606084,
10.1507176685639));
#153843=CARTESIAN_POINT('Ctrl Pts',(-16.6396196516928,-17.4772435963691,
10.1551041305764));
#153844=CARTESIAN_POINT('Ctrl Pts',(-16.5914816570985,-17.5508522025387,
10.159490592589));
#153845=CARTESIAN_POINT('Ctrl Pts',(-16.5433436625043,-17.6244608087082,
10.1638770546015));
#153846=CARTESIAN_POINT('Ctrl Pts',(-16.49907784951,-17.7004390456585,10.1682635166141));
#153847=CARTESIAN_POINT('Ctrl Pts',(-16.4588952312818,-17.7783312684767,
10.1726499786266));
#153848=CARTESIAN_POINT('Ctrl Pts',(-16.4205614748832,-17.8526395546591,
10.1768346130196));
#153849=CARTESIAN_POINT('Ctrl Pts',(-16.3858007370466,-17.9289661561368,
10.1810192474127));
#153850=CARTESIAN_POINT('Ctrl Pts',(-16.3548302568731,-18.0069331593007,
10.1852038818057));
#153851=CARTESIAN_POINT('Ctrl Pts',(-16.3239038593448,-18.0847891860859,
10.1893825598897));
#153852=CARTESIAN_POINT('Ctrl Pts',(-16.2967571717624,-18.1642805528127,
10.1935612379736));
#153853=CARTESIAN_POINT('Ctrl Pts',(-16.2735613224931,-18.2450052940595,
10.1977399160576));
#153854=CARTESIAN_POINT('Ctrl Pts',(-16.2499497042961,-18.3271769682774,
10.201993493943));
#153855=CARTESIAN_POINT('Ctrl Pts',(-16.2304321761497,-18.4106262399197,
10.2062470718284));
#153856=CARTESIAN_POINT('Ctrl Pts',(-16.2151377103691,-18.4949083616217,
10.2105006497139));
#153857=CARTESIAN_POINT('Ctrl Pts',(-16.2001397576524,-18.5775565099315,
10.2146717636918));
#153858=CARTESIAN_POINT('Ctrl Pts',(-16.1892026698429,-18.6610050301436,
10.2188428776698));
#153859=CARTESIAN_POINT('Ctrl Pts',(-16.1823971528,-18.7448215499598,10.2230139916477));
#153860=CARTESIAN_POINT('Ctrl Pts',(-16.1755939194141,-18.8286099443332,
10.2271837059681));
#153861=CARTESIAN_POINT('Ctrl Pts',(-16.1729195406043,-18.9127656349237,
10.2313534202885));
#153862=CARTESIAN_POINT('Ctrl Pts',(-16.1743929164357,-18.9968506161333,
10.2355231346088));
#153863=CARTESIAN_POINT('Ctrl Pts',(-16.1758662398381,-19.0809326052385,
10.2396927005529));
#153864=CARTESIAN_POINT('Ctrl Pts',(-16.1814870155134,-19.1649434300184,
10.2438622664969));
#153865=CARTESIAN_POINT('Ctrl Pts',(-16.1912220304804,-19.2484459440194,
10.248031832441));
#153866=CARTESIAN_POINT('Ctrl Pts',(-16.2012993165641,-19.3348843034011,
10.2523479951799));
#153867=CARTESIAN_POINT('Ctrl Pts',(-16.2157854771197,-19.4207774186556,
10.2566641579188));
#153868=CARTESIAN_POINT('Ctrl Pts',(-16.2345855425419,-19.505649139663,
10.2609803206577));
#153869=CARTESIAN_POINT('Ctrl Pts',(-16.2527731978104,-19.5877561732855,
10.2651558848494));
#153870=CARTESIAN_POINT('Ctrl Pts',(-16.274997853126,-19.6689068927551,
10.2693314490411));
#153871=CARTESIAN_POINT('Ctrl Pts',(-16.3011224991718,-19.7486850481613,
10.2735070132328));
#153872=CARTESIAN_POINT('Ctrl Pts',(-16.3285666389839,-19.8324926085424,
10.2778934752453));
#153873=CARTESIAN_POINT('Ctrl Pts',(-16.3603148903336,-19.9147847597328,
10.2822799372579));
#153874=CARTESIAN_POINT('Ctrl Pts',(-16.3961518958431,-19.9951041376056,
10.2866663992704));
#153875=CARTESIAN_POINT('Ctrl Pts',(-16.4319889013526,-20.0754235154785,
10.2910528612829));
#153876=CARTESIAN_POINT('Ctrl Pts',(-16.4719143298048,-20.1537696376098,
10.2954393232955));
#153877=CARTESIAN_POINT('Ctrl Pts',(-16.5156592733601,-20.2297184433711,
10.299825785308));
#153878=CARTESIAN_POINT('Ctrl Pts',(-16.5573791055785,-20.3021513047724,
10.3040091821608));
#153879=CARTESIAN_POINT('Ctrl Pts',(-16.6027278790407,-20.3726734305059,
10.3081925790136));
#153880=CARTESIAN_POINT('Ctrl Pts',(-16.6515056001626,-20.4408979396339,
10.3123759758664));
#153881=CARTESIAN_POINT('Ctrl Pts',(-16.7002227477719,-20.5090377256943,
10.3165541776622));
#153882=CARTESIAN_POINT('Ctrl Pts',(-16.7523601281892,-20.5748851865602,
10.320732379458));
#153883=CARTESIAN_POINT('Ctrl Pts',(-16.8076724802166,-20.6380789680573,
10.3249105812538));
#153884=CARTESIAN_POINT('Ctrl Pts',(-16.8629267562013,-20.7012063982853,
10.3290843960833));
#153885=CARTESIAN_POINT('Ctrl Pts',(-16.9213490806984,-20.761685339555,
10.3332582109128));
#153886=CARTESIAN_POINT('Ctrl Pts',(-16.9826524926142,-20.8191855580991,
10.3374320257423));
#153887=CARTESIAN_POINT('Ctrl Pts',(-17.0438286128232,-20.8765663819678,
10.341597173974));
#153888=CARTESIAN_POINT('Ctrl Pts',(-17.1078735520966,-20.9309805098277,
10.3457623222057));
#153889=CARTESIAN_POINT('Ctrl Pts',(-17.1744641402401,-20.9821349467765,
10.3499274704374));
#153890=CARTESIAN_POINT('Ctrl Pts',(-17.1725833834245,-20.9846205132764,
9.54996331522893));
#153891=CARTESIAN_POINT('Ctrl Pts',(-17.7798204361626,-21.4438297111124,
9.58795779411958));
#153892=CARTESIAN_POINT('Ctrl Pts',(-19.5298543219429,-21.8241544890203,
9.66834420857071));
#153893=CARTESIAN_POINT('Ctrl Pts',(-21.1196059552395,-20.3720005573578,
9.76278617060466));
#153894=CARTESIAN_POINT('Ctrl Pts',(-21.2937096219977,-19.2372014343179,
9.81923365374796));
#153895=CARTESIAN_POINT('Ctrl Pts',(-21.2916488755515,-18.9540199903513,
9.83328920133079));
#153896=CARTESIAN_POINT('',(-21.2939989766127,-18.9497109517324,9.7667098901893));
#153897=CARTESIAN_POINT('Ctrl Pts',(-17.1744641402402,-20.9821349467765,
9.48328065029978));
#153898=CARTESIAN_POINT('Ctrl Pts',(-17.2411530785286,-21.0333649356377,
9.48745092761406));
#153899=CARTESIAN_POINT('Ctrl Pts',(-17.3103520349426,-21.0812924251398,
9.49162120492833));
#153900=CARTESIAN_POINT('Ctrl Pts',(-17.3816948054842,-21.125676760902,
9.49579148224261));
#153901=CARTESIAN_POINT('Ctrl Pts',(-17.4531169624092,-21.170110485157,
9.49996640001634));
#153902=CARTESIAN_POINT('Ctrl Pts',(-17.5266873027709,-21.2109929445286,
9.50414131779007));
#153903=CARTESIAN_POINT('Ctrl Pts',(-17.6020133887381,-21.2481285486496,
9.5083162355638));
#153904=CARTESIAN_POINT('Ctrl Pts',(-17.6773879055774,-21.2852880290901,
9.51249383759898));
#153905=CARTESIAN_POINT('Ctrl Pts',(-17.7545199929606,-21.3186956771203,
9.51667143963415));
#153906=CARTESIAN_POINT('Ctrl Pts',(-17.8329977297368,-21.3482042711298,
9.52084904166933));
#153907=CARTESIAN_POINT('Ctrl Pts',(-17.9116029975094,-21.377760818362,
9.52503343255664));
#153908=CARTESIAN_POINT('Ctrl Pts',(-17.9915578414719,-21.4034055266289,
9.52921782344394));
#153909=CARTESIAN_POINT('Ctrl Pts',(-18.0724361918796,-21.4250413113786,
9.53340221433124));
#153910=CARTESIAN_POINT('Ctrl Pts',(-18.1032542451651,-21.4332854553792,
9.53499664325669));
#153911=CARTESIAN_POINT('Ctrl Pts',(-18.1342062953107,-21.4409480643631,
9.53659107218214));
#153912=CARTESIAN_POINT('Ctrl Pts',(-18.1652685194105,-21.4480257416514,
9.53818550110758));
#153913=CARTESIAN_POINT('Ctrl Pts',(-18.2467924112678,-21.4666013528503,
9.54237013550063));
#153914=CARTESIAN_POINT('Ctrl Pts',(-18.3293790330749,-21.4812132961356,
9.54655476989367));
#153915=CARTESIAN_POINT('Ctrl Pts',(-18.4126082132397,-21.4917455225678,
9.55073940428672));
#153916=CARTESIAN_POINT('Ctrl Pts',(-18.4957189269683,-21.5022627576792,
9.55491808237066));
#153917=CARTESIAN_POINT('Ctrl Pts',(-18.5794699298769,-21.508711753151,
9.55909676045461));
#153918=CARTESIAN_POINT('Ctrl Pts',(-18.663429267508,-21.5110271142986,
9.56327543853855));
#153919=CARTESIAN_POINT('Ctrl Pts',(-18.7488935159257,-21.5133839766308,
9.56752901642398));
#153920=CARTESIAN_POINT('Ctrl Pts',(-18.8345731712378,-21.5114574491382,
9.57178259430942));
#153921=CARTESIAN_POINT('Ctrl Pts',(-18.9200053717026,-21.5052336363321,
9.57603617219486));
#153922=CARTESIAN_POINT('Ctrl Pts',(-19.0037813022541,-21.499130484282,
9.58020728617281));
#153923=CARTESIAN_POINT('Ctrl Pts',(-19.0873188071793,-21.4888952174951,
9.58437840015076));
#153924=CARTESIAN_POINT('Ctrl Pts',(-19.1701815497897,-21.4745672747467,
9.58854951412871));
#153925=CARTESIAN_POINT('Ctrl Pts',(-19.2530164870065,-21.4602441398779,
9.59271922844908));
#153926=CARTESIAN_POINT('Ctrl Pts',(-19.3351766586592,-21.4418311348332,
9.59688894276945));
#153927=CARTESIAN_POINT('Ctrl Pts',(-19.4162332022014,-21.4194192707795,
9.60105865708982));
#153928=CARTESIAN_POINT('Ctrl Pts',(-19.497286861404,-21.3970082042361,
9.60522822303387));
#153929=CARTESIAN_POINT('Ctrl Pts',(-19.5772365274095,-21.3705986850247,
9.60939778897791));
#153930=CARTESIAN_POINT('Ctrl Pts',(-19.6556671754965,-21.3403319739124,
9.61356735492196));
#153931=CARTESIAN_POINT('Ctrl Pts',(-19.7368553484155,-21.3090011225755,
9.61788351766088));
#153932=CARTESIAN_POINT('Ctrl Pts',(-19.8164152065819,-21.2735369848544,
9.6221996803998));
#153933=CARTESIAN_POINT('Ctrl Pts',(-19.8939093684295,-21.2341503581117,
9.62651584313872));
#153934=CARTESIAN_POINT('Ctrl Pts',(-19.9688791661059,-21.1960467465925,
9.63069140733039));
#153935=CARTESIAN_POINT('Ctrl Pts',(-20.0419153954164,-21.1542725466308,
9.63486697152208));
#153936=CARTESIAN_POINT('Ctrl Pts',(-20.112649171425,-21.1090643157146,
9.63904253571376));
#153937=CARTESIAN_POINT('Ctrl Pts',(-20.1869555423062,-21.0615727245271,
9.6434289977263));
#153938=CARTESIAN_POINT('Ctrl Pts',(-20.2587202783153,-21.0102914191921,
9.64781545973884));
#153939=CARTESIAN_POINT('Ctrl Pts',(-20.3275542346358,-20.9555430869523,
9.65220192175138));
#153940=CARTESIAN_POINT('Ctrl Pts',(-20.3963881909563,-20.9007947547124,
9.65658838376392));
#153941=CARTESIAN_POINT('Ctrl Pts',(-20.4622909830917,-20.8425798367028,
9.66097484577646));
#153942=CARTESIAN_POINT('Ctrl Pts',(-20.5249190804939,-20.7812645645513,
9.665361307789));
#153943=CARTESIAN_POINT('Ctrl Pts',(-20.5852113014986,-20.722236203594,
9.66958416538901));
#153944=CARTESIAN_POINT('Ctrl Pts',(-20.6427127908697,-20.6600954577448,
9.67380702298902));
#153945=CARTESIAN_POINT('Ctrl Pts',(-20.6970796830689,-20.5951427685755,
9.67802988058904));
#153946=CARTESIAN_POINT('Ctrl Pts',(-20.7500936846377,-20.5318063918539,
9.68214765466763));
#153947=CARTESIAN_POINT('Ctrl Pts',(-20.8001269202378,-20.465796754398,
9.68626542874623));
#153948=CARTESIAN_POINT('Ctrl Pts',(-20.8468954124061,-20.3974317611819,
9.69038320282483));
#153949=CARTESIAN_POINT('Ctrl Pts',(-20.89361966769,-20.3291314323191,9.69449708202704));
#153950=CARTESIAN_POINT('Ctrl Pts',(-20.9370850392269,-20.2584805564847,
9.69861096122924));
#153951=CARTESIAN_POINT('Ctrl Pts',(-20.9770478427321,-20.1858299620349,
9.70272484043145));
#153952=CARTESIAN_POINT('Ctrl Pts',(-21.0169856434319,-20.1132248215702,
9.70683614577717));
#153953=CARTESIAN_POINT('Ctrl Pts',(-21.0534249974543,-20.038622860247,
9.71094745112288));
#153954=CARTESIAN_POINT('Ctrl Pts',(-21.0861664418207,-19.9624024099201,
9.7150587564686));
#153955=CARTESIAN_POINT('Ctrl Pts',(-21.1204445396302,-19.88260470698,9.71936301761199));
#153956=CARTESIAN_POINT('Ctrl Pts',(-21.1506688210158,-19.8010333411259,
9.72366727875538));
#153957=CARTESIAN_POINT('Ctrl Pts',(-21.1766659614561,-19.7181481584811,
9.72797153989877));
#153958=CARTESIAN_POINT('Ctrl Pts',(-21.2014998963995,-19.6389715567968,
9.73208321292912));
#153959=CARTESIAN_POINT('Ctrl Pts',(-21.222476755318,-19.5585966865054,
9.73619488595946));
#153960=CARTESIAN_POINT('Ctrl Pts',(-21.2394965458156,-19.4774398718274,
9.74030655898981));
#153961=CARTESIAN_POINT('Ctrl Pts',(-21.2565208804896,-19.3962613887936,
9.74441932981082));
#153962=CARTESIAN_POINT('Ctrl Pts',(-21.2695859645564,-19.3143010135805,
9.74853210063183));
#153963=CARTESIAN_POINT('Ctrl Pts',(-21.2786432445868,-19.2319834955467,
9.75264487145285));
#153964=CARTESIAN_POINT('Ctrl Pts',(-21.2877094512626,-19.1495848472747,
9.75676169572548));
#153965=CARTESIAN_POINT('Ctrl Pts',(-21.2927599450141,-19.066828826857,
9.76087851999811));
#153966=CARTESIAN_POINT('Ctrl Pts',(-21.2937982075177,-18.9841424452888,
9.76499534427074));
#153967=CARTESIAN_POINT('Ctrl Pts',(-21.2939423435977,-18.9726635650768,
9.76556685957692));
#153968=CARTESIAN_POINT('Ctrl Pts',(-21.2940092371596,-18.9611860219109,
9.76613837488311));
#153969=CARTESIAN_POINT('Ctrl Pts',(-21.2939989766127,-18.9497109517324,
9.7667098901893));
#153970=CARTESIAN_POINT('Ctrl Pts',(-21.293998976612,-18.9497109509451,
9.76670989022851));
#153971=CARTESIAN_POINT('Ctrl Pts',(-21.2938920610985,-18.8301400729742,
9.77266511192846));
#153972=CARTESIAN_POINT('Ctrl Pts',(-21.2854044483395,-18.7109297707717,
9.77862033362841));
#153973=CARTESIAN_POINT('Ctrl Pts',(-21.2687069780221,-18.5930285031284,
9.78457555532836));
#153974=CARTESIAN_POINT('Ctrl Pts',(-21.2612660069352,-18.5404876147807,
9.78722940837572));
#153975=CARTESIAN_POINT('Ctrl Pts',(-21.2521952261608,-18.4882062515499,
9.78988326142308));
#153976=CARTESIAN_POINT('Ctrl Pts',(-21.2415125421986,-18.4362666864387,
9.79253711447044));
#153977=CARTESIAN_POINT('Ctrl Pts',(-21.2246679295087,-18.3543676186888,
9.79672174886349));
#153978=CARTESIAN_POINT('Ctrl Pts',(-21.2037753333229,-18.2731422629634,
9.80090638325654));
#153979=CARTESIAN_POINT('Ctrl Pts',(-21.1789030820534,-18.1930211337819,
9.80509101764958));
#153980=CARTESIAN_POINT('Ctrl Pts',(-21.1540662333551,-18.1130140471107,
9.80926969573353));
#153981=CARTESIAN_POINT('Ctrl Pts',(-21.125261116367,-18.0341085006255,
9.81344837381748));
#153982=CARTESIAN_POINT('Ctrl Pts',(-21.0926070466711,-17.9567247619913,
9.81762705190143));
#153983=CARTESIAN_POINT('Ctrl Pts',(-21.059367676244,-17.8779539754568,
9.82188062978687));
#153984=CARTESIAN_POINT('Ctrl Pts',(-21.022140108072,-17.8007605624569,
9.8261342076723));
#153985=CARTESIAN_POINT('Ctrl Pts',(-20.9811033321017,-17.7255716022296,
9.83038778555774));
#153986=CARTESIAN_POINT('Ctrl Pts',(-20.9408621341102,-17.6518403267155,
9.83455889953569));
#153987=CARTESIAN_POINT('Ctrl Pts',(-20.8969583386824,-17.5800368994828,
9.83873001351364));
#153988=CARTESIAN_POINT('Ctrl Pts',(-20.8496085018329,-17.5105421730164,
9.84290112749159));
#153989=CARTESIAN_POINT('Ctrl Pts',(-20.8022745536785,-17.4410707661766,
9.84707084181197));
#153990=CARTESIAN_POINT('Ctrl Pts',(-20.7514971194517,-17.3739069013821,
9.85124055613235));
#153991=CARTESIAN_POINT('Ctrl Pts',(-20.69753660511,-17.3094032751789,9.85541027045272));
#153992=CARTESIAN_POINT('Ctrl Pts',(-20.643578010915,-17.2449019442916,
9.85957983639677));
#153993=CARTESIAN_POINT('Ctrl Pts',(-20.5864368576392,-17.1830610160831,
9.86374940234081));
#153994=CARTESIAN_POINT('Ctrl Pts',(-20.5264135623406,-17.1241997862082,
9.86791896828485));
#153995=CARTESIAN_POINT('Ctrl Pts',(-20.4642799220261,-17.063269068104,
9.87223513102377));
#153996=CARTESIAN_POINT('Ctrl Pts',(-20.3990580731256,-17.0055318485508,
9.87655129376269));
#153997=CARTESIAN_POINT('Ctrl Pts',(-20.3311209857106,-16.9512989836053,
9.88086745650161));
#153998=CARTESIAN_POINT('Ctrl Pts',(-20.2653969417724,-16.8988327485311,
9.88504302069329));
#153999=CARTESIAN_POINT('Ctrl Pts',(-20.1971322502977,-16.84964630251,9.88921858488496));
#154000=CARTESIAN_POINT('Ctrl Pts',(-20.1266949702185,-16.8039774861682,
9.89339414907664));
#154001=CARTESIAN_POINT('Ctrl Pts',(-20.0527000705712,-16.7560020464804,
9.89778061108918));
#154002=CARTESIAN_POINT('Ctrl Pts',(-19.9763078452048,-16.7119092180967,
9.90216707310172));
#154003=CARTESIAN_POINT('Ctrl Pts',(-19.8979731420051,-16.6719196231951,
9.90655353511426));
#154004=CARTESIAN_POINT('Ctrl Pts',(-19.8196384388055,-16.6319300282936,
9.9109399971268));
#154005=CARTESIAN_POINT('Ctrl Pts',(-19.7393618185146,-16.5960438342244,
9.91532645913934));
#154006=CARTESIAN_POINT('Ctrl Pts',(-19.6576188802165,-16.5644221134992,
9.91971292115188));
#154007=CARTESIAN_POINT('Ctrl Pts',(-19.5796370556816,-16.5342553550192,
9.92389755554493));
#154008=CARTESIAN_POINT('Ctrl Pts',(-19.5000306196518,-16.5078569775931,
9.92808218993798));
#154009=CARTESIAN_POINT('Ctrl Pts',(-19.4191985515812,-16.4854025571831,
9.93226682433103));
#154010=CARTESIAN_POINT('Ctrl Pts',(-19.3384815379545,-16.4629800978612,
9.93644550241497));
#154011=CARTESIAN_POINT('Ctrl Pts',(-19.2565427969406,-16.4444905669892,
9.94062418049891));
#154012=CARTESIAN_POINT('Ctrl Pts',(-19.1738002903985,-16.4300611219609,
9.94480285858285));
#154013=CARTESIAN_POINT('Ctrl Pts',(-19.0895746838926,-16.4153730395006,
9.94905643646829));
#154014=CARTESIAN_POINT('Ctrl Pts',(-19.0045166631073,-16.404892202575,
9.95331001435372));
#154015=CARTESIAN_POINT('Ctrl Pts',(-18.9190822179583,-16.3986992788558,
9.95756359223916));
#154016=CARTESIAN_POINT('Ctrl Pts',(-18.8353040862402,-16.3926264170474,
9.96173470621711));
#154017=CARTESIAN_POINT('Ctrl Pts',(-18.7511644753125,-16.3906767277746,
9.96590582019506));
#154018=CARTESIAN_POINT('Ctrl Pts',(-18.6671008395072,-16.3928742699263,
9.97007693417301));
#154019=CARTESIAN_POINT('Ctrl Pts',(-18.5830654120668,-16.3950710746715,
9.97424664849338));
#154020=CARTESIAN_POINT('Ctrl Pts',(-18.4991063686099,-16.4014123350032,
9.97841636281375));
#154021=CARTESIAN_POINT('Ctrl Pts',(-18.4156612239222,-16.4118699986723,
9.98258607713413));
#154022=CARTESIAN_POINT('Ctrl Pts',(-18.3322190485708,-16.4223272902127,
9.98675564307817));
#154023=CARTESIAN_POINT('Ctrl Pts',(-18.2492911919861,-16.4369006358009,
9.99092520902222));
#154024=CARTESIAN_POINT('Ctrl Pts',(-18.1673087413395,-16.4555102609148,
9.99509477496626));
#154025=CARTESIAN_POINT('Ctrl Pts',(-18.0824438888645,-16.4747741774902,
9.99941093770518));
#154026=CARTESIAN_POINT('Ctrl Pts',(-17.9985926745536,-16.498363368963,
10.0037271004441));
#154027=CARTESIAN_POINT('Ctrl Pts',(-17.9162183607824,-16.5261324870145,
10.008043263183));
#154028=CARTESIAN_POINT('Ctrl Pts',(-17.836527381618,-16.5529970289662,
10.0122188273747));
#154029=CARTESIAN_POINT('Ctrl Pts',(-17.7582189816851,-16.5837731410384,
10.0163943915664));
#154030=CARTESIAN_POINT('Ctrl Pts',(-17.6816923706303,-16.6182800825355,
10.0205699557581));
#154031=CARTESIAN_POINT('Ctrl Pts',(-17.6013005823759,-16.6545298876153,
10.0249564177706));
#154032=CARTESIAN_POINT('Ctrl Pts',(-17.5228758288488,-16.6948970480992,
10.0293428797831));
#154033=CARTESIAN_POINT('Ctrl Pts',(-17.4468498189204,-16.7391185274971,
10.0337293417957));
#154034=CARTESIAN_POINT('Ctrl Pts',(-17.3708238089919,-16.7833400068949,
10.0381158038082));
#154035=CARTESIAN_POINT('Ctrl Pts',(-17.2971969868961,-16.8314154242948,
10.0425022658208));
#154036=CARTESIAN_POINT('Ctrl Pts',(-17.2263622218887,-16.8830320616279,
10.0468887278333));
#154037=CARTESIAN_POINT('Ctrl Pts',(-17.1587866694216,-16.9322737409631,
10.0510733622264));
#154038=CARTESIAN_POINT('Ctrl Pts',(-17.0935003576726,-16.9849212146566,
10.0552579966194));
#154039=CARTESIAN_POINT('Ctrl Pts',(-17.0308668782516,-17.0407340400657,
10.0594426310125));
#154040=CARTESIAN_POINT('Ctrl Pts',(-16.9683225498361,-17.0964674228261,
10.0636213090964));
#154041=CARTESIAN_POINT('Ctrl Pts',(-16.9084238939848,-17.1553569045525,
10.0677999871804));
#154042=CARTESIAN_POINT('Ctrl Pts',(-16.8515040647696,-17.2171198733512,
10.0719786652643));
#154043=CARTESIAN_POINT('Ctrl Pts',(-16.7935639885233,-17.2799898989772,
10.0762322431497));
#154044=CARTESIAN_POINT('Ctrl Pts',(-16.7387109698991,-17.345837155491,
10.0804858210352));
#154045=CARTESIAN_POINT('Ctrl Pts',(-16.687259656336,-17.4143218914161,
10.0847393989206));
#154046=CARTESIAN_POINT('Ctrl Pts',(-16.6368058268853,-17.4814789170983,
10.0889105128986));
#154047=CARTESIAN_POINT('Ctrl Pts',(-16.5896232711907,-17.5511716846818,
10.0930816268765));
#154048=CARTESIAN_POINT('Ctrl Pts',(-16.5459690047032,-17.6230453869223,
10.0972527408545));
#154049=CARTESIAN_POINT('Ctrl Pts',(-16.5023293868265,-17.6948949712479,
10.1014224551748));
#154050=CARTESIAN_POINT('Ctrl Pts',(-16.4622159454253,-17.7689236439344,
10.1055921694952));
#154051=CARTESIAN_POINT('Ctrl Pts',(-16.4258419114526,-17.8447483401352,
10.1097618838156));
#154052=CARTESIAN_POINT('Ctrl Pts',(-16.3894691718242,-17.9205703381678,
10.1139314497596));
#154053=CARTESIAN_POINT('Ctrl Pts',(-16.3568357732638,-17.9981878174993,
10.1181010157037));
#154054=CARTESIAN_POINT('Ctrl Pts',(-16.3281079773328,-18.0771951216036,
10.1222705816477));
#154055=CARTESIAN_POINT('Ctrl Pts',(-16.2983701475363,-18.1589802250542,
10.1265867443867));
#154056=CARTESIAN_POINT('Ctrl Pts',(-16.2728178525521,-18.2422542084871,
10.1309029071256));
#154057=CARTESIAN_POINT('Ctrl Pts',(-16.2515796325832,-18.3265488672692,
10.1352190698645));
#154058=CARTESIAN_POINT('Ctrl Pts',(-16.231033245396,-18.4080976364077,
10.1393946340562));
#154059=CARTESIAN_POINT('Ctrl Pts',(-16.2145242335759,-18.4906011339278,
10.1435701982479));
#154060=CARTESIAN_POINT('Ctrl Pts',(-16.2021167074112,-18.5736258561826,
10.1477457624395));
#154061=CARTESIAN_POINT('Ctrl Pts',(-16.189082506596,-18.660843959786,10.1521322244521));
#154062=CARTESIAN_POINT('Ctrl Pts',(-16.1805750686802,-18.7486367448621,
10.1565186864646));
#154063=CARTESIAN_POINT('Ctrl Pts',(-16.176606897426,-18.8364988359063,
10.1609051484772));
#154064=CARTESIAN_POINT('Ctrl Pts',(-16.1726387261718,-18.9243609269505,
10.1652916104897));
#154065=CARTESIAN_POINT('Ctrl Pts',(-16.173209741748,-19.0122917442521,
10.1696780725022));
#154066=CARTESIAN_POINT('Ctrl Pts',(-16.1782696504243,-19.0997916785801,
10.1740645345148));
#154067=CARTESIAN_POINT('Ctrl Pts',(-16.1830972264459,-19.1832739332768,
10.1782495861009));
#154068=CARTESIAN_POINT('Ctrl Pts',(-16.192028478113,-19.2666747744999,
10.1824346376871));
#154069=CARTESIAN_POINT('Ctrl Pts',(-16.2050580322525,-19.3495582017334,
10.1866196892733));
#154070=CARTESIAN_POINT('Ctrl Pts',(-16.218065180498,-19.4322991008905,
10.1907975441571));
#154071=CARTESIAN_POINT('Ctrl Pts',(-16.2351565463996,-19.5145239047392,
10.1949753990409));
#154072=CARTESIAN_POINT('Ctrl Pts',(-16.2562748618458,-19.5957997668208,
10.1991532539248));
#154073=CARTESIAN_POINT('Ctrl Pts',(-16.2773725113785,-19.6769960941531,
10.2033270204528));
#154074=CARTESIAN_POINT('Ctrl Pts',(-16.3024891716641,-19.7572448807793,
10.2075007869809));
#154075=CARTESIAN_POINT('Ctrl Pts',(-16.3315163412368,-19.8361223158454,
10.211674553509));
#154076=CARTESIAN_POINT('Ctrl Pts',(-16.3605238139077,-19.9149462272259,
10.2158454878535));
#154077=CARTESIAN_POINT('Ctrl Pts',(-16.3934363672028,-19.9924002048188,
10.2200164221981));
#154078=CARTESIAN_POINT('Ctrl Pts',(-16.4300957454804,-20.0680757976081,
10.2241873565427));
#154079=CARTESIAN_POINT('Ctrl Pts',(-16.4667412452146,-20.1437227410571,
10.2283567118509));
#154080=CARTESIAN_POINT('Ctrl Pts',(-16.5071305503819,-20.2175922243166,
10.2325260671591));
#154081=CARTESIAN_POINT('Ctrl Pts',(-16.5510579279926,-20.2892972408032,
10.2366954224672));
#154082=CARTESIAN_POINT('Ctrl Pts',(-16.5950001276811,-20.3610264521632,
10.240866184609));
#154083=CARTESIAN_POINT('Ctrl Pts',(-16.6424825511957,-20.4305893408586,
10.2450369467507));
#154084=CARTESIAN_POINT('Ctrl Pts',(-16.6932547035596,-20.497625645186,
10.2492077088924));
#154085=CARTESIAN_POINT('Ctrl Pts',(-16.7440345632818,-20.5646721258164,
10.2533791041678));
#154086=CARTESIAN_POINT('Ctrl Pts',(-16.7981048585996,-20.6291908988194,
10.2575504994432));
#154087=CARTESIAN_POINT('Ctrl Pts',(-16.8551743953647,-20.6908543203405,
10.2617218947185));
#154088=CARTESIAN_POINT('Ctrl Pts',(-16.9123064332259,-20.7525852740627,
10.2658978583993));
#154089=CARTESIAN_POINT('Ctrl Pts',(-16.9724439504671,-20.8114543015288,
10.27007382208));
#154090=CARTESIAN_POINT('Ctrl Pts',(-17.0352588291791,-20.8671706019459,
10.2742497857607));
#154091=CARTESIAN_POINT('Ctrl Pts',(-17.0803268259774,-20.9071455585216,
10.2772459281023));
#154092=CARTESIAN_POINT('Ctrl Pts',(-17.1267722730037,-20.9454983787039,
10.2802420704439));
#154093=CARTESIAN_POINT('Ctrl Pts',(-17.1744641402401,-20.9821349467765,
10.2832382127855));
#154094=CARTESIAN_POINT('Origin',(-18.734,-18.952,-1.76670989022851));
#154095=CARTESIAN_POINT('',(-17.1757180887844,-20.9805344762227,11.1497835108638));
#154096=CARTESIAN_POINT('',(-17.1731949481218,-20.9838169785964,11.0834063298428));
#154097=CARTESIAN_POINT('',(-17.1744641402401,-20.9821349467765,-1.76670989022851));
#154098=CARTESIAN_POINT('',(-21.2939995125392,-18.9504201902087,10.6332901097715));
#154099=CARTESIAN_POINT('Ctrl Pts',(-21.2907951936029,-18.9504028914923,
10.633291065733));
#154100=CARTESIAN_POINT('Ctrl Pts',(-21.2926071610387,-18.6273578228792,
10.6493117789394));
#154101=CARTESIAN_POINT('Ctrl Pts',(-21.0857645521851,-17.4517521226135,
10.7077244277063));
#154102=CARTESIAN_POINT('Ctrl Pts',(-19.3189847766872,-15.9819690623319,
10.8085290120338));
#154103=CARTESIAN_POINT('Ctrl Pts',(-16.553315163514,-16.8524989631863,
10.9357048187152));
#154104=CARTESIAN_POINT('Ctrl Pts',(-15.869042517464,-19.3539801303507,
11.0494563183253));
#154105=CARTESIAN_POINT('Ctrl Pts',(-16.7160809834605,-20.6211555874542,
11.1208158823748));
#154106=CARTESIAN_POINT('Ctrl Pts',(-17.1757180887841,-20.9805344762225,
11.1497835108638));
#154107=CARTESIAN_POINT('Ctrl Pts',(-17.1744641402401,-20.9821349467765,
10.3499274704374));
#154108=CARTESIAN_POINT('Ctrl Pts',(-17.2411279928465,-21.0333456649873,
10.3540972012588));
#154109=CARTESIAN_POINT('Ctrl Pts',(-17.3103427550984,-21.0812892113262,
10.3582669320803));
#154110=CARTESIAN_POINT('Ctrl Pts',(-17.3817509985227,-21.1257117191577,
10.3624366629017));
#154111=CARTESIAN_POINT('Ctrl Pts',(-17.453156251782,-21.1701323668311,
10.366606219119));
#154112=CARTESIAN_POINT('Ctrl Pts',(-17.526754412567,-21.2110320268083,
10.3707757753362));
#154113=CARTESIAN_POINT('Ctrl Pts',(-17.6021604511976,-21.2482010442831,
10.3749453315534));
#154114=CARTESIAN_POINT('Ctrl Pts',(-17.6806131725609,-21.2868718274757,
10.3792833532564));
#154115=CARTESIAN_POINT('Ctrl Pts',(-17.7610224891159,-21.321503848979,
10.3836213749594));
#154116=CARTESIAN_POINT('Ctrl Pts',(-17.8429301077372,-21.3519155083258,
10.3879593966624));
#154117=CARTESIAN_POINT('Ctrl Pts',(-17.9217695912436,-21.3811879930572,
10.3921349226545));
#154118=CARTESIAN_POINT('Ctrl Pts',(-18.0019966600383,-21.4065505716589,
10.3963104486466));
#154119=CARTESIAN_POINT('Ctrl Pts',(-18.0831873454017,-21.427892341887,
10.4004859746387));
#154120=CARTESIAN_POINT('Ctrl Pts',(-18.1644360817491,-21.4492493713872,
10.4046644861136));
#154121=CARTESIAN_POINT('Ctrl Pts',(-18.2466493563219,-21.4665797778481,
10.4088429975885));
#154122=CARTESIAN_POINT('Ctrl Pts',(-18.3293941447886,-21.4798239855513,
10.4130215090634));
#154123=CARTESIAN_POINT('Ctrl Pts',(-18.4122671639293,-21.4930887179754,
10.4172064960318));
#154124=CARTESIAN_POINT('Ctrl Pts',(-18.4956728843019,-21.5022545728989,
10.4213914830002));
#154125=CARTESIAN_POINT('Ctrl Pts',(-18.5791750022087,-21.5073139181046,
10.4255764699687));
#154126=CARTESIAN_POINT('Ctrl Pts',(-18.5886533835364,-21.5078882077673,
10.4260515106423));
#154127=CARTESIAN_POINT('Ctrl Pts',(-18.5981330099311,-21.5084096415651,
10.4265265513159));
#154128=CARTESIAN_POINT('Ctrl Pts',(-18.607613246377,-21.5088782506229,
10.4270015919895));
#154129=CARTESIAN_POINT('Ctrl Pts',(-18.6911246711664,-21.5130062288976,
10.4311862263825));
#154130=CARTESIAN_POINT('Ctrl Pts',(-18.7749939587053,-21.5130461767751,
10.4353708607756));
#154131=CARTESIAN_POINT('Ctrl Pts',(-18.8587871646377,-21.5089568169098,
10.4395554951686));
#154132=CARTESIAN_POINT('Ctrl Pts',(-18.9424611013132,-21.5048732777422,
10.4437341732526));
#154133=CARTESIAN_POINT('Ctrl Pts',(-19.0260587159297,-21.496672127745,
10.4479128513366));
#154134=CARTESIAN_POINT('Ctrl Pts',(-19.1091432618602,-21.4843640206497,
10.4520915294205));
#154135=CARTESIAN_POINT('Ctrl Pts',(-19.1937170385644,-21.4718352995804,
10.4563451073059));
#154136=CARTESIAN_POINT('Ctrl Pts',(-19.2777586906012,-21.4550509150071,
10.4605986851914));
#154137=CARTESIAN_POINT('Ctrl Pts',(-19.3608099823642,-21.4340776067659,
10.4648522630768));
#154138=CARTESIAN_POINT('Ctrl Pts',(-19.4422511627753,-21.4135109070309,
10.4690233770548));
#154139=CARTESIAN_POINT('Ctrl Pts',(-19.5227395737981,-21.388916372956,
10.4731944910327));
#154140=CARTESIAN_POINT('Ctrl Pts',(-19.6018523684388,-21.3604086585535,
10.4773656050107));
#154141=CARTESIAN_POINT('Ctrl Pts',(-19.6809386160172,-21.3319105101898,
10.481535319331));
#154142=CARTESIAN_POINT('Ctrl Pts',(-19.7586497315295,-21.2995019451702,
10.4857050336514));
#154143=CARTESIAN_POINT('Ctrl Pts',(-19.834579189332,-21.2633471067776,
10.4898747479718));
#154144=CARTESIAN_POINT('Ctrl Pts',(-19.9105059452386,-21.2271935549294,
10.4940443139158));
#154145=CARTESIAN_POINT('Ctrl Pts',(-19.9846507545054,-21.1872941933034,
10.4982138798599));
#154146=CARTESIAN_POINT('Ctrl Pts',(-20.0566294498849,-21.1438602460689,
10.5023834458039));
#154147=CARTESIAN_POINT('Ctrl Pts',(-20.1311388273984,-21.0988992148313,
10.5066996085428));
#154148=CARTESIAN_POINT('Ctrl Pts',(-20.203326484239,-21.0501506938732,
10.5110157712818));
#154149=CARTESIAN_POINT('Ctrl Pts',(-20.2727983186254,-20.9978982708326,
10.5153319340207));
#154150=CARTESIAN_POINT('Ctrl Pts',(-20.3400071153138,-20.9473479649765,
10.5195074982123));
#154151=CARTESIAN_POINT('Ctrl Pts',(-20.4046739763899,-20.8935188682638,
10.523683062404));
#154152=CARTESIAN_POINT('Ctrl Pts',(-20.4664767307277,-20.8367080350778,
10.5278586265957));
#154153=CARTESIAN_POINT('Ctrl Pts',(-20.5314009952649,-20.7770278217627,
10.5322450886082));
#154154=CARTESIAN_POINT('Ctrl Pts',(-20.5931638083648,-20.7140571577257,
10.5366315506208));
#154155=CARTESIAN_POINT('Ctrl Pts',(-20.6514380125593,-20.6481814372268,
10.5410180126333));
#154156=CARTESIAN_POINT('Ctrl Pts',(-20.7097122167537,-20.5823057167279,
10.5454044746458));
#154157=CARTESIAN_POINT('Ctrl Pts',(-20.7644975100436,-20.5135254409999,
10.5497909366584));
#154158=CARTESIAN_POINT('Ctrl Pts',(-20.8155192213965,-20.4422609606901,
10.5541773986709));
#154159=CARTESIAN_POINT('Ctrl Pts',(-20.8646271615163,-20.3736695367859,
10.5583993290636));
#154160=CARTESIAN_POINT('Ctrl Pts',(-20.9104308246501,-20.302523084569,
10.5626212594563));
#154161=CARTESIAN_POINT('Ctrl Pts',(-20.9526566798058,-20.2291697370174,
10.5668431898491));
#154162=CARTESIAN_POINT('Ctrl Pts',(-20.9948201353165,-20.1559247880485,
10.5710588812454));
#154163=CARTESIAN_POINT('Ctrl Pts',(-21.0334160638335,-20.0804798079433,
10.5752745726417));
#154164=CARTESIAN_POINT('Ctrl Pts',(-21.0682129788551,-20.003213474678,
10.5794902640381));
#154165=CARTESIAN_POINT('Ctrl Pts',(-21.1029682787105,-19.9260395476302,
10.583700913703));
#154166=CARTESIAN_POINT('Ctrl Pts',(-21.1339334100815,-19.8470490030809,
10.587911563368));
#154167=CARTESIAN_POINT('Ctrl Pts',(-21.1609223976385,-19.7666457364035,
10.592122213033));
#154168=CARTESIAN_POINT('Ctrl Pts',(-21.1878844462892,-19.6863227237952,
10.5963286598616));
#154169=CARTESIAN_POINT('Ctrl Pts',(-21.2108781024615,-19.6045902181226,
10.6005351066903));
#154170=CARTESIAN_POINT('Ctrl Pts',(-21.2297657078558,-19.5218715043685,
10.6047415535189));
#154171=CARTESIAN_POINT('Ctrl Pts',(-21.24864245849,-19.4392003292924,10.6089455828907));
#154172=CARTESIAN_POINT('Ctrl Pts',(-21.2634177498248,-19.3555445100527,
10.6131496122625));
#154173=CARTESIAN_POINT('Ctrl Pts',(-21.27400421321,-19.2713408788045,10.6173536416343));
#154174=CARTESIAN_POINT('Ctrl Pts',(-21.2845883389273,-19.1871558411237,
10.6215567426863));
#154175=CARTESIAN_POINT('Ctrl Pts',(-21.2909854180498,-19.1024236771956,
10.6257598437382));
#154176=CARTESIAN_POINT('Ctrl Pts',(-21.2931596531403,-19.0175886403171,
10.6299629447901));
#154177=CARTESIAN_POINT('Ctrl Pts',(-21.2937333596144,-18.99520356793,10.6310719997839));
#154178=CARTESIAN_POINT('Ctrl Pts',(-21.2940133304248,-18.9728113543426,
10.6321810547777));
#154179=CARTESIAN_POINT('Ctrl Pts',(-21.2939995125392,-18.9504201902087,
10.6332901097715));
#154180=CARTESIAN_POINT('',(-21.2940195635259,-18.9533010451044,10.566709896691));
#154181=CARTESIAN_POINT('Ctrl Pts',(-17.1744641402401,-20.9821349467765,
10.2832382127855));
#154182=CARTESIAN_POINT('Ctrl Pts',(-17.2410685654238,-21.0333000132453,
10.2874224972348));
#154183=CARTESIAN_POINT('Ctrl Pts',(-17.3101047703225,-21.0811157710451,
10.291606781684));
#154184=CARTESIAN_POINT('Ctrl Pts',(-17.3811935362982,-21.125364827121,
10.2957910661332));
#154185=CARTESIAN_POINT('Ctrl Pts',(-17.4120536307295,-21.1445736293875,
10.2976074911542));
#154186=CARTESIAN_POINT('Ctrl Pts',(-17.443300225641,-21.1631108865338,
10.2994239161752));
#154187=CARTESIAN_POINT('Ctrl Pts',(-17.4749010481802,-21.1809616034213,
10.3012403411962));
#154188=CARTESIAN_POINT('Ctrl Pts',(-17.5477022303472,-21.2220856371494,
10.3054249755892));
#154189=CARTESIAN_POINT('Ctrl Pts',(-17.622655768781,-21.2597157589185,
10.3096096099823));
#154190=CARTESIAN_POINT('Ctrl Pts',(-17.6993922596291,-21.2936205549928,
10.3137942443753));
#154191=CARTESIAN_POINT('Ctrl Pts',(-17.7760195255806,-21.3274770917864,
10.3179729224593));
#154192=CARTESIAN_POINT('Ctrl Pts',(-17.8544242858622,-21.3576186510691,
10.3221516005432));
#154193=CARTESIAN_POINT('Ctrl Pts',(-17.9342113535407,-21.3838589846031,
10.3263302786272));
#154194=CARTESIAN_POINT('Ctrl Pts',(-18.0154285470654,-21.4105696572571,
10.3305838565126));
#154195=CARTESIAN_POINT('Ctrl Pts',(-18.098077671342,-21.43323763244,10.334837434398));
#154196=CARTESIAN_POINT('Ctrl Pts',(-18.1817191896633,-21.4517171653077,
10.3390910122835));
#154197=CARTESIAN_POINT('Ctrl Pts',(-18.2637391539389,-21.4698384363709,
10.3432621262614));
#154198=CARTESIAN_POINT('Ctrl Pts',(-18.3467129067618,-21.4839321143086,
10.3474332402394));
#154199=CARTESIAN_POINT('Ctrl Pts',(-18.4302110680644,-21.4939111480997,
10.3516043542173));
#154200=CARTESIAN_POINT('Ctrl Pts',(-18.5136812107526,-21.5038868333296,
10.3557740685377));
#154201=CARTESIAN_POINT('Ctrl Pts',(-18.5976749560384,-21.5097505619763,
10.3599437828581));
#154202=CARTESIAN_POINT('Ctrl Pts',(-18.6817553300755,-21.5114668379302,
10.3641134971784));
#154203=CARTESIAN_POINT('Ctrl Pts',(-18.765832712172,-21.5131830528116,
10.3682830631225));
#154204=CARTESIAN_POINT('Ctrl Pts',(-18.8499962569364,-21.510752099899,
10.3724526290665));
#154205=CARTESIAN_POINT('Ctrl Pts',(-18.9338078728664,-21.5041905912256,
10.3766221950106));
#154206=CARTESIAN_POINT('Ctrl Pts',(-19.0205662018199,-21.4973983880018,
10.3809383577495));
#154207=CARTESIAN_POINT('Ctrl Pts',(-19.1069468680351,-21.4861798052051,
10.3852545204884));
#154208=CARTESIAN_POINT('Ctrl Pts',(-19.1924704625207,-21.4706116880131,
10.3895706832273));
#154209=CARTESIAN_POINT('Ctrl Pts',(-19.2752081349114,-21.4555507006011,
10.393746247419));
#154210=CARTESIAN_POINT('Ctrl Pts',(-19.3571432683312,-21.4364193523527,
10.3979218116107));
#154211=CARTESIAN_POINT('Ctrl Pts',(-19.4378547167232,-21.413338769399,
10.4020973758024));
#154212=CARTESIAN_POINT('Ctrl Pts',(-19.5226427085003,-21.3890924410692,
10.4064838378149));
#154213=CARTESIAN_POINT('Ctrl Pts',(-19.6060795975568,-21.3604876310562,
10.4108702998275));
#154214=CARTESIAN_POINT('Ctrl Pts',(-19.6877001821497,-21.3277221981048,
10.41525676184));
#154215=CARTESIAN_POINT('Ctrl Pts',(-19.7693207667425,-21.2949567651533,
10.4196432238525));
#154216=CARTESIAN_POINT('Ctrl Pts',(-19.8491245522345,-21.2580310219481,
10.4240296858651));
#154217=CARTESIAN_POINT('Ctrl Pts',(-19.9266775857364,-21.2171976020829,
10.4284161478776));
#154218=CARTESIAN_POINT('Ctrl Pts',(-20.0006622892057,-21.1782429883953,
10.4326007822707));
#154219=CARTESIAN_POINT('Ctrl Pts',(-20.0728741952655,-21.1355873954291,
10.4367854166637));
#154220=CARTESIAN_POINT('Ctrl Pts',(-20.1429187702871,-21.0894161734984,
10.4409700510568));
#154221=CARTESIAN_POINT('Ctrl Pts',(-20.212863645526,-21.0433106705873,
10.4451487291407));
#154222=CARTESIAN_POINT('Ctrl Pts',(-20.2806469365542,-20.9936997293726,
10.4493274072247));
#154223=CARTESIAN_POINT('Ctrl Pts',(-20.3458981308864,-20.9408148268869,
10.4535060853086));
#154224=CARTESIAN_POINT('Ctrl Pts',(-20.4123189059818,-20.8869820005318,
10.4577596631941));
#154225=CARTESIAN_POINT('Ctrl Pts',(-20.476115489232,-20.829756911557,10.4620132410795));
#154226=CARTESIAN_POINT('Ctrl Pts',(-20.5369274194047,-20.7694302518553,
10.4662668189649));
#154227=CARTESIAN_POINT('Ctrl Pts',(-20.5965603916463,-20.7102731421696,
10.4704379329429));
#154228=CARTESIAN_POINT('Ctrl Pts',(-20.6533230631004,-20.6481339874866,
10.4746090469208));
#154229=CARTESIAN_POINT('Ctrl Pts',(-20.7069098223475,-20.5833267094254,
10.4787801608988));
#154230=CARTESIAN_POINT('Ctrl Pts',(-20.7604786000401,-20.5185411780722,
10.4829498752192));
#154231=CARTESIAN_POINT('Ctrl Pts',(-20.8108732891326,-20.4510896556873,
10.4871195895395));
#154232=CARTESIAN_POINT('Ctrl Pts',(-20.8578275173592,-20.3813203547519,
10.4912893038599));
#154233=CARTESIAN_POINT('Ctrl Pts',(-20.9047800747528,-20.3115535365075,
10.4954588698039));
#154234=CARTESIAN_POINT('Ctrl Pts',(-20.948292158553,-20.2394694858254,
10.499628435748));
#154235=CARTESIAN_POINT('Ctrl Pts',(-20.9881406062299,-20.1654455601079,
10.503798001692));
#154236=CARTESIAN_POINT('Ctrl Pts',(-21.0293900761687,-20.0888190444805,
10.508114164431));
#154237=CARTESIAN_POINT('Ctrl Pts',(-21.0667132396993,-20.0101141681398,
10.5124303271699));
#154238=CARTESIAN_POINT('Ctrl Pts',(-21.0999152164605,-19.9297756330163,
10.5167464899088));
#154239=CARTESIAN_POINT('Ctrl Pts',(-21.132035642321,-19.8520541172245,
10.5209220541005));
#154240=CARTESIAN_POINT('Ctrl Pts',(-21.160299139743,-19.7728042005822,
10.5250976182921));
#154241=CARTESIAN_POINT('Ctrl Pts',(-21.1845795982613,-19.6924455635532,
10.5292731824838));
#154242=CARTESIAN_POINT('Ctrl Pts',(-21.210086405018,-19.6080282028024,
10.5336596444964));
#154243=CARTESIAN_POINT('Ctrl Pts',(-21.231197092147,-19.522387742153,10.5380461065089));
#154244=CARTESIAN_POINT('Ctrl Pts',(-21.2478262226603,-19.4360224398369,
10.5424325685214));
#154245=CARTESIAN_POINT('Ctrl Pts',(-21.2644553531735,-19.3496571375209,
10.546819030534));
#154246=CARTESIAN_POINT('Ctrl Pts',(-21.2766029222518,-19.2625675787001,
10.5512054925465));
#154247=CARTESIAN_POINT('Ctrl Pts',(-21.2842464642989,-19.1752553948527,
10.555591954559));
#154248=CARTESIAN_POINT('Ctrl Pts',(-21.2907042434478,-19.1014881810632,
10.5592979331155));
#154249=CARTESIAN_POINT('Ctrl Pts',(-21.293961988618,-19.0274367677245,
10.563003911672));
#154250=CARTESIAN_POINT('Ctrl Pts',(-21.2939996693303,-18.9533011644427,
10.5667098902285));
#154251=CARTESIAN_POINT('Ctrl Pts',(-21.2974134575541,-18.9532806863302,
10.5667109991706));
#154252=CARTESIAN_POINT('Ctrl Pts',(-21.2925956544959,-18.178366843738,
10.6053965865272));
#154253=CARTESIAN_POINT('Ctrl Pts',(-20.5048167981983,-16.5458335938225,
10.6864741094444));
#154254=CARTESIAN_POINT('Ctrl Pts',(-17.7257693559758,-16.0977467181734,
10.8099435679219));
#154255=CARTESIAN_POINT('Ctrl Pts',(-15.7882885603548,-18.254809249408,
10.9371193746034));
#154256=CARTESIAN_POINT('Ctrl Pts',(-16.3366273719947,-20.2593599478178,
11.028273628577));
#154257=CARTESIAN_POINT('Ctrl Pts',(-17.0711421117158,-20.9069199380455,
11.0770359469901));
#154258=CARTESIAN_POINT('Ctrl Pts',(-17.1731949481218,-20.9838169785965,
11.0834063298428));
#154259=CARTESIAN_POINT('Origin',(-18.734,-18.952,-1.76670989022851));
#154260=CARTESIAN_POINT('',(-17.1744641402401,-20.9821349467765,11.949868723648));
#154261=CARTESIAN_POINT('',(-17.1744641402401,-20.9821349467765,11.8833305046723));
#154262=CARTESIAN_POINT('',(-17.1744641402401,-20.9821349467765,-1.76670989022851));
#154263=CARTESIAN_POINT('',(-21.2940195831445,-18.9506989550129,11.4332901033027));
#154264=CARTESIAN_POINT('Ctrl Pts',(-21.2939996693303,-18.9506988355569,
11.4332901097715));
#154265=CARTESIAN_POINT('Ctrl Pts',(-21.293961988618,-18.8765632322752,
11.436996088328));
#154266=CARTESIAN_POINT('Ctrl Pts',(-21.2907042434478,-18.8025118189363,
11.4407020668845));
#154267=CARTESIAN_POINT('Ctrl Pts',(-21.2842464642989,-18.7287446051466,
11.444408045441));
#154268=CARTESIAN_POINT('Ctrl Pts',(-21.2769546129518,-18.6454497843058,
11.4485926798341));
#154269=CARTESIAN_POINT('Ctrl Pts',(-21.2655641024497,-18.5623575749322,
11.4527773142271));
#154270=CARTESIAN_POINT('Ctrl Pts',(-21.250093180474,-18.4799034980303,
11.4569619486201));
#154271=CARTESIAN_POINT('Ctrl Pts',(-21.2346442794409,-18.3975667843011,
11.4611406267041));
#154272=CARTESIAN_POINT('Ctrl Pts',(-21.2151265874821,-18.3158668471444,
11.465319304788));
#154273=CARTESIAN_POINT('Ctrl Pts',(-21.1916101807317,-18.2352349062881,
11.469497982872));
#154274=CARTESIAN_POINT('Ctrl Pts',(-21.1676722592913,-18.1531576958412,
11.4737515607574));
#154275=CARTESIAN_POINT('Ctrl Pts',(-21.1395909011584,-18.07218762626,11.4780051386429));
#154276=CARTESIAN_POINT('Ctrl Pts',(-21.1074946738889,-17.9927695620858,
11.4822587165283));
#154277=CARTESIAN_POINT('Ctrl Pts',(-21.0760206946157,-17.9148911720574,
11.4864298305062));
#154278=CARTESIAN_POINT('Ctrl Pts',(-21.0406863094724,-17.8385055933015,
11.4906009444842));
#154279=CARTESIAN_POINT('Ctrl Pts',(-21.0016627302193,-17.7640161019717,
11.4947720584621));
#154280=CARTESIAN_POINT('Ctrl Pts',(-20.962652245705,-17.6895516063101,
11.4989417727825));
#154281=CARTESIAN_POINT('Ctrl Pts',(-20.9199552389621,-17.6169823416316,
11.5031114871029));
#154282=CARTESIAN_POINT('Ctrl Pts',(-20.8737897249261,-17.5466886704004,
11.5072812014233));
#154283=CARTESIAN_POINT('Ctrl Pts',(-20.8276258536571,-17.4763975005198,
11.5114507673673));
#154284=CARTESIAN_POINT('Ctrl Pts',(-20.7779939737416,-17.4083821471397,
11.5156203333113));
#154285=CARTESIAN_POINT('Ctrl Pts',(-20.725155694621,-17.3429944065422,
11.5197898992554));
#154286=CARTESIAN_POINT('Ctrl Pts',(-20.6704596867895,-17.2753077136497,
11.5241060619943));
#154287=CARTESIAN_POINT('Ctrl Pts',(-20.6123279420988,-17.2104372553888,
11.5284222247332));
#154288=CARTESIAN_POINT('Ctrl Pts',(-20.5510951122123,-17.1487348078626,
11.5327383874721));
#154289=CARTESIAN_POINT('Ctrl Pts',(-20.4918569353188,-17.0890423110747,
11.5369139516638));
#154290=CARTESIAN_POINT('Ctrl Pts',(-20.4297169860238,-17.0323148814138,
11.5410895158555));
#154291=CARTESIAN_POINT('Ctrl Pts',(-20.3650134540526,-16.9788312001506,
11.5452650800472));
#154292=CARTESIAN_POINT('Ctrl Pts',(-20.2970419004996,-16.9226461852921,
11.5496515420597));
#154293=CARTESIAN_POINT('Ctrl Pts',(-20.2262414538865,-16.8700415621995,
11.5540380040722));
#154294=CARTESIAN_POINT('Ctrl Pts',(-20.1530384991427,-16.8212889126043,
11.5584244660848));
#154295=CARTESIAN_POINT('Ctrl Pts',(-20.0798355443989,-16.7725362630091,
11.5628109280973));
#154296=CARTESIAN_POINT('Ctrl Pts',(-20.0042306192382,-16.7276358177823,
11.5671973901099));
#154297=CARTESIAN_POINT('Ctrl Pts',(-19.9266775857363,-16.6868023979171,
11.5715838521224));
#154298=CARTESIAN_POINT('Ctrl Pts',(-19.852692882267,-16.6478477842295,
11.5757684865155));
#154299=CARTESIAN_POINT('Ctrl Pts',(-19.7766600165143,-16.6124491640088,
11.5799531209085));
#154300=CARTESIAN_POINT('Ctrl Pts',(-19.6989550698441,-16.5808269331021,
11.5841377553016));
#154301=CARTESIAN_POINT('Ctrl Pts',(-19.6213607265476,-16.549249712527,
11.5883164333855));
#154302=CARTESIAN_POINT('Ctrl Pts',(-19.5420994522192,-16.5214383763015,
11.5924951114694));
#154303=CARTESIAN_POINT('Ctrl Pts',(-19.4615717652903,-16.4975674125468,
11.5966737895534));
#154304=CARTESIAN_POINT('Ctrl Pts',(-19.3796006774474,-16.4732685789225,
11.6009273674388));
#154305=CARTESIAN_POINT('Ctrl Pts',(-19.2963177561687,-16.4530529941954,
11.6051809453242));
#154306=CARTESIAN_POINT('Ctrl Pts',(-19.2121666533115,-16.4370533501363,
11.6094345232097));
#154307=CARTESIAN_POINT('Ctrl Pts',(-19.1296469837906,-16.4213638903979,
11.6136056371876));
#154308=CARTESIAN_POINT('Ctrl Pts',(-19.0462929678283,-16.4097284515022,
11.6177767511656));
#154309=CARTESIAN_POINT('Ctrl Pts',(-18.9625363705284,-16.4022213571869,
11.6219478651435));
#154310=CARTESIAN_POINT('Ctrl Pts',(-18.8788078785636,-16.3947167819496,
11.6261175794639));
#154311=CARTESIAN_POINT('Ctrl Pts',(-18.794677531367,-16.3913378410871,
11.6302872937843));
#154312=CARTESIAN_POINT('Ctrl Pts',(-18.7105831609267,-16.3921071015279,
11.6344570081047));
#154313=CARTESIAN_POINT('Ctrl Pts',(-18.626491782925,-16.3928763345952,
11.6386265740487));
#154314=CARTESIAN_POINT('Ctrl Pts',(-18.5424368391401,-16.3977934704174,
11.6427961399927));
#154315=CARTESIAN_POINT('Ctrl Pts',(-18.458855738801,-16.4068289575101,
11.6469657059368));
#154316=CARTESIAN_POINT('Ctrl Pts',(-18.3723360300824,-16.4161821211824,
11.6512818686757));
#154317=CARTESIAN_POINT('Ctrl Pts',(-18.2863246298124,-16.4299485702282,
11.6555980314146));
#154318=CARTESIAN_POINT('Ctrl Pts',(-18.2012984666218,-16.4480373252909,
11.6599141941535));
#154319=CARTESIAN_POINT('Ctrl Pts',(-18.1190420217539,-16.46553684106,11.6640897583452));
#154320=CARTESIAN_POINT('Ctrl Pts',(-18.0377080547433,-16.4870812228023,
11.6682653225369));
#154321=CARTESIAN_POINT('Ctrl Pts',(-17.9577139481205,-16.5125369513646,
11.6724408867286));
#154322=CARTESIAN_POINT('Ctrl Pts',(-17.8736795293402,-16.5392783882614,
11.6768273487411));
#154323=CARTESIAN_POINT('Ctrl Pts',(-17.7911244272665,-16.570336474695,
11.6812138107537));
#154324=CARTESIAN_POINT('Ctrl Pts',(-17.7105077932321,-16.605499690457,
11.6856002727662));
#154325=CARTESIAN_POINT('Ctrl Pts',(-17.6298911591977,-16.640662906219,
11.6899867347788));
#154326=CARTESIAN_POINT('Ctrl Pts',(-17.5512134783828,-16.6799309241434,
11.6943731967913));
#154327=CARTESIAN_POINT('Ctrl Pts',(-17.4749010481801,-16.7230383965788,
11.6987596588038));
#154328=CARTESIAN_POINT('Ctrl Pts',(-17.4020998660131,-16.7641624303069,
11.7029442931969));
#154329=CARTESIAN_POINT('Ctrl Pts',(-17.3311800802061,-16.8089334362055,
11.7071289275899));
#154330=CARTESIAN_POINT('Ctrl Pts',(-17.2625305744984,-16.8571544854539,
11.711313561983));
#154331=CARTESIAN_POINT('Ctrl Pts',(-17.193978782865,-16.9053068980072,
11.7154922400669));
#154332=CARTESIAN_POINT('Ctrl Pts',(-17.1276912258538,-16.9568993375337,
11.7196709181509));
#154333=CARTESIAN_POINT('Ctrl Pts',(-17.0640314133917,-17.0116894785263,
11.7238495962348));
#154334=CARTESIAN_POINT('Ctrl Pts',(-16.9992305445427,-17.0674616934193,
11.7281031741202));
#154335=CARTESIAN_POINT('Ctrl Pts',(-16.9371529712703,-17.1265471378129,
11.7323567520057));
#154336=CARTESIAN_POINT('Ctrl Pts',(-16.8781504066903,-17.188644594243,
11.7366103298911));
#154337=CARTESIAN_POINT('Ctrl Pts',(-16.8202917219588,-17.2495381703071,
11.7407814438691));
#154338=CARTESIAN_POINT('Ctrl Pts',(-16.7653902112893,-17.3133276642816,
11.744952557847));
#154339=CARTESIAN_POINT('Ctrl Pts',(-16.7137420754447,-17.3796902600723,
11.749123671825));
#154340=CARTESIAN_POINT('Ctrl Pts',(-16.6621112706308,-17.4460305872531,
11.7532933861453));
#154341=CARTESIAN_POINT('Ctrl Pts',(-16.6137319548151,-17.5149419387272,
11.7574631004657));
#154342=CARTESIAN_POINT('Ctrl Pts',(-16.5688600933643,-17.5860683821312,
11.7616328147861));
#154343=CARTESIAN_POINT('Ctrl Pts',(-16.5239898286469,-17.6571922945512,
11.7658023807301));
#154344=CARTESIAN_POINT('Ctrl Pts',(-16.4826270148772,-17.7305307526507,
11.7699719466742));
#154345=CARTESIAN_POINT('Ctrl Pts',(-16.4449835652527,-17.8056999688316,
11.7741415126182));
#154346=CARTESIAN_POINT('Ctrl Pts',(-16.4060166183775,-17.8835120419223,
11.7784576753571));
#154347=CARTESIAN_POINT('Ctrl Pts',(-16.3710356838062,-17.9632855357175,
11.7827738380961));
#154348=CARTESIAN_POINT('Ctrl Pts',(-16.34022241472,-18.0445701833138,11.787090000835));
#154349=CARTESIAN_POINT('Ctrl Pts',(-16.3104128846333,-18.1232069920643,
11.7912655650267));
#154350=CARTESIAN_POINT('Ctrl Pts',(-16.2845037664842,-18.2032575521564,
11.7954411292184));
#154351=CARTESIAN_POINT('Ctrl Pts',(-16.262608713042,-18.2842986395491,
11.79961669341));
#154352=CARTESIAN_POINT('Ctrl Pts',(-16.239607792501,-18.3694329196091,
11.8040031554226));
#154353=CARTESIAN_POINT('Ctrl Pts',(-16.2210372171718,-18.4556598489484,
11.8083896174351));
#154354=CARTESIAN_POINT('Ctrl Pts',(-16.2069676619406,-18.5424788620814,
11.8127760794477));
#154355=CARTESIAN_POINT('Ctrl Pts',(-16.1928981067095,-18.6292978752144,
11.8171625414602));
#154356=CARTESIAN_POINT('Ctrl Pts',(-16.1833295591005,-18.7167083870925,
11.8215490034728));
#154357=CARTESIAN_POINT('Ctrl Pts',(-16.1782696504242,-18.8042083214207,
11.8259354654853));
#154358=CARTESIAN_POINT('Ctrl Pts',(-16.1734424727601,-18.8876836874068,
11.8301201717333));
#154359=CARTESIAN_POINT('Ctrl Pts',(-16.1727003261448,-18.9715511471448,
11.8343048779813));
#154360=CARTESIAN_POINT('Ctrl Pts',(-16.176088121868,-19.0553770947132,
11.8384895842293));
#154361=CARTESIAN_POINT('Ctrl Pts',(-16.1794710795846,-19.1390833330277,
11.8426683144272));
#154362=CARTESIAN_POINT('Ctrl Pts',(-16.1869722459993,-19.222747721166,
11.8468470446251));
#154363=CARTESIAN_POINT('Ctrl Pts',(-16.1985846232559,-19.3059334222275,
11.8510257748229));
#154364=CARTESIAN_POINT('Ctrl Pts',(-16.2101833131999,-19.3890210737101,
11.8551995796222));
#154365=CARTESIAN_POINT('Ctrl Pts',(-16.2258835179307,-19.4716307065061,
11.8593733844215));
#154366=CARTESIAN_POINT('Ctrl Pts',(-16.2456263033261,-19.5533288166232,
11.8635471892208));
#154367=CARTESIAN_POINT('Ctrl Pts',(-16.2653562958475,-19.6349739882308,
11.8677182894898));
#154368=CARTESIAN_POINT('Ctrl Pts',(-16.2891235604533,-19.7157083639801,
11.8718893897589));
#154369=CARTESIAN_POINT('Ctrl Pts',(-16.3168179573538,-19.79510792471,11.876060490028));
#154370=CARTESIAN_POINT('Ctrl Pts',(-16.3445027167196,-19.8744798547236,
11.8802301387716));
#154371=CARTESIAN_POINT('Ctrl Pts',(-16.3761117424979,-19.9525174584114,
11.8843997875152));
#154372=CARTESIAN_POINT('Ctrl Pts',(-16.4114852391772,-20.0288125118887,
11.8885694362587));
#154373=CARTESIAN_POINT('Ctrl Pts',(-16.4468570371484,-20.1051039015206,
11.8927388847672));
#154374=CARTESIAN_POINT('Ctrl Pts',(-16.4859927520516,-20.1796524905064,
11.8969083332757));
#154375=CARTESIAN_POINT('Ctrl Pts',(-16.5286852775857,-20.2520719115121,
11.9010777817841));
#154376=CARTESIAN_POINT('Ctrl Pts',(-16.5714158514074,-20.3245558739082,
11.9052509461743));
#154377=CARTESIAN_POINT('Ctrl Pts',(-16.6177093345226,-20.3949064802965,
11.9094241105645));
#154378=CARTESIAN_POINT('Ctrl Pts',(-16.6673139151431,-20.462764252509,
11.9135972749547));
#154379=CARTESIAN_POINT('Ctrl Pts',(-16.7169399758274,-20.5306514088884,
11.9177722464328));
#154380=CARTESIAN_POINT('Ctrl Pts',(-16.7698797015918,-20.59604322183,11.9219472179109));
#154381=CARTESIAN_POINT('Ctrl Pts',(-16.8258408815955,-20.6586132481759,
11.9261221893889));
#154382=CARTESIAN_POINT('Ctrl Pts',(-16.8818951703622,-20.7212873791486,
11.9303041072257));
#154383=CARTESIAN_POINT('Ctrl Pts',(-16.9409806346913,-20.7811300140031,
11.9344860250625));
#154384=CARTESIAN_POINT('Ctrl Pts',(-17.0027682220265,-20.8378516725699,
11.9386679428993));
#154385=CARTESIAN_POINT('Ctrl Pts',(-17.0579318451728,-20.888492461964,
11.9424015364822));
#154386=CARTESIAN_POINT('Ctrl Pts',(-17.1152486151753,-20.9366459831291,
11.9461351300651));
#154387=CARTESIAN_POINT('Ctrl Pts',(-17.1744641402401,-20.9821349467765,
11.949868723648));
#154388=CARTESIAN_POINT('Ctrl Pts',(-17.1757180887841,-20.9805344762225,
11.1497835108638));
#154389=CARTESIAN_POINT('Ctrl Pts',(-17.388725157886,-21.1470794372515,
11.1632078179353));
#154390=CARTESIAN_POINT('Ctrl Pts',(-18.3777720013044,-21.7011259744509,
11.2190240605671));
#154391=CARTESIAN_POINT('Ctrl Pts',(-20.5048168108401,-21.3581664234228,
11.3135258905536));
#154392=CARTESIAN_POINT('Ctrl Pts',(-21.2925956727874,-19.7256331618843,
11.3946034134688));
#154393=CARTESIAN_POINT('Ctrl Pts',(-21.2974134759181,-18.9507193137797,
11.4332890008234));
#154394=CARTESIAN_POINT('',(-21.2939995125392,-18.9535798097909,11.3667098902285));
#154395=CARTESIAN_POINT('Ctrl Pts',(-17.1731949481218,-20.9838169785965,
11.0834063298428));
#154396=CARTESIAN_POINT('Ctrl Pts',(-17.7502562818926,-21.4186339846309,
11.1194278825506));
#154397=CARTESIAN_POINT('Ctrl Pts',(-19.4306370706601,-21.8291474349523,
11.1978413708189));
#154398=CARTESIAN_POINT('Ctrl Pts',(-21.0857645353049,-20.4522478666649,
11.2922755722919));
#154399=CARTESIAN_POINT('Ctrl Pts',(-21.2926071426957,-19.2766421748681,
11.3506882210569));
#154400=CARTESIAN_POINT('Ctrl Pts',(-21.2907951752863,-18.9535971086061,
11.3667089342616));
#154401=CARTESIAN_POINT('Ctrl Pts',(-21.2939995125392,-18.9535798097909,
11.3667098902285));
#154402=CARTESIAN_POINT('Ctrl Pts',(-21.2940518853803,-18.8687123476393,
11.3709134538372));
#154403=CARTESIAN_POINT('Ctrl Pts',(-21.2898797137862,-18.7838299700766,
11.3751170174459));
#154404=CARTESIAN_POINT('Ctrl Pts',(-21.2815050782104,-18.699377996817,
11.3793205810546));
#154405=CARTESIAN_POINT('Ctrl Pts',(-21.2731292177987,-18.6149136719984,
11.3835247594572));
#154406=CARTESIAN_POINT('Ctrl Pts',(-21.2605497166712,-18.5308803238371,
11.3877289378599));
#154407=CARTESIAN_POINT('Ctrl Pts',(-21.2438404672875,-18.4477175109462,
11.3919331162626));
#154408=CARTESIAN_POINT('Ctrl Pts',(-21.2271240709727,-18.3645191274038,
11.3961390928892));
#154409=CARTESIAN_POINT('Ctrl Pts',(-21.2062745049673,-18.2821924593938,
11.4003450695159));
#154410=CARTESIAN_POINT('Ctrl Pts',(-21.1814163656274,-18.2011650425965,
11.4045510461425));
#154411=CARTESIAN_POINT('Ctrl Pts',(-21.1565238219894,-18.1200254817903,
11.408762843948));
#154412=CARTESIAN_POINT('Ctrl Pts',(-21.1276117659034,-18.0401891906194,
11.4129746417534));
#154413=CARTESIAN_POINT('Ctrl Pts',(-21.0948539828413,-17.9620664306619,
11.4171864395589));
#154414=CARTESIAN_POINT('Ctrl Pts',(-21.0620694457193,-17.8838798659899,
11.4214016772397));
#154415=CARTESIAN_POINT('Ctrl Pts',(-21.0254331231614,-17.8074100228063,
11.4256169149205));
#154416=CARTESIAN_POINT('Ctrl Pts',(-20.985165001354,-17.7330430127856,
11.4298321526013));
#154417=CARTESIAN_POINT('Ctrl Pts',(-20.9448260993907,-17.6585452862494,
11.4340547994973));
#154418=CARTESIAN_POINT('Ctrl Pts',(-20.9008428915851,-17.5861581518394,
11.4382774463933));
#154419=CARTESIAN_POINT('Ctrl Pts',(-20.853478708255,-17.5162388759777,
11.4425000932894));
#154420=CARTESIAN_POINT('Ctrl Pts',(-20.8410561777281,-17.497900666011,
11.4436075959693));
#154421=CARTESIAN_POINT('Ctrl Pts',(-20.828401284867,-17.4797320374709,
11.4447150986492));
#154422=CARTESIAN_POINT('Ctrl Pts',(-20.8155192213963,-17.4617390393097,
11.4458226013291));
#154423=CARTESIAN_POINT('Ctrl Pts',(-20.7668450946151,-17.3937535433782,
11.4500072357222));
#154424=CARTESIAN_POINT('Ctrl Pts',(-20.7147461245074,-17.3280286903786,
11.4541918701152));
#154425=CARTESIAN_POINT('Ctrl Pts',(-20.6594597008472,-17.2649300724589,
11.4583765045082));
#154426=CARTESIAN_POINT('Ctrl Pts',(-20.6042519705678,-17.2019212676116,
11.4625551825922));
#154427=CARTESIAN_POINT('Ctrl Pts',(-20.5458660991114,-17.1415316158067,
11.4667338606761));
#154428=CARTESIAN_POINT('Ctrl Pts',(-20.4845818988857,-17.0840966258144,
11.4709125387601));
#154429=CARTESIAN_POINT('Ctrl Pts',(-20.4221992234151,-17.0256321549044,
11.4751661166455));
#154430=CARTESIAN_POINT('Ctrl Pts',(-20.3568135727525,-16.9702297043269,
11.479419694531));
#154431=CARTESIAN_POINT('Ctrl Pts',(-20.2887620518452,-16.9182067553111,
11.4836732724164));
#154432=CARTESIAN_POINT('Ctrl Pts',(-20.2220298424622,-16.8671923726764,
11.4878443863944));
#154433=CARTESIAN_POINT('Ctrl Pts',(-20.1527345889107,-16.8194279167436,
11.4920155003723));
#154434=CARTESIAN_POINT('Ctrl Pts',(-20.0812289339446,-16.7751733648399,
11.4961866143503));
#154435=CARTESIAN_POINT('Ctrl Pts',(-20.0097472733917,-16.7309336629786,
11.5003563286706));
#154436=CARTESIAN_POINT('Ctrl Pts',(-19.9360570753459,-16.6902017679483,
11.504526042991));
#154437=CARTESIAN_POINT('Ctrl Pts',(-19.8605396057914,-16.6531941107211,
11.5086957573114));
#154438=CARTESIAN_POINT('Ctrl Pts',(-19.7850248234724,-16.6161877703851,
11.5128653232554));
#154439=CARTESIAN_POINT('Ctrl Pts',(-19.7076833123966,-16.582905606034,
11.5170348891995));
#154440=CARTESIAN_POINT('Ctrl Pts',(-19.6289193227213,-16.5535172700601,
11.5212044551435));
#154441=CARTESIAN_POINT('Ctrl Pts',(-19.5473860883349,-16.5230956764478,
11.5255206178824));
#154442=CARTESIAN_POINT('Ctrl Pts',(-19.4643289796725,-16.4968470041692,
11.5298367806213));
#154443=CARTESIAN_POINT('Ctrl Pts',(-19.3802151086559,-16.4749037093111,
11.5341529433603));
#154444=CARTESIAN_POINT('Ctrl Pts',(-19.2988412381404,-16.453675214975,
11.5383285075519));
#154445=CARTESIAN_POINT('Ctrl Pts',(-19.2164788667989,-16.436475960301,
11.5425040717436));
#154446=CARTESIAN_POINT('Ctrl Pts',(-19.1335609462705,-16.4233736831601,
11.5466796359353));
#154447=CARTESIAN_POINT('Ctrl Pts',(-19.046455038695,-16.4096096411485,
11.5510660979478));
#154448=CARTESIAN_POINT('Ctrl Pts',(-18.9587365661201,-16.4003673913993,
11.5554525599604));
#154449=CARTESIAN_POINT('Ctrl Pts',(-18.8709107816369,-16.3956636688668,
11.5598390219729));
#154450=CARTESIAN_POINT('Ctrl Pts',(-18.7830849971537,-16.3909599463343,
11.5642254839855));
#154451=CARTESIAN_POINT('Ctrl Pts',(-18.6951524811211,-16.3907946760441,
11.568611945998));
#154452=CARTESIAN_POINT('Ctrl Pts',(-18.607613246377,-16.3951217493771,
11.5729984080105));
#154453=CARTESIAN_POINT('Ctrl Pts',(-18.5241018215877,-16.3992497276517,
11.5771830424036));
#154454=CARTESIAN_POINT('Ctrl Pts',(-18.4406374370144,-16.4074811003133,
11.5813676767966));
#154455=CARTESIAN_POINT('Ctrl Pts',(-18.3576559923793,-16.4198141482253,
11.5855523111897));
#154456=CARTESIAN_POINT('Ctrl Pts',(-18.2747926615594,-16.4321296415702,
11.5897309892736));
#154457=CARTESIAN_POINT('Ctrl Pts',(-18.1924113564174,-16.4485351465589,
11.5939096673576));
#154458=CARTESIAN_POINT('Ctrl Pts',(-18.1109456438827,-16.4689769897717,
11.5980883454415));
#154459=CARTESIAN_POINT('Ctrl Pts',(-18.0280197169993,-16.4897852383328,
11.602341923327));
#154460=CARTESIAN_POINT('Ctrl Pts',(-17.9460430111247,-16.5147759273295,
11.6065955012124));
#154461=CARTESIAN_POINT('Ctrl Pts',(-17.8654649462447,-16.5438374514169,
11.6108490790978));
#154462=CARTESIAN_POINT('Ctrl Pts',(-17.7864490443875,-16.572335561151,
11.6150201930758));
#154463=CARTESIAN_POINT('Ctrl Pts',(-17.708778489378,-16.6047479091043,
11.6191913070537));
#154464=CARTESIAN_POINT('Ctrl Pts',(-17.6328627598405,-16.6409186993241,
11.6233624210317));
#154465=CARTESIAN_POINT('Ctrl Pts',(-17.5569725045593,-16.6770773520858,
11.6275321353521));
#154466=CARTESIAN_POINT('Ctrl Pts',(-17.4828363202439,-16.7169917446773,
11.6317018496724));
#154467=CARTESIAN_POINT('Ctrl Pts',(-17.4108425631367,-16.7604584427227,
11.6358715639928));
#154468=CARTESIAN_POINT('Ctrl Pts',(-17.3388513678763,-16.8039235940365,
11.6400411299369));
#154469=CARTESIAN_POINT('Ctrl Pts',(-17.2690028416262,-16.8509405609746,
11.6442106958809));
#154470=CARTESIAN_POINT('Ctrl Pts',(-17.2016584481431,-16.9012612627512,
11.648380261825));
#154471=CARTESIAN_POINT('Ctrl Pts',(-17.1319463088635,-16.9533511783249,
11.6526964245639));
#154472=CARTESIAN_POINT('Ctrl Pts',(-17.0649180918033,-17.0089811541786,
11.6570125873028));
#154473=CARTESIAN_POINT('Ctrl Pts',(-17.0009380103939,-17.0678301190757,
11.6613287500417));
#154474=CARTESIAN_POINT('Ctrl Pts',(-16.9390420734068,-17.1247620851311,
11.6655043142334));
#154475=CARTESIAN_POINT('Ctrl Pts',(-16.8799990325859,-17.1847061749561,
11.6696798784251));
#154476=CARTESIAN_POINT('Ctrl Pts',(-16.8241001932714,-17.2473350099629,
11.6738554426168));
#154477=CARTESIAN_POINT('Ctrl Pts',(-16.7653780364702,-17.31312707854,11.6782419046293));
#154478=CARTESIAN_POINT('Ctrl Pts',(-16.7101264215565,-17.3818817777301,
11.6826283666418));
#154479=CARTESIAN_POINT('Ctrl Pts',(-16.6586329038938,-17.4531833279551,
11.6870148286544));
#154480=CARTESIAN_POINT('Ctrl Pts',(-16.6071393862312,-17.52448487818,11.6914012906669));
#154481=CARTESIAN_POINT('Ctrl Pts',(-16.5594042169153,-17.5983327508676,
11.6957877526794));
#154482=CARTESIAN_POINT('Ctrl Pts',(-16.5156592733601,-17.6742815566288,
11.700174214692));
#154483=CARTESIAN_POINT('Ctrl Pts',(-16.4739270995034,-17.7467358452539,
11.704358849085));
#154484=CARTESIAN_POINT('Ctrl Pts',(-16.4356706929265,-17.8213716700561,
11.7085434834781));
#154485=CARTESIAN_POINT('Ctrl Pts',(-16.4011245523601,-17.8978215778158,
11.7127281178711));
#154486=CARTESIAN_POINT('Ctrl Pts',(-16.3666275839487,-17.9741626685945,
11.7169067959551));
#154487=CARTESIAN_POINT('Ctrl Pts',(-16.3358305794284,-18.0523122977899,
11.721085474039));
#154488=CARTESIAN_POINT('Ctrl Pts',(-16.308923089503,-18.1318768518237,
11.7252641521229));
#154489=CARTESIAN_POINT('Ctrl Pts',(-16.2815333021588,-18.2128675433067,
11.7295177300084));
#154490=CARTESIAN_POINT('Ctrl Pts',(-16.258174080664,-18.2953239658203,
11.7337713078938));
#154491=CARTESIAN_POINT('Ctrl Pts',(-16.2389948450999,-18.3788078184223,
11.7380248857792));
#154492=CARTESIAN_POINT('Ctrl Pts',(-16.2201874364424,-18.4606731736363,
11.7421959997572));
#154493=CARTESIAN_POINT('Ctrl Pts',(-16.2053994934178,-18.5435260079658,
11.7463671137352));
#154494=CARTESIAN_POINT('Ctrl Pts',(-16.194721659298,-18.6269376852947,
11.7505382277131));
#154495=CARTESIAN_POINT('Ctrl Pts',(-16.1840474082286,-18.7103213730297,
11.7547079420335));
#154496=CARTESIAN_POINT('Ctrl Pts',(-16.1774805853424,-18.7942630754067,
11.7588776563538));
#154497=CARTESIAN_POINT('Ctrl Pts',(-16.1750603443919,-18.8783261311156,
11.7630473706742));
#154498=CARTESIAN_POINT('Ctrl Pts',(-16.172640189564,-18.9623861955001,
11.7672169366182));
#154499=CARTESIAN_POINT('Ctrl Pts',(-16.1743663356855,-19.0465671447637,
11.7713865025623));
#154500=CARTESIAN_POINT('Ctrl Pts',(-16.1802258395509,-19.1304307636657,
11.7755560685063));
#154501=CARTESIAN_POINT('Ctrl Pts',(-16.1862913563437,-19.2172429239514,
11.7798722312452));
#154502=CARTESIAN_POINT('Ctrl Pts',(-16.1967862597981,-19.3037144978774,
11.7841883939842));
#154503=CARTESIAN_POINT('Ctrl Pts',(-16.2116377216372,-19.3893654498155,
11.7885045567231));
#154504=CARTESIAN_POINT('Ctrl Pts',(-16.2260053986689,-19.4722263310029,
11.7926801209148));
#154505=CARTESIAN_POINT('Ctrl Pts',(-16.2444500136973,-19.5543187834622,
11.7968556851065));
#154506=CARTESIAN_POINT('Ctrl Pts',(-16.2668539711945,-19.635220661682,
11.8010312492981));
#154507=CARTESIAN_POINT('Ctrl Pts',(-16.2903894993245,-19.7202087014447,
11.8054177113107));
#154508=CARTESIAN_POINT('Ctrl Pts',(-16.3182946694534,-19.8038821804653,
11.8098041733232));
#154509=CARTESIAN_POINT('Ctrl Pts',(-16.3503755250187,-19.8857742565899,
11.8141906353358));
#154510=CARTESIAN_POINT('Ctrl Pts',(-16.382456380584,-19.9676663327144,
11.8185770973483));
#154511=CARTESIAN_POINT('Ctrl Pts',(-16.4187126130535,-20.047776508705,
11.8229635593609));
#154512=CARTESIAN_POINT('Ctrl Pts',(-16.4588952312817,-20.1256687315232,
11.8273500213734));
#154513=CARTESIAN_POINT('Ctrl Pts',(-16.4972321909917,-20.1999832271826,
11.8315350054501));
#154514=CARTESIAN_POINT('Ctrl Pts',(-16.5392854659906,-20.2725556853913,
11.8357199895268));
#154515=CARTESIAN_POINT('Ctrl Pts',(-16.5848729683257,-20.3429899358826,
11.8399049736034));
#154516=CARTESIAN_POINT('Ctrl Pts',(-16.6303841734451,-20.4133063045659,
11.8440829535097));
#154517=CARTESIAN_POINT('Ctrl Pts',(-16.6794175976995,-20.4814911976367,
11.8482609334161));
#154518=CARTESIAN_POINT('Ctrl Pts',(-16.7317449889769,-20.5471723639885,
11.8524389133224));
#154519=CARTESIAN_POINT('Ctrl Pts',(-16.7840217296592,-20.612789953883,
11.8566128491293));
#154520=CARTESIAN_POINT('Ctrl Pts',(-16.8395858226484,-20.6759082705201,
11.8607867849363));
#154521=CARTESIAN_POINT('Ctrl Pts',(-16.8981658620059,-20.7361841322508,
11.8649607207433));
#154522=CARTESIAN_POINT('Ctrl Pts',(-16.9567039826349,-20.7964168617556,
11.8691316697636));
#154523=CARTESIAN_POINT('Ctrl Pts',(-17.0182534419654,-20.8538108487294,
11.8733026187839));
#154524=CARTESIAN_POINT('Ctrl Pts',(-17.0825036449483,-20.9080572050048,
11.8774735678041));
#154525=CARTESIAN_POINT('Ctrl Pts',(-17.1125774867215,-20.9334485074389,
11.8794258800935));
#154526=CARTESIAN_POINT('Ctrl Pts',(-17.1432425028621,-20.9581506972719,
11.8813781923829));
#154527=CARTESIAN_POINT('Ctrl Pts',(-17.1744641402401,-20.9821349467765,
11.8833305046723));
#154528=CARTESIAN_POINT('Origin',(-18.734,-18.952,-1.76670989022851));
#154529=CARTESIAN_POINT('',(-17.1744641402401,-20.9821349467765,12.7499597538068));
#154530=CARTESIAN_POINT('',(-17.1750494479187,-20.9813915763786,12.6831923855689));
#154531=CARTESIAN_POINT('',(-17.1744641402401,-20.9821349467765,-1.76670989022851));
#154532=CARTESIAN_POINT('',(-21.2939989766127,-18.9542890482673,12.2332901098107));
#154533=CARTESIAN_POINT('Ctrl Pts',(-21.2939989766127,-18.9542890482673,
12.2332901098107));
#154534=CARTESIAN_POINT('Ctrl Pts',(-21.2940747905549,-18.869501140071,
12.2375129674107));
#154535=CARTESIAN_POINT('Ctrl Pts',(-21.2899336304853,-18.7845778436852,
12.2417358250107));
#154536=CARTESIAN_POINT('Ctrl Pts',(-21.2815646644669,-18.699979603286,
12.2459586826108));
#154537=CARTESIAN_POINT('Ctrl Pts',(-21.2734134565488,-18.6175825848873,
12.2500716626647));
#154538=CARTESIAN_POINT('Ctrl Pts',(-21.2612518149667,-18.5354944186517,
12.2541846427187));
#154539=CARTESIAN_POINT('Ctrl Pts',(-21.2451224198776,-18.4541403888767,
12.2582976227727));
#154540=CARTESIAN_POINT('Ctrl Pts',(-21.2290007459443,-18.3728253033476,
12.2624086339395));
#154541=CARTESIAN_POINT('Ctrl Pts',(-21.2089151790601,-18.2922441216167,
12.2665196451063));
#154542=CARTESIAN_POINT('Ctrl Pts',(-21.1849598944702,-18.2128142346483,
12.2706306562731));
#154543=CARTESIAN_POINT('Ctrl Pts',(-21.1610084101084,-18.1333969483105,
12.2747410152756));
#154544=CARTESIAN_POINT('Ctrl Pts',(-21.133188564531,-18.0551310480641,
12.2788513742782));
#154545=CARTESIAN_POINT('Ctrl Pts',(-21.1016446063283,-17.9784194855459,
12.2829617332807));
#154546=CARTESIAN_POINT('Ctrl Pts',(-21.0685960771622,-17.8980489659376,
12.2872681465249));
#154547=CARTESIAN_POINT('Ctrl Pts',(-21.031459503672,-17.8193852938559,
12.2915745597691));
#154548=CARTESIAN_POINT('Ctrl Pts',(-20.9904568914618,-17.7428671301405,
12.2958809730133));
#154549=CARTESIAN_POINT('Ctrl Pts',(-20.9512718262792,-17.669740832297,
12.2999964933321));
#154550=CARTESIAN_POINT('Ctrl Pts',(-20.9085564982552,-17.5985742591841,
12.304112013651));
#154551=CARTESIAN_POINT('Ctrl Pts',(-20.8625501361326,-17.5297221375659,
12.3082275339698));
#154552=CARTESIAN_POINT('Ctrl Pts',(-20.8165130556118,-17.4608240434608,
12.3123458022171));
#154553=CARTESIAN_POINT('Ctrl Pts',(-20.7671808550883,-17.3942438526559,
12.3164640704644));
#154554=CARTESIAN_POINT('Ctrl Pts',(-20.7148334041519,-17.3303036582036,
12.3205823387118));
#154555=CARTESIAN_POINT('Ctrl Pts',(-20.6624054653519,-17.2662651512345,
12.3247069390843));
#154556=CARTESIAN_POINT('Ctrl Pts',(-20.6069533520103,-17.204875081262,
12.3288315394568));
#154557=CARTESIAN_POINT('Ctrl Pts',(-20.5487934990227,-17.146418499235,
12.3329561398293));
#154558=CARTESIAN_POINT('Ctrl Pts',(-20.5408850965653,-17.1384697484523,
12.3335169906232));
#154559=CARTESIAN_POINT('Ctrl Pts',(-20.5329266770602,-17.1305751748486,
12.3340778414171));
#154560=CARTESIAN_POINT('Ctrl Pts',(-20.524919080494,-17.1227354354489,
12.334638692211));
#154561=CARTESIAN_POINT('Ctrl Pts',(-20.4651725946905,-17.0642413698601,
12.338823326604));
#154562=CARTESIAN_POINT('Ctrl Pts',(-20.4024461555816,-17.0085686402269,
12.3430079609971));
#154563=CARTESIAN_POINT('Ctrl Pts',(-20.3370370650427,-16.9560360303604,
12.3471925953901));
#154564=CARTESIAN_POINT('Ctrl Pts',(-20.2717210762481,-16.9035781941618,
12.3513712734741));
#154565=CARTESIAN_POINT('Ctrl Pts',(-20.2037303762193,-16.8542518853563,
12.355549951558));
#154566=CARTESIAN_POINT('Ctrl Pts',(-20.1333988170804,-16.8083388908799,
12.3597286296419));
#154567=CARTESIAN_POINT('Ctrl Pts',(-20.0618066152903,-16.7616029389746,
12.3639822075274));
#154568=CARTESIAN_POINT('Ctrl Pts',(-19.9877891536757,-16.7184042096101,
12.3682357854128));
#154569=CARTESIAN_POINT('Ctrl Pts',(-19.9117335730786,-16.6789967816029,
12.3724893632982));
#154570=CARTESIAN_POINT('Ctrl Pts',(-19.8371524783216,-16.6403533434849,
12.3766604772762));
#154571=CARTESIAN_POINT('Ctrl Pts',(-19.760612012467,-16.605355736394,12.3808315912541));
#154572=CARTESIAN_POINT('Ctrl Pts',(-19.6825046263014,-16.5741987101768,
12.3850027052321));
#154573=CARTESIAN_POINT('Ctrl Pts',(-19.6044234498237,-16.5430521390007,
12.3891724195525));
#154574=CARTESIAN_POINT('Ctrl Pts',(-19.5247768242089,-16.5157437595369,
12.3933421338728));
#154575=CARTESIAN_POINT('Ctrl Pts',(-19.443977821747,-16.4924204642607,
12.3975118481932));
#154576=CARTESIAN_POINT('Ctrl Pts',(-19.3631816944604,-16.4690979989275,
12.4016814141372));
#154577=CARTESIAN_POINT('Ctrl Pts',(-19.281233714082,-16.449760462599,12.4058509800813));
#154578=CARTESIAN_POINT('Ctrl Pts',(-19.1985614595122,-16.4345046871273,
12.4100205460253));
#154579=CARTESIAN_POINT('Ctrl Pts',(-19.112982550459,-16.4187125374101,
12.4143367087642));
#154580=CARTESIAN_POINT('Ctrl Pts',(-19.0266280073015,-16.4072946141391,
12.4186528715032));
#154581=CARTESIAN_POINT('Ctrl Pts',(-18.9399808515254,-16.400300196182,
12.4229690342421));
#154582=CARTESIAN_POINT('Ctrl Pts',(-18.8561562177351,-16.3935336206541,
12.4271445984338));
#154583=CARTESIAN_POINT('Ctrl Pts',(-18.7720582145669,-16.3909067522804,
12.4313201626255));
#154584=CARTESIAN_POINT('Ctrl Pts',(-18.6881249777989,-16.3924110716097,
12.4354957268171));
#154585=CARTESIAN_POINT('Ctrl Pts',(-18.5999524727738,-16.3939913705322,
12.4398821888297));
#154586=CARTESIAN_POINT('Ctrl Pts',(-18.5119623987477,-16.4001311167978,
12.4442686508422));
#154587=CARTESIAN_POINT('Ctrl Pts',(-18.4246552312346,-16.4107590011891,
12.4486551128548));
#154588=CARTESIAN_POINT('Ctrl Pts',(-18.3373480637215,-16.4213868855804,
12.4530415748673));
#154589=CARTESIAN_POINT('Ctrl Pts',(-18.2507243612257,-16.4365027334242,
12.4574280368799));
#154590=CARTESIAN_POINT('Ctrl Pts',(-18.1652685194104,-16.4559742583486,
12.4618144988924));
#154591=CARTESIAN_POINT('Ctrl Pts',(-18.083744627553,-16.4745498695476,
12.4659991332854));
#154592=CARTESIAN_POINT('Ctrl Pts',(-18.0029800405432,-16.4971582855303,
12.4701837676785));
#154593=CARTESIAN_POINT('Ctrl Pts',(-17.923403728984,-16.5237220740997,
12.4743684020715));
#154594=CARTESIAN_POINT('Ctrl Pts',(-17.8439406844548,-16.5502480524038,
12.4785470801555));
#154595=CARTESIAN_POINT('Ctrl Pts',(-17.7656629884269,-16.5807180759576,
12.4827257582394));
#154596=CARTESIAN_POINT('Ctrl Pts',(-17.6889882869429,-16.6150039538815,
12.4869044363234));
#154597=CARTESIAN_POINT('Ctrl Pts',(-17.6109392465397,-16.6499043815265,
12.4911580142088));
#154598=CARTESIAN_POINT('Ctrl Pts',(-17.5345517033716,-16.6887587003509,
12.4954115920942));
#154599=CARTESIAN_POINT('Ctrl Pts',(-17.4602488495092,-16.7313789142172,
12.4996651699797));
#154600=CARTESIAN_POINT('Ctrl Pts',(-17.3873865014589,-16.7731728520712,
12.5038362839576));
#154601=CARTESIAN_POINT('Ctrl Pts',(-17.3165291499245,-16.8185877301275,
12.5080073979356));
#154602=CARTESIAN_POINT('Ctrl Pts',(-17.2480529748744,-16.8673989737793,
12.5121785119135));
#154603=CARTESIAN_POINT('Ctrl Pts',(-17.1795997776662,-16.9161938383469,
12.5163482262339));
#154604=CARTESIAN_POINT('Ctrl Pts',(-17.1135265443543,-16.9683825382779,
12.5205179405543));
#154605=CARTESIAN_POINT('Ctrl Pts',(-17.0501803764602,-17.0236972552573,
12.5246876548747));
#154606=CARTESIAN_POINT('Ctrl Pts',(-16.9868364626947,-17.0790100039016,
12.5288572208187));
#154607=CARTESIAN_POINT('Ctrl Pts',(-16.9262197673615,-17.1374482452015,
12.5330267867627));
#154608=CARTESIAN_POINT('Ctrl Pts',(-16.8686431510734,-17.1987048662126,
12.5371963527068));
#154609=CARTESIAN_POINT('Ctrl Pts',(-16.809042211985,-17.2621151944502,
12.5415125154457));
#154610=CARTESIAN_POINT('Ctrl Pts',(-16.752699469072,-17.3285453940344,
12.5458286781846));
#154611=CARTESIAN_POINT('Ctrl Pts',(-16.6999178084324,-17.3976159940518,
12.5501448409235));
#154612=CARTESIAN_POINT('Ctrl Pts',(-16.6488555048365,-17.4644366265386,
12.5543204051152));
#154613=CARTESIAN_POINT('Ctrl Pts',(-16.6011260701749,-17.5337278643774,
12.5584959693069));
#154614=CARTESIAN_POINT('Ctrl Pts',(-16.5569594955243,-17.6051166932981,
12.5626715334986));
#154615=CARTESIAN_POINT('Ctrl Pts',(-16.5105621721843,-17.6801112022566,
12.5670579955111));
#154616=CARTESIAN_POINT('Ctrl Pts',(-16.4680973689511,-17.7574202579854,
12.5714444575237));
#154617=CARTESIAN_POINT('Ctrl Pts',(-16.4297760239617,-17.8365844414523,
12.5758309195362));
#154618=CARTESIAN_POINT('Ctrl Pts',(-16.3914546789723,-17.9157486249192,
12.5802173815487));
#154619=CARTESIAN_POINT('Ctrl Pts',(-16.3572769476616,-17.9967673719631,
12.5846038435613));
#154620=CARTESIAN_POINT('Ctrl Pts',(-16.3273937923111,-18.0791617783844,
12.5889903055738));
#154621=CARTESIAN_POINT('Ctrl Pts',(-16.2988856052357,-18.1577650960284,
12.5931749399669));
#154622=CARTESIAN_POINT('Ctrl Pts',(-16.274179366091,-18.2379128391994,
12.5973595743599));
#154623=CARTESIAN_POINT('Ctrl Pts',(-16.2534421603043,-18.3192023989268,
12.601544208753));
#154624=CARTESIAN_POINT('Ctrl Pts',(-16.2327344713631,-18.4003762530276,
12.6057228868369));
#154625=CARTESIAN_POINT('Ctrl Pts',(-16.2159847069801,-18.4826882535132,
12.6099015649209));
#154626=CARTESIAN_POINT('Ctrl Pts',(-16.2033111427937,-18.565717838864,
12.6140802430048));
#154627=CARTESIAN_POINT('Ctrl Pts',(-16.1904104140776,-18.6502356698599,
12.6183338208902));
#154628=CARTESIAN_POINT('Ctrl Pts',(-16.1817336190671,-18.7354966109228,
12.6225873987757));
#154629=CARTESIAN_POINT('Ctrl Pts',(-16.177351748603,-18.821043065749,12.6268409766611));
#154630=CARTESIAN_POINT('Ctrl Pts',(-16.1730548292482,-18.9049310356184,
12.6310120906391));
#154631=CARTESIAN_POINT('Ctrl Pts',(-16.1728878141637,-18.9890930669704,
12.635183204617));
#154632=CARTESIAN_POINT('Ctrl Pts',(-16.1768654907269,-19.0730912940081,
12.639354318595));
#154633=CARTESIAN_POINT('Ctrl Pts',(-16.1808418325423,-19.1570613346296,
12.6435240329154));
#154634=CARTESIAN_POINT('Ctrl Pts',(-16.1889600821297,-19.2408672209648,
12.6476937472357));
#154635=CARTESIAN_POINT('Ctrl Pts',(-16.2011829261397,-19.3240721305897,
12.6518634615561));
#154636=CARTESIAN_POINT('Ctrl Pts',(-16.2134053352084,-19.4072740794267,
12.6560330275002));
#154637=CARTESIAN_POINT('Ctrl Pts',(-16.2297319805921,-19.4898746390488,
12.6602025934442));
#154638=CARTESIAN_POINT('Ctrl Pts',(-16.2500739744222,-19.5714445087795,
12.6643721593882));
#154639=CARTESIAN_POINT('Ctrl Pts',(-16.2711311676607,-19.6558822745028,
12.6686883221272));
#154640=CARTESIAN_POINT('Ctrl Pts',(-16.2964911945898,-19.7392150119469,
12.6730044848661));
#154641=CARTESIAN_POINT('Ctrl Pts',(-16.3259989267242,-19.8209826414278,
12.677320647605));
#154642=CARTESIAN_POINT('Ctrl Pts',(-16.354545447588,-19.9000866989788,
12.6814962117967));
#154643=CARTESIAN_POINT('Ctrl Pts',(-16.3869733753123,-19.9777256330122,
12.6856717759884));
#154644=CARTESIAN_POINT('Ctrl Pts',(-16.4230935537345,-20.0535041518799,
12.6898473401801));
#154645=CARTESIAN_POINT('Ctrl Pts',(-16.4610380765012,-20.1331100635892,
12.6942338021926));
#154646=CARTESIAN_POINT('Ctrl Pts',(-16.5030573653645,-20.2106621684913,
12.6986202642052));
#154647=CARTESIAN_POINT('Ctrl Pts',(-16.5488792984355,-20.2857344261862,
12.7030067262177));
#154648=CARTESIAN_POINT('Ctrl Pts',(-16.5947012315065,-20.3608066838811,
12.7073931882302));
#154649=CARTESIAN_POINT('Ctrl Pts',(-16.6443254185492,-20.433398658303,
12.7117796502428));
#154650=CARTESIAN_POINT('Ctrl Pts',(-16.6974308899397,-20.5031241923032,
12.7161661122553));
#154651=CARTESIAN_POINT('Ctrl Pts',(-16.7480908287789,-20.5696388318591,
12.7203505755782));
#154652=CARTESIAN_POINT('Ctrl Pts',(-16.8021070326506,-20.6337927963332,
12.724535038901));
#154653=CARTESIAN_POINT('Ctrl Pts',(-16.8592314426267,-20.6952277121147,
12.7287195022239));
#154654=CARTESIAN_POINT('Ctrl Pts',(-16.9162677654097,-20.756567893801,
12.7328975130051));
#154655=CARTESIAN_POINT('Ctrl Pts',(-16.9764024588243,-20.8151970253541,
12.7370755237864));
#154656=CARTESIAN_POINT('Ctrl Pts',(-17.0393460611412,-20.8707881663984,
12.7412535345677));
#154657=CARTESIAN_POINT('Ctrl Pts',(-17.0830670909289,-20.9094021294393,
12.7441556076474));
#154658=CARTESIAN_POINT('Ctrl Pts',(-17.1281424629339,-20.94655094929,12.7470576807271));
#154659=CARTESIAN_POINT('Ctrl Pts',(-17.1744641402401,-20.9821349467765,
12.7499597538068));
#154660=CARTESIAN_POINT('Ctrl Pts',(-17.1744641402401,-20.9821349467765,
11.949868723648));
#154661=CARTESIAN_POINT('Ctrl Pts',(-17.1916066249818,-20.995303686974,
11.9509495731542));
#154662=CARTESIAN_POINT('Ctrl Pts',(-17.2089081277772,-21.0082493016174,
11.9520304226604));
#154663=CARTESIAN_POINT('Ctrl Pts',(-17.2263622218881,-21.0209679383717,
11.9531112721667));
#154664=CARTESIAN_POINT('Ctrl Pts',(-17.2939377743551,-21.0702096177068,
11.9572959065597));
#154665=CARTESIAN_POINT('Ctrl Pts',(-17.3640540780906,-21.1162287760929,
11.9614805409527));
#154666=CARTESIAN_POINT('Ctrl Pts',(-17.4363708665884,-21.1587529612807,
11.9656651753458));
#154667=CARTESIAN_POINT('Ctrl Pts',(-17.5085847210887,-21.2012166185545,
11.9698438534297));
#154668=CARTESIAN_POINT('Ctrl Pts',(-17.5829924458174,-21.2401949526837,
11.9740225315137));
#154669=CARTESIAN_POINT('Ctrl Pts',(-17.659222956839,-21.2754574038476,
11.9782012095976));
#154670=CARTESIAN_POINT('Ctrl Pts',(-17.7368198449848,-21.3113519091059,
11.9824547874831));
#154671=CARTESIAN_POINT('Ctrl Pts',(-17.8163051194007,-21.3433957227619,
11.9867083653685));
#154672=CARTESIAN_POINT('Ctrl Pts',(-17.8972589731891,-21.3713934062181,
11.9909619432539));
#154673=CARTESIAN_POINT('Ctrl Pts',(-17.9766433785533,-21.3988482999474,
11.9951330572319));
#154674=CARTESIAN_POINT('Ctrl Pts',(-18.0574394740936,-21.4224123904404,
11.9993041712098));
#154675=CARTESIAN_POINT('Ctrl Pts',(-18.1392307762324,-21.4419497124358,
12.0034752851878));
#154676=CARTESIAN_POINT('Ctrl Pts',(-18.2209946325099,-21.461480478494,
12.0076449995081));
#154677=CARTESIAN_POINT('Ctrl Pts',(-18.303752585081,-21.4769870528098,
12.0118147138285));
#154678=CARTESIAN_POINT('Ctrl Pts',(-18.3870746644898,-21.4883838060477,
12.0159844281489));
#154679=CARTESIAN_POINT('Ctrl Pts',(-18.4703937789414,-21.4997801537403,
12.0201539940929));
#154680=CARTESIAN_POINT('Ctrl Pts',(-18.5542765244138,-21.5070669096296,
12.024323560037));
#154681=CARTESIAN_POINT('Ctrl Pts',(-18.6382858147563,-21.5102100763509,
12.028493125981));
#154682=CARTESIAN_POINT('Ctrl Pts',(-18.7252487681107,-21.5134637529366,
12.0328092887199));
#154683=CARTESIAN_POINT('Ctrl Pts',(-18.8123468034828,-21.5122770220956,
12.0371254514589));
#154684=CARTESIAN_POINT('Ctrl Pts',(-18.8990948495902,-21.5066709554537,
12.0414416141978));
#154685=CARTESIAN_POINT('Ctrl Pts',(-18.9830170872199,-21.501247505843,
12.0456171783895));
#154686=CARTESIAN_POINT('Ctrl Pts',(-19.0666113245951,-21.4916883190585,
12.0497927425811));
#154687=CARTESIAN_POINT('Ctrl Pts',(-19.1494452607497,-21.4780651684627,
12.0539683067728));
#154688=CARTESIAN_POINT('Ctrl Pts',(-19.2364629421006,-21.4637539449163,
12.0583547687854));
#154689=CARTESIAN_POINT('Ctrl Pts',(-19.3226409276417,-21.444957551129,
12.0627412307979));
#154690=CARTESIAN_POINT('Ctrl Pts',(-19.4074943094419,-21.4218189033104,
12.0671276928105));
#154691=CARTESIAN_POINT('Ctrl Pts',(-19.4923476912421,-21.3986802554918,
12.071514154823));
#154692=CARTESIAN_POINT('Ctrl Pts',(-19.5758759419182,-21.371199607226,
12.0759006168356));
#154693=CARTESIAN_POINT('Ctrl Pts',(-19.6576188802164,-21.3395778865008,
12.0802870788481));
#154694=CARTESIAN_POINT('Ctrl Pts',(-19.7356007047513,-21.3094111280209,
12.0844717132412));
#154695=CARTESIAN_POINT('Ctrl Pts',(-19.8122481596154,-21.2753637103369,
12.0886563476342));
#154696=CARTESIAN_POINT('Ctrl Pts',(-19.8871479757777,-21.2375742704974,
12.0928409820272));
#154697=CARTESIAN_POINT('Ctrl Pts',(-19.9619411813225,-21.1998386192481,
12.0970196601112));
#154698=CARTESIAN_POINT('Ctrl Pts',(-20.0349912820117,-21.1583717310105,
12.1011983381951));
#154699=CARTESIAN_POINT('Ctrl Pts',(-20.1059035528267,-21.1133608309908,
12.1053770162791));
#154700=CARTESIAN_POINT('Ctrl Pts',(-20.1780868751323,-21.0675431429372,
12.1096305941645));
#154701=CARTESIAN_POINT('Ctrl Pts',(-20.2480545228573,-21.0180533145438,
12.11388417205));
#154702=CARTESIAN_POINT('Ctrl Pts',(-20.3154149295588,-20.9651385497696,
12.1181377499354));
#154703=CARTESIAN_POINT('Ctrl Pts',(-20.3814694233334,-20.9132496409652,
12.1223088639134));
#154704=CARTESIAN_POINT('Ctrl Pts',(-20.4450164884367,-20.8580677061306,
12.1264799778913));
#154705=CARTESIAN_POINT('Ctrl Pts',(-20.5057163649395,-20.7998693466275,
12.1306510918693));
#154706=CARTESIAN_POINT('Ctrl Pts',(-20.5663958730126,-20.7416905161459,
12.1348208061896));
#154707=CARTESIAN_POINT('Ctrl Pts',(-20.6242297581416,-20.6804975893352,
12.13899052051));
#154708=CARTESIAN_POINT('Ctrl Pts',(-20.6789132852951,-20.6166057529285,
12.1431602348304));
#154709=CARTESIAN_POINT('Ctrl Pts',(-20.7335948665741,-20.5527161900675,
12.1473298007744));
#154710=CARTESIAN_POINT('Ctrl Pts',(-20.785126014285,-20.486128258616,12.1514993667185));
#154711=CARTESIAN_POINT('Ctrl Pts',(-20.8332415555809,-20.4171910767277,
12.1556689326625));
#154712=CARTESIAN_POINT('Ctrl Pts',(-20.8830487799517,-20.3458301485675,
12.1599850954014));
#154713=CARTESIAN_POINT('Ctrl Pts',(-20.9291954417206,-20.2719521294864,
12.1643012581404));
#154714=CARTESIAN_POINT('Ctrl Pts',(-20.9714366989051,-20.1959762933403,
12.1686174208793));
#154715=CARTESIAN_POINT('Ctrl Pts',(-21.0123019515798,-20.1224753620654,
12.172792985071));
#154716=CARTESIAN_POINT('Ctrl Pts',(-21.0495121634692,-20.0470116310055,
12.1769685492626));
#154717=CARTESIAN_POINT('Ctrl Pts',(-21.0828936882991,-19.96998744642,12.1811441134543));
#154718=CARTESIAN_POINT('Ctrl Pts',(-21.117961234591,-19.8890729533789,
12.1855305754669));
#154719=CARTESIAN_POINT('Ctrl Pts',(-21.1488029510882,-19.8064367740456,
12.1899170374794));
#154720=CARTESIAN_POINT('Ctrl Pts',(-21.1752765362399,-19.7225639970856,
12.1943034994919));
#154721=CARTESIAN_POINT('Ctrl Pts',(-21.2017501213916,-19.6386912201256,
12.1986899615045));
#154722=CARTESIAN_POINT('Ctrl Pts',(-21.2238555029593,-19.5535824262448,
12.203076423517));
#154723=CARTESIAN_POINT('Ctrl Pts',(-21.2415125421985,-19.4677333135615,
12.2074628855296));
#154724=CARTESIAN_POINT('Ctrl Pts',(-21.2654843862316,-19.3511814097151,
12.2134181072288));
#154725=CARTESIAN_POINT('Ctrl Pts',(-21.2813366135095,-19.2329068373031,
12.219373328928));
#154726=CARTESIAN_POINT('Ctrl Pts',(-21.2888788650992,-19.1138455580776,
12.2253285506272));
#154727=CARTESIAN_POINT('Ctrl Pts',(-21.2922399536332,-19.060787728371,
12.2279824036753));
#154728=CARTESIAN_POINT('Ctrl Pts',(-21.2939513313562,-19.0075739736056,
12.2306362567234));
#154729=CARTESIAN_POINT('Ctrl Pts',(-21.293998976612,-18.9542890490546,
12.2332901097715));
#154730=CARTESIAN_POINT('',(-21.2939992159918,-18.9499964727371,12.1667098902285));
#154731=CARTESIAN_POINT('Ctrl Pts',(-17.1744641402401,-20.9821349467765,
11.8833305046723));
#154732=CARTESIAN_POINT('Ctrl Pts',(-17.2411432256658,-21.0333573667355,
11.887499997654));
#154733=CARTESIAN_POINT('Ctrl Pts',(-17.3103630271814,-21.0813023994611,
11.8916694906356));
#154734=CARTESIAN_POINT('Ctrl Pts',(-17.3817636652371,-21.1257195989702,
11.8958389836172));
#154735=CARTESIAN_POINT('Ctrl Pts',(-17.4531713785687,-21.1701411998956,
11.9000088897648));
#154736=CARTESIAN_POINT('Ctrl Pts',(-17.5267599662335,-21.2110340315857,
11.9041787959124));
#154737=CARTESIAN_POINT('Ctrl Pts',(-17.6021424969676,-21.2481921942271,
11.90834870206));
#154738=CARTESIAN_POINT('Ctrl Pts',(-17.6776049649932,-21.2853897602004,
11.9125230300676));
#154739=CARTESIAN_POINT('Ctrl Pts',(-17.7548647608072,-21.3188445462589,
11.9166973580753));
#154740=CARTESIAN_POINT('Ctrl Pts',(-17.8335128509122,-21.3483978998338,
11.9208716860829));
#154741=CARTESIAN_POINT('Ctrl Pts',(-17.9122051113765,-21.3779678511702,
11.9250483584777));
#154742=CARTESIAN_POINT('Ctrl Pts',(-17.9922867803495,-21.4036318669961,
11.9292250308725));
#154743=CARTESIAN_POINT('Ctrl Pts',(-18.0733337771331,-21.425281250073,
11.9334017032672));
#154744=CARTESIAN_POINT('Ctrl Pts',(-18.1545198069368,-21.4469677718377,
11.9375855405836));
#154745=CARTESIAN_POINT('Ctrl Pts',(-18.2366740216876,-21.4646258106057,
11.9417693778999));
#154746=CARTESIAN_POINT('Ctrl Pts',(-18.3193625425945,-21.4781978898963,
11.9459532152163));
#154747=CARTESIAN_POINT('Ctrl Pts',(-18.3758383423869,-21.4874675445518,
11.9488107528291));
#154748=CARTESIAN_POINT('Ctrl Pts',(-18.4325632297361,-21.4948322585704,
11.951668290442));
#154749=CARTESIAN_POINT('Ctrl Pts',(-18.489398605575,-21.500287691342,11.9545258280548));
#154750=CARTESIAN_POINT('Ctrl Pts',(-18.5726294499945,-21.5082767346017,
11.9587104624479));
#154751=CARTESIAN_POINT('Ctrl Pts',(-18.6564069960724,-21.5121986934545,
11.9628950968409));
#154752=CARTESIAN_POINT('Ctrl Pts',(-18.7402996751639,-21.5119922488345,
11.967079731234));
#154753=CARTESIAN_POINT('Ctrl Pts',(-18.8240729434107,-21.5117860980629,
11.9712584093179));
#154754=CARTESIAN_POINT('Ctrl Pts',(-18.9079605630616,-21.507463217065,
11.9754370874019));
#154755=CARTESIAN_POINT('Ctrl Pts',(-18.9915257624727,-21.4990140324825,
11.9796157654858));
#154756=CARTESIAN_POINT('Ctrl Pts',(-19.0765888080259,-21.4904134023388,
11.9838693433713));
#154757=CARTESIAN_POINT('Ctrl Pts',(-19.1613172809487,-21.4775370395472,
11.9881229212567));
#154758=CARTESIAN_POINT('Ctrl Pts',(-19.2452503475953,-21.4604304020809,
11.9923764991421));
#154759=CARTESIAN_POINT('Ctrl Pts',(-19.327556207963,-21.4436554101627,
11.9965476131201));
#154760=CARTESIAN_POINT('Ctrl Pts',(-19.4090967563153,-21.4228128002074,
12.000718727098));
#154761=CARTESIAN_POINT('Ctrl Pts',(-19.4894442918872,-21.3979975310403,
12.004889841076));
#154762=CARTESIAN_POINT('Ctrl Pts',(-19.5697648660674,-21.3731905888764,
12.0090595553964));
#154763=CARTESIAN_POINT('Ctrl Pts',(-19.6488927833423,-21.3444137706278,
12.0132292697167));
#154764=CARTESIAN_POINT('Ctrl Pts',(-19.7264143560961,-21.3118122268126,
12.0173989840371));
#154765=CARTESIAN_POINT('Ctrl Pts',(-19.8039331702998,-21.2792118431002,
12.0215685499811));
#154766=CARTESIAN_POINT('Ctrl Pts',(-19.8798453299036,-21.2427871835461,
12.0257381159252));
#154767=CARTESIAN_POINT('Ctrl Pts',(-19.9537573024932,-21.2027314639944,
12.0299076818692));
#154768=CARTESIAN_POINT('Ctrl Pts',(-20.0302679288589,-21.1612674347574,
12.0342238446082));
#154769=CARTESIAN_POINT('Ctrl Pts',(-20.1046346343672,-21.1159125099134,
12.0385400073471));
#154770=CARTESIAN_POINT('Ctrl Pts',(-20.1764506132335,-21.0669317313763,
12.042856170086));
#154771=CARTESIAN_POINT('Ctrl Pts',(-20.245927194142,-21.0195464965481,
12.0470317342777));
#154772=CARTESIAN_POINT('Ctrl Pts',(-20.3130163291631,-20.9687683266671,
12.0512072984694));
#154773=CARTESIAN_POINT('Ctrl Pts',(-20.3773824427363,-20.9148790454091,
12.055382862661));
#154774=CARTESIAN_POINT('Ctrl Pts',(-20.4449995356902,-20.8582679446644,
12.0597693246736));
#154775=CARTESIAN_POINT('Ctrl Pts',(-20.509610870638,-20.7982235859987,
12.0641557866861));
#154776=CARTESIAN_POINT('Ctrl Pts',(-20.5708718020378,-20.7351158074781,
12.0685422486987));
#154777=CARTESIAN_POINT('Ctrl Pts',(-20.6321327334377,-20.6720080289575,
12.0729287107112));
#154778=CARTESIAN_POINT('Ctrl Pts',(-20.6900429364135,-20.6058373172988,
12.0773151727238));
#154779=CARTESIAN_POINT('Ctrl Pts',(-20.7443085775788,-20.5370108589259,
12.0817016347363));
#154780=CARTESIAN_POINT('Ctrl Pts',(-20.796026764239,-20.4714154002739,
12.0858821780095));
#154781=CARTESIAN_POINT('Ctrl Pts',(-20.8446312405901,-20.4031588919979,
12.0900627212828));
#154782=CARTESIAN_POINT('Ctrl Pts',(-20.8898359348525,-20.3325692383937,
12.0942432645561));
#154783=CARTESIAN_POINT('Ctrl Pts',(-20.9349778718437,-20.2620775837717,
12.0984180040186));
#154784=CARTESIAN_POINT('Ctrl Pts',(-20.9767291512524,-20.1892595981083,
12.1025927434812));
#154785=CARTESIAN_POINT('Ctrl Pts',(-21.0148441174669,-20.114475854294,
12.1067674829437));
#154786=CARTESIAN_POINT('Ctrl Pts',(-21.0529176328921,-20.0397734392993,
12.1109376822935));
#154787=CARTESIAN_POINT('Ctrl Pts',(-21.0873624809752,-19.9631099194739,
12.1151078816433));
#154788=CARTESIAN_POINT('Ctrl Pts',(-21.1179772351408,-19.884873272385,
12.119278080993));
#154789=CARTESIAN_POINT('Ctrl Pts',(-21.1485693987593,-19.8066943559137,
12.1234452031636));
#154790=CARTESIAN_POINT('Ctrl Pts',(-21.1753369141578,-19.7269450449952,
12.1276123253341));
#154791=CARTESIAN_POINT('Ctrl Pts',(-21.1981256703524,-19.6460350716717,
12.1317794475047));
#154792=CARTESIAN_POINT('Ctrl Pts',(-21.2209040463206,-19.5651619526563,
12.1359446715606));
#154793=CARTESIAN_POINT('Ctrl Pts',(-21.2397071410259,-19.4831296648113,
12.1401098956165));
#154794=CARTESIAN_POINT('Ctrl Pts',(-21.2544305326003,-19.4003636139743,
12.1442751196725));
#154795=CARTESIAN_POINT('Ctrl Pts',(-21.2691564647156,-19.3175832817451,
12.1484410624433));
#154796=CARTESIAN_POINT('Ctrl Pts',(-21.2798011983648,-19.2340693856731,
12.1526070052142));
#154797=CARTESIAN_POINT('Ctrl Pts',(-21.2863115236391,-19.1502571216861,
12.1567729479851));
#154798=CARTESIAN_POINT('Ctrl Pts',(-21.2914878410454,-19.0836185341096,
12.1600852620662));
#154799=CARTESIAN_POINT('Ctrl Pts',(-21.2940514917317,-19.0167915973239,
12.1633975761474));
#154800=CARTESIAN_POINT('Ctrl Pts',(-21.2939992159918,-18.9499964727371,
12.1667098902285));
#154801=CARTESIAN_POINT('Ctrl Pts',(-21.2916488572292,-18.9499800095201,
12.1667107986763));
#154802=CARTESIAN_POINT('Ctrl Pts',(-21.2937096036451,-18.6667985676303,
12.1807663462568));
#154803=CARTESIAN_POINT('Ctrl Pts',(-21.1196059381089,-17.531999452779,
12.2372138293977));
#154804=CARTESIAN_POINT('Ctrl Pts',(-19.4558314590011,-16.0122295713503,
12.3360532480991));
#154805=CARTESIAN_POINT('Ctrl Pts',(-16.6528319764031,-16.753811999413,
12.4632290547806));
#154806=CARTESIAN_POINT('Ctrl Pts',(-15.8397231370972,-19.2634826000374,
12.5789421006038));
#154807=CARTESIAN_POINT('Ctrl Pts',(-16.6852502659176,-20.5975253964419,
12.6522632108666));
#154808=CARTESIAN_POINT('Ctrl Pts',(-17.1750494479184,-20.9813915763783,
12.6831923855689));
#154809=CARTESIAN_POINT('Origin',(-18.734,-18.952,-1.76670989022851));
#154810=CARTESIAN_POINT('',(-17.1744641402401,-20.9821349467765,13.549865697334));
#154811=CARTESIAN_POINT('',(-17.1744641402401,-20.9821349467765,13.4833228496967));
#154812=CARTESIAN_POINT('',(-17.1744641402401,-20.9821349467765,-1.76670989022851));
#154813=CARTESIAN_POINT('',(-21.293999998394,-18.9520906788001,13.0332901097364));
#154814=CARTESIAN_POINT('Ctrl Pts',(-21.293999998394,-18.9520906780896,
13.0332901097715));
#154815=CARTESIAN_POINT('Ctrl Pts',(-21.2940031178915,-18.8640218456489,
13.0376462156856));
#154816=CARTESIAN_POINT('Ctrl Pts',(-21.2894573285641,-18.7760356076548,
13.0420023215996));
#154817=CARTESIAN_POINT('Ctrl Pts',(-21.2804139262416,-18.6886065372051,
13.0463584275137));
#154818=CARTESIAN_POINT('Ctrl Pts',(-21.2713470661108,-18.600950683262,
13.0507258327921));
#154819=CARTESIAN_POINT('Ctrl Pts',(-21.2577593163574,-18.5138552818864,
13.0550932380704));
#154820=CARTESIAN_POINT('Ctrl Pts',(-21.2397536148681,-18.4277874271106,
13.0594606433487));
#154821=CARTESIAN_POINT('Ctrl Pts',(-21.2217244341812,-18.3416073409855,
13.0638337436661));
#154822=CARTESIAN_POINT('Ctrl Pts',(-21.1992659159007,-18.25645785704,13.0682068439834));
#154823=CARTESIAN_POINT('Ctrl Pts',(-21.172530963322,-18.1727909517209,
13.0725799443007));
#154824=CARTESIAN_POINT('Ctrl Pts',(-21.1457232584229,-18.0888963683656,
13.0769649448896));
#154825=CARTESIAN_POINT('Ctrl Pts',(-21.114615990053,-18.0064928038113,
13.0813499454785));
#154826=CARTESIAN_POINT('Ctrl Pts',(-21.0794107185113,-17.9260133716796,
13.0857349460673));
#154827=CARTESIAN_POINT('Ctrl Pts',(-21.0474072811094,-17.8528533488881,
13.0897211414781));
#154828=CARTESIAN_POINT('Ctrl Pts',(-21.0120180507083,-17.7812832866316,
13.0937073368888));
#154829=CARTESIAN_POINT('Ctrl Pts',(-20.9734262024016,-17.7116088181557,
13.0976935322996));
#154830=CARTESIAN_POINT('Ctrl Pts',(-20.9329131921061,-17.638465846711,
13.1018781666926));
#154831=CARTESIAN_POINT('Ctrl Pts',(-20.8887375841054,-17.5671736686978,
13.1060628010856));
#154832=CARTESIAN_POINT('Ctrl Pts',(-20.8410930441,-17.4981228031551,13.1102474354787));
#154833=CARTESIAN_POINT('Ctrl Pts',(-20.7935163202,-17.4291702229728,13.1144261135626));
#154834=CARTESIAN_POINT('Ctrl Pts',(-20.742480730941,-17.3624529938654,
13.1186047916466));
#154835=CARTESIAN_POINT('Ctrl Pts',(-20.6882255495789,-17.2983366420662,
13.1227834697305));
#154836=CARTESIAN_POINT('Ctrl Pts',(-20.6329978830833,-17.2330710507404,
13.1270370476159));
#154837=CARTESIAN_POINT('Ctrl Pts',(-20.5744343004285,-17.1705009170565,
13.1312906255014));
#154838=CARTESIAN_POINT('Ctrl Pts',(-20.5128330635405,-17.110980463967,
13.1355442033868));
#154839=CARTESIAN_POINT('Ctrl Pts',(-20.4524260868345,-17.0526139310052,
13.1397153173648));
#154840=CARTESIAN_POINT('Ctrl Pts',(-20.3890985326093,-16.9971802202221,
13.1438864313427));
#154841=CARTESIAN_POINT('Ctrl Pts',(-20.3231707254824,-16.9449782250135,
13.1480575453207));
#154842=CARTESIAN_POINT('Ctrl Pts',(-20.2572650410679,-16.8927937466886,
13.152227259641));
#154843=CARTESIAN_POINT('Ctrl Pts',(-20.1887611969923,-16.8438391155733,
13.1563969739614));
#154844=CARTESIAN_POINT('Ctrl Pts',(-20.1180129698817,-16.7983732683682,
13.1605666882818));
#154845=CARTESIAN_POINT('Ctrl Pts',(-20.0472672602966,-16.752909039033,
13.1647362542258));
#154846=CARTESIAN_POINT('Ctrl Pts',(-19.9742777139364,-16.7109335947648,
13.1689058201699));
#154847=CARTESIAN_POINT('Ctrl Pts',(-19.899426330545,-16.6726620548781,
13.1730753861139));
#154848=CARTESIAN_POINT('Ctrl Pts',(-19.8219432648527,-16.633044934862,
13.1773915488528));
#154849=CARTESIAN_POINT('Ctrl Pts',(-19.7424654713777,-16.5973972639688,
13.1817077115918));
#154850=CARTESIAN_POINT('Ctrl Pts',(-19.6614416802129,-16.5659044592046,
13.1860238743307));
#154851=CARTESIAN_POINT('Ctrl Pts',(-19.5830572305231,-16.5354375292431,
13.1901994385224));
#154852=CARTESIAN_POINT('Ctrl Pts',(-19.5032264199666,-16.508859036806,
13.1943750027141));
#154853=CARTESIAN_POINT('Ctrl Pts',(-19.422371506106,-16.4862861744352,
13.1985505669057));
#154854=CARTESIAN_POINT('Ctrl Pts',(-19.3374328027605,-16.4625732104479,
13.2029370289183));
#154855=CARTESIAN_POINT('Ctrl Pts',(-19.2513643920955,-16.4432812873466,
13.2073234909308));
#154856=CARTESIAN_POINT('Ctrl Pts',(-19.1646662302709,-16.4284852688949,
13.2117099529434));
#154857=CARTESIAN_POINT('Ctrl Pts',(-19.0779680684463,-16.4136892504433,
13.2160964149559));
#154858=CARTESIAN_POINT('Ctrl Pts',(-18.9906407405946,-16.4033891290646,
13.2204828769685));
#154859=CARTESIAN_POINT('Ctrl Pts',(-18.9031862415112,-16.3975967398073,
13.224869338981));
#154860=CARTESIAN_POINT('Ctrl Pts',(-18.8197556535693,-16.3920708669661,
13.2290539733741));
#154861=CARTESIAN_POINT('Ctrl Pts',(-18.7358987953378,-16.3906264585577,
13.2332386077671));
#154862=CARTESIAN_POINT('Ctrl Pts',(-18.6520488590979,-16.3933120529254,
13.2374232421602));
#154863=CARTESIAN_POINT('Ctrl Pts',(-18.5683182728639,-16.3959938246819,
13.2416019202441));
#154864=CARTESIAN_POINT('Ctrl Pts',(-18.4845950449155,-16.4027939079682,
13.2457805983281));
#154865=CARTESIAN_POINT('Ctrl Pts',(-18.4013160390444,-16.413708964259,
13.249959276412));
#154866=CARTESIAN_POINT('Ctrl Pts',(-18.3165443168447,-16.4248196650894,
13.2542128542974));
#154867=CARTESIAN_POINT('Ctrl Pts',(-18.2322333798101,-16.4401943435876,
13.2584664321829));
#154868=CARTESIAN_POINT('Ctrl Pts',(-18.1488425169102,-16.4597739428407,
13.2627200100683));
#154869=CARTESIAN_POINT('Ctrl Pts',(-18.0670683486115,-16.4789739533558,
13.2668911240463));
#154870=CARTESIAN_POINT('Ctrl Pts',(-17.9861793664178,-16.502217188393,
13.2710622380242));
#154871=CARTESIAN_POINT('Ctrl Pts',(-17.9066002780142,-16.5293960909679,
13.2752333520022));
#154872=CARTESIAN_POINT('Ctrl Pts',(-17.8270478931422,-16.5565658733995,
13.2794030663225));
#154873=CARTESIAN_POINT('Ctrl Pts',(-17.7488049640925,-16.587668551974,
13.2835727806429));
#154874=CARTESIAN_POINT('Ctrl Pts',(-17.6722807082305,-16.6225468140603,
13.2877424949633));
#154875=CARTESIAN_POINT('Ctrl Pts',(-17.59575917543,-16.6574238350284,13.2919120609074));
#154876=CARTESIAN_POINT('Ctrl Pts',(-17.52095661247,-16.6960759808161,13.2960816268514));
#154877=CARTESIAN_POINT('Ctrl Pts',(-17.4482606698669,-16.7382984900966,
13.3002511927954));
#154878=CARTESIAN_POINT('Ctrl Pts',(-17.373008827602,-16.7820054907161,
13.3045673555344));
#154879=CARTESIAN_POINT('Ctrl Pts',(-17.3000149555547,-16.8295383292521,
13.3088835182733));
#154880=CARTESIAN_POINT('Ctrl Pts',(-17.2296778491727,-16.8806200574182,
13.3131996810122));
#154881=CARTESIAN_POINT('Ctrl Pts',(-17.1616319666328,-16.9300378036622,
13.3173752452039));
#154882=CARTESIAN_POINT('Ctrl Pts',(-17.0960727569876,-16.9827764479854,
13.3215508093956));
#154883=CARTESIAN_POINT('Ctrl Pts',(-17.0333273206286,-17.0385443727017,
13.3257263735873));
#154884=CARTESIAN_POINT('Ctrl Pts',(-16.9674127614424,-17.0971290027195,
13.3301128355998));
#154885=CARTESIAN_POINT('Ctrl Pts',(-16.904604108851,-17.1590565633928,
13.3344992976123));
#154886=CARTESIAN_POINT('Ctrl Pts',(-16.845234928219,-17.2239471930464,
13.3388857596249));
#154887=CARTESIAN_POINT('Ctrl Pts',(-16.7858657475871,-17.2888378227,13.3432722216374));
#154888=CARTESIAN_POINT('Ctrl Pts',(-16.7299363492649,-17.3566910252288,
13.34765868365));
#154889=CARTESIAN_POINT('Ctrl Pts',(-16.677728404917,-17.4270911085396,
13.3520451456625));
#154890=CARTESIAN_POINT('Ctrl Pts',(-16.6279226254792,-17.4942519796595,
13.3562297800555));
#154891=CARTESIAN_POINT('Ctrl Pts',(-16.5813179797007,-17.5639804959206,
13.3604144144486));
#154892=CARTESIAN_POINT('Ctrl Pts',(-16.5381897594127,-17.6359386840531,
13.3645990488416));
#154893=CARTESIAN_POINT('Ctrl Pts',(-16.495122926808,-17.7077944486114,
13.3687777269256));
#154894=CARTESIAN_POINT('Ctrl Pts',(-16.4555229253635,-17.7818731899369,
13.3729564050095));
#154895=CARTESIAN_POINT('Ctrl Pts',(-16.4196234139922,-17.8578057676358,
13.3771350830935));
#154896=CARTESIAN_POINT('Ctrl Pts',(-16.3830804296802,-17.9350993822182,
13.3813886609789));
#154897=CARTESIAN_POINT('Ctrl Pts',(-16.3503721900681,-18.0143135596365,
13.3856422388643));
#154898=CARTESIAN_POINT('Ctrl Pts',(-16.3216976420463,-18.0950301441644,
13.3898958167498));
#154899=CARTESIAN_POINT('Ctrl Pts',(-16.2935790060916,-18.1741818801958,
13.3940669307277));
#154900=CARTESIAN_POINT('Ctrl Pts',(-16.2693392165557,-18.2547778355446,
13.3982380447057));
#154901=CARTESIAN_POINT('Ctrl Pts',(-16.2491177212504,-18.3364026797034,
13.4024091586836));
#154902=CARTESIAN_POINT('Ctrl Pts',(-16.2289030114633,-18.4180001338574,
13.406578873004));
#154903=CARTESIAN_POINT('Ctrl Pts',(-16.2127040285388,-18.5006253449796,
13.4107485873244));
#154904=CARTESIAN_POINT('Ctrl Pts',(-16.2006099990479,-18.5838490756821,
13.4149183016447));
#154905=CARTESIAN_POINT('Ctrl Pts',(-16.1885163999146,-18.6670698449272,
13.4190878675888));
#154906=CARTESIAN_POINT('Ctrl Pts',(-16.1805275291,-18.7508886360333,13.4232574335328));
#154907=CARTESIAN_POINT('Ctrl Pts',(-16.1766810426043,-18.8348686628405,
13.4274269994769));
#154908=CARTESIAN_POINT('Ctrl Pts',(-16.1726993183887,-18.9218013237896,
13.4317431622158));
#154909=CARTESIAN_POINT('Ctrl Pts',(-16.1731567148618,-19.0089062426187,
13.4360593249547));
#154910=CARTESIAN_POINT('Ctrl Pts',(-16.1780362227548,-19.0956981886122,
13.4403754876936));
#154911=CARTESIAN_POINT('Ctrl Pts',(-16.1827567811915,-19.179662896094,
13.4445510518853));
#154912=CARTESIAN_POINT('Ctrl Pts',(-16.1916156782437,-19.2633342443403,
13.448726616077));
#154913=CARTESIAN_POINT('Ctrl Pts',(-16.2045447628248,-19.3462793465641,
13.4529021802687));
#154914=CARTESIAN_POINT('Ctrl Pts',(-16.2181268647321,-19.4334138087179,
13.4572886422812));
#154915=CARTESIAN_POINT('Ctrl Pts',(-16.236201010622,-19.519746159906,13.4616751042938));
#154916=CARTESIAN_POINT('Ctrl Pts',(-16.2586283495454,-19.6047903125244,
13.4660615663063));
#154917=CARTESIAN_POINT('Ctrl Pts',(-16.2810556884688,-19.6898344651428,
13.4704480283188));
#154918=CARTESIAN_POINT('Ctrl Pts',(-16.3078359712666,-19.7735898897036,
13.4748344903314));
#154919=CARTESIAN_POINT('Ctrl Pts',(-16.3387721302028,-19.8555947386669,
13.4792209523439));
#154920=CARTESIAN_POINT('Ctrl Pts',(-16.3682827836193,-19.9338208908285,
13.4834052908212));
#154921=CARTESIAN_POINT('Ctrl Pts',(-16.4016845822221,-20.0107453980617,
13.4875896292985));
#154922=CARTESIAN_POINT('Ctrl Pts',(-16.438842384675,-20.0859539324045,
13.4917739677759));
#154923=CARTESIAN_POINT('Ctrl Pts',(-16.4759497063984,-20.1610602921992,
13.4959526216205));
#154924=CARTESIAN_POINT('Ctrl Pts',(-16.5168026975527,-20.2344548994179,
13.5001312754651));
#154925=CARTESIAN_POINT('Ctrl Pts',(-16.5612174513804,-20.3057414806432,
13.5043099293097));
#154926=CARTESIAN_POINT('Ctrl Pts',(-16.6055802939412,-20.3769447432318,
13.5084836992093));
#154927=CARTESIAN_POINT('Ctrl Pts',(-16.653496382317,-20.4460444889661,
13.512657469109));
#154928=CARTESIAN_POINT('Ctrl Pts',(-16.704735706151,-20.5126685829187,
13.5168312390086));
#154929=CARTESIAN_POINT('Ctrl Pts',(-16.7559398356268,-20.5792469152951,
13.5210021421032));
#154930=CARTESIAN_POINT('Ctrl Pts',(-16.8104623870239,-20.6433526099033,
13.5251730451978));
#154931=CARTESIAN_POINT('Ctrl Pts',(-16.8680304516944,-20.7046430454591,
13.5293439482923));
#154932=CARTESIAN_POINT('Ctrl Pts',(-16.9255842027873,-20.7659182419165,
13.5335138143442));
#154933=CARTESIAN_POINT('Ctrl Pts',(-16.9861816530085,-20.824379230409,
13.537683680396));
#154934=CARTESIAN_POINT('Ctrl Pts',(-17.0495108542933,-20.8797179041541,
13.5418535464478));
#154935=CARTESIAN_POINT('Ctrl Pts',(-17.0900719586463,-20.9151612332186,
13.5445242634099));
#154936=CARTESIAN_POINT('Ctrl Pts',(-17.1317528860808,-20.949324451798,
13.5471949803719));
#154937=CARTESIAN_POINT('Ctrl Pts',(-17.1744641402401,-20.9821349467765,
13.549865697334));
#154938=CARTESIAN_POINT('Ctrl Pts',(-17.1744641402401,-20.9821349467765,
12.7499597538068));
#154939=CARTESIAN_POINT('Ctrl Pts',(-17.2410532476537,-21.0332882462385,
12.7541315901319));
#154940=CARTESIAN_POINT('Ctrl Pts',(-17.3102191359587,-21.0812059542882,
12.7583034264569));
#154941=CARTESIAN_POINT('Ctrl Pts',(-17.3816116482452,-21.1256250242482,
12.762475262782));
#154942=CARTESIAN_POINT('Ctrl Pts',(-17.4529732632018,-21.1700248704743,
12.7666452936152));
#154943=CARTESIAN_POINT('Ctrl Pts',(-17.5265591985511,-21.2109288425684,
12.7708153244484));
#154944=CARTESIAN_POINT('Ctrl Pts',(-17.6019902058278,-21.2481171193775,
12.7749853552815));
#154945=CARTESIAN_POINT('Ctrl Pts',(-17.6774111955606,-21.2853004574325,
12.7791548323177));
#154946=CARTESIAN_POINT('Ctrl Pts',(-17.7546763576364,-21.3187688776167,
12.7833243093538));
#154947=CARTESIAN_POINT('Ctrl Pts',(-17.8333829516401,-21.3483490839616,
12.78749378639));
#154948=CARTESIAN_POINT('Ctrl Pts',(-17.9121027028482,-21.3779342351631,
12.7916639604283));
#154949=CARTESIAN_POINT('Ctrl Pts',(-17.9922639334031,-21.4036297212893,
12.7958341344665));
#154950=CARTESIAN_POINT('Ctrl Pts',(-18.0734463868029,-21.4253113277734,
12.8000043085048));
#154951=CARTESIAN_POINT('Ctrl Pts',(-18.154718137836,-21.447016783206,12.804179069577));
#154952=CARTESIAN_POINT('Ctrl Pts',(-18.2370129084748,-21.4646994283686,
12.8083538306493));
#154953=CARTESIAN_POINT('Ctrl Pts',(-18.3198983570486,-21.4782857774419,
12.8125285917215));
#154954=CARTESIAN_POINT('Ctrl Pts',(-18.4028354155234,-21.4918805862646,
12.816705952273));
#154955=CARTESIAN_POINT('Ctrl Pts',(-18.486363427206,-21.501373970334,12.8208833128245));
#154956=CARTESIAN_POINT('Ctrl Pts',(-18.5700453931146,-21.5067443877776,
12.825060673376));
#154957=CARTESIAN_POINT('Ctrl Pts',(-18.6538651895487,-21.5121236507048,
12.8292449143563));
#154958=CARTESIAN_POINT('Ctrl Pts',(-18.7378389869997,-21.5133663857226,
12.8334291553365));
#154959=CARTESIAN_POINT('Ctrl Pts',(-18.8215306928142,-21.5105031518088,
12.8376133963167));
#154960=CARTESIAN_POINT('Ctrl Pts',(-18.8597239861841,-21.5091964950524,
12.8395229038567));
#154961=CARTESIAN_POINT('Ctrl Pts',(-18.8978586153629,-21.5070354359871,
12.8414324113967));
#154962=CARTESIAN_POINT('Ctrl Pts',(-18.9358937423124,-21.5040264334084,
12.8433419189367));
#154963=CARTESIAN_POINT('Ctrl Pts',(-19.0192466995766,-21.497432285223,
12.8475265533297));
#154964=CARTESIAN_POINT('Ctrl Pts',(-19.1024313715337,-21.4867379250515,
12.8517111877228));
#154965=CARTESIAN_POINT('Ctrl Pts',(-19.1850120996547,-21.4719579532137,
12.8558958221158));
#154966=CARTESIAN_POINT('Ctrl Pts',(-19.2674752843307,-21.4571990188365,
12.8600745001998));
#154967=CARTESIAN_POINT('Ctrl Pts',(-19.3493357837206,-21.4383661042867,
12.8642531782837));
#154968=CARTESIAN_POINT('Ctrl Pts',(-19.4301618064492,-21.4155256725355,
12.8684318563676));
#154969=CARTESIAN_POINT('Ctrl Pts',(-19.5124365775465,-21.3922758424603,
12.8726854342531));
#154970=CARTESIAN_POINT('Ctrl Pts',(-19.5936389405807,-21.3648734505894,
12.8769390121385));
#154971=CARTESIAN_POINT('Ctrl Pts',(-19.6733229700786,-21.333443335014,
12.881192590024));
#154972=CARTESIAN_POINT('Ctrl Pts',(-19.7514621691741,-21.3026225535599,
12.8853637040019));
#154973=CARTESIAN_POINT('Ctrl Pts',(-19.8281409334345,-21.2679290018995,
12.8895348179798));
#154974=CARTESIAN_POINT('Ctrl Pts',(-19.9029545672468,-21.229530509063,
12.8937059319578));
#154975=CARTESIAN_POINT('Ctrl Pts',(-19.9777430966217,-21.1911449012117,
12.8978756462782));
#154976=CARTESIAN_POINT('Ctrl Pts',(-20.0506673295888,-21.149057031143,
12.9020453605985));
#154977=CARTESIAN_POINT('Ctrl Pts',(-20.1213450915268,-21.1034817212834,
12.9062150749189));
#154978=CARTESIAN_POINT('Ctrl Pts',(-20.1920203384466,-21.0579080331889,
12.9103846408629));
#154979=CARTESIAN_POINT('Ctrl Pts',(-20.2604488871165,-21.008847402065,
12.914554206807));
#154980=CARTESIAN_POINT('Ctrl Pts',(-20.3262767630685,-20.9565584825073,
12.918723772751));
#154981=CARTESIAN_POINT('Ctrl Pts',(-20.3944190659317,-20.9024311490432,
12.9230399354899));
#154982=CARTESIAN_POINT('Ctrl Pts',(-20.4597740011395,-20.8448446181548,
12.9273560982289));
#154983=CARTESIAN_POINT('Ctrl Pts',(-20.521987002802,-20.7841305842682,
12.9316722609678));
#154984=CARTESIAN_POINT('Ctrl Pts',(-20.582173422479,-20.7253943036496,
12.9358478251595));
#154985=CARTESIAN_POINT('Ctrl Pts',(-20.63941917621,-20.6637315251353,12.9400233893512));
#154986=CARTESIAN_POINT('Ctrl Pts',(-20.6934427607502,-20.5994780931301,
12.9441989535428));
#154987=CARTESIAN_POINT('Ctrl Pts',(-20.7501949481167,-20.5319793730223,
12.9485854155554));
#154988=CARTESIAN_POINT('Ctrl Pts',(-20.803390556233,-20.4616218795445,
12.9529718775679));
#154989=CARTESIAN_POINT('Ctrl Pts',(-20.852754442665,-20.3888297086597,
12.9573583395805));
#154990=CARTESIAN_POINT('Ctrl Pts',(-20.9021183290971,-20.316037537775,
12.961744801593));
#154991=CARTESIAN_POINT('Ctrl Pts',(-20.9476502584794,-20.240811225245,
12.9661312636056));
#154992=CARTESIAN_POINT('Ctrl Pts',(-20.9891316170535,-20.1636028184871,
12.9705177256181));
#154993=CARTESIAN_POINT('Ctrl Pts',(-21.0308618762442,-20.0859311380874,
12.9749305077209));
#154994=CARTESIAN_POINT('Ctrl Pts',(-21.0686351706121,-20.0059905501583,
12.9793432898236));
#154995=CARTESIAN_POINT('Ctrl Pts',(-21.1022126120118,-19.9241980375974,
12.9837560719264));
#154996=CARTESIAN_POINT('Ctrl Pts',(-21.1356929152447,-19.8426421474353,
12.9881560880307));
#154997=CARTESIAN_POINT('Ctrl Pts',(-21.1650014030469,-19.759245362016,
12.9925561041351));
#154998=CARTESIAN_POINT('Ctrl Pts',(-21.1899457627449,-19.6744475139796,
12.9969561202394));
#154999=CARTESIAN_POINT('Ctrl Pts',(-21.2148467487816,-19.5897971138308,
13.0013484855236));
#155000=CARTESIAN_POINT('Ctrl Pts',(-21.235398596884,-19.5037508664335,
13.0057408508078));
#155001=CARTESIAN_POINT('Ctrl Pts',(-21.2514572537729,-19.4167676574658,
13.0101332160921));
#155002=CARTESIAN_POINT('Ctrl Pts',(-21.2674789983323,-19.3299843875645,
13.0145154851126));
#155003=CARTESIAN_POINT('Ctrl Pts',(-21.2790280568698,-19.2422688247272,
13.0188977541331));
#155004=CARTESIAN_POINT('Ctrl Pts',(-21.2860106924303,-19.1540926166924,
13.0232800231537));
#155005=CARTESIAN_POINT('Ctrl Pts',(-21.2913273283411,-19.0869545296399,
13.0266167186812));
#155006=CARTESIAN_POINT('Ctrl Pts',(-21.2939976088987,-19.0195497546626,
13.0299534142088));
#155007=CARTESIAN_POINT('Ctrl Pts',(-21.293999998394,-18.9520906788001,
13.0332901097364));
#155008=CARTESIAN_POINT('',(-21.2943301210028,-18.9513574887884,12.9667098341108));
#155009=CARTESIAN_POINT('Ctrl Pts',(-17.1750494479184,-20.9813915763783,
12.6831923855689));
#155010=CARTESIAN_POINT('Ctrl Pts',(-17.356575497218,-21.1236574552614,
12.6946551464271));
#155011=CARTESIAN_POINT('Ctrl Pts',(-18.2953377646256,-21.6766232007702,
12.7485098428457));
#155012=CARTESIAN_POINT('Ctrl Pts',(-20.4360628533385,-21.4324759086211,
12.8430154491812));
#155013=CARTESIAN_POINT('Ctrl Pts',(-21.2952859035193,-19.7651270969621,
12.9260582946585));
#155014=CARTESIAN_POINT('Ctrl Pts',(-21.2980343668152,-18.9513691597422,
12.9667092045753));
#155015=CARTESIAN_POINT('Ctrl Pts',(-21.2939999191096,-18.9513564484225,
12.9667098902285));
#155016=CARTESIAN_POINT('Ctrl Pts',(-21.2939911726516,-18.9165636940744,
12.9684506873211));
#155017=CARTESIAN_POINT('Ctrl Pts',(-21.2932731600888,-18.881780730387,
12.9701914844137));
#155018=CARTESIAN_POINT('Ctrl Pts',(-21.2918468828523,-18.8470270326106,
12.9719322815063));
#155019=CARTESIAN_POINT('Ctrl Pts',(-21.2884183105029,-18.7634839708603,
12.9761169158993));
#155020=CARTESIAN_POINT('Ctrl Pts',(-21.2808860937369,-18.6799535889704,
12.9803015502924));
#155021=CARTESIAN_POINT('Ctrl Pts',(-21.2692483017375,-18.5968717857769,
12.9844861846854));
#155022=CARTESIAN_POINT('Ctrl Pts',(-21.2576270746945,-18.5139082392468,
12.9886648627694));
#155023=CARTESIAN_POINT('Ctrl Pts',(-21.2419119432712,-18.4313924548469,
12.9928435408533));
#155024=CARTESIAN_POINT('Ctrl Pts',(-21.2221529486457,-18.3497584337279,
12.9970222189372));
#155025=CARTESIAN_POINT('Ctrl Pts',(-21.2020397882419,-18.2666611814494,
13.0012757968227));
#155026=CARTESIAN_POINT('Ctrl Pts',(-21.1777363859676,-18.1844780963255,
13.0055293747081));
#155027=CARTESIAN_POINT('Ctrl Pts',(-21.1493505801536,-18.1036595170853,
13.0097829525935));
#155028=CARTESIAN_POINT('Ctrl Pts',(-21.1215150885756,-18.0244077637083,
13.0139540665715));
#155029=CARTESIAN_POINT('Ctrl Pts',(-21.0897542310845,-17.9464685351597,
13.0181251805494));
#155030=CARTESIAN_POINT('Ctrl Pts',(-21.0542203695086,-17.8702526002261,
13.0222962945274));
#155031=CARTESIAN_POINT('Ctrl Pts',(-21.0186984316631,-17.7940622402855,
13.0264660088478));
#155032=CARTESIAN_POINT('Ctrl Pts',(-20.9794061983924,-17.7195944421082,
13.0306357231681));
#155033=CARTESIAN_POINT('Ctrl Pts',(-20.9365438451406,-17.6472392517272,
13.0348054374885));
#155034=CARTESIAN_POINT('Ctrl Pts',(-20.8936830171152,-17.5748866360543,
13.0389750034325));
#155035=CARTESIAN_POINT('Ctrl Pts',(-20.8472525568965,-17.5046468740728,
13.0431445693766));
#155036=CARTESIAN_POINT('Ctrl Pts',(-20.7974975099507,-17.4368834941077,
13.0473141353206));
#155037=CARTESIAN_POINT('Ctrl Pts',(-20.7459931369336,-17.366737637298,
13.0516302980595));
#155038=CARTESIAN_POINT('Ctrl Pts',(-20.6909263546122,-17.2992459668448,
13.0559464607985));
#155039=CARTESIAN_POINT('Ctrl Pts',(-20.6326151733211,-17.234775371818,
13.0602626235374));
#155040=CARTESIAN_POINT('Ctrl Pts',(-20.5762034726275,-17.1724048996433,
13.0644381877291));
#155041=CARTESIAN_POINT('Ctrl Pts',(-20.5167558657732,-17.1128620023875,
13.0686137519208));
#155042=CARTESIAN_POINT('Ctrl Pts',(-20.4545972806997,-17.0564407163983,
13.0727893161124));
#155043=CARTESIAN_POINT('Ctrl Pts',(-20.3892992132619,-16.9971697253824,
13.077175778125));
#155044=CARTESIAN_POINT('Ctrl Pts',(-20.3210095593889,-16.9413443477726,
13.0815622401375));
#155045=CARTESIAN_POINT('Ctrl Pts',(-20.2501416763133,-16.889255610274,
13.0859487021501));
#155046=CARTESIAN_POINT('Ctrl Pts',(-20.1792737932376,-16.8371668727754,
13.0903351641627));
#155047=CARTESIAN_POINT('Ctrl Pts',(-20.1058282074104,-16.7888150309008,
13.0947216261752));
#155048=CARTESIAN_POINT('Ctrl Pts',(-20.0302483510417,-16.7444356832877,
13.0991080881878));
#155049=CARTESIAN_POINT('Ctrl Pts',(-19.958146035901,-16.7020982952443,
13.1032927225808));
#155050=CARTESIAN_POINT('Ctrl Pts',(-19.8838331576254,-16.6632182861073,
13.1074773569739));
#155051=CARTESIAN_POINT('Ctrl Pts',(-19.8076751930389,-16.6280332231607,
13.1116619913669));
#155052=CARTESIAN_POINT('Ctrl Pts',(-19.7316256298885,-16.5928982417961,
13.1158406694508));
#155053=CARTESIAN_POINT('Ctrl Pts',(-19.6537366110356,-16.5614479512896,
13.1200193475348));
#155054=CARTESIAN_POINT('Ctrl Pts',(-19.5744001491065,-16.533875191521,
13.1241980256187));
#155055=CARTESIAN_POINT('Ctrl Pts',(-19.4936416381154,-16.5058082098496,
13.1284516035042));
#155056=CARTESIAN_POINT('Ctrl Pts',(-19.4113836985809,-16.4817593798136,
13.1327051813896));
#155057=CARTESIAN_POINT('Ctrl Pts',(-19.3280633649497,-16.461881786255,
13.136958759275));
#155058=CARTESIAN_POINT('Ctrl Pts',(-19.2463583585721,-16.4423895586354,
13.141129873253));
#155059=CARTESIAN_POINT('Ctrl Pts',(-19.1636322517454,-16.4269083873419,
13.1453009872309));
#155060=CARTESIAN_POINT('Ctrl Pts',(-19.0803129065813,-16.4155325015417,
13.1494721012089));
#155061=CARTESIAN_POINT('Ctrl Pts',(-18.9970215200281,-16.4041604330299,
13.1536418155293));
#155062=CARTESIAN_POINT('Ctrl Pts',(-18.9131377459123,-16.39689097632,13.1578115298496));
#155063=CARTESIAN_POINT('Ctrl Pts',(-18.8290979023925,-16.3937669400618,
13.16198124417));
#155064=CARTESIAN_POINT('Ctrl Pts',(-18.745061049371,-16.3906430149703,
13.1661508101141));
#155065=CARTESIAN_POINT('Ctrl Pts',(-18.6608685977347,-16.3916642332765,
13.1703203760581));
#155066=CARTESIAN_POINT('Ctrl Pts',(-18.5769588557387,-16.3968213215102,
13.1744899420021));
#155067=CARTESIAN_POINT('Ctrl Pts',(-18.4900989507281,-16.4021597266041,
13.1788061047411));
#155068=CARTESIAN_POINT('Ctrl Pts',(-18.4035425318192,-16.4119302148937,
13.18312226748));
#155069=CARTESIAN_POINT('Ctrl Pts',(-18.317770227621,-16.4260639801085,
13.1874384302189));
#155070=CARTESIAN_POINT('Ctrl Pts',(-18.2347919472103,-16.4397373394081,
13.1916139944106));
#155071=CARTESIAN_POINT('Ctrl Pts',(-18.1525479314087,-16.4574939280206,
13.1957895586023));
#155072=CARTESIAN_POINT('Ctrl Pts',(-18.0714612955844,-16.4792196892665,
13.1999651227939));
#155073=CARTESIAN_POINT('Ctrl Pts',(-17.9862791665499,-16.5020427670648,
13.2043515848065));
#155074=CARTESIAN_POINT('Ctrl Pts',(-17.9023749641123,-16.5292463408116,
13.208738046819));
#155075=CARTESIAN_POINT('Ctrl Pts',(-17.8202171381047,-16.5606403697255,
13.2131245088315));
#155076=CARTESIAN_POINT('Ctrl Pts',(-17.7380593120971,-16.5920343986394,
13.2175109708441));
#155077=CARTESIAN_POINT('Ctrl Pts',(-17.6576483623233,-16.6276185783625,
13.2218974328566));
#155078=CARTESIAN_POINT('Ctrl Pts',(-17.579422411398,-16.6671475776545,
13.2262838948691));
#155079=CARTESIAN_POINT('Ctrl Pts',(-17.5047957524333,-16.7048577890932,
13.2304685292622));
#155080=CARTESIAN_POINT('Ctrl Pts',(-17.4318796660886,-16.7462981479269,
13.2346531636552));
#155081=CARTESIAN_POINT('Ctrl Pts',(-17.3610717345267,-16.7912899366494,
13.2388377980483));
#155082=CARTESIAN_POINT('Ctrl Pts',(-17.2903645892912,-16.8362176851296,
13.2430164761322));
#155083=CARTESIAN_POINT('Ctrl Pts',(-17.2217600234685,-16.8846865780311,
13.2471951542162));
#155084=CARTESIAN_POINT('Ctrl Pts',(-17.1556323738796,-16.9364713753421,
13.2513738323001));
#155085=CARTESIAN_POINT('Ctrl Pts',(-17.0883194336969,-16.989184377928,
13.2556274101856));
#155086=CARTESIAN_POINT('Ctrl Pts',(-17.0235735109215,-17.045333111899,
13.259880988071));
#155087=CARTESIAN_POINT('Ctrl Pts',(-16.9617598841366,-17.1046329623693,
13.2641345659564));
#155088=CARTESIAN_POINT('Ctrl Pts',(-16.9011446351263,-17.1627831695241,
13.2683056799344));
#155089=CARTESIAN_POINT('Ctrl Pts',(-16.8433493474163,-17.2239630692775,
13.2724767939123));
#155090=CARTESIAN_POINT('Ctrl Pts',(-16.7886848464703,-17.2878639017653,
13.2766479078903));
#155091=CARTESIAN_POINT('Ctrl Pts',(-16.7340386887256,-17.3517432917117,
13.2808176222107));
#155092=CARTESIAN_POINT('Ctrl Pts',(-16.6825215301017,-17.4183414518072,
13.284987336531));
#155093=CARTESIAN_POINT('Ctrl Pts',(-16.6344055366424,-17.4873146790392,
13.2891570508514));
#155094=CARTESIAN_POINT('Ctrl Pts',(-16.5862912553567,-17.5562854519078,
13.2933266167954));
#155095=CARTESIAN_POINT('Ctrl Pts',(-16.5415781611062,-17.6276307460898,
13.2974961827395));
#155096=CARTESIAN_POINT('Ctrl Pts',(-16.5004957043155,-17.7009769941529,
13.3016657486835));
#155097=CARTESIAN_POINT('Ctrl Pts',(-16.4579688390246,-17.7769020058155,
13.3059819114224));
#155098=CARTESIAN_POINT('Ctrl Pts',(-16.4193329255797,-17.8549708362668,
13.3102980741614));
#155099=CARTESIAN_POINT('Ctrl Pts',(-16.3847902639464,-17.934742109379,
13.3146142369003));
#155100=CARTESIAN_POINT('Ctrl Pts',(-16.3513728258825,-18.0119148416598,
13.318789801092));
#155101=CARTESIAN_POINT('Ctrl Pts',(-16.3217861809923,-18.0906803481869,
13.3229653652836));
#155102=CARTESIAN_POINT('Ctrl Pts',(-16.2961634499818,-18.1706211191776,
13.3271409294753));
#155103=CARTESIAN_POINT('Ctrl Pts',(-16.2692465757401,-18.2545995084699,
13.3315273914879));
#155104=CARTESIAN_POINT('Ctrl Pts',(-16.2467047227919,-18.3398744431048,
13.3359138535004));
#155105=CARTESIAN_POINT('Ctrl Pts',(-16.2286316599242,-18.4259491654359,
13.340300315513));
#155106=CARTESIAN_POINT('Ctrl Pts',(-16.2105585970564,-18.5120238877669,
13.3446867775255));
#155107=CARTESIAN_POINT('Ctrl Pts',(-16.1969543388866,-18.598897812795,
13.3490732395381));
#155108=CARTESIAN_POINT('Ctrl Pts',(-16.1878497481281,-18.6860697555883,
13.3534597015506));
#155109=CARTESIAN_POINT('Ctrl Pts',(-16.1791640730867,-18.7692307880738,
13.3576443359436));
#155110=CARTESIAN_POINT('Ctrl Pts',(-16.1745407622114,-18.852972557727,
13.3618289703367));
#155111=CARTESIAN_POINT('Ctrl Pts',(-16.1740447460464,-18.9368640244712,
13.3660136047297));
#155112=CARTESIAN_POINT('Ctrl Pts',(-16.173549435899,-19.0206360820962,
13.3701922828137));
#155113=CARTESIAN_POINT('Ctrl Pts',(-16.1771697541693,-19.1045569574875,
13.3743709608976));
#155114=CARTESIAN_POINT('Ctrl Pts',(-16.1849189310737,-19.1881899744725,
13.3785496389816));
#155115=CARTESIAN_POINT('Ctrl Pts',(-16.1928070064048,-19.2733220531809,
13.382803216867));
#155116=CARTESIAN_POINT('Ctrl Pts',(-16.2049734659499,-19.3581553727241,
13.3870567947524));
#155117=CARTESIAN_POINT('Ctrl Pts',(-16.2213767120001,-19.4422287349806,
13.3913103726379));
#155118=CARTESIAN_POINT('Ctrl Pts',(-16.2374619491174,-19.5246721710542,
13.3954814866158));
#155119=CARTESIAN_POINT('Ctrl Pts',(-16.2576210698179,-19.6063843810837,
13.3996526005938));
#155120=CARTESIAN_POINT('Ctrl Pts',(-16.2817626998464,-19.686936884185,
13.4038237145717));
#155121=CARTESIAN_POINT('Ctrl Pts',(-16.3058962289179,-19.767462357116,
13.4079934288921));
#155122=CARTESIAN_POINT('Ctrl Pts',(-16.334009481308,-19.8468284556772,
13.4121631432125));
#155123=CARTESIAN_POINT('Ctrl Pts',(-16.3659607754928,-19.9246202913754,
13.4163328575329));
#155124=CARTESIAN_POINT('Ctrl Pts',(-16.3979109327134,-20.0024093589062,
13.4205024234769));
#155125=CARTESIAN_POINT('Ctrl Pts',(-16.4336986846161,-20.0786238497405,
13.4246719894209));
#155126=CARTESIAN_POINT('Ctrl Pts',(-16.4731341172713,-20.1528686274167,
13.428841555365));
#155127=CARTESIAN_POINT('Ctrl Pts',(-16.5139560510899,-20.2297237598851,
13.4331577181039));
#155128=CARTESIAN_POINT('Ctrl Pts',(-16.5586866956795,-20.3044676260571,
13.4374738808428));
#155129=CARTESIAN_POINT('Ctrl Pts',(-16.6070644247003,-20.3766912151497,
13.4417900435817));
#155130=CARTESIAN_POINT('Ctrl Pts',(-16.6538662542868,-20.4465621284242,
13.4459656077734));
#155131=CARTESIAN_POINT('Ctrl Pts',(-16.7040808906406,-20.5140740893659,
13.4501411719651));
#155132=CARTESIAN_POINT('Ctrl Pts',(-16.75742932982,-20.5788891744013,13.4543167361568));
#155133=CARTESIAN_POINT('Ctrl Pts',(-16.8134722718384,-20.6469779152985,
13.4587031981693));
#155134=CARTESIAN_POINT('Ctrl Pts',(-16.8729735193545,-20.7120897510531,
13.4630896601819));
#155135=CARTESIAN_POINT('Ctrl Pts',(-16.9355661330672,-20.7738769514621,
13.4674761221944));
#155136=CARTESIAN_POINT('Ctrl Pts',(-16.9981587467798,-20.8356641518712,
13.4718625842069));
#155137=CARTESIAN_POINT('Ctrl Pts',(-17.0638422427094,-20.8941263879947,
13.4762490462195));
#155138=CARTESIAN_POINT('Ctrl Pts',(-17.1322119090441,-20.9489664272771,
13.480635508232));
#155139=CARTESIAN_POINT('Ctrl Pts',(-17.1461740071802,-20.9601655752516,
13.4815312887202));
#155140=CARTESIAN_POINT('Ctrl Pts',(-17.160259106387,-20.9712227363748,
13.4824270692085));
#155141=CARTESIAN_POINT('Ctrl Pts',(-17.1744641402401,-20.9821349467765,
13.4833228496967));
#155142=CARTESIAN_POINT('Origin',(-18.734,-18.952,-1.76670989022851));
#155143=CARTESIAN_POINT('',(-17.1732300411181,-20.9837128798172,14.34978651614));
#155144=CARTESIAN_POINT('',(-17.1756294737623,-20.9805869941177,14.2834124255784));
#155145=CARTESIAN_POINT('',(-17.1744641402401,-20.9821349467765,-1.76670989022851));
#155146=CARTESIAN_POINT('',(-21.2939989424941,-18.949673107456,13.8332901097715));
#155147=CARTESIAN_POINT('Ctrl Pts',(-21.294449633852,-18.9496726978033,
13.8332901097715));
#155148=CARTESIAN_POINT('Ctrl Pts',(-21.2961551522482,-18.7657813487039,
13.8424428639771));
#155149=CARTESIAN_POINT('Ctrl Pts',(-21.1940976782198,-17.7320561538789,
13.8939875537431));
#155150=CARTESIAN_POINT('Ctrl Pts',(-19.7898862958127,-16.1150306505046,
13.9879241790696));
#155151=CARTESIAN_POINT('Ctrl Pts',(-16.9200889626634,-16.5285690213481,
14.1150999857511));
#155152=CARTESIAN_POINT('Ctrl Pts',(-15.7765851098014,-19.0295417863752,
14.2357207647745));
#155153=CARTESIAN_POINT('Ctrl Pts',(-16.6072658624459,-20.5404052968016,
14.3139496082375));
#155154=CARTESIAN_POINT('Ctrl Pts',(-17.1732300411181,-20.9837128798172,
14.34978651614));
#155155=CARTESIAN_POINT('Ctrl Pts',(-17.1744641402401,-20.9821349467765,
13.549865697334));
#155156=CARTESIAN_POINT('Ctrl Pts',(-17.2411542319938,-21.0333658217219,
13.5540358010398));
#155157=CARTESIAN_POINT('Ctrl Pts',(-17.3103575700477,-21.0812964944487,
13.5582059047456));
#155158=CARTESIAN_POINT('Ctrl Pts',(-17.3817085509902,-21.1256853123061,
13.5623760084514));
#155159=CARTESIAN_POINT('Ctrl Pts',(-17.4531373470503,-21.1701225404449,
13.5665506600569));
#155160=CARTESIAN_POINT('Ctrl Pts',(-17.5267180697703,-21.211009960323,
13.5707253116625));
#155161=CARTESIAN_POINT('Ctrl Pts',(-17.6020587050214,-21.2481508889274,
13.5748999632681));
#155162=CARTESIAN_POINT('Ctrl Pts',(-17.6774451458419,-21.2853143984588,
13.5790771529766));
#155163=CARTESIAN_POINT('Ctrl Pts',(-17.7545932070973,-21.3187266999457,
13.5832543426852));
#155164=CARTESIAN_POINT('Ctrl Pts',(-17.8330912166259,-21.3482394212681,
13.5874315323938));
#155165=CARTESIAN_POINT('Ctrl Pts',(-17.9117197868307,-21.3778012291964,
13.5916156697526));
#155166=CARTESIAN_POINT('Ctrl Pts',(-17.9917023498214,-21.4034503690721,
13.5957998071114));
#155167=CARTESIAN_POINT('Ctrl Pts',(-18.0726128098124,-21.4250885517215,
13.5999839444702));
#155168=CARTESIAN_POINT('Ctrl Pts',(-18.1139485923167,-21.4361431324504,
13.6021215493219));
#155169=CARTESIAN_POINT('Ctrl Pts',(-18.1555264006885,-21.4461516743427,
13.6042591541736));
#155170=CARTESIAN_POINT('Ctrl Pts',(-18.1972887614197,-21.4551062794819,
13.6063967590253));
#155171=CARTESIAN_POINT('Ctrl Pts',(-18.2790439141132,-21.4726360622251,
13.6105813934184));
#155172=CARTESIAN_POINT('Ctrl Pts',(-18.3618109357872,-21.4861888889159,
13.6147660278114));
#155173=CARTESIAN_POINT('Ctrl Pts',(-18.4451682027607,-21.4956541024486,
13.6189506622045));
#155174=CARTESIAN_POINT('Ctrl Pts',(-18.5284068209824,-21.5051058434214,
13.6231293402884));
#155175=CARTESIAN_POINT('Ctrl Pts',(-18.6122335625332,-21.5104814765754,
13.6273080183723));
#155176=CARTESIAN_POINT('Ctrl Pts',(-18.6962156707041,-21.5117211458398,
13.6314866964563));
#155177=CARTESIAN_POINT('Ctrl Pts',(-18.781703097807,-21.5129830352849,
13.6357402743417));
#155178=CARTESIAN_POINT('Ctrl Pts',(-18.8673510447846,-21.5099591270341,
13.6399938522272));
#155179=CARTESIAN_POINT('Ctrl Pts',(-18.9526965098739,-21.5026414559026,
13.6442474301126));
#155180=CARTESIAN_POINT('Ctrl Pts',(-19.0363873865845,-21.4954656521053,
13.6484185440906));
#155181=CARTESIAN_POINT('Ctrl Pts',(-19.1197869256883,-21.4841611267896,
13.6525896580685));
#155182=CARTESIAN_POINT('Ctrl Pts',(-19.2024593315003,-21.4687729048785,
13.6567607720465));
#155183=CARTESIAN_POINT('Ctrl Pts',(-19.285103995788,-21.4533898466338,
13.6609304863668));
#155184=CARTESIAN_POINT('Ctrl Pts',(-19.3670215594764,-21.4339258973909,
13.6651002006872));
#155185=CARTESIAN_POINT('Ctrl Pts',(-19.4477843610412,-21.4104775544904,
13.6692699150076));
#155186=CARTESIAN_POINT('Ctrl Pts',(-19.5285442887191,-21.3870300459825,
13.6734394809516));
#155187=CARTESIAN_POINT('Ctrl Pts',(-19.6081490944219,-21.3595985548015,
13.6776090468957));
#155188=CARTESIAN_POINT('Ctrl Pts',(-19.6861855970018,-21.3283296465058,
13.6817786128397));
#155189=CARTESIAN_POINT('Ctrl Pts',(-19.7669657667439,-21.2959613619688,
13.6860947755787));
#155190=CARTESIAN_POINT('Ctrl Pts',(-19.846064808783,-21.2594809885573,
13.6904109383176));
#155191=CARTESIAN_POINT('Ctrl Pts',(-19.9230480777106,-21.2191049091061,
13.6947271010565));
#155192=CARTESIAN_POINT('Ctrl Pts',(-19.9975236247501,-21.1800440761961,
13.6989026652482));
#155193=CARTESIAN_POINT('Ctrl Pts',(-20.070018742585,-21.1373377246258,
13.7030782294399));
#155194=CARTESIAN_POINT('Ctrl Pts',(-20.1401676067986,-21.0912271178139,
13.7072537936316));
#155195=CARTESIAN_POINT('Ctrl Pts',(-20.2138595233805,-21.0427875738695,
13.7116402556441));
#155196=CARTESIAN_POINT('Ctrl Pts',(-20.2849614681667,-20.990591184541,
13.7160267176566));
#155197=CARTESIAN_POINT('Ctrl Pts',(-20.3530884618269,-20.9349655954602,
13.7204131796692));
#155198=CARTESIAN_POINT('Ctrl Pts',(-20.4212154554872,-20.8793400063795,
13.7247996416817));
#155199=CARTESIAN_POINT('Ctrl Pts',(-20.4863671192075,-20.8202856635707,
13.7291861036943));
#155200=CARTESIAN_POINT('Ctrl Pts',(-20.548204641978,-20.7581731691688,
13.7335725657068));
#155201=CARTESIAN_POINT('Ctrl Pts',(-20.6067777194386,-20.6993396360183,
13.7377274633762));
#155202=CARTESIAN_POINT('Ctrl Pts',(-20.6626103382647,-20.6375286216454,
13.7418823610455));
#155203=CARTESIAN_POINT('Ctrl Pts',(-20.7153787245626,-20.5730300274365,
13.7460372587149));
#155204=CARTESIAN_POINT('Ctrl Pts',(-20.7677053791601,-20.5090713601742,
13.7501573751423));
#155205=CARTESIAN_POINT('Ctrl Pts',(-20.8170185699061,-20.4424702805591,
13.7542774915697));
#155206=CARTESIAN_POINT('Ctrl Pts',(-20.8630375889924,-20.3735480803185,
13.7583976079971));
#155207=CARTESIAN_POINT('Ctrl Pts',(-20.909012526032,-20.3046919012951,
13.7625137777266));
#155208=CARTESIAN_POINT('Ctrl Pts',(-20.9516992900879,-20.233519404422,
13.7666299474561));
#155209=CARTESIAN_POINT('Ctrl Pts',(-20.9908578231796,-20.1603843618457,
13.7707461171856));
#155210=CARTESIAN_POINT('Ctrl Pts',(-21.0299913601116,-20.0872960037352,
13.7748596594307));
#155211=CARTESIAN_POINT('Ctrl Pts',(-21.0656009133713,-20.0122480031423,
13.7789732016758));
#155212=CARTESIAN_POINT('Ctrl Pts',(-21.0974909394085,-19.9356211564083,
13.7830867439209));
#155213=CARTESIAN_POINT('Ctrl Pts',(-21.1299241917561,-19.8576890200775,
13.7872703577418));
#155214=CARTESIAN_POINT('Ctrl Pts',(-21.158509766141,-19.7781241832438,
13.7914539715627));
#155215=CARTESIAN_POINT('Ctrl Pts',(-21.1830923574769,-19.6973500013741,
13.7956375853835));
#155216=CARTESIAN_POINT('Ctrl Pts',(-21.2072638620763,-19.6179265800633,
13.7997512379815));
#155217=CARTESIAN_POINT('Ctrl Pts',(-21.227565151866,-19.5373344318,13.8038648905795));
#155218=CARTESIAN_POINT('Ctrl Pts',(-21.2438990336339,-19.4559909135726,
13.8079785431775));
#155219=CARTESIAN_POINT('Ctrl Pts',(-21.260649602877,-19.372572271641,13.8121971376098));
#155220=CARTESIAN_POINT('Ctrl Pts',(-21.2732274574716,-19.2883639128976,
13.8164157320421));
#155221=CARTESIAN_POINT('Ctrl Pts',(-21.2815840465261,-19.2038243949373,
13.8206343264745));
#155222=CARTESIAN_POINT('Ctrl Pts',(-21.2899406355806,-19.119284876977,
13.8248529209068));
#155223=CARTESIAN_POINT('Ctrl Pts',(-21.2940759677847,-19.0344147354448,
13.8290715153392));
#155224=CARTESIAN_POINT('Ctrl Pts',(-21.2939989424941,-18.949673107456,
13.8332901097715));
#155225=CARTESIAN_POINT('',(-21.2939989173812,-18.9543543592142,13.7667098774877));
#155226=CARTESIAN_POINT('Ctrl Pts',(-17.1744641402401,-20.9821349467765,
13.4833228496967));
#155227=CARTESIAN_POINT('Ctrl Pts',(-17.2408008210132,-21.0330943338099,
13.4875060924052));
#155228=CARTESIAN_POINT('Ctrl Pts',(-17.3097559456157,-21.0808895947018,
13.4916893351137));
#155229=CARTESIAN_POINT('Ctrl Pts',(-17.3809948073905,-21.1252411161148,
13.4958725778222));
#155230=CARTESIAN_POINT('Ctrl Pts',(-17.4521373200177,-21.1695326529747,
13.5000501627779));
#155231=CARTESIAN_POINT('Ctrl Pts',(-17.5255570468011,-21.2103894610906,
13.5042277477337));
#155232=CARTESIAN_POINT('Ctrl Pts',(-17.6008876366303,-21.2475732120711,
13.5084053326894));
#155233=CARTESIAN_POINT('Ctrl Pts',(-17.6761382792445,-21.2847175004996,
13.5125784840374));
#155234=CARTESIAN_POINT('Ctrl Pts',(-17.7532953436455,-21.3181962768837,
13.5167516353855));
#155235=CARTESIAN_POINT('Ctrl Pts',(-17.8319662179374,-21.3478161565566,
13.5209247867335));
#155236=CARTESIAN_POINT('Ctrl Pts',(-17.9105916919263,-21.377418942845,
13.5250955297908));
#155237=CARTESIAN_POINT('Ctrl Pts',(-17.9907288118313,-21.4031670920381,
13.5292662728482));
#155238=CARTESIAN_POINT('Ctrl Pts',(-18.0719642714498,-21.4249150195919,
13.5334370159055));
#155239=CARTESIAN_POINT('Ctrl Pts',(-18.1531772197455,-21.4466569205333,
13.5376066031998));
#155240=CARTESIAN_POINT('Ctrl Pts',(-18.2354874590825,-21.4644006827327,
13.541776190494));
#155241=CARTESIAN_POINT('Ctrl Pts',(-18.3184670930211,-21.4780507523044,
13.5459457777883));
#155242=CARTESIAN_POINT('Ctrl Pts',(-18.4014486240669,-21.4917011339484,
13.550115460409));
#155243=CARTESIAN_POINT('Ctrl Pts',(-18.4850991259487,-21.5012575637275,
13.5542851430298));
#155244=CARTESIAN_POINT('Ctrl Pts',(-18.5689824521641,-21.5066759498821,
13.5584548256505));
#155245=CARTESIAN_POINT('Ctrl Pts',(-18.6529508563463,-21.5120998315899,
13.5626287373372));
#155246=CARTESIAN_POINT('Ctrl Pts',(-18.7371520964114,-21.5133772565597,
13.5668026490239));
#155247=CARTESIAN_POINT('Ctrl Pts',(-18.8211473385815,-21.5105162382479,
13.5709765607106));
#155248=CARTESIAN_POINT('Ctrl Pts',(-18.9051840123408,-21.5076538087069,
13.5751525312257));
#155249=CARTESIAN_POINT('Ctrl Pts',(-18.9890140268519,-21.500648907998,
13.5793285017409));
#155250=CARTESIAN_POINT('Ctrl Pts',(-19.0722034479546,-21.4895615121198,
13.583504472256));
#155251=CARTESIAN_POINT('Ctrl Pts',(-19.1555422636085,-21.4784542050977,
13.587687942129));
#155252=CARTESIAN_POINT('Ctrl Pts',(-19.238237733707,-21.4632498369034,
13.5918714120021));
#155253=CARTESIAN_POINT('Ctrl Pts',(-19.3198659781615,-21.4440596011398,
13.5960548818751));
#155254=CARTESIAN_POINT('Ctrl Pts',(-19.3963301748768,-21.4260833972872,
13.5999736928879));
#155255=CARTESIAN_POINT('Ctrl Pts',(-19.4718577384313,-21.4046102735867,
13.6038925039007));
#155256=CARTESIAN_POINT('Ctrl Pts',(-19.546115225231,-21.379770347654,13.6078113149135));
#155257=CARTESIAN_POINT('Ctrl Pts',(-19.6254097949839,-21.353245463438,
13.6119959493065));
#155258=CARTESIAN_POINT('Ctrl Pts',(-19.7035510491553,-21.3227823154618,
13.6161805836996));
#155259=CARTESIAN_POINT('Ctrl Pts',(-19.7801197445754,-21.2885002632162,
13.6203652180926));
#155260=CARTESIAN_POINT('Ctrl Pts',(-19.8565794539351,-21.2542670072287,
13.6245438961766));
#155261=CARTESIAN_POINT('Ctrl Pts',(-19.9314706343179,-21.2162258304372,
13.6287225742605));
#155262=CARTESIAN_POINT('Ctrl Pts',(-20.0043903176931,-21.1745454867587,
13.6329012523444));
#155263=CARTESIAN_POINT('Ctrl Pts',(-20.0786170339864,-21.1321180528749,
13.6371548302299));
#155264=CARTESIAN_POINT('Ctrl Pts',(-20.1508004226817,-21.0859198576824,
13.6414084081153));
#155265=CARTESIAN_POINT('Ctrl Pts',(-20.2205378947047,-21.0361797157652,
13.6456619860008));
#155266=CARTESIAN_POINT('Ctrl Pts',(-20.288923369751,-20.9874038835589,
13.6498330999787));
#155267=CARTESIAN_POINT('Ctrl Pts',(-20.3549565277687,-20.9352224936049,
13.6540042139567));
#155268=CARTESIAN_POINT('Ctrl Pts',(-20.4182851699542,-20.879896124347,
13.6581753279346));
#155269=CARTESIAN_POINT('Ctrl Pts',(-20.4815925616022,-20.8245883203867,
13.662345042255));
#155270=CARTESIAN_POINT('Ctrl Pts',(-20.5421968936247,-20.7661379354359,
13.6665147565753));
#155271=CARTESIAN_POINT('Ctrl Pts',(-20.5997791685762,-20.7048457131497,
13.6706844708957));
#155272=CARTESIAN_POINT('Ctrl Pts',(-20.6573593945033,-20.6435556719038,
13.6748540368398));
#155273=CARTESIAN_POINT('Ctrl Pts',(-20.7119174628063,-20.5794243302492,
13.6790236027838));
#155274=CARTESIAN_POINT('Ctrl Pts',(-20.763172325239,-20.512788158106,13.6831931687278));
#155275=CARTESIAN_POINT('Ctrl Pts',(-20.8162292454053,-20.4438091403549,
13.6875093314668));
#155276=CARTESIAN_POINT('Ctrl Pts',(-20.8657460348867,-20.3721462932499,
13.6918254942057));
#155277=CARTESIAN_POINT('Ctrl Pts',(-20.9114587072171,-20.2982071082729,
13.6961416569446));
#155278=CARTESIAN_POINT('Ctrl Pts',(-20.9556822940544,-20.2266764844696,
13.7003172211363));
#155279=CARTESIAN_POINT('Ctrl Pts',(-20.9963456096573,-20.1530159839384,
13.704492785328));
#155280=CARTESIAN_POINT('Ctrl Pts',(-21.0332565704859,-20.0776194841408,
13.7086683495196));
#155281=CARTESIAN_POINT('Ctrl Pts',(-21.0720318161985,-19.9984148863766,
13.7130548115322));
#155282=CARTESIAN_POINT('Ctrl Pts',(-21.1066654530388,-19.9172948468639,
13.7174412735447));
#155283=CARTESIAN_POINT('Ctrl Pts',(-21.1369928787006,-19.8347373476376,
13.7218277355573));
#155284=CARTESIAN_POINT('Ctrl Pts',(-21.1673203043624,-19.7521798484113,
13.7262141975698));
#155285=CARTESIAN_POINT('Ctrl Pts',(-21.1933414198056,-19.668185466211,
13.7306006595824));
#155286=CARTESIAN_POINT('Ctrl Pts',(-21.214953227824,-19.5832456584798,
13.7349871215949));
#155287=CARTESIAN_POINT('Ctrl Pts',(-21.2416966549182,-19.4781373050501,
13.740415127754));
#155288=CARTESIAN_POINT('Ctrl Pts',(-21.261771847948,-19.3712684537292,
13.7458431339132));
#155289=CARTESIAN_POINT('Ctrl Pts',(-21.2749934581328,-19.2633715557439,
13.7512711400723));
#155290=CARTESIAN_POINT('Ctrl Pts',(-21.2875287526693,-19.1610754377283,
13.7564173858775));
#155291=CARTESIAN_POINT('Ctrl Pts',(-21.2939037306885,-19.05785506064,13.7615636316826));
#155292=CARTESIAN_POINT('Ctrl Pts',(-21.2939989173812,-18.9543543592142,
13.7667098774877));
#155293=CARTESIAN_POINT('Ctrl Pts',(-21.2935815865034,-18.9543537192076,
13.7667098902285));
#155294=CARTESIAN_POINT('Ctrl Pts',(-21.2877697346816,-18.3145386563719,
13.7985275695778));
#155295=CARTESIAN_POINT('Ctrl Pts',(-20.7208249375185,-16.8130884735802,
13.8727371844876));
#155296=CARTESIAN_POINT('Ctrl Pts',(-18.1988330759633,-15.9725894556499,
13.9893387349578));
#155297=CARTESIAN_POINT('Ctrl Pts',(-15.939111528405,-17.7892922724466,
14.1165145416392));
#155298=CARTESIAN_POINT('Ctrl Pts',(-16.1737486300813,-20.0117707719198,
14.2145391051794));
#155299=CARTESIAN_POINT('Ctrl Pts',(-16.9627571743812,-20.8199785653492,
14.2701717331591));
#155300=CARTESIAN_POINT('Ctrl Pts',(-17.1756294737626,-20.9805869941179,
14.2834124255784));
#155301=CARTESIAN_POINT('Origin',(-18.734,-18.952,-1.76670989022851));
#155302=CARTESIAN_POINT('',(-17.1744641402401,-20.9821349467764,15.1499553790579));
#155303=CARTESIAN_POINT('',(-17.1744641402401,-20.9821349467765,15.0832685784559));
#155304=CARTESIAN_POINT('',(-17.1744641402401,-20.9821349467765,-1.76670989022851));
#155305=CARTESIAN_POINT('',(-21.2941233742573,-18.953130183291,14.6332901097715));
#155306=CARTESIAN_POINT('Ctrl Pts',(-21.2939997505486,-18.9531301287165,
14.6332901097715));
#155307=CARTESIAN_POINT('Ctrl Pts',(-21.2940362985033,-18.8703406609988,
14.6374299052976));
#155308=CARTESIAN_POINT('Ctrl Pts',(-21.2900525381051,-18.7873874928942,
14.6415697008237));
#155309=CARTESIAN_POINT('Ctrl Pts',(-21.2820270867845,-18.7046986352398,
14.6457094963498));
#155310=CARTESIAN_POINT('Ctrl Pts',(-21.2740124509524,-18.6221212131097,
14.6498437128863));
#155311=CARTESIAN_POINT('Ctrl Pts',(-21.2619669829652,-18.5398078587026,
14.6539779294227));
#155312=CARTESIAN_POINT('Ctrl Pts',(-21.2459213201025,-18.4581869973214,
14.6581121459591));
#155313=CARTESIAN_POINT('Ctrl Pts',(-21.2298921267196,-18.3766499126674,
14.6622421190812));
#155314=CARTESIAN_POINT('Ctrl Pts',(-21.2098709847548,-18.2958043686398,
14.6663720922033));
#155315=CARTESIAN_POINT('Ctrl Pts',(-21.1859402178852,-18.2160725797221,
14.6705020653254));
#155316=CARTESIAN_POINT('Ctrl Pts',(-21.1620224032905,-18.1363839447932,
14.6746298031432));
#155317=CARTESIAN_POINT('Ctrl Pts',(-21.1341992976673,-18.0578083185522,
14.6787575409609));
#155318=CARTESIAN_POINT('Ctrl Pts',(-21.1026037847562,-17.9807553805356,
14.6828852787787));
#155319=CARTESIAN_POINT('Ctrl Pts',(-21.0710154147149,-17.9037198620526,
14.6870120834293));
#155320=CARTESIAN_POINT('Ctrl Pts',(-21.0356565094079,-17.8282067834225,
14.69113888808));
#155321=CARTESIAN_POINT('Ctrl Pts',(-20.9967085276618,-17.7546069488901,
14.6952656927306));
#155322=CARTESIAN_POINT('Ctrl Pts',(-20.9577570758465,-17.6810005569824,
14.6993928650588));
#155323=CARTESIAN_POINT('Ctrl Pts',(-20.9152161348637,-17.6093081624228,
14.703520037387));
#155324=CARTESIAN_POINT('Ctrl Pts',(-20.8693129406038,-17.5398956675621,
14.7076472097152));
#155325=CARTESIAN_POINT('Ctrl Pts',(-20.8233622278895,-17.4704113176916,
14.7117786544444));
#155326=CARTESIAN_POINT('Ctrl Pts',(-20.7740425759674,-17.4032119705945,
14.7159100991735));
#155327=CARTESIAN_POINT('Ctrl Pts',(-20.7216239583869,-17.3386336435743,
14.7200415439027));
#155328=CARTESIAN_POINT('Ctrl Pts',(-20.6691749218115,-17.2740178411706,
14.7241753861463));
#155329=CARTESIAN_POINT('Ctrl Pts',(-20.6136236562292,-17.2120264344647,
14.7283092283899));
#155330=CARTESIAN_POINT('Ctrl Pts',(-20.5552780488236,-17.1529596255578,
14.7324430706336));
#155331=CARTESIAN_POINT('Ctrl Pts',(-20.4968364594113,-17.0937956482246,
14.7365837132944));
#155332=CARTESIAN_POINT('Ctrl Pts',(-20.4355917013472,-17.0375661867587,
14.7407243559553));
#155333=CARTESIAN_POINT('Ctrl Pts',(-20.3718854170603,-16.9845317383548,
14.7448649986162));
#155334=CARTESIAN_POINT('Ctrl Pts',(-20.3405294527256,-16.9584284066148,
14.7469030054636));
#155335=CARTESIAN_POINT('Ctrl Pts',(-20.3085776248464,-16.9330984310457,
14.7489410123109));
#155336=CARTESIAN_POINT('Ctrl Pts',(-20.2760730898183,-16.9085689182999,
14.7509790191583));
#155337=CARTESIAN_POINT('Ctrl Pts',(-20.2093316088542,-16.8582025307612,
14.7551636535514));
#155338=CARTESIAN_POINT('Ctrl Pts',(-20.1399957688999,-16.811015665153,
14.7593482879444));
#155339=CARTESIAN_POINT('Ctrl Pts',(-20.0684012262925,-16.767286433587,
14.7635329223375));
#155340=CARTESIAN_POINT('Ctrl Pts',(-19.9969085896549,-16.7236194451695,
14.7677116004214));
#155341=CARTESIAN_POINT('Ctrl Pts',(-19.9231640255692,-16.6834005528598,
14.7718902785053));
#155342=CARTESIAN_POINT('Ctrl Pts',(-19.8475347050067,-16.6468664982814,
14.7760689565893));
#155343=CARTESIAN_POINT('Ctrl Pts',(-19.7705497832269,-16.6096775970311,
14.7803225344747));
#155344=CARTESIAN_POINT('Ctrl Pts',(-19.6916122567006,-16.5763072247155,
14.7845761123601));
#155345=CARTESIAN_POINT('Ctrl Pts',(-19.6111386006651,-16.5469578225688,
14.7888296902456));
#155346=CARTESIAN_POINT('Ctrl Pts',(-19.5322250834833,-16.5181774158532,
14.7930008042235));
#155347=CARTESIAN_POINT('Ctrl Pts',(-19.4518349191003,-16.4932636267838,
14.7971719182015));
#155348=CARTESIAN_POINT('Ctrl Pts',(-19.3703822558338,-16.4723593759458,
14.8013430321794));
#155349=CARTESIAN_POINT('Ctrl Pts',(-19.288956924795,-16.4514621397311,
14.8055127464998));
#155350=CARTESIAN_POINT('Ctrl Pts',(-19.2064702481718,-16.4345718839471,
14.8096824608202));
#155351=CARTESIAN_POINT('Ctrl Pts',(-19.1233507011893,-16.4217814261445,
14.8138521751405));
#155352=CARTESIAN_POINT('Ctrl Pts',(-19.040234111957,-16.4089914234813,
14.8180217410846));
#155353=CARTESIAN_POINT('Ctrl Pts',(-18.9564851519522,-16.4003009978601,
14.8221913070286));
#155354=CARTESIAN_POINT('Ctrl Pts',(-18.8725402767199,-16.3957514612764,
14.8263608729727));
#155355=CARTESIAN_POINT('Ctrl Pts',(-18.7856440032318,-16.3910419685989,
14.8306770357116));
#155356=CARTESIAN_POINT('Ctrl Pts',(-18.6985383080788,-16.3907699986349,
14.8349931984505));
#155357=CARTESIAN_POINT('Ctrl Pts',(-18.6117085473889,-16.3949226056652,
14.8393093611894));
#155358=CARTESIAN_POINT('Ctrl Pts',(-18.5277072570205,-16.3989399419582,
14.8434849253811));
#155359=CARTESIAN_POINT('Ctrl Pts',(-18.4439646643006,-16.4070979281598,
14.8476604895728));
#155360=CARTESIAN_POINT('Ctrl Pts',(-18.3609142114861,-16.4193320402372,
14.8518360537644));
#155361=CARTESIAN_POINT('Ctrl Pts',(-18.2736690777338,-16.4321840682319,
14.856222515777));
#155362=CARTESIAN_POINT('Ctrl Pts',(-18.1871884138653,-16.4495346990029,
14.8606089777895));
#155363=CARTESIAN_POINT('Ctrl Pts',(-18.1019594530764,-16.471249156597,
14.864995439802));
#155364=CARTESIAN_POINT('Ctrl Pts',(-18.0167304922876,-16.4929636141912,
14.8693819018146));
#155365=CARTESIAN_POINT('Ctrl Pts',(-17.932753766134,-16.5190416538915,
14.8737683638271));
#155366=CARTESIAN_POINT('Ctrl Pts',(-17.8504927560606,-16.549290082031,
14.8781548258397));
#155367=CARTESIAN_POINT('Ctrl Pts',(-17.7720166970007,-16.5781467351529,
14.8823394602327));
#155368=CARTESIAN_POINT('Ctrl Pts',(-17.6948098353985,-16.6109058485358,
14.8865240946257));
#155369=CARTESIAN_POINT('Ctrl Pts',(-17.6192877039368,-16.6474357251303,
14.8907087290188));
#155370=CARTESIAN_POINT('Ctrl Pts',(-17.5438730688816,-16.683913605967,
14.8948874071027));
#155371=CARTESIAN_POINT('Ctrl Pts',(-17.4701388113635,-16.7241513904372,
14.8990660851867));
#155372=CARTESIAN_POINT('Ctrl Pts',(-17.3984827363055,-16.7679684896106,
14.9032447632706));
#155373=CARTESIAN_POINT('Ctrl Pts',(-17.3255422776003,-16.8125709787959,
14.9074983411561));
#155374=CARTESIAN_POINT('Ctrl Pts',(-17.2547556895186,-16.8608821968549,
14.9117519190415));
#155375=CARTESIAN_POINT('Ctrl Pts',(-17.1865186232482,-16.912661531622,
14.9160054969269));
#155376=CARTESIAN_POINT('Ctrl Pts',(-17.1196044656613,-16.9634370229455,
14.9201766109049));
#155377=CARTESIAN_POINT('Ctrl Pts',(-17.0551422404859,-17.0175470676763,
14.9243477248828));
#155378=CARTESIAN_POINT('Ctrl Pts',(-16.9934762919463,-17.0747207928219,
14.9285188388608));
#155379=CARTESIAN_POINT('Ctrl Pts',(-16.9318310360114,-17.1318753327718,
14.9326885531811));
#155380=CARTESIAN_POINT('Ctrl Pts',(-16.8729805302655,-17.1920911989054,
14.9368582675015));
#155381=CARTESIAN_POINT('Ctrl Pts',(-16.8172347450926,-17.2550583517457,
14.9410279818219));
#155382=CARTESIAN_POINT('Ctrl Pts',(-16.7614909435939,-17.3180232639448,
14.9451975477659));
#155383=CARTESIAN_POINT('Ctrl Pts',(-16.70885194731,-17.383738923187,14.94936711371));
#155384=CARTESIAN_POINT('Ctrl Pts',(-16.6595887382,-17.451860700829,14.953536679654));
#155385=CARTESIAN_POINT('Ctrl Pts',(-16.6085934954305,-17.5223775561355,
14.957852842393));
#155386=CARTESIAN_POINT('Ctrl Pts',(-16.5612161510347,-17.5954724488009,
14.9621690051319));
#155387=CARTESIAN_POINT('Ctrl Pts',(-16.517708533778,-17.6707302638587,
14.9664851678708));
#155388=CARTESIAN_POINT('Ctrl Pts',(-16.4756181725772,-17.7435365635068,
14.9706607320625));
#155389=CARTESIAN_POINT('Ctrl Pts',(-16.437149470808,-17.8183665946342,
14.9748362962542));
#155390=CARTESIAN_POINT('Ctrl Pts',(-16.4024827880428,-17.8948209752613,
14.9790118604458));
#155391=CARTESIAN_POINT('Ctrl Pts',(-16.3660651735434,-17.9751368849009,
14.9833983224584));
#155392=CARTESIAN_POINT('Ctrl Pts',(-16.3338439651084,-18.0572450047083,
14.9877847844709));
#155393=CARTESIAN_POINT('Ctrl Pts',(-16.3059695675778,-18.1406626970049,
14.9921712464835));
#155394=CARTESIAN_POINT('Ctrl Pts',(-16.2780951700471,-18.2240803893014,
14.996557708496));
#155395=CARTESIAN_POINT('Ctrl Pts',(-16.2545676653734,-18.3088070746724,
15.0009441705086));
#155396=CARTESIAN_POINT('Ctrl Pts',(-16.2354754819719,-18.3943484665023,
15.0053306325211));
#155397=CARTESIAN_POINT('Ctrl Pts',(-16.21726175823,-18.4759539720914,15.0095152669141));
#155398=CARTESIAN_POINT('Ctrl Pts',(-16.2030163785017,-18.5586046111966,
15.0136999013072));
#155399=CARTESIAN_POINT('Ctrl Pts',(-16.1928535263697,-18.6418797014763,
15.0178845357003));
#155400=CARTESIAN_POINT('Ctrl Pts',(-16.1827051397999,-18.7250362599721,
15.0220632137842));
#155401=CARTESIAN_POINT('Ctrl Pts',(-16.1766277936582,-18.8088150514092,
15.0262418918681));
#155402=CARTESIAN_POINT('Ctrl Pts',(-16.1746849654928,-18.8927838354387,
15.0304205699521));
#155403=CARTESIAN_POINT('Ctrl Pts',(-16.1727073135288,-18.9782576995748,
15.0346741478375));
#155404=CARTESIAN_POINT('Ctrl Pts',(-16.1750139649456,-19.0639279639716,
15.0389277257229));
#155405=CARTESIAN_POINT('Ctrl Pts',(-16.1816167614736,-19.1493317097918,
15.0431813036084));
#155406=CARTESIAN_POINT('Ctrl Pts',(-16.1880915499065,-19.2330797373476,
15.0473524175863));
#155407=CARTESIAN_POINT('Ctrl Pts',(-16.1986973545603,-19.3165710082865,
15.0515235315643));
#155408=CARTESIAN_POINT('Ctrl Pts',(-16.2133928011124,-19.3993693651963,
15.0556946455422));
#155409=CARTESIAN_POINT('Ctrl Pts',(-16.2280833164655,-19.4821399383178,
15.0598643598626));
#155410=CARTESIAN_POINT('Ctrl Pts',(-16.2468606679443,-19.5642176066097,
15.064034074183));
#155411=CARTESIAN_POINT('Ctrl Pts',(-16.2696319425036,-19.6451739155444,
15.0682037885034));
#155412=CARTESIAN_POINT('Ctrl Pts',(-16.2924024067631,-19.7261273437062,
15.0723733544474));
#155413=CARTESIAN_POINT('Ctrl Pts',(-16.3191663861463,-19.8059590492308,
15.0765429203914));
#155414=CARTESIAN_POINT('Ctrl Pts',(-16.3497807798976,-19.8842546382262,
15.0807124863355));
#155415=CARTESIAN_POINT('Ctrl Pts',(-16.3814715379662,-19.9653030035426,
15.0850286490744));
#155416=CARTESIAN_POINT('Ctrl Pts',(-16.4172883172412,-20.0447047315975,
15.0893448118133));
#155417=CARTESIAN_POINT('Ctrl Pts',(-16.4570183818636,-20.1220233803941,
15.0936609745523));
#155418=CARTESIAN_POINT('Ctrl Pts',(-16.4954542438098,-20.1968233823387,
15.0978365387439));
#155419=CARTESIAN_POINT('Ctrl Pts',(-16.5375520792277,-20.2696735493081,
15.1020121029356));
#155420=CARTESIAN_POINT('Ctrl Pts',(-16.583073696292,-20.3402060495535,
15.1061876671273));
#155421=CARTESIAN_POINT('Ctrl Pts',(-16.6308945020168,-20.4143009787112,
15.1105741291398));
#155422=CARTESIAN_POINT('Ctrl Pts',(-16.6824937078808,-20.4858374838362,
15.1149605911524));
#155423=CARTESIAN_POINT('Ctrl Pts',(-16.7375469032625,-20.5544278556389,
15.1193470531649));
#155424=CARTESIAN_POINT('Ctrl Pts',(-16.7926000986442,-20.6230182274415,
15.1237335151774));
#155425=CARTESIAN_POINT('Ctrl Pts',(-16.8511068407071,-20.6886620833861,
15.12811997719));
#155426=CARTESIAN_POINT('Ctrl Pts',(-16.9126993772538,-20.7510175211999,
15.1325064392025));
#155427=CARTESIAN_POINT('Ctrl Pts',(-16.9714542743191,-20.8105001717875,
15.1366908118307));
#155428=CARTESIAN_POINT('Ctrl Pts',(-17.0332355735422,-20.8672121310249,
15.1408751844589));
#155429=CARTESIAN_POINT('Ctrl Pts',(-17.0977514090968,-20.9208297409291,
15.1450595570871));
#155430=CARTESIAN_POINT('Ctrl Pts',(-17.1229131297205,-20.9417410615271,
15.146691497744));
#155431=CARTESIAN_POINT('Ctrl Pts',(-17.1484903532052,-20.9621820602163,
15.1483234384009));
#155432=CARTESIAN_POINT('Ctrl Pts',(-17.1744641402401,-20.9821349467764,
15.1499553790579));
#155433=CARTESIAN_POINT('Ctrl Pts',(-17.1732300411181,-20.9837128798172,
14.34978651614));
#155434=CARTESIAN_POINT('Ctrl Pts',(-17.2767521098951,-21.0647994924116,
14.356341543798));
#155435=CARTESIAN_POINT('Ctrl Pts',(-18.0960849332152,-21.6081172949695,
14.4052885070165));
#155436=CARTESIAN_POINT('Ctrl Pts',(-20.1784866529944,-21.6122160192327,
14.4966274057954));
#155437=CARTESIAN_POINT('Ctrl Pts',(-21.2671017221445,-19.9284206152422,
14.5845735760146));
#155438=CARTESIAN_POINT('Ctrl Pts',(-21.2979708163172,-19.0164624131716,
14.6301278106733));
#155439=CARTESIAN_POINT('Ctrl Pts',(-21.2976210374783,-18.9531317273574,
14.6332901097715));
#155440=CARTESIAN_POINT('',(-21.2936354977614,-18.9514398261094,14.566709915054));
#155441=CARTESIAN_POINT('Ctrl Pts',(-17.1756294737626,-20.9805869941179,
14.2834124255784));
#155442=CARTESIAN_POINT('Ctrl Pts',(-17.6442977246966,-21.3341889968917,
14.3125636687196));
#155443=CARTESIAN_POINT('Ctrl Pts',(-19.0929371519294,-21.824338083774,
14.3841068474214));
#155444=CARTESIAN_POINT('Ctrl Pts',(-20.9482575115022,-20.7321304478324,
14.478539335638));
#155445=CARTESIAN_POINT('Ctrl Pts',(-21.2889974874197,-19.4133916920799,
14.5438205807135));
#155446=CARTESIAN_POINT('Ctrl Pts',(-21.2898969963344,-18.9514411453738,
14.5667098902285));
#155447=CARTESIAN_POINT('Ctrl Pts',(-21.2939999386838,-18.9514396975034,
14.566709917474));
#155448=CARTESIAN_POINT('Ctrl Pts',(-21.2939802627005,-18.8615409084184,
14.571157199273));
#155449=CARTESIAN_POINT('Ctrl Pts',(-21.2892209204008,-18.7717655181781,
14.575604481072));
#155450=CARTESIAN_POINT('Ctrl Pts',(-21.2797861099468,-18.6826060832129,
14.5800517628709));
#155451=CARTESIAN_POINT('Ctrl Pts',(-21.2703167670437,-18.5931203148612,
14.5845153222128));
#155452=CARTESIAN_POINT('Ctrl Pts',(-21.2561377674616,-18.5042553694628,
14.5889788815547));
#155453=CARTESIAN_POINT('Ctrl Pts',(-21.2373647797459,-18.4164957707656,
14.5934424408966));
#155454=CARTESIAN_POINT('Ctrl Pts',(-21.2185553401018,-18.3285657673013,
14.5979146672311));
#155455=CARTESIAN_POINT('Ctrl Pts',(-21.1951342035189,-18.2417457397356,
14.6023868935656));
#155456=CARTESIAN_POINT('Ctrl Pts',(-21.1672666877164,-18.1565044145631,
14.6068591199));
#155457=CARTESIAN_POINT('Ctrl Pts',(-21.139316159677,-18.0710091710603,
14.6113446681795));
#155458=CARTESIAN_POINT('Ctrl Pts',(-21.1068928974786,-17.9871023685111,
14.6158302164589));
#155459=CARTESIAN_POINT('Ctrl Pts',(-21.0702104967804,-17.9052333045357,
14.6203157647383));
#155460=CARTESIAN_POINT('Ctrl Pts',(-21.0568477853901,-17.875409938211,
14.6219497659472));
#155461=CARTESIAN_POINT('Ctrl Pts',(-21.0429203172351,-17.8458567318452,
14.6235837671561));
#155462=CARTESIAN_POINT('Ctrl Pts',(-21.0284398795323,-17.8165945044999,
14.625217768365));
#155463=CARTESIAN_POINT('Ctrl Pts',(-20.9913558570061,-17.7416547050056,
14.629402402758));
#155464=CARTESIAN_POINT('Ctrl Pts',(-20.9505274948144,-17.6683941847451,
14.6335870371511));
#155465=CARTESIAN_POINT('Ctrl Pts',(-20.9061301751471,-17.5972120083883,
14.6377716715441));
#155466=CARTESIAN_POINT('Ctrl Pts',(-20.8617960495691,-17.526131151049,
14.641950349628));
#155467=CARTESIAN_POINT('Ctrl Pts',(-20.8139032983065,-17.4571231485616,
14.646129027712));
#155468=CARTESIAN_POINT('Ctrl Pts',(-20.7626740190629,-17.3905642106128,
14.6503077057959));
#155469=CARTESIAN_POINT('Ctrl Pts',(-20.7105264918066,-17.3228122515362,
14.6545612836814));
#155470=CARTESIAN_POINT('Ctrl Pts',(-20.6549218593555,-17.2575984516732,
14.6588148615668));
#155471=CARTESIAN_POINT('Ctrl Pts',(-20.5961416680529,-17.1952904599504,
14.6630684394522));
#155472=CARTESIAN_POINT('Ctrl Pts',(-20.5385010454588,-17.1341904302312,
14.6672395534302));
#155473=CARTESIAN_POINT('Ctrl Pts',(-20.4778072242623,-17.0758848946115,
14.6714106674082));
#155474=CARTESIAN_POINT('Ctrl Pts',(-20.4143663508876,-17.0206872529792,
14.6755817813861));
#155475=CARTESIAN_POINT('Ctrl Pts',(-20.3509467657105,-16.9655081334487,
14.6797514957065));
#155476=CARTESIAN_POINT('Ctrl Pts',(-20.2847823058332,-16.9134351384329,
14.6839212100269));
#155477=CARTESIAN_POINT('Ctrl Pts',(-20.2162143833074,-16.8647433023423,
14.6880909243472));
#155478=CARTESIAN_POINT('Ctrl Pts',(-20.1476489007225,-16.8160531989163,
14.6922604902913));
#155479=CARTESIAN_POINT('Ctrl Pts',(-20.0766805011101,-16.7707442808557,
14.6964300562353));
#155480=CARTESIAN_POINT('Ctrl Pts',(-20.0036808175632,-16.7290491185112,
14.7005996221793));
#155481=CARTESIAN_POINT('Ctrl Pts',(-19.9281145551976,-16.6858880056951,
14.7049157849183));
#155482=CARTESIAN_POINT('Ctrl Pts',(-19.8503719693232,-16.6465997576134,
14.7092319476572));
#155483=CARTESIAN_POINT('Ctrl Pts',(-19.7708927266888,-16.6113903628884,
14.7135481103961));
#155484=CARTESIAN_POINT('Ctrl Pts',(-19.6940025120236,-16.5773279104931,
14.7177236745878));
#155485=CARTESIAN_POINT('Ctrl Pts',(-19.6154875027975,-16.5470827802972,
14.7218992387795));
#155486=CARTESIAN_POINT('Ctrl Pts',(-19.5357640795054,-16.5207915842498,
14.7260748029711));
#155487=CARTESIAN_POINT('Ctrl Pts',(-19.4520140156272,-16.4931724823913,
14.7304612649837));
#155488=CARTESIAN_POINT('Ctrl Pts',(-19.3669308187545,-16.4699173921691,
14.7348477269962));
#155489=CARTESIAN_POINT('Ctrl Pts',(-19.2810104439707,-16.4511242385542,
14.7392341890088));
#155490=CARTESIAN_POINT('Ctrl Pts',(-19.1950900691869,-16.4323310849393,
14.7436206510213));
#155491=CARTESIAN_POINT('Ctrl Pts',(-19.1083331013483,-16.4179998874471,
14.7480071130339));
#155492=CARTESIAN_POINT('Ctrl Pts',(-19.021240449396,-16.4081657042506,
14.7523935750464));
#155493=CARTESIAN_POINT('Ctrl Pts',(-18.9381550594622,-16.3987840064008,
14.7565782094394));
#155494=CARTESIAN_POINT('Ctrl Pts',(-18.8544549375686,-16.3934596676543,
14.7607628438325));
#155495=CARTESIAN_POINT('Ctrl Pts',(-18.770570565002,-16.3922612254811,
14.7649474782255));
#155496=CARTESIAN_POINT('Ctrl Pts',(-18.6868055914571,-16.3910644891421,
14.7691261563095));
#155497=CARTESIAN_POINT('Ctrl Pts',(-18.6028573442178,-16.3939819908556,
14.7733048343934));
#155498=CARTESIAN_POINT('Ctrl Pts',(-18.5191623733687,-16.4010306167687,
14.7774835124774));
#155499=CARTESIAN_POINT('Ctrl Pts',(-18.4339672303176,-16.4082055842356,
14.7817370903628));
#155500=CARTESIAN_POINT('Ctrl Pts',(-18.3490350120199,-16.4196612875147,
14.7859906682482));
#155501=CARTESIAN_POINT('Ctrl Pts',(-18.2648272487369,-16.4353599920783,
14.7902442461337));
#155502=CARTESIAN_POINT('Ctrl Pts',(-18.182252017263,-16.4507543466204,
14.7944153601116));
#155503=CARTESIAN_POINT('Ctrl Pts',(-18.1003738745937,-16.4702285646622,
14.7985864740896));
#155504=CARTESIAN_POINT('Ctrl Pts',(-18.0196220516907,-16.493694862925,
14.8027575880675));
#155505=CARTESIAN_POINT('Ctrl Pts',(-17.9388973258418,-16.5171532868448,
14.8069273023879));
#155506=CARTESIAN_POINT('Ctrl Pts',(-17.8592986105402,-16.5446010022893,
14.8110970167083));
#155507=CARTESIAN_POINT('Ctrl Pts',(-17.7812419660685,-16.5758998066624,
14.8152667310286));
#155508=CARTESIAN_POINT('Ctrl Pts',(-17.7031880991871,-16.6071974972898,
14.8194362969727));
#155509=CARTESIAN_POINT('Ctrl Pts',(-17.6266766207018,-16.6423458323765,
14.8236058629167));
#155510=CARTESIAN_POINT('Ctrl Pts',(-17.552104243417,-16.6811582132233,
14.8277754288608));
#155511=CARTESIAN_POINT('Ctrl Pts',(-17.4749099933419,-16.7213351895004,
14.8320915915997));
#155512=CARTESIAN_POINT('Ctrl Pts',(-17.3997942069763,-16.7654384176638,
14.8364077543386));
#155513=CARTESIAN_POINT('Ctrl Pts',(-17.3271680714252,-16.8132097052907,
14.8407239170775));
#155514=CARTESIAN_POINT('Ctrl Pts',(-17.2569077246007,-16.8594248482479,
14.8448994812692));
#155515=CARTESIAN_POINT('Ctrl Pts',(-17.1889776711625,-16.9090724304067,
14.8490750454609));
#155516=CARTESIAN_POINT('Ctrl Pts',(-17.1237181590048,-16.9618762871215,
14.8532506096526));
#155517=CARTESIAN_POINT('Ctrl Pts',(-17.0551625440278,-17.0173471411098,
14.8576370716651));
#155518=CARTESIAN_POINT('Ctrl Pts',(-16.9895547726121,-17.0763011057024,
14.8620235336777));
#155519=CARTESIAN_POINT('Ctrl Pts',(-16.9272456352414,-17.13837416609,14.8664099956902));
#155520=CARTESIAN_POINT('Ctrl Pts',(-16.8649364978707,-17.2004472264777,
14.8707964577027));
#155521=CARTESIAN_POINT('Ctrl Pts',(-16.8059263275258,-17.2656389014522,
14.8751829197153));
#155522=CARTESIAN_POINT('Ctrl Pts',(-16.7505157350919,-17.3335469821889,
14.8795693817278));
#155523=CARTESIAN_POINT('Ctrl Pts',(-16.6976546661539,-17.398330511467,
14.8837540161209));
#155524=CARTESIAN_POINT('Ctrl Pts',(-16.6478724513803,-17.4658271045687,
14.8879386505139));
#155525=CARTESIAN_POINT('Ctrl Pts',(-16.6014597312929,-17.5357118928894,
14.892123284907));
#155526=CARTESIAN_POINT('Ctrl Pts',(-16.5551130739679,-17.605497208864,
14.8963019629909));
#155527=CARTESIAN_POINT('Ctrl Pts',(-16.5121266371781,-17.6776635880369,
14.9004806410749));
#155528=CARTESIAN_POINT('Ctrl Pts',(-16.4727509157818,-17.7518531010238,
14.9046593191588));
#155529=CARTESIAN_POINT('Ctrl Pts',(-16.4326694128783,-17.8273724077119,
14.9089128970443));
#155530=CARTESIAN_POINT('Ctrl Pts',(-16.3963296475342,-17.9049877173956,
14.9131664749297));
#155531=CARTESIAN_POINT('Ctrl Pts',(-16.3639497085597,-17.98429053118,14.9174200528151));
#155532=CARTESIAN_POINT('Ctrl Pts',(-16.3321975178866,-18.0620559051724,
14.9215911667931));
#155533=CARTESIAN_POINT('Ctrl Pts',(-16.3042531677127,-18.1414434905287,
14.925762280771));
#155534=CARTESIAN_POINT('Ctrl Pts',(-16.2802751807717,-18.2220448565132,
14.929933394749));
#155535=CARTESIAN_POINT('Ctrl Pts',(-16.2563052398757,-18.302619175931,
14.9341031090694));
#155536=CARTESIAN_POINT('Ctrl Pts',(-16.2362991499856,-18.3844060265128,
14.9382728233897));
#155537=CARTESIAN_POINT('Ctrl Pts',(-16.2203659101291,-18.4669807609602,
14.9424425377101));
#155538=CARTESIAN_POINT('Ctrl Pts',(-16.2044332372455,-18.5495525570442,
14.9466121036542));
#155539=CARTESIAN_POINT('Ctrl Pts',(-16.1925732125598,-18.6329117293879,
14.9507816695982));
#155540=CARTESIAN_POINT('Ctrl Pts',(-16.1848436692123,-18.7166237029672,
14.9549512355423));
#155541=CARTESIAN_POINT('Ctrl Pts',(-16.1768423646561,-18.8032788862675,
14.9592673982812));
#155542=CARTESIAN_POINT('Ctrl Pts',(-16.1732674495782,-18.890311616191,
14.9635835610201));
#155543=CARTESIAN_POINT('Ctrl Pts',(-16.1741243927921,-18.9772363947927,
14.967899723759));
#155544=CARTESIAN_POINT('Ctrl Pts',(-16.174953421171,-19.0613296078744,
14.9720752879507));
#155545=CARTESIAN_POINT('Ctrl Pts',(-16.1799299313356,-19.1453213272336,
14.9762508521424));
#155546=CARTESIAN_POINT('Ctrl Pts',(-16.1890058822549,-19.228775975552,
14.9804264163341));
#155547=CARTESIAN_POINT('Ctrl Pts',(-16.1985402378791,-19.3164457197621,
14.9848128783466));
#155548=CARTESIAN_POINT('Ctrl Pts',(-16.2125989501167,-19.4035221357512,
14.9891993403591));
#155549=CARTESIAN_POINT('Ctrl Pts',(-16.2310658163555,-19.4895132299243,
14.9935858023717));
#155550=CARTESIAN_POINT('Ctrl Pts',(-16.2495326825942,-19.5755043240973,
14.9979722643842));
#155551=CARTESIAN_POINT('Ctrl Pts',(-16.2724074784503,-19.660409556001,
15.0023587263968));
#155552=CARTESIAN_POINT('Ctrl Pts',(-16.2995147249235,-19.7437584514457,
15.0067451884093));
#155553=CARTESIAN_POINT('Ctrl Pts',(-16.325371504027,-19.8232624313191,
15.0109293012964));
#155554=CARTESIAN_POINT('Ctrl Pts',(-16.3551750808466,-19.9016463915223,
15.0151134141836));
#155555=CARTESIAN_POINT('Ctrl Pts',(-16.3888096569738,-19.9784902605368,
15.0192975270708));
#155556=CARTESIAN_POINT('Ctrl Pts',(-16.422398948156,-20.0552306684471,
15.023476006549));
#155557=CARTESIAN_POINT('Ctrl Pts',(-16.4598088143048,-20.1304346847381,
15.0276544860272));
#155558=CARTESIAN_POINT('Ctrl Pts',(-16.5008739124384,-20.2036979975424,
15.0318329655054));
#155559=CARTESIAN_POINT('Ctrl Pts',(-16.5429986555096,-20.2788517989138,
15.0361192665846));
#155560=CARTESIAN_POINT('Ctrl Pts',(-16.5889697394115,-20.3519628838743,
15.0404055676638));
#155561=CARTESIAN_POINT('Ctrl Pts',(-16.63855629866,-20.4226174534917,15.044691868743));
#155562=CARTESIAN_POINT('Ctrl Pts',(-16.6868081648856,-20.4913702545144,
15.0488627979103));
#155563=CARTESIAN_POINT('Ctrl Pts',(-16.7384830491083,-20.5577967113089,
15.0530337270777));
#155564=CARTESIAN_POINT('Ctrl Pts',(-16.7933230379798,-20.6215427305356,
15.057204656245));
#155565=CARTESIAN_POINT('Ctrl Pts',(-16.8504384170978,-20.6879336640552,
15.0615486432802));
#155566=CARTESIAN_POINT('Ctrl Pts',(-16.9109869827439,-20.7514164472448,
15.0658926303153));
#155567=CARTESIAN_POINT('Ctrl Pts',(-16.974630487842,-20.8116287047927,
15.0702366173505));
#155568=CARTESIAN_POINT('Ctrl Pts',(-17.03827399294,-20.8718409623405,15.0745806043856));
#155569=CARTESIAN_POINT('Ctrl Pts',(-17.1050120275129,-20.9287823061029,
15.0789245914208));
#155570=CARTESIAN_POINT('Ctrl Pts',(-17.1744641402401,-20.9821349467765,
15.0832685784559));
#155571=CARTESIAN_POINT('Origin',(-18.734,-18.952,-1.76670989022851));
#155572=CARTESIAN_POINT('',(-17.1744641402401,-20.9821349467765,15.9499155181261));
#155573=CARTESIAN_POINT('',(-17.172599330006,-20.9845253206546,15.883228700071));
#155574=CARTESIAN_POINT('',(-17.1744641402401,-20.9821349467765,-1.76670989022851));
#155575=CARTESIAN_POINT('',(-21.293999428374,-18.9537107672548,15.4332901097416));
#155576=CARTESIAN_POINT('Ctrl Pts',(-21.2939994283744,-18.9537107666516,
15.4332901097715));
#155577=CARTESIAN_POINT('Ctrl Pts',(-21.2940559692553,-18.8691027211111,
15.437482057942));
#155578=CARTESIAN_POINT('Ctrl Pts',(-21.2899137324165,-18.7844696898645,
15.4416740061124));
#155579=CARTESIAN_POINT('Ctrl Pts',(-21.2815918669692,-18.7002547332074,
15.4458659542829));
#155580=CARTESIAN_POINT('Ctrl Pts',(-21.2732695913204,-18.6160356254257,
15.4500581090829));
#155581=CARTESIAN_POINT('Ctrl Pts',(-21.2607673227297,-18.5322350838833,
15.4542502638829));
#155582=CARTESIAN_POINT('Ctrl Pts',(-21.2441560631151,-18.449290800953,
15.4584424186829));
#155583=CARTESIAN_POINT('Ctrl Pts',(-21.2275392030056,-18.3663185533138,
15.4626359868701));
#155584=CARTESIAN_POINT('Ctrl Pts',(-21.2068106889621,-18.2842035816671,
15.4668295550574));
#155585=CARTESIAN_POINT('Ctrl Pts',(-21.1820923104735,-18.2033718951306,
15.4710231232446));
#155586=CARTESIAN_POINT('Ctrl Pts',(-21.1573415752886,-18.1224343988081,
15.4752221808701));
#155587=CARTESIAN_POINT('Ctrl Pts',(-21.1285906849035,-18.0427839738201,
15.4794212384956));
#155588=CARTESIAN_POINT('Ctrl Pts',(-21.0960107310926,-17.9648296468171,
15.483620296121));
#155589=CARTESIAN_POINT('Ctrl Pts',(-21.0634063961442,-17.8868169828631,
15.4878224961022));
#155590=CARTESIAN_POINT('Ctrl Pts',(-21.0269674888688,-17.8105033515339,
15.4920246960833));
#155591=CARTESIAN_POINT('Ctrl Pts',(-20.9869114421218,-17.7362738655615,
15.4962268960644));
#155592=CARTESIAN_POINT('Ctrl Pts',(-20.9467843119657,-17.6619126520388,
15.5004365532642));
#155593=CARTESIAN_POINT('Ctrl Pts',(-20.9030274638811,-17.5896433529156,
15.5046462104641));
#155594=CARTESIAN_POINT('Ctrl Pts',(-20.8559018807132,-17.5198224940232,
15.5088558676639));
#155595=CARTESIAN_POINT('Ctrl Pts',(-20.8365799691019,-17.4911953158865,
15.5105818648582));
#155596=CARTESIAN_POINT('Ctrl Pts',(-20.8166922183615,-17.4629793510679,
15.5123078620525));
#155597=CARTESIAN_POINT('Ctrl Pts',(-20.7962584977301,-17.435197478727,
15.5140338592469));
#155598=CARTESIAN_POINT('Ctrl Pts',(-20.7467174843303,-17.3678410665132,
15.5182184936399));
#155599=CARTESIAN_POINT('Ctrl Pts',(-20.6937808669812,-17.3027889832896,
15.522403128033));
#155600=CARTESIAN_POINT('Ctrl Pts',(-20.6376906991394,-17.2404037502932,
15.526587762426));
#155601=CARTESIAN_POINT('Ctrl Pts',(-20.581680368709,-17.1781073149544,
15.53076644051));
#155602=CARTESIAN_POINT('Ctrl Pts',(-20.522525708678,-17.1184705290968,
15.5349451185939));
#155603=CARTESIAN_POINT('Ctrl Pts',(-20.4605108062944,-17.061825289623,
15.5391237966778));
#155604=CARTESIAN_POINT('Ctrl Pts',(-20.3973843313549,-17.0041647249419,
15.5433773745633));
#155605=CARTESIAN_POINT('Ctrl Pts',(-20.3312943514667,-16.9496043968549,
15.5476309524487));
#155606=CARTESIAN_POINT('Ctrl Pts',(-20.2625820107878,-16.8984574422973,
15.5518845303342));
#155607=CARTESIAN_POINT('Ctrl Pts',(-20.195201792914,-16.8483020712589,
15.5560556443121));
#155608=CARTESIAN_POINT('Ctrl Pts',(-20.1253003720614,-16.8014291923403,
15.5602267582901));
#155609=CARTESIAN_POINT('Ctrl Pts',(-20.0532336923064,-16.7580942442567,
15.564397872268));
#155610=CARTESIAN_POINT('Ctrl Pts',(-19.9811911952218,-16.7147738376335,
15.5685675865884));
#155611=CARTESIAN_POINT('Ctrl Pts',(-19.9069852761389,-16.6749892409427,
15.5727373009088));
#155612=CARTESIAN_POINT('Ctrl Pts',(-19.8309999421957,-16.6389519834594,
15.5769070152291));
#155613=CARTESIAN_POINT('Ctrl Pts',(-19.7550173121369,-16.6029160083363,
15.5810765811732));
#155614=CARTESIAN_POINT('Ctrl Pts',(-19.6772558091333,-16.5706273036551,
15.5852461471172));
#155615=CARTESIAN_POINT('Ctrl Pts',(-19.5981218233864,-16.5422503295265,
15.5894157130613));
#155616=CARTESIAN_POINT('Ctrl Pts',(-19.516205584323,-16.5128756559943,
15.5937318758002));
#155617=CARTESIAN_POINT('Ctrl Pts',(-19.4328190502828,-16.4876930819298,
15.5980480385391));
#155618=CARTESIAN_POINT('Ctrl Pts',(-19.3484309915969,-16.4668290689441,
15.602364201278));
#155619=CARTESIAN_POINT('Ctrl Pts',(-19.2667918650466,-16.4466446989869,
15.6065397654697));
#155620=CARTESIAN_POINT('Ctrl Pts',(-19.1842159325101,-16.4305019005906,
15.6107153296614));
#155621=CARTESIAN_POINT('Ctrl Pts',(-19.1011369778115,-16.4184628600466,
15.6148908938531));
#155622=CARTESIAN_POINT('Ctrl Pts',(-19.0138619026127,-16.4058157561847,
15.6192773558656));
#155623=CARTESIAN_POINT('Ctrl Pts',(-18.9260322359069,-16.3976979204099,
15.6236638178782));
#155624=CARTESIAN_POINT('Ctrl Pts',(-18.8381534037013,-16.3941196141146,
15.6280502798907));
#155625=CARTESIAN_POINT('Ctrl Pts',(-18.7502745714957,-16.3905413078192,
15.6324367419032));
#155626=CARTESIAN_POINT('Ctrl Pts',(-18.6623471531411,-16.391502448601,
15.6368232039158));
#155627=CARTESIAN_POINT('Ctrl Pts',(-18.5748705298081,-16.3969505265619,
15.6412096659283));
#155628=CARTESIAN_POINT('Ctrl Pts',(-18.4914188355861,-16.4021479303798,
15.6453943003213));
#155629=CARTESIAN_POINT('Ctrl Pts',(-18.4080667413618,-16.4114477893304,
15.6495789347144));
#155630=CARTESIAN_POINT('Ctrl Pts',(-18.3252500890705,-16.4248428006325,
15.6537635691074));
#155631=CARTESIAN_POINT('Ctrl Pts',(-18.242551316033,-16.4382187457939,
15.6579422471914));
#155632=CARTESIAN_POINT('Ctrl Pts',(-18.1603869213347,-16.4556781923685,
15.6621209252753));
#155633=CARTESIAN_POINT('Ctrl Pts',(-18.079189748786,-16.4771619174368,
15.6662996033593));
#155634=CARTESIAN_POINT('Ctrl Pts',(-17.9965371752748,-16.4990307228369,
15.6705531812447));
#155635=CARTESIAN_POINT('Ctrl Pts',(-17.9148873210948,-16.5250694661818,
15.6748067591302));
#155636=CARTESIAN_POINT('Ctrl Pts',(-17.834688139716,-16.5551607943059,
15.6790603370156));
#155637=CARTESIAN_POINT('Ctrl Pts',(-17.756043775964,-16.5846687433158,
15.6832314509935));
#155638=CARTESIAN_POINT('Ctrl Pts',(-17.6787947892653,-16.618073375769,
15.6874025649715));
#155639=CARTESIAN_POINT('Ctrl Pts',(-17.6033486289325,-16.6552136631582,
15.6915736789494));
#155640=CARTESIAN_POINT('Ctrl Pts',(-17.5279277852875,-16.6923414877653,
15.6957433932698));
#155641=CARTESIAN_POINT('Ctrl Pts',(-17.4543089789465,-16.7332022747586,
15.6999131075902));
#155642=CARTESIAN_POINT('Ctrl Pts',(-17.3828779283351,-16.7775876316899,
15.7040828219106));
#155643=CARTESIAN_POINT('Ctrl Pts',(-17.311449419547,-16.8219714091997,
15.7082523878546));
#155644=CARTESIAN_POINT('Ctrl Pts',(-17.2422089019961,-16.8698792637608,
15.7124219537986));
#155645=CARTESIAN_POINT('Ctrl Pts',(-17.1755146319174,-16.9210585046653,
15.7165915197427));
#155646=CARTESIAN_POINT('Ctrl Pts',(-17.106475473579,-16.9740371445436,
15.7209076824816));
#155647=CARTESIAN_POINT('Ctrl Pts',(-17.0401653646942,-17.0305211737505,
15.7252238452205));
#155648=CARTESIAN_POINT('Ctrl Pts',(-16.9769443759542,-17.0901848818937,
15.7295400079594));
#155649=CARTESIAN_POINT('Ctrl Pts',(-16.9157828042729,-17.1479050510196,
15.7337155721511));
#155650=CARTESIAN_POINT('Ctrl Pts',(-16.8575124793693,-17.2086005517587,
15.7378911363428));
#155651=CARTESIAN_POINT('Ctrl Pts',(-16.8024204890299,-17.2719403008225,
15.7420667005345));
#155652=CARTESIAN_POINT('Ctrl Pts',(-16.7445459332272,-17.3384791900356,
15.746453162547));
#155653=CARTESIAN_POINT('Ctrl Pts',(-16.6901795852494,-17.4079360098511,
15.7508396245596));
#155654=CARTESIAN_POINT('Ctrl Pts',(-16.6396036508152,-17.4798913312797,
15.7552260865721));
#155655=CARTESIAN_POINT('Ctrl Pts',(-16.589027716381,-17.5518466527083,
15.7596125485847));
#155656=CARTESIAN_POINT('Ctrl Pts',(-16.5422424397947,-17.6262999440046,
15.7639990105972));
#155657=CARTESIAN_POINT('Ctrl Pts',(-16.4994739740979,-17.7028028820213,
15.7683854726097));
#155658=CARTESIAN_POINT('Ctrl Pts',(-16.458673348906,-17.7757858064552,
15.7725701070028));
#155659=CARTESIAN_POINT('Ctrl Pts',(-16.4213761508428,-17.8509055642073,
15.7767547413958));
#155660=CARTESIAN_POINT('Ctrl Pts',(-16.3878121523981,-17.9277917283262,
15.7809393757889));
#155661=CARTESIAN_POINT('Ctrl Pts',(-16.3542959281508,-18.004568454507,
15.7851180538728));
#155662=CARTESIAN_POINT('Ctrl Pts',(-16.3245025312236,-18.0831061749369,
15.7892967319568));
#155663=CARTESIAN_POINT('Ctrl Pts',(-16.2986164546585,-18.1630088802274,
15.7934754100407));
#155664=CARTESIAN_POINT('Ctrl Pts',(-16.272266388775,-18.2443437840853,
15.7977289879261));
#155665=CARTESIAN_POINT('Ctrl Pts',(-16.249965333752,-18.3270926679897,
15.8019825658115));
#155666=CARTESIAN_POINT('Ctrl Pts',(-16.2318570828658,-18.41081535292,15.806236143697));
#155667=CARTESIAN_POINT('Ctrl Pts',(-16.2140998957584,-18.4929149102316,
15.8104072576749));
#155668=CARTESIAN_POINT('Ctrl Pts',(-16.2003744938966,-18.575950377106,
15.8145783716529));
#155669=CARTESIAN_POINT('Ctrl Pts',(-16.1907660223746,-18.6594919914747,
15.8187494856308));
#155670=CARTESIAN_POINT('Ctrl Pts',(-16.1811607750679,-18.7430055726478,
15.8229191999512));
#155671=CARTESIAN_POINT('Ctrl Pts',(-16.1756697669882,-18.8270245073652,
15.8270889142716));
#155672=CARTESIAN_POINT('Ctrl Pts',(-16.1743265551335,-18.9111116685926,
15.8312586285919));
#155673=CARTESIAN_POINT('Ctrl Pts',(-16.172983391076,-18.9951958376379,
15.835428194536));
#155674=CARTESIAN_POINT('Ctrl Pts',(-16.1757877362795,-19.0793477683783,
15.83959776048));
#155675=CARTESIAN_POINT('Ctrl Pts',(-16.182721035153,-19.1631294473279,
15.8437673264241));
#155676=CARTESIAN_POINT('Ctrl Pts',(-16.1898981002616,-19.2498567867534,
15.848083489163));
#155677=CARTESIAN_POINT('Ctrl Pts',(-16.2014998257646,-19.3361868282285,
15.8523996519019));
#155678=CARTESIAN_POINT('Ctrl Pts',(-16.2174472402024,-19.4216405084265,
15.8567158146408));
#155679=CARTESIAN_POINT('Ctrl Pts',(-16.2328751692923,-19.5043105439801,
15.8608913788325));
#155680=CARTESIAN_POINT('Ctrl Pts',(-16.2523698584563,-19.5861599891139,
15.8650669430242));
#155681=CARTESIAN_POINT('Ctrl Pts',(-16.2758083142179,-19.6667682393277,
15.8692425072158));
#155682=CARTESIAN_POINT('Ctrl Pts',(-16.3004305906603,-19.7514478206318,
15.8736289692284));
#155683=CARTESIAN_POINT('Ctrl Pts',(-16.329405311324,-19.8347569748333,
15.8780154312409));
#155684=CARTESIAN_POINT('Ctrl Pts',(-16.3625325554081,-19.9162313826259,
15.8824018932535));
#155685=CARTESIAN_POINT('Ctrl Pts',(-16.3956597994922,-19.9977057904185,
15.886788355266));
#155686=CARTESIAN_POINT('Ctrl Pts',(-16.4329392521203,-20.0773449585574,
15.8911748172785));
#155687=CARTESIAN_POINT('Ctrl Pts',(-16.4741163568262,-20.1547160593073,
15.8955612792911));
#155688=CARTESIAN_POINT('Ctrl Pts',(-16.5134028649757,-20.2285347603028,
15.8997463422486));
#155689=CARTESIAN_POINT('Ctrl Pts',(-16.5563832077462,-20.3005638940195,
15.9039314052061));
#155690=CARTESIAN_POINT('Ctrl Pts',(-16.602870226229,-20.3704096331268,
15.9081164681637));
#155691=CARTESIAN_POINT('Ctrl Pts',(-16.6492791580943,-20.4401380487813,
15.9122945012573));
#155692=CARTESIAN_POINT('Ctrl Pts',(-16.6991828014366,-20.5076899821208,
15.916472534351));
#155693=CARTESIAN_POINT('Ctrl Pts',(-16.7523481443704,-20.5726961229916,
15.9206505674447));
#155694=CARTESIAN_POINT('Ctrl Pts',(-16.8054619536597,-20.637639252826,
15.9248245507334));
#155695=CARTESIAN_POINT('Ctrl Pts',(-16.861830896424,-20.700041135037,15.928998534022));
#155696=CARTESIAN_POINT('Ctrl Pts',(-16.9211791819455,-20.7595620823718,
15.9331725173107));
#155697=CARTESIAN_POINT('Ctrl Pts',(-16.9804837256674,-20.819039160649,
15.9373434242251));
#155698=CARTESIAN_POINT('Ctrl Pts',(-17.0427629244445,-20.8756391989201,
15.9415143311394));
#155699=CARTESIAN_POINT('Ctrl Pts',(-17.1077022600319,-20.9290573236441,
15.9456852380538));
#155700=CARTESIAN_POINT('Ctrl Pts',(-17.1296568439216,-20.9471168354927,
15.9470953314112));
#155701=CARTESIAN_POINT('Ctrl Pts',(-17.1519151618286,-20.9648129749097,
15.9485054247686));
#155702=CARTESIAN_POINT('Ctrl Pts',(-17.1744641402401,-20.9821349467765,
15.9499155181261));
#155703=CARTESIAN_POINT('Ctrl Pts',(-17.1744641402401,-20.9821349467764,
15.1499553790579));
#155704=CARTESIAN_POINT('Ctrl Pts',(-17.2409405369923,-21.0332016626749,
15.1541321105618));
#155705=CARTESIAN_POINT('Ctrl Pts',(-17.3100169746969,-21.0810682907154,
15.1583088420657));
#155706=CARTESIAN_POINT('Ctrl Pts',(-17.3813511233023,-21.125462908901,
15.1624855735696));
#155707=CARTESIAN_POINT('Ctrl Pts',(-17.4526153147779,-21.1698139894525,
15.1666582089688));
#155708=CARTESIAN_POINT('Ctrl Pts',(-17.5261324278215,-21.2106995852222,
15.1708308443679));
#155709=CARTESIAN_POINT('Ctrl Pts',(-17.6015297561884,-21.2478900554864,
15.1750034797671));
#155710=CARTESIAN_POINT('Ctrl Pts',(-17.6768875635137,-21.2850610316099,
15.1791739279946));
#155711=CARTESIAN_POINT('Ctrl Pts',(-17.7541232175784,-21.3185405247747,
15.1833443762221));
#155712=CARTESIAN_POINT('Ctrl Pts',(-17.8328389420969,-21.3481445590196,
15.1875148244496));
#155713=CARTESIAN_POINT('Ctrl Pts',(-17.9115370192045,-21.377741956286,
15.1916843376973));
#155714=CARTESIAN_POINT('Ctrl Pts',(-17.9917140771595,-21.4034654587896,
15.195853850945));
#155715=CARTESIAN_POINT('Ctrl Pts',(-18.0729531407356,-21.4251795425841,
15.2000233641926));
#155716=CARTESIAN_POINT('Ctrl Pts',(-18.1541983607488,-21.4468952719096,
15.2041931934133));
#155717=CARTESIAN_POINT('Ctrl Pts',(-18.2365053014123,-21.4646008616881,
15.2083630226339));
#155718=CARTESIAN_POINT('Ctrl Pts',(-18.3194439686069,-21.4782112534061,
15.2125328518545));
#155719=CARTESIAN_POINT('Ctrl Pts',(-18.4024694322536,-21.4918358885856,
15.2167070448586));
#155720=CARTESIAN_POINT('Ctrl Pts',(-18.4861274876637,-21.5013566932214,
15.2208812378627));
#155721=CARTESIAN_POINT('Ctrl Pts',(-18.5699806281551,-21.5067402305635,
15.2250554308667));
#155722=CARTESIAN_POINT('Ctrl Pts',(-18.6538791094179,-21.5121266788727,
15.2292318809256));
#155723=CARTESIAN_POINT('Ctrl Pts',(-18.7379724256015,-21.5133713983878,
15.2334083309844));
#155724=CARTESIAN_POINT('Ctrl Pts',(-18.821823103729,-21.5104931312105,
15.2375847810432));
#155725=CARTESIAN_POINT('Ctrl Pts',(-18.9058196496713,-21.5076098569593,
15.2417684965131));
#155726=CARTESIAN_POINT('Ctrl Pts',(-18.9895722555945,-21.5005893083999,
15.245952211983));
#155727=CARTESIAN_POINT('Ctrl Pts',(-19.072648815734,-21.4895021142064,
15.2501359274529));
#155728=CARTESIAN_POINT('Ctrl Pts',(-19.1358362944999,-21.4810692680884,
15.2533180335966));
#155729=CARTESIAN_POINT('Ctrl Pts',(-19.1986327885576,-21.4702849361346,
15.2565001397403));
#155730=CARTESIAN_POINT('Ctrl Pts',(-19.2608535512399,-21.4571996598167,
15.259682245884));
#155731=CARTESIAN_POINT('Ctrl Pts',(-19.3426770768309,-21.4399918437197,
15.263866880277));
#155732=CARTESIAN_POINT('Ctrl Pts',(-19.4238089369639,-21.4187390730901,
15.2680515146701));
#155733=CARTESIAN_POINT('Ctrl Pts',(-19.5038189245161,-21.3935115857716,
15.2722361490631));
#155734=CARTESIAN_POINT('Ctrl Pts',(-19.5837150277544,-21.3683200066587,
15.2764148271471));
#155735=CARTESIAN_POINT('Ctrl Pts',(-19.6624919952641,-21.33916508562,15.280593505231));
#155736=CARTESIAN_POINT('Ctrl Pts',(-19.7397300928954,-21.3061680017035,
15.284772183315));
#155737=CARTESIAN_POINT('Ctrl Pts',(-19.8183526279167,-21.2725794687723,
15.2890257612004));
#155738=CARTESIAN_POINT('Ctrl Pts',(-19.8953801101215,-21.2350097758302,
15.2932793390858));
#155739=CARTESIAN_POINT('Ctrl Pts',(-19.9703862586167,-21.1936398059242,
15.2975329169713));
#155740=CARTESIAN_POINT('Ctrl Pts',(-20.0439382665608,-21.1530718736117,
15.3017040309492));
#155741=CARTESIAN_POINT('Ctrl Pts',(-20.1155461950122,-21.1088499333759,
15.3058751449272));
#155742=CARTESIAN_POINT('Ctrl Pts',(-20.1848301560489,-21.0611922288637,
15.3100462589051));
#155743=CARTESIAN_POINT('Ctrl Pts',(-20.2540908681833,-21.0135505163546,
15.3142159732255));
#155744=CARTESIAN_POINT('Ctrl Pts',(-20.3210287829501,-20.9624755897522,
15.3183856875459));
#155745=CARTESIAN_POINT('Ctrl Pts',(-20.385292362642,-20.9082294172924,
15.3225554018662));
#155746=CARTESIAN_POINT('Ctrl Pts',(-20.4495536555601,-20.8539851751442,
15.3267249678103));
#155747=CARTESIAN_POINT('Ctrl Pts',(-20.511140451629,-20.7965702088955,
15.3308945337543));
#155748=CARTESIAN_POINT('Ctrl Pts',(-20.5697347912253,-20.7362863492963,
15.3350640996984));
#155749=CARTESIAN_POINT('Ctrl Pts',(-20.6303892355178,-20.6738829835618,
15.3393802624373));
#155750=CARTESIAN_POINT('Ctrl Pts',(-20.6878365109499,-20.6084056085288,
15.3436964251762));
#155751=CARTESIAN_POINT('Ctrl Pts',(-20.7417674193153,-20.5402285698022,
15.3480125879151));
#155752=CARTESIAN_POINT('Ctrl Pts',(-20.7939415340131,-20.4742723909413,
15.3521881521068));
#155753=CARTESIAN_POINT('Ctrl Pts',(-20.8428246196126,-20.4057901412951,
15.3563637162985));
#155754=CARTESIAN_POINT('Ctrl Pts',(-20.8881804708297,-20.3351509314228,
15.3605392804902));
#155755=CARTESIAN_POINT('Ctrl Pts',(-20.9358271382687,-20.2609439029885,
15.3649257425027));
#155756=CARTESIAN_POINT('Ctrl Pts',(-20.9795805961807,-20.1843567987732,
15.3693122045153));
#155757=CARTESIAN_POINT('Ctrl Pts',(-21.0192222426252,-20.1058454410409,
15.3736986665278));
#155758=CARTESIAN_POINT('Ctrl Pts',(-21.0588638890698,-20.0273340833086,
15.3780851285404));
#155759=CARTESIAN_POINT('Ctrl Pts',(-21.0943935591862,-19.9468990335383,
15.3824715905529));
#155760=CARTESIAN_POINT('Ctrl Pts',(-21.1256522921828,-19.8650166007783,
15.3868580525655));
#155761=CARTESIAN_POINT('Ctrl Pts',(-21.1596866697226,-19.7758633510054,
15.3916340140293));
#155762=CARTESIAN_POINT('Ctrl Pts',(-21.1887650239783,-19.6847190703918,
15.3964099754931));
#155763=CARTESIAN_POINT('Ctrl Pts',(-21.2126811308614,-19.5921092496689,
15.4011859369569));
#155764=CARTESIAN_POINT('Ctrl Pts',(-21.2364993763692,-19.4998783754223,
15.4059423558521));
#155765=CARTESIAN_POINT('Ctrl Pts',(-21.2551974088384,-19.4061941121839,
15.4106987747474));
#155766=CARTESIAN_POINT('Ctrl Pts',(-21.2686182636666,-19.3115973546727,
15.4154551936427));
#155767=CARTESIAN_POINT('Ctrl Pts',(-21.2819450244391,-19.2176638181475,
15.4201782651282));
#155768=CARTESIAN_POINT('Ctrl Pts',(-21.2900682365862,-19.1228307363249,
15.4249013366138));
#155769=CARTESIAN_POINT('Ctrl Pts',(-21.2928821031965,-19.0276464271503,
15.4296244080994));
#155770=CARTESIAN_POINT('Ctrl Pts',(-21.2936100754836,-19.0030214008636,
15.4308463086468));
#155771=CARTESIAN_POINT('Ctrl Pts',(-21.2939829474075,-18.9783729560409,
15.4320682091942));
#155772=CARTESIAN_POINT('Ctrl Pts',(-21.293999428374,-18.9537107672549,
15.4332901097416));
#155773=CARTESIAN_POINT('',(-21.2939991231355,-18.9498811452879,15.3667098902285));
#155774=CARTESIAN_POINT('Ctrl Pts',(-17.1744641402401,-20.9821349467765,
15.0832685784559));
#155775=CARTESIAN_POINT('Ctrl Pts',(-17.2419504786654,-21.0339774929999,
15.0874896131755));
#155776=CARTESIAN_POINT('Ctrl Pts',(-17.3119988557323,-21.0824315373856,
15.0917106478951));
#155777=CARTESIAN_POINT('Ctrl Pts',(-17.3842279220291,-21.1272506378645,
15.0959316826146));
#155778=CARTESIAN_POINT('Ctrl Pts',(-17.4556818103574,-21.1715887300592,
15.1001074162762));
#155779=CARTESIAN_POINT('Ctrl Pts',(-17.5292693675069,-21.2123693557197,
15.1042831499379));
#155780=CARTESIAN_POINT('Ctrl Pts',(-17.6045968204046,-21.2494003695307,
15.1084588835995));
#155781=CARTESIAN_POINT('Ctrl Pts',(-17.6811500746533,-21.2870339879037,
15.112702568848));
#155782=CARTESIAN_POINT('Ctrl Pts',(-17.7594999004546,-21.3207946763895,
15.1169462540966));
#155783=CARTESIAN_POINT('Ctrl Pts',(-17.8392139384063,-21.3505324479727,
15.1211899393451));
#155784=CARTESIAN_POINT('Ctrl Pts',(-17.9189279763581,-21.3802702195558,
15.1254336245937));
#155785=CARTESIAN_POINT('Ctrl Pts',(-18.000005738032,-21.4059849886204,
15.1296773098422));
#155786=CARTESIAN_POINT('Ctrl Pts',(-18.0820028534413,-21.4275806835729,
15.1339209950908));
#155787=CARTESIAN_POINT('Ctrl Pts',(-18.1628589794675,-21.4488758745561,
15.1381056294838));
#155788=CARTESIAN_POINT('Ctrl Pts',(-18.2449099711163,-21.4662452083818,
15.1422902638769));
#155789=CARTESIAN_POINT('Ctrl Pts',(-18.3277397785898,-21.4795586308728,
15.1464748982699));
#155790=CARTESIAN_POINT('Ctrl Pts',(-18.4104516880846,-21.4928531033548,
15.1506535763538));
#155791=CARTESIAN_POINT('Ctrl Pts',(-18.4939397611609,-21.5021030592902,
15.1548322544378));
#155792=CARTESIAN_POINT('Ctrl Pts',(-18.5777744755002,-21.5072286757734,
15.1590109325217));
#155793=CARTESIAN_POINT('Ctrl Pts',(-18.6631118668432,-21.5124461652484,
15.1632645104072));
#155794=CARTESIAN_POINT('Ctrl Pts',(-18.7488079825307,-21.5133898805874,
15.1675180882926));
#155795=CARTESIAN_POINT('Ctrl Pts',(-18.8344006857365,-21.510030434202,
15.171771666178));
#155796=CARTESIAN_POINT('Ctrl Pts',(-18.9183340073703,-21.5067361172402,
15.175942780156));
#155797=CARTESIAN_POINT('Ctrl Pts',(-19.0021674095972,-21.4993040188572,
15.1801138941339));
#155798=CARTESIAN_POINT('Ctrl Pts',(-19.0854634797585,-21.4877589440631,
15.1842850081119));
#155799=CARTESIAN_POINT('Ctrl Pts',(-19.1687315991189,-21.4762177433303,
15.1884547224322));
#155800=CARTESIAN_POINT('Ctrl Pts',(-19.2514622892087,-21.4605663702897,
15.1926244367526));
#155801=CARTESIAN_POINT('Ctrl Pts',(-19.3332238803096,-21.4408814237056,
15.196794151073));
#155802=CARTESIAN_POINT('Ctrl Pts',(-19.4149825619822,-21.4211971775964,
15.200963717017));
#155803=CARTESIAN_POINT('Ctrl Pts',(-19.4957717661771,-21.3974797518312,
15.2051332829611));
#155804=CARTESIAN_POINT('Ctrl Pts',(-19.5751719705272,-21.3698564299808,
15.2093028489051));
#155805=CARTESIAN_POINT('Ctrl Pts',(-19.6573637881115,-21.3412619062112,
15.2136190116441));
#155806=CARTESIAN_POINT('Ctrl Pts',(-19.7380666159169,-21.3084818866878,
15.217935174383));
#155807=CARTESIAN_POINT('Ctrl Pts',(-19.8168362586924,-21.2717124039115,
15.2222513371219));
#155808=CARTESIAN_POINT('Ctrl Pts',(-19.8930399886396,-21.2361406831692,
15.2264269013136));
#155809=CARTESIAN_POINT('Ctrl Pts',(-19.9674341519886,-21.1968356830555,
15.2306024655052));
#155810=CARTESIAN_POINT('Ctrl Pts',(-20.0396421490703,-21.1540214755018,
15.2347780296969));
#155811=CARTESIAN_POINT('Ctrl Pts',(-20.1154972004264,-21.1090448241057,
15.2391644917094));
#155812=CARTESIAN_POINT('Ctrl Pts',(-20.188938948885,-21.0601954720668,
15.243550953722));
#155813=CARTESIAN_POINT('Ctrl Pts',(-20.259567662025,-21.0077828943212,
15.2479374157345));
#155814=CARTESIAN_POINT('Ctrl Pts',(-20.330196375165,-20.9553703165755,
15.252323877747));
#155815=CARTESIAN_POINT('Ctrl Pts',(-20.398011653933,-20.899394941135,15.2567103397596));
#155816=CARTESIAN_POINT('Ctrl Pts',(-20.4626578964185,-20.8402112903883,
15.2610968017721));
#155817=CARTESIAN_POINT('Ctrl Pts',(-20.5234100187943,-20.7845927075509,
15.2652190348167));
#155818=CARTESIAN_POINT('Ctrl Pts',(-20.5816044022752,-20.7259204795934,
15.2693412678613));
#155819=CARTESIAN_POINT('Ctrl Pts',(-20.6369112461382,-20.6644627847987,
15.2734635009059));
#155820=CARTESIAN_POINT('Ctrl Pts',(-20.6921256485478,-20.6031078121671,
15.2775788439313));
#155821=CARTESIAN_POINT('Ctrl Pts',(-20.7444617859852,-20.538976972769,
15.2816941869567));
#155822=CARTESIAN_POINT('Ctrl Pts',(-20.7936245240703,-20.4723771965695,
15.2858095299821));
#155823=CARTESIAN_POINT('Ctrl Pts',(-20.8427410076358,-20.4058400804406,
15.2899210011074));
#155824=CARTESIAN_POINT('Ctrl Pts',(-20.888689733586,-20.3368390147958,
15.2940324722326));
#155825=CARTESIAN_POINT('Ctrl Pts',(-20.9312146121388,-20.26571532236,15.2981439433578));
#155826=CARTESIAN_POINT('Ctrl Pts',(-20.9737131282065,-20.1946357216972,
15.3022528656552));
#155827=CARTESIAN_POINT('Ctrl Pts',(-21.0127917657816,-20.1214365120737,
15.3063617879525));
#155828=CARTESIAN_POINT('Ctrl Pts',(-21.0482376124058,-20.0464881330222,
15.3104707102499));
#155829=CARTESIAN_POINT('Ctrl Pts',(-21.0836728562216,-19.9715621730513,
15.3145784034578));
#155830=CARTESIAN_POINT('Ctrl Pts',(-21.1154772648505,-19.8948885121031,
15.3186860966657));
#155831=CARTESIAN_POINT('Ctrl Pts',(-21.1434845038947,-19.8168609284106,
15.3227937898736));
#155832=CARTESIAN_POINT('Ctrl Pts',(-21.1715053065238,-19.7387955568538,
15.3269034723903));
#155833=CARTESIAN_POINT('Ctrl Pts',(-21.1957251016683,-19.6593753990475,
15.3310131549069));
#155834=CARTESIAN_POINT('Ctrl Pts',(-21.2160265895469,-19.5790119686115,
15.3351228374236));
#155835=CARTESIAN_POINT('Ctrl Pts',(-21.2363332616042,-19.4986280166064,
15.3392335693869));
#155836=CARTESIAN_POINT('Ctrl Pts',(-21.2527195357624,-19.4173007774455,
15.3433443013502));
#155837=CARTESIAN_POINT('Ctrl Pts',(-21.265119175788,-19.3354523672614,
15.3474550333135));
#155838=CARTESIAN_POINT('Ctrl Pts',(-21.277533866187,-19.2535046115213,
15.3515707547806));
#155839=CARTESIAN_POINT('Ctrl Pts',(-21.2859522113271,-19.1710348943524,
15.3556864762477));
#155840=CARTESIAN_POINT('Ctrl Pts',(-21.2903598951029,-19.0884700945603,
15.3598021977147));
#155841=CARTESIAN_POINT('Ctrl Pts',(-21.2928257992759,-19.0422787399392,
15.362104761886));
#155842=CARTESIAN_POINT('Ctrl Pts',(-21.294037342402,-18.9960576424384,
15.3644073260573));
#155843=CARTESIAN_POINT('Ctrl Pts',(-21.2939991231355,-18.9498811452879,
15.3667098902285));
#155844=CARTESIAN_POINT('Ctrl Pts',(-21.2956373739999,-18.9498797893439,
15.3667098902285));
#155845=CARTESIAN_POINT('Ctrl Pts',(-21.296922788715,-18.8056440679786,
15.3738974629702));
#155846=CARTESIAN_POINT('Ctrl Pts',(-21.2201491749354,-17.8120820090192,
15.4234769712724));
#155847=CARTESIAN_POINT('Ctrl Pts',(-19.9200692397814,-16.166945137558,
15.515448415135));
#155848=CARTESIAN_POINT('Ctrl Pts',(-17.0342063890851,-16.4472060945738,
15.6426242218164));
#155849=CARTESIAN_POINT('Ctrl Pts',(-15.7555915863648,-18.9325607617256,
15.7652176501285));
#155850=CARTESIAN_POINT('Ctrl Pts',(-16.5753465902488,-20.5182929546658,
15.84541914288));
#155851=CARTESIAN_POINT('Ctrl Pts',(-17.172599330006,-20.9845253206546,
15.883228700071));
#155852=CARTESIAN_POINT('Origin',(-18.734,-18.952,-1.76670989022851));
#155853=CARTESIAN_POINT('',(-17.1744641402402,-20.9821349467765,16.7498176584939));
#155854=CARTESIAN_POINT('',(-17.1744641402401,-20.9821349467765,16.6833822503202));
#155855=CARTESIAN_POINT('',(-17.1744641402401,-20.9821349467765,-1.76670989022851));
#155856=CARTESIAN_POINT('',(-21.2939992944986,-18.9500994299065,16.2332901098004));
#155857=CARTESIAN_POINT('Ctrl Pts',(-21.2939992944986,-18.9500994299065,
16.2332901098004));
#155858=CARTESIAN_POINT('Ctrl Pts',(-21.2939272486892,-18.8530563258845,
16.2381006886061));
#155859=CARTESIAN_POINT('Ctrl Pts',(-21.2883332378637,-18.7562381388316,
16.2429112674119));
#155860=CARTESIAN_POINT('Ctrl Pts',(-21.277317503626,-18.6602191305971,
16.2477218462176));
#155861=CARTESIAN_POINT('Ctrl Pts',(-21.2661096544806,-18.5625255464771,
16.2526163217373));
#155862=CARTESIAN_POINT('Ctrl Pts',(-21.2492893600035,-18.4656594493969,
16.2575107972569));
#155863=CARTESIAN_POINT('Ctrl Pts',(-21.2270132516535,-18.3702054253606,
16.2624052727766));
#155864=CARTESIAN_POINT('Ctrl Pts',(-21.2047371433035,-18.2747514013242,
16.2672997482962));
#155865=CARTESIAN_POINT('Ctrl Pts',(-21.1770053785921,-18.1807095711097,
16.2721942238158));
#155866=CARTESIAN_POINT('Ctrl Pts',(-21.1440235064311,-18.088642195582,
16.2770886993355));
#155867=CARTESIAN_POINT('Ctrl Pts',(-21.1158249638011,-18.0099272639074,
16.2812733337285));
#155868=CARTESIAN_POINT('Ctrl Pts',(-21.0837134704203,-17.9324488089605,
16.2854579681216));
#155869=CARTESIAN_POINT('Ctrl Pts',(-21.0478172393664,-17.856623451588,
16.2896426025146));
#155870=CARTESIAN_POINT('Ctrl Pts',(-21.0119721021543,-17.7809060222264,
16.2938212805986));
#155871=CARTESIAN_POINT('Ctrl Pts',(-20.9723531229121,-17.7068374289185,
16.2979999586825));
#155872=CARTESIAN_POINT('Ctrl Pts',(-20.9291375533229,-17.6348169747558,
16.3021786367665));
#155873=CARTESIAN_POINT('Ctrl Pts',(-20.8851473757074,-17.5615056057125,
16.3064322146519));
#155874=CARTESIAN_POINT('Ctrl Pts',(-20.8374305643562,-17.4903169777088,
16.3106857925373));
#155875=CARTESIAN_POINT('Ctrl Pts',(-20.7862244101174,-17.4216487427658,
16.3149393704228));
#155876=CARTESIAN_POINT('Ctrl Pts',(-20.7360109870992,-17.3543117755523,
16.3191104844007));
#155877=CARTESIAN_POINT('Ctrl Pts',(-20.6824425969515,-17.2893987337786,
16.3232815983787));
#155878=CARTESIAN_POINT('Ctrl Pts',(-20.6257872198942,-17.2272562176819,
16.3274527123566));
#155879=CARTESIAN_POINT('Ctrl Pts',(-20.5691508540959,-17.1651345541068,
16.331622426677));
#155880=CARTESIAN_POINT('Ctrl Pts',(-20.5094298683179,-17.105781909528,
16.3357921409974));
#155881=CARTESIAN_POINT('Ctrl Pts',(-20.4469316957118,-17.0495108394984,
16.3399618553177));
#155882=CARTESIAN_POINT('Ctrl Pts',(-20.3844357470588,-16.993241771835,
16.3441314212618));
#155883=CARTESIAN_POINT('Ctrl Pts',(-20.3191631505139,-16.9400543678782,
16.3483009872058));
#155884=CARTESIAN_POINT('Ctrl Pts',(-20.2514562536418,-16.890222485746,
16.3524705531499));
#155885=CARTESIAN_POINT('Ctrl Pts',(-20.1813688658012,-16.8386385761122,
16.3567867158888));
#155886=CARTESIAN_POINT('Ctrl Pts',(-20.108673237446,-16.7906508514966,
16.3611028786277));
#155887=CARTESIAN_POINT('Ctrl Pts',(-20.0337823603675,-16.7465146076935,
16.3654190413666));
#155888=CARTESIAN_POINT('Ctrl Pts',(-19.9613310457328,-16.7038160973899,
16.3695946055583));
#155889=CARTESIAN_POINT('Ctrl Pts',(-19.8868257455389,-16.6647221743667,
16.37377016975));
#155890=CARTESIAN_POINT('Ctrl Pts',(-19.8106643175706,-16.6294165359948,
16.3779457339417));
#155891=CARTESIAN_POINT('Ctrl Pts',(-19.7306561569322,-16.59232769376,16.3823321959542));
#155892=CARTESIAN_POINT('Ctrl Pts',(-19.6488207114385,-16.5594201038734,
16.3867186579667));
#155893=CARTESIAN_POINT('Ctrl Pts',(-19.5656393424726,-16.5308482071436,
16.3911051199793));
#155894=CARTESIAN_POINT('Ctrl Pts',(-19.4824579735068,-16.5022763104138,
16.3954915819918));
#155895=CARTESIAN_POINT('Ctrl Pts',(-19.3979312597771,-16.4780401936422,
16.3998780440044));
#155896=CARTESIAN_POINT('Ctrl Pts',(-19.3125527301389,-16.4582324209244,
16.4042645060169));
#155897=CARTESIAN_POINT('Ctrl Pts',(-19.2311025932107,-16.4393360331914,
16.4084491404099));
#155898=CARTESIAN_POINT('Ctrl Pts',(-19.1485741315074,-16.4243990992031,
16.412633774803));
#155899=CARTESIAN_POINT('Ctrl Pts',(-19.0653870565365,-16.4135393210136,
16.416818409196));
#155900=CARTESIAN_POINT('Ctrl Pts',(-18.9823183880704,-16.4026950003742,
16.42099708728));
#155901=CARTESIAN_POINT('Ctrl Pts',(-18.8985934206771,-16.3959163673419,
16.4251757653639));
#155902=CARTESIAN_POINT('Ctrl Pts',(-18.8146438480398,-16.393270516492,
16.4293544434479));
#155903=CARTESIAN_POINT('Ctrl Pts',(-18.7291895396465,-16.390577240667,
16.4336080213333));
#155904=CARTESIAN_POINT('Ctrl Pts',(-18.6435029643765,-16.392166473525,
16.4378615992187));
#155905=CARTESIAN_POINT('Ctrl Pts',(-18.5580469256853,-16.3980539325117,
16.4421151771042));
#155906=CARTESIAN_POINT('Ctrl Pts',(-18.4742476190579,-16.4038272516174,
16.4462862910821));
#155907=CARTESIAN_POINT('Ctrl Pts',(-18.3906704700557,-16.4137335920112,
16.4504574050601));
#155908=CARTESIAN_POINT('Ctrl Pts',(-18.307751967238,-16.4277352328715,
16.454628519038));
#155909=CARTESIAN_POINT('Ctrl Pts',(-18.2248612885247,-16.4417321753459,
16.4587982333584));
#155910=CARTESIAN_POINT('Ctrl Pts',(-18.1426292702901,-16.4598216125358,
16.4629679476788));
#155911=CARTESIAN_POINT('Ctrl Pts',(-18.0614851300251,-16.4819142222055,
16.4671376619991));
#155912=CARTESIAN_POINT('Ctrl Pts',(-17.9803438772167,-16.5040060457254,
16.4713072279432));
#155913=CARTESIAN_POINT('Ctrl Pts',(-17.9002908690612,-16.5301006368245,
16.4754767938872));
#155914=CARTESIAN_POINT('Ctrl Pts',(-17.8217416831402,-16.5600583695834,
16.4796463598313));
#155915=CARTESIAN_POINT('Ctrl Pts',(-17.7404308047433,-16.5910693792692,
16.4839625225702));
#155916=CARTESIAN_POINT('Ctrl Pts',(-17.6607319577165,-16.6262200532081,
16.4882786853091));
#155917=CARTESIAN_POINT('Ctrl Pts',(-17.5830833500453,-16.6653013174323,
16.492594848048));
#155918=CARTESIAN_POINT('Ctrl Pts',(-17.5079641376018,-16.703109513585,
16.4967704122397));
#155919=CARTESIAN_POINT('Ctrl Pts',(-17.4347640291965,-16.7445958812711,
16.5009459764314));
#155920=CARTESIAN_POINT('Ctrl Pts',(-17.3638528381206,-16.7895253169588,
16.5051215406231));
#155921=CARTESIAN_POINT('Ctrl Pts',(-17.2893600913589,-16.8367240316336,
16.5095080026356));
#155922=CARTESIAN_POINT('Ctrl Pts',(-17.2173940414895,-16.8877224362901,
16.5138944646482));
#155923=CARTESIAN_POINT('Ctrl Pts',(-17.1483451005787,-16.9421993780623,
16.5182809266607));
#155924=CARTESIAN_POINT('Ctrl Pts',(-17.0792961596678,-16.9966763198346,
16.5226673886732));
#155925=CARTESIAN_POINT('Ctrl Pts',(-17.0131647139456,-17.0546313591046,
16.5270538506858));
#155926=CARTESIAN_POINT('Ctrl Pts',(-16.9502957329766,-17.115699619397,
16.5314403126983));
#155927=CARTESIAN_POINT('Ctrl Pts',(-16.8903194470162,-17.1739580385086,
16.5356249470914));
#155928=CARTESIAN_POINT('Ctrl Pts',(-16.8330887583091,-17.2352663353223,
16.5398095814844));
#155929=CARTESIAN_POINT('Ctrl Pts',(-16.7789298175348,-17.2993353087708,
16.5439942158775));
#155930=CARTESIAN_POINT('Ctrl Pts',(-16.7248479653093,-17.3633130879657,
16.5481728939614));
#155931=CARTESIAN_POINT('Ctrl Pts',(-16.6738294707906,-17.4300433902867,
16.5523515720454));
#155932=CARTESIAN_POINT('Ctrl Pts',(-16.6261644175018,-17.4991995466842,
16.5565302501293));
#155933=CARTESIAN_POINT('Ctrl Pts',(-16.577645002389,-17.5695952774835,
16.5607838280147));
#155934=CARTESIAN_POINT('Ctrl Pts',(-16.5326007777018,-17.6425043486949,
16.5650374059002));
#155935=CARTESIAN_POINT('Ctrl Pts',(-16.4912954660574,-17.7175461234078,
16.5692909837856));
#155936=CARTESIAN_POINT('Ctrl Pts',(-16.45079093848,-17.791133066886,16.5734620977636));
#155937=CARTESIAN_POINT('Ctrl Pts',(-16.4138818774499,-17.8667703369927,
16.5776332117415));
#155938=CARTESIAN_POINT('Ctrl Pts',(-16.3807728287042,-17.9440704983605,
16.5818043257195));
#155939=CARTESIAN_POINT('Ctrl Pts',(-16.3476748900196,-18.0213447209125,
16.5859740400399));
#155940=CARTESIAN_POINT('Ctrl Pts',(-16.318374612164,-18.1002803040064,
16.5901437543602));
#155941=CARTESIAN_POINT('Ctrl Pts',(-16.2930292165598,-18.1804679952255,
16.5943134686806));
#155942=CARTESIAN_POINT('Ctrl Pts',(-16.2676847228536,-18.2606528330224,
16.5984830346246));
#155943=CARTESIAN_POINT('Ctrl Pts',(-16.2462949694201,-18.3420892514569,
16.6026526005687));
#155944=CARTESIAN_POINT('Ctrl Pts',(-16.2289674972205,-18.4243522386873,
16.6068221665127));
#155945=CARTESIAN_POINT('Ctrl Pts',(-16.2110308124741,-18.5095074910663,
16.6111383292517));
#155946=CARTESIAN_POINT('Ctrl Pts',(-16.1974474922546,-18.5955480019176,
16.6154544919906));
#155947=CARTESIAN_POINT('Ctrl Pts',(-16.1882789321129,-18.6819921399002,
16.6197706547295));
#155948=CARTESIAN_POINT('Ctrl Pts',(-16.1794090368535,-18.7656203691804,
16.6239462189212));
#155949=CARTESIAN_POINT('Ctrl Pts',(-16.1746706763875,-18.8496258601583,
16.6281217831129));
#155950=CARTESIAN_POINT('Ctrl Pts',(-16.1740663387713,-18.9335704012975,
16.6322973473045));
#155951=CARTESIAN_POINT('Ctrl Pts',(-16.1734314774988,-19.0217547816503,
16.6366838093171));
#155952=CARTESIAN_POINT('Ctrl Pts',(-16.1773592072922,-19.1098713098955,
16.6410702713296));
#155953=CARTESIAN_POINT('Ctrl Pts',(-16.1857908120614,-19.1974178773141,
16.6454567333422));
#155954=CARTESIAN_POINT('Ctrl Pts',(-16.1942224168306,-19.2849644447327,
16.6498431953547));
#155955=CARTESIAN_POINT('Ctrl Pts',(-16.2071577359856,-19.3719404886095,
16.6542296573672));
#155956=CARTESIAN_POINT('Ctrl Pts',(-16.2244766916358,-19.4578584434176,
16.6586161193798));
#155957=CARTESIAN_POINT('Ctrl Pts',(-16.2409948213726,-19.539803564873,
16.6627997520463));
#155958=CARTESIAN_POINT('Ctrl Pts',(-16.2615616142029,-19.6210912295922,
16.6669833847129));
#155959=CARTESIAN_POINT('Ctrl Pts',(-16.2861104910148,-19.7012909660474,
16.6711670173794));
#155960=CARTESIAN_POINT('Ctrl Pts',(-16.3106270618244,-19.7813851606933,
16.6753451444398));
#155961=CARTESIAN_POINT('Ctrl Pts',(-16.339115179781,-19.8603938336953,
16.6795232715002));
#155962=CARTESIAN_POINT('Ctrl Pts',(-16.3714572466738,-19.9378964137807,
16.6837013985606));
#155963=CARTESIAN_POINT('Ctrl Pts',(-16.4037664575643,-20.0153202597224,
16.6878752811009));
#155964=CARTESIAN_POINT('Ctrl Pts',(-16.4399216659544,-20.0912406291382,
16.6920491636412));
#155965=CARTESIAN_POINT('Ctrl Pts',(-16.4797558270926,-20.1652531512068,
16.6962230461816));
#155966=CARTESIAN_POINT('Ctrl Pts',(-16.5195614728711,-20.2392126912711,
16.7003939408402));
#155967=CARTESIAN_POINT('Ctrl Pts',(-16.563040621407,-20.3112666936583,
16.7045648354988));
#155968=CARTESIAN_POINT('Ctrl Pts',(-16.6099791482511,-20.3810330371743,
16.7087357301574));
#155969=CARTESIAN_POINT('Ctrl Pts',(-16.656906125228,-20.4507822137264,
16.7129055985102));
#155970=CARTESIAN_POINT('Ctrl Pts',(-16.707290538528,-20.5182444646104,
16.7170754668631));
#155971=CARTESIAN_POINT('Ctrl Pts',(-16.7608741705717,-20.5830654374497,
16.721245335216));
#155972=CARTESIAN_POINT('Ctrl Pts',(-16.814450725416,-20.6478778488882,
16.7254146528225));
#155973=CARTESIAN_POINT('Ctrl Pts',(-16.8712253612539,-20.7100493251438,
16.729583970429));
#155974=CARTESIAN_POINT('Ctrl Pts',(-16.9308997149153,-20.7692587493055,
16.7337532880356));
#155975=CARTESIAN_POINT('Ctrl Pts',(-16.9906010255816,-20.8284949204471,
16.7379244890695));
#155976=CARTESIAN_POINT('Ctrl Pts',(-17.0532043371944,-20.8847660495707,
16.7420956901035));
#155977=CARTESIAN_POINT('Ctrl Pts',(-17.1183753222518,-20.9377887351506,
16.7462668911375));
#155978=CARTESIAN_POINT('Ctrl Pts',(-17.1368677583985,-20.9528340597924,
16.7474504802563));
#155979=CARTESIAN_POINT('Ctrl Pts',(-17.1555667305739,-20.9676180851866,
16.7486340693751));
#155980=CARTESIAN_POINT('Ctrl Pts',(-17.1744641402402,-20.9821349467765,
16.7498176584939));
#155981=CARTESIAN_POINT('Ctrl Pts',(-17.1744641402401,-20.9821349467765,
15.9499155181261));
#155982=CARTESIAN_POINT('Ctrl Pts',(-17.2411396316843,-21.0333546058634,
15.9540850492628));
#155983=CARTESIAN_POINT('Ctrl Pts',(-17.3103587055251,-21.0812996420495,
15.9582545803995));
#155984=CARTESIAN_POINT('Ctrl Pts',(-17.3817621512649,-21.1257186571514,
15.9624241115362));
#155985=CARTESIAN_POINT('Ctrl Pts',(-17.4531698880323,-21.1701403416375,
15.9665938932431));
#155986=CARTESIAN_POINT('Ctrl Pts',(-17.5267618660371,-21.2110353423976,
15.97076367495));
#155987=CARTESIAN_POINT('Ctrl Pts',(-17.6021516704121,-21.2481967160522,
15.9749334566569));
#155988=CARTESIAN_POINT('Ctrl Pts',(-17.6776196576944,-21.2853966278654,
15.979107562631));
#155989=CARTESIAN_POINT('Ctrl Pts',(-17.7548887811624,-21.3188549763378,
15.983281668605));
#155990=CARTESIAN_POINT('Ctrl Pts',(-17.8335503409496,-21.3484119870164,
15.9874557745791));
#155991=CARTESIAN_POINT('Ctrl Pts',(-17.9122533278425,-21.377984563893,
15.9916320788458));
#155992=CARTESIAN_POINT('Ctrl Pts',(-17.9923497730624,-21.4036515707366,
15.9958083831126));
#155993=CARTESIAN_POINT('Ctrl Pts',(-18.0734157506516,-21.4253031454945,
15.9999846873793));
#155994=CARTESIAN_POINT('Ctrl Pts',(-18.1546240863822,-21.4469927420961,
16.0041683255601));
#155995=CARTESIAN_POINT('Ctrl Pts',(-18.2368049051917,-21.4646527238166,
16.0083519637409));
#155996=CARTESIAN_POINT('Ctrl Pts',(-18.3195242010686,-21.478224418396,
16.0125356019217));
#155997=CARTESIAN_POINT('Ctrl Pts',(-18.3867591085121,-21.4892556006519,
16.0159360966053));
#155998=CARTESIAN_POINT('Ctrl Pts',(-18.4543495129699,-21.4975868065142,
16.019336591289));
#155999=CARTESIAN_POINT('Ctrl Pts',(-18.5220617179685,-21.5032119011579,
16.0227370859726));
#156000=CARTESIAN_POINT('Ctrl Pts',(-18.605388071405,-21.5101341188644,
16.0269217203656));
#156001=CARTESIAN_POINT('Ctrl Pts',(-18.6892089831259,-21.5129825827272,
16.0311063547587));
#156002=CARTESIAN_POINT('Ctrl Pts',(-18.7730921344112,-21.5117015070174,
16.0352909891517));
#156003=CARTESIAN_POINT('Ctrl Pts',(-18.8568558884132,-21.5104222547604,
16.0394696672357));
#156004=CARTESIAN_POINT('Ctrl Pts',(-18.9406812499664,-21.5050251452316,
16.0436483453196));
#156005=CARTESIAN_POINT('Ctrl Pts',(-19.0241313606306,-21.4955062008139,
16.0478270234036));
#156006=CARTESIAN_POINT('Ctrl Pts',(-19.1090772545539,-21.4858166361586,
16.052080601289));
#156007=CARTESIAN_POINT('Ctrl Pts',(-19.1936338320392,-21.471855975481,
16.0563341791744));
#156008=CARTESIAN_POINT('Ctrl Pts',(-19.2773408795586,-21.453675576209,
16.0605877570599));
#156009=CARTESIAN_POINT('Ctrl Pts',(-19.359425102621,-21.435847639453,16.0647588710378));
#156010=CARTESIAN_POINT('Ctrl Pts',(-19.4406919711073,-21.4139622218931,
16.0689299850158));
#156011=CARTESIAN_POINT('Ctrl Pts',(-19.5207150357481,-21.3881197533225,
16.0731010989937));
#156012=CARTESIAN_POINT('Ctrl Pts',(-19.6007112478768,-21.3622859564417,
16.0772708133141));
#156013=CARTESIAN_POINT('Ctrl Pts',(-19.6794640476569,-21.3324978868904,
16.0814405276345));
#156014=CARTESIAN_POINT('Ctrl Pts',(-19.7565616407639,-21.2989059825307,
16.0856102419549));
#156015=CARTESIAN_POINT('Ctrl Pts',(-19.8336564904078,-21.265315273515,
16.0897798078989));
#156016=CARTESIAN_POINT('Ctrl Pts',(-19.9090958290862,-21.2279211833509,
16.093949373843));
#156017=CARTESIAN_POINT('Ctrl Pts',(-19.9824886317286,-21.1869219530991,
16.0981189397871));
#156018=CARTESIAN_POINT('Ctrl Pts',(-20.0584618347717,-21.14448124049,16.102435102526));
#156019=CARTESIAN_POINT('Ctrl Pts',(-20.1322414512882,-21.0981774147041,
16.1067512652649));
#156020=CARTESIAN_POINT('Ctrl Pts',(-20.203424104004,-21.0482807070076,
16.1110674280038));
#156021=CARTESIAN_POINT('Ctrl Pts',(-20.2722879892948,-21.0000093793159,
16.1152429921955));
#156022=CARTESIAN_POINT('Ctrl Pts',(-20.3387211617825,-20.9483759776501,
16.1194185563872));
#156023=CARTESIAN_POINT('Ctrl Pts',(-20.4023916835437,-20.8936666012171,
16.1235941205789));
#156024=CARTESIAN_POINT('Ctrl Pts',(-20.4692780519966,-20.83619398424,16.1279805825914));
#156025=CARTESIAN_POINT('Ctrl Pts',(-20.5331149297317,-20.7753268941806,
16.1323670446039));
#156026=CARTESIAN_POINT('Ctrl Pts',(-20.5935624370348,-20.7114395535991,
16.1367535066165));
#156027=CARTESIAN_POINT('Ctrl Pts',(-20.6540099443379,-20.6475522130177,
16.141139968629));
#156028=CARTESIAN_POINT('Ctrl Pts',(-20.7110677625944,-20.5806451127527,
16.1455264306415));
#156029=CARTESIAN_POINT('Ctrl Pts',(-20.764447298501,-20.5111291697643,
16.149912892654));
#156030=CARTESIAN_POINT('Ctrl Pts',(-20.8154455601759,-20.4447143500982,
16.1541036735168));
#156031=CARTESIAN_POINT('Ctrl Pts',(-20.8632791399794,-20.3756679864259,
16.1582944543796));
#156032=CARTESIAN_POINT('Ctrl Pts',(-20.9076654294935,-20.3043234082959,
16.1624852352424));
#156033=CARTESIAN_POINT('Ctrl Pts',(-20.9519891627481,-20.233079380358,
16.1666701097864));
#156034=CARTESIAN_POINT('Ctrl Pts',(-20.9928750133147,-20.1595439541276,
16.1708549843304));
#156035=CARTESIAN_POINT('Ctrl Pts',(-21.0300812471761,-20.0840825528053,
16.1750398588744));
#156036=CARTESIAN_POINT('Ctrl Pts',(-21.0672460755937,-20.0087051296902,
16.1792200762261));
#156037=CARTESIAN_POINT('Ctrl Pts',(-21.1007392197538,-19.9314063968234,
16.1834002935778));
#156038=CARTESIAN_POINT('Ctrl Pts',(-21.1303635397436,-19.8525785836825,
16.1875805109294));
#156039=CARTESIAN_POINT('Ctrl Pts',(-21.159964013956,-19.7738142221411,
16.1917573634601));
#156040=CARTESIAN_POINT('Ctrl Pts',(-21.1857016914125,-19.6935236530682,
16.1959342159908));
#156041=CARTESIAN_POINT('Ctrl Pts',(-21.2074270380285,-19.6121202068937,
16.2001110685216));
#156042=CARTESIAN_POINT('Ctrl Pts',(-21.2291418983467,-19.5307560521882,
16.2042859049869));
#156043=CARTESIAN_POINT('Ctrl Pts',(-21.2468481598046,-19.4482805298198,
16.2084607414522));
#156044=CARTESIAN_POINT('Ctrl Pts',(-21.2604461548152,-19.3651220483335,
16.2126355779175));
#156045=CARTESIAN_POINT('Ctrl Pts',(-21.2740449836494,-19.2819584676034,
16.216810670382));
#156046=CARTESIAN_POINT('Ctrl Pts',(-21.2835349604933,-19.1981122945302,
16.2209857628466));
#156047=CARTESIAN_POINT('Ctrl Pts',(-21.2888677421722,-19.1140210480402,
16.2251608553111));
#156048=CARTESIAN_POINT('Ctrl Pts',(-21.2923288662564,-19.0594434830793,
16.2278706067979));
#156049=CARTESIAN_POINT('Ctrl Pts',(-21.2940398771788,-19.0047628516758,
16.2305803582847));
#156050=CARTESIAN_POINT('Ctrl Pts',(-21.293999294499,-18.9500994304893,
16.2332901097715));
#156051=CARTESIAN_POINT('',(-21.2939994369002,-18.9536979607663,16.1667098902285));
#156052=CARTESIAN_POINT('Ctrl Pts',(-17.172599330006,-20.9845253206546,
15.883228700071));
#156053=CARTESIAN_POINT('Ctrl Pts',(-17.2449841511746,-21.0410309575293,
15.8878110784405));
#156054=CARTESIAN_POINT('Ctrl Pts',(-18.0187464880494,-21.577913384796,
15.9347853923704));
#156055=CARTESIAN_POINT('Ctrl Pts',(-20.0538051259393,-21.6762256253679,
16.0241516418607));
#156056=CARTESIAN_POINT('Ctrl Pts',(-21.2452320241039,-20.0081650284355,
16.1140629935438));
#156057=CARTESIAN_POINT('Ctrl Pts',(-21.2975539525536,-19.0564768252052,
16.1615824096664));
#156058=CARTESIAN_POINT('Ctrl Pts',(-21.2967673506771,-18.9536997966296,
16.1667098902285));
#156059=CARTESIAN_POINT('Ctrl Pts',(-21.2939994369002,-18.9536979607663,
16.1667098902285));
#156060=CARTESIAN_POINT('Ctrl Pts',(-21.2940542005915,-18.8711312597184,
16.1708335669039));
#156061=CARTESIAN_POINT('Ctrl Pts',(-21.2901102644712,-18.7884072256502,
16.1749572435793));
#156062=CARTESIAN_POINT('Ctrl Pts',(-21.282148407848,-18.7059518510906,
16.1790809202548));
#156063=CARTESIAN_POINT('Ctrl Pts',(-21.274150019936,-18.6231181475505,
16.1832235175451));
#156064=CARTESIAN_POINT('Ctrl Pts',(-21.2620966823449,-18.5405560554535,
16.1873661148355));
#156065=CARTESIAN_POINT('Ctrl Pts',(-21.2460219433306,-18.45869912201,16.1915087121259));
#156066=CARTESIAN_POINT('Ctrl Pts',(-21.2300543085101,-18.3773875921873,
16.1956237077524));
#156067=CARTESIAN_POINT('Ctrl Pts',(-21.2101187777555,-18.2967723256484,
16.1997387033789));
#156068=CARTESIAN_POINT('Ctrl Pts',(-21.1863001253011,-18.2172727748014,
16.2038536990054));
#156069=CARTESIAN_POINT('Ctrl Pts',(-21.1624916905598,-18.1378073276301,
16.2079669293832));
#156070=CARTESIAN_POINT('Ctrl Pts',(-21.1348035753301,-18.0594570997617,
16.2120801597611));
#156071=CARTESIAN_POINT('Ctrl Pts',(-21.1033710027997,-17.9826285278121,
16.2161933901389));
#156072=CARTESIAN_POINT('Ctrl Pts',(-21.0719418753926,-17.9058083765509,
16.2203061696918));
#156073=CARTESIAN_POINT('Ctrl Pts',(-21.0367692860286,-17.830509988201,
16.2244189492448));
#156074=CARTESIAN_POINT('Ctrl Pts',(-20.998036835518,-17.757120421374,16.2285317287978));
#156075=CARTESIAN_POINT('Ctrl Pts',(-20.9588192445656,-17.68281161896,16.2326960226666));
#156076=CARTESIAN_POINT('Ctrl Pts',(-20.9159522062818,-17.610460238745,
16.2368603165354));
#156077=CARTESIAN_POINT('Ctrl Pts',(-20.8696736494984,-17.5404412648287,
16.2410246104042));
#156078=CARTESIAN_POINT('Ctrl Pts',(-20.8239074514183,-17.4711974842889,
16.2451428005836));
#156079=CARTESIAN_POINT('Ctrl Pts',(-20.7748052350545,-17.4042350697679,
16.2492609907631));
#156080=CARTESIAN_POINT('Ctrl Pts',(-20.7226388747277,-17.3398847975651,
16.2533791809425));
#156081=CARTESIAN_POINT('Ctrl Pts',(-20.6695965003384,-17.2744539105173,
16.257566526656));
#156082=CARTESIAN_POINT('Ctrl Pts',(-20.6133864683218,-17.2117240820488,
16.2617538723695));
#156083=CARTESIAN_POINT('Ctrl Pts',(-20.5543334369044,-17.152003839313,
16.265941218083));
#156084=CARTESIAN_POINT('Ctrl Pts',(-20.495280405487,-17.0922835965773,
16.2701285637965));
#156085=CARTESIAN_POINT('Ctrl Pts',(-20.4333847973435,-17.0355732283015,
16.27431590951));
#156086=CARTESIAN_POINT('Ctrl Pts',(-20.369004471075,-16.9821369642625,
16.2785032552236));
#156087=CARTESIAN_POINT('Ctrl Pts',(-20.3046658312848,-16.9287353003847,
16.2826878896166));
#156088=CARTESIAN_POINT('Ctrl Pts',(-20.2375884427954,-16.8783896656033,
16.2868725240096));
#156089=CARTESIAN_POINT('Ctrl Pts',(-20.1680947292198,-16.8313934104545,
16.2910571584027));
#156090=CARTESIAN_POINT('Ctrl Pts',(-20.0986999313439,-16.7844640486578,
16.2952358364866));
#156091=CARTESIAN_POINT('Ctrl Pts',(-20.0268960178072,-16.740874852386,
16.2994145145706));
#156092=CARTESIAN_POINT('Ctrl Pts',(-19.9530388079927,-16.7008793047445,
16.3035931926545));
#156093=CARTESIAN_POINT('Ctrl Pts',(-19.8778577607726,-16.6601668656558,
16.30784677054));
#156094=CARTESIAN_POINT('Ctrl Pts',(-19.8005494535676,-16.623178482619,
16.3121003484254));
#156095=CARTESIAN_POINT('Ctrl Pts',(-19.7215205448425,-16.5901356572584,
16.3163539263108));
#156096=CARTESIAN_POINT('Ctrl Pts',(-19.6440237657252,-16.5577334315452,
16.3205250402888));
#156097=CARTESIAN_POINT('Ctrl Pts',(-19.5648729481497,-16.5291253296777,
16.3246961542668));
#156098=CARTESIAN_POINT('Ctrl Pts',(-19.4844751811847,-16.5044732887207,
16.3288672682447));
#156099=CARTESIAN_POINT('Ctrl Pts',(-19.4041043924667,-16.479829519994,
16.3330369825651));
#156100=CARTESIAN_POINT('Ctrl Pts',(-19.322487924815,-16.4591393105012,
16.3372066968855));
#156101=CARTESIAN_POINT('Ctrl Pts',(-19.2400494979666,-16.4425152111225,
16.3413764112058));
#156102=CARTESIAN_POINT('Ctrl Pts',(-19.1576140046313,-16.4258917033005,
16.3455459771499));
#156103=CARTESIAN_POINT('Ctrl Pts',(-19.0743570613773,-16.4133341080143,
16.3497155430939));
#156104=CARTESIAN_POINT('Ctrl Pts',(-18.9907127437434,-16.4049038951779,
16.353885109038));
#156105=CARTESIAN_POINT('Ctrl Pts',(-18.9041275950881,-16.396177286458,
16.3582012717769));
#156106=CARTESIAN_POINT('Ctrl Pts',(-18.8171278498229,-16.3918737507556,
16.3625174345158));
#156107=CARTESIAN_POINT('Ctrl Pts',(-18.7301989430813,-16.3920028218831,
16.3668335972547));
#156108=CARTESIAN_POINT('Ctrl Pts',(-18.6461017363336,-16.3921276885323,
16.3710091614464));
#156109=CARTESIAN_POINT('Ctrl Pts',(-18.5620712918894,-16.3964007414036,
16.3751847256381));
#156110=CARTESIAN_POINT('Ctrl Pts',(-18.4785435740566,-16.4047775883437,
16.3793602898298));
#156111=CARTESIAN_POINT('Ctrl Pts',(-18.3907970697643,-16.4135775299086,
16.3837467518423));
#156112=CARTESIAN_POINT('Ctrl Pts',(-18.3036059893689,-16.42690663756,16.3881332138549));
#156113=CARTESIAN_POINT('Ctrl Pts',(-18.2174632822103,-16.4446528323395,
16.3925196758674));
#156114=CARTESIAN_POINT('Ctrl Pts',(-18.1313205750517,-16.4623990271191,
16.3969061378799));
#156115=CARTESIAN_POINT('Ctrl Pts',(-18.0462267834429,-16.4845620891763,
16.4012925998925));
#156116=CARTESIAN_POINT('Ctrl Pts',(-17.9626538344087,-16.510970485056,
16.405679061905));
#156117=CARTESIAN_POINT('Ctrl Pts',(-17.8829262006443,-16.5361637914947,
16.4098636962981));
#156118=CARTESIAN_POINT('Ctrl Pts',(-17.8042857709966,-16.5653141227608,
16.4140483306911));
#156119=CARTESIAN_POINT('Ctrl Pts',(-17.7271537286292,-16.5983091567016,
16.4182329650842));
#156120=CARTESIAN_POINT('Ctrl Pts',(-17.6501314741771,-16.6312572262956,
16.4224116431681));
#156121=CARTESIAN_POINT('Ctrl Pts',(-17.5746137617239,-16.6680389491568,
16.426590321252));
#156122=CARTESIAN_POINT('Ctrl Pts',(-17.5010063287304,-16.708492343091,
16.430768999336));
#156123=CARTESIAN_POINT('Ctrl Pts',(-17.4260795354011,-16.7496708350382,
16.4350225772214));
#156124=CARTESIAN_POINT('Ctrl Pts',(-17.3531326383836,-16.7946537768951,
16.4392761551069));
#156125=CARTESIAN_POINT('Ctrl Pts',(-17.2825720020047,-16.8432191278762,
16.4435297329923));
#156126=CARTESIAN_POINT('Ctrl Pts',(-17.2133793212498,-16.8908429447609,
16.4477008469703));
#156127=CARTESIAN_POINT('Ctrl Pts',(-17.1464815985698,-16.9419112335081,
16.4518719609482));
#156128=CARTESIAN_POINT('Ctrl Pts',(-17.082235347001,-16.9961693500962,
16.4560430749262));
#156129=CARTESIAN_POINT('Ctrl Pts',(-17.0180106538824,-17.0504092598493,
16.4602127892466));
#156130=CARTESIAN_POINT('Ctrl Pts',(-16.9564360160344,-17.1078365750808,
16.4643825035669));
#156131=CARTESIAN_POINT('Ctrl Pts',(-16.897835422393,-17.1681559362037,
16.4685522178873));
#156132=CARTESIAN_POINT('Ctrl Pts',(-16.8392369140123,-17.2284731509048,
16.4727217838314));
#156133=CARTESIAN_POINT('Ctrl Pts',(-16.7836125593685,-17.2916818763298,
16.4768913497754));
#156134=CARTESIAN_POINT('Ctrl Pts',(-16.731249001788,-17.3574503961429,
16.4810609157195));
#156135=CARTESIAN_POINT('Ctrl Pts',(-16.6770444061204,-17.4255312559784,
16.4853770784584));
#156136=CARTESIAN_POINT('Ctrl Pts',(-16.6263345016126,-17.4963548514855,
16.4896932411973));
#156137=CARTESIAN_POINT('Ctrl Pts',(-16.5793900615229,-17.5695181690106,
16.4940094039362));
#156138=CARTESIAN_POINT('Ctrl Pts',(-16.5339748316314,-17.6402981991629,
16.4981849681279));
#156139=CARTESIAN_POINT('Ctrl Pts',(-16.4920837070567,-17.7132674273088,
16.5023605323196));
#156140=CARTESIAN_POINT('Ctrl Pts',(-16.453915340234,-17.7880352478275,
16.5065360965113));
#156141=CARTESIAN_POINT('Ctrl Pts',(-16.41381917994,-17.8665794132169,16.5109225585238));
#156142=CARTESIAN_POINT('Ctrl Pts',(-16.3778319719893,-17.9471081067069,
16.5153090205363));
#156143=CARTESIAN_POINT('Ctrl Pts',(-16.3461262998435,-18.0291461696993,
16.5196954825489));
#156144=CARTESIAN_POINT('Ctrl Pts',(-16.3144206276976,-18.1111842326916,
16.5240819445614));
#156145=CARTESIAN_POINT('Ctrl Pts',(-16.2869966000408,-18.1947310901858,
16.5284684065739));
#156146=CARTESIAN_POINT('Ctrl Pts',(-16.2639654295305,-18.2792970784325,
16.5328548685865));
#156147=CARTESIAN_POINT('Ctrl Pts',(-16.2419939573157,-18.3599720602031,
16.5370395029795));
#156148=CARTESIAN_POINT('Ctrl Pts',(-16.223938199736,-18.4418747378536,
16.5412241373726));
#156149=CARTESIAN_POINT('Ctrl Pts',(-16.2099316900943,-18.5245901651461,
16.5454087717656));
#156150=CARTESIAN_POINT('Ctrl Pts',(-16.1959451169854,-18.607187857266,
16.5495874498496));
#156151=CARTESIAN_POINT('Ctrl Pts',(-16.1859964196337,-18.6905955514663,
16.5537661279335));
#156152=CARTESIAN_POINT('Ctrl Pts',(-16.18016901464,-18.7743844088623,16.5579448060175));
#156153=CARTESIAN_POINT('Ctrl Pts',(-16.1742371575999,-18.8596751213092,
16.5621983839029));
#156154=CARTESIAN_POINT('Ctrl Pts',(-16.1725759211884,-18.9453603308624,
16.5664519617883));
#156155=CARTESIAN_POINT('Ctrl Pts',(-16.1752185615464,-19.0309781629655,
16.5707055396738));
#156156=CARTESIAN_POINT('Ctrl Pts',(-16.1778099691644,-19.1149361263239,
16.5748766536517));
#156157=CARTESIAN_POINT('Ctrl Pts',(-16.1845398497979,-19.1988288204158,
16.5790477676297));
#156158=CARTESIAN_POINT('Ctrl Pts',(-16.1953870618677,-19.2822186402179,
16.5832188816076));
#156159=CARTESIAN_POINT('Ctrl Pts',(-16.2062306340508,-19.3655804777606,
16.587388595928));
#156160=CARTESIAN_POINT('Ctrl Pts',(-16.221188734479,-19.4484393203326,
16.5915583102484));
#156161=CARTESIAN_POINT('Ctrl Pts',(-16.2401883815476,-19.5303628719685,
16.5957280245687));
#156162=CARTESIAN_POINT('Ctrl Pts',(-16.2591873525271,-19.6122835084129,
16.5998975905128));
#156163=CARTESIAN_POINT('Ctrl Pts',(-16.2822274794425,-19.6932684721474,
16.6040671564568));
#156164=CARTESIAN_POINT('Ctrl Pts',(-16.3091849959464,-19.7728971897362,
16.6082367224009));
#156165=CARTESIAN_POINT('Ctrl Pts',(-16.337090305475,-19.8553255548027,
16.6125528851398));
#156166=CARTESIAN_POINT('Ctrl Pts',(-16.3691934316988,-19.9363000284497,
16.6168690478787));
#156167=CARTESIAN_POINT('Ctrl Pts',(-16.4053020683426,-20.0153747895708,
16.6211852106176));
#156168=CARTESIAN_POINT('Ctrl Pts',(-16.4402344699458,-20.0918736986655,
16.6253607748093));
#156169=CARTESIAN_POINT('Ctrl Pts',(-16.4789151719814,-20.1665943642432,
16.629536339001));
#156170=CARTESIAN_POINT('Ctrl Pts',(-16.5211232637327,-20.2391583236289,
16.6337119031927));
#156171=CARTESIAN_POINT('Ctrl Pts',(-16.5654631858582,-20.3153873160987,
16.6380983652052));
#156172=CARTESIAN_POINT('Ctrl Pts',(-16.613695880029,-20.3892355173248,
16.6424848272177));
#156173=CARTESIAN_POINT('Ctrl Pts',(-16.6655152292138,-20.460300617591,
16.6468712892303));
#156174=CARTESIAN_POINT('Ctrl Pts',(-16.7173345783985,-20.5313657178572,
16.6512577512428));
#156175=CARTESIAN_POINT('Ctrl Pts',(-16.7727401579416,-20.5996473145404,
16.6556442132554));
#156176=CARTESIAN_POINT('Ctrl Pts',(-16.8313804354228,-20.664786849695,
16.6600306752679));
#156177=CARTESIAN_POINT('Ctrl Pts',(-16.8873083679682,-20.7269134235218,
16.6642142460504));
#156178=CARTESIAN_POINT('Ctrl Pts',(-16.9463864967696,-20.7864133665619,
16.668397816833));
#156179=CARTESIAN_POINT('Ctrl Pts',(-17.0083384129404,-20.8429500487709,
16.6725813876155));
#156180=CARTESIAN_POINT('Ctrl Pts',(-17.0616528481945,-20.8916042546362,
16.6761816751837));
#156181=CARTESIAN_POINT('Ctrl Pts',(-17.1170947828409,-20.9380641965746,
16.679781962752));
#156182=CARTESIAN_POINT('Ctrl Pts',(-17.1744641402401,-20.9821349467765,
16.6833822503202));
#156183=CARTESIAN_POINT('Origin',(-18.734,-18.952,-1.76670989022851));
#156184=CARTESIAN_POINT('',(-17.1718942801479,-20.9854857634355,17.5498940685532));
#156185=CARTESIAN_POINT('',(-17.1769969312964,-20.9788274605145,17.483325298233));
#156186=CARTESIAN_POINT('',(-17.1744641402401,-20.9821349467765,-1.76670989022851));
#156187=CARTESIAN_POINT('',(-21.2942629985695,-18.9511644346814,17.0332901097715));
#156188=CARTESIAN_POINT('Ctrl Pts',(-21.2979001731334,-18.9511632476561,
17.0332901097715));
#156189=CARTESIAN_POINT('Ctrl Pts',(-21.2980948808476,-18.9054257555603,
17.0355745863224));
#156190=CARTESIAN_POINT('Ctrl Pts',(-21.2762380388006,-18.0111494605167,
17.0802509984337));
#156191=CARTESIAN_POINT('Ctrl Pts',(-20.2331955662249,-16.3222274596702,
17.1673193461055));
#156192=CARTESIAN_POINT('Ctrl Pts',(-17.3342635896144,-16.2679677831473,
17.2944951527869));
#156193=CARTESIAN_POINT('Ctrl Pts',(-15.7195028920934,-18.6761410757601,
17.4216709594684));
#156194=CARTESIAN_POINT('Ctrl Pts',(-16.4898975455887,-20.4576174486145,
17.5068039313905));
#156195=CARTESIAN_POINT('Ctrl Pts',(-17.1663500614582,-20.9812337393009,
17.5495449677521));
#156196=CARTESIAN_POINT('Ctrl Pts',(-17.1718942801479,-20.9854857634355,
17.5498940685532));
#156197=CARTESIAN_POINT('Ctrl Pts',(-17.1744641402402,-20.9821349467765,
16.7498176584939));
#156198=CARTESIAN_POINT('Ctrl Pts',(-17.2411413997508,-21.03335596408,16.7539938117457));
#156199=CARTESIAN_POINT('Ctrl Pts',(-17.3102910949476,-21.0812474621041,
16.7581699649975));
#156200=CARTESIAN_POINT('Ctrl Pts',(-17.3815399059492,-21.1255803859071,
16.7623461182494));
#156201=CARTESIAN_POINT('Ctrl Pts',(-17.452915090555,-21.1699919427608,
16.7665296787201));
#156202=CARTESIAN_POINT('Ctrl Pts',(-17.5263964265398,-21.2108320914119,
16.7707132391908));
#156203=CARTESIAN_POINT('Ctrl Pts',(-17.6015859266022,-21.2479177612386,
16.7748967996615));
#156204=CARTESIAN_POINT('Ctrl Pts',(-17.6668572118987,-21.2801114762341,
16.7785285084614));
#156205=CARTESIAN_POINT('Ctrl Pts',(-17.7334152100966,-21.3094765764609,
16.7821602172613));
#156206=CARTESIAN_POINT('Ctrl Pts',(-17.8009895271371,-21.3359235427186,
16.7857919260613));
#156207=CARTESIAN_POINT('Ctrl Pts',(-17.8788519954,-21.3663970445028,16.7899765604543));
#156208=CARTESIAN_POINT('Ctrl Pts',(-17.9583538968788,-21.3931085897472,
16.7941611948473));
#156209=CARTESIAN_POINT('Ctrl Pts',(-18.0390969463692,-21.4158810332592,
16.7983458292404));
#156210=CARTESIAN_POINT('Ctrl Pts',(-18.1197250681227,-21.4386210630166,
16.8025245073243));
#156211=CARTESIAN_POINT('Ctrl Pts',(-18.2015903898501,-21.4574330041517,
16.8067031854083));
#156212=CARTESIAN_POINT('Ctrl Pts',(-18.2842754534887,-21.4721880549406,
16.8108818634922));
#156213=CARTESIAN_POINT('Ctrl Pts',(-18.3684425874682,-21.4872075794106,
16.8151354413777));
#156214=CARTESIAN_POINT('Ctrl Pts',(-18.4534586911853,-21.49802316776,16.8193890192631));
#156215=CARTESIAN_POINT('Ctrl Pts',(-18.538868095807,-21.5045523579284,
16.8236425971485));
#156216=CARTESIAN_POINT('Ctrl Pts',(-18.6226216724574,-21.5109549670048,
16.8278137111265));
#156217=CARTESIAN_POINT('Ctrl Pts',(-18.7067529564692,-21.5132358584627,
16.8319848251044));
#156218=CARTESIAN_POINT('Ctrl Pts',(-18.7908245916082,-21.5113692515517,
16.8361559390824));
#156219=CARTESIAN_POINT('Ctrl Pts',(-18.8748680156982,-21.5095032709988,
16.8403256534027));
#156220=CARTESIAN_POINT('Ctrl Pts',(-18.9588513711302,-21.503492566284,
16.8444953677231));
#156221=CARTESIAN_POINT('Ctrl Pts',(-19.0423370360803,-21.4933634671533,
16.8486650820435));
#156222=CARTESIAN_POINT('Ctrl Pts',(-19.1258197302523,-21.4832347284594,
16.8528346479875));
#156223=CARTESIAN_POINT('Ctrl Pts',(-19.2088043125732,-21.4689879429832,
16.8570042139316));
#156224=CARTESIAN_POINT('Ctrl Pts',(-19.2908593851775,-21.4507011876452,
16.8611737798756));
#156225=CARTESIAN_POINT('Ctrl Pts',(-19.3757994129086,-21.4317714925488,
16.8654899426145));
#156226=CARTESIAN_POINT('Ctrl Pts',(-19.4597428368621,-21.4085125658604,
16.8698061053535));
#156227=CARTESIAN_POINT('Ctrl Pts',(-19.5422258260852,-21.381067931131,
16.8741222680924));
#156228=CARTESIAN_POINT('Ctrl Pts',(-19.6220219406102,-21.3545173024912,
16.8782978322841));
#156229=CARTESIAN_POINT('Ctrl Pts',(-19.7004508845915,-21.3240496914869,
16.8824733964757));
#156230=CARTESIAN_POINT('Ctrl Pts',(-19.7771127399862,-21.2898442659165,
16.8866489606674));
#156231=CARTESIAN_POINT('Ctrl Pts',(-19.8576466034505,-21.2539112056161,
16.8910354226799));
#156232=CARTESIAN_POINT('Ctrl Pts',(-19.9362296554817,-21.2138530785412,
16.8954218846925));
#156233=CARTESIAN_POINT('Ctrl Pts',(-20.0124291551049,-21.169931219713,
16.899808346705));
#156234=CARTESIAN_POINT('Ctrl Pts',(-20.0886286547281,-21.1260093608849,
16.9041948087175));
#156235=CARTESIAN_POINT('Ctrl Pts',(-20.1624441562134,-21.0782241494638,
16.9085812707301));
#156236=CARTESIAN_POINT('Ctrl Pts',(-20.2334815623277,-21.0268867545577,
16.9129677327426));
#156237=CARTESIAN_POINT('Ctrl Pts',(-20.3007008312569,-20.9783086554537,
16.9171184300413));
#156238=CARTESIAN_POINT('Ctrl Pts',(-20.3656920487852,-20.9263629083339,
16.9212691273401));
#156239=CARTESIAN_POINT('Ctrl Pts',(-20.4280939407346,-20.8712826055499,
16.9254198246388));
#156240=CARTESIAN_POINT('Ctrl Pts',(-20.4904067758306,-20.816280910614,
16.9295645982704));
#156241=CARTESIAN_POINT('Ctrl Pts',(-20.5501372744547,-20.758153849065,
16.9337093719019));
#156242=CARTESIAN_POINT('Ctrl Pts',(-20.6069541187602,-20.6971770308536,
16.9378541455334));
#156243=CARTESIAN_POINT('Ctrl Pts',(-20.6637057912846,-20.636270156123,
16.9419941649009));
#156244=CARTESIAN_POINT('Ctrl Pts',(-20.7175501324576,-20.5725203603438,
16.9461341842684));
#156245=CARTESIAN_POINT('Ctrl Pts',(-20.7681909845743,-20.5062416280221,
16.9502742036359));
#156246=CARTESIAN_POINT('Ctrl Pts',(-20.8188004163148,-20.4400040186795,
16.9544116543072));
#156247=CARTESIAN_POINT('Ctrl Pts',(-20.8662100198436,-20.3712409577298,
16.9585491049784));
#156248=CARTESIAN_POINT('Ctrl Pts',(-20.9101632231194,-20.3003002730633,
16.9626865556497));
#156249=CARTESIAN_POINT('Ctrl Pts',(-20.9541028768145,-20.2293814574863,
16.9668227308571));
#156250=CARTESIAN_POINT('Ctrl Pts',(-20.9945879994369,-20.1562867489274,
16.9709589060645));
#156251=CARTESIAN_POINT('Ctrl Pts',(-21.0314055962389,-20.0813925475095,
16.9750950812719));
#156252=CARTESIAN_POINT('Ctrl Pts',(-21.0682233367814,-20.0064980536955,
16.9792312726275));
#156253=CARTESIAN_POINT('Ctrl Pts',(-21.101373318238,-19.9298044742117,
16.983367463983));
#156254=CARTESIAN_POINT('Ctrl Pts',(-21.1306893947114,-19.8517110343203,
16.9875036553386));
#156255=CARTESIAN_POINT('Ctrl Pts',(-21.1600333335746,-19.773543373383,
16.9916437777855));
#156256=CARTESIAN_POINT('Ctrl Pts',(-21.1855359272153,-19.6939736349119,
16.9957839002324));
#156257=CARTESIAN_POINT('Ctrl Pts',(-21.2070801670876,-19.6134185415892,
16.9999240226793));
#156258=CARTESIAN_POINT('Ctrl Pts',(-21.2286351815299,-19.5328231615589,
17.0040662156583));
#156259=CARTESIAN_POINT('Ctrl Pts',(-21.2462278030767,-19.4512419037244,
17.0082084086373));
#156260=CARTESIAN_POINT('Ctrl Pts',(-21.2597921942375,-19.3691016561091,
17.0123506016163));
#156261=CARTESIAN_POINT('Ctrl Pts',(-21.2733789861849,-19.286825758752,
17.016499635181));
#156262=CARTESIAN_POINT('Ctrl Pts',(-21.2829242114339,-19.2039894937101,
17.0206486687457));
#156263=CARTESIAN_POINT('Ctrl Pts',(-21.2884139728529,-19.1210244221818,
17.0247977023105));
#156264=CARTESIAN_POINT('Ctrl Pts',(-21.2921595270972,-19.0644190158498,
17.0276285047975));
#156265=CARTESIAN_POINT('Ctrl Pts',(-21.2940183320645,-19.0077536994293,
17.0304593072845));
#156266=CARTESIAN_POINT('Ctrl Pts',(-21.2939998636668,-18.9511645205579,
17.0332901097715));
#156267=CARTESIAN_POINT('',(-21.2938494935628,-18.9531967451209,16.9667098397524));
#156268=CARTESIAN_POINT('Ctrl Pts',(-17.1744641402401,-20.9821349467765,
16.6833822503202));
#156269=CARTESIAN_POINT('Ctrl Pts',(-17.2433976321044,-21.0350891864301,
16.6877082599714));
#156270=CARTESIAN_POINT('Ctrl Pts',(-17.3151146538089,-21.0845925459325,
16.6920342696226));
#156271=CARTESIAN_POINT('Ctrl Pts',(-17.3892303913309,-21.1303467813,16.6963602792738));
#156272=CARTESIAN_POINT('Ctrl Pts',(-17.4606967411856,-21.1744654570554,
16.7005316486691));
#156273=CARTESIAN_POINT('Ctrl Pts',(-17.5343928021794,-21.2150982250402,
16.7047030180644));
#156274=CARTESIAN_POINT('Ctrl Pts',(-17.6099424306077,-21.2520205609281,
16.7088743874597));
#156275=CARTESIAN_POINT('Ctrl Pts',(-17.6854639536298,-21.2889291612454,
16.7130442050534));
#156276=CARTESIAN_POINT('Ctrl Pts',(-17.7628372618191,-21.3221298688539,
16.7172140226471));
#156277=CARTESIAN_POINT('Ctrl Pts',(-17.8416619148195,-21.3514442568512,
16.7213838402409));
#156278=CARTESIAN_POINT('Ctrl Pts',(-17.9204808895674,-21.3807565331426,
16.7255533574555));
#156279=CARTESIAN_POINT('Ctrl Pts',(-18.0007505699482,-21.4061828864854,
16.7297228746702));
#156280=CARTESIAN_POINT('Ctrl Pts',(-18.0820521418072,-21.4275936641941,
16.7338923918848));
#156281=CARTESIAN_POINT('Ctrl Pts',(-18.163372245078,-21.4490093221521,
16.7380628594752));
#156282=CARTESIAN_POINT('Ctrl Pts',(-18.2457242617706,-21.4664074711392,
16.7422333270656));
#156283=CARTESIAN_POINT('Ctrl Pts',(-18.3286772203917,-21.4797091296925,
16.746403794656));
#156284=CARTESIAN_POINT('Ctrl Pts',(-18.4117242396608,-21.4930258710425,
16.750578991154));
#156285=CARTESIAN_POINT('Ctrl Pts',(-18.4953731056364,-21.5022367814287,
16.7547541876521));
#156286=CARTESIAN_POINT('Ctrl Pts',(-18.5791863014753,-21.5073146026955,
16.7589293841502));
#156287=CARTESIAN_POINT('Ctrl Pts',(-18.6630562519229,-21.5123958624395,
16.7631074079076));
#156288=CARTESIAN_POINT('Ctrl Pts',(-18.7470902943607,-21.5133384585987,
16.767285431665));
#156289=CARTESIAN_POINT('Ctrl Pts',(-18.8308518534922,-21.5101672577209,
16.7714634554225));
#156290=CARTESIAN_POINT('Ctrl Pts',(-18.914746487242,-21.5069910186567,
16.7756481169374));
#156291=CARTESIAN_POINT('Ctrl Pts',(-18.9983673171488,-21.4996879836572,
16.7798327784523));
#156292=CARTESIAN_POINT('Ctrl Pts',(-19.0812844001845,-21.4883346674657,
16.7840174399673));
#156293=CARTESIAN_POINT('Ctrl Pts',(-19.1023475182635,-21.4854506267979,
16.7850804539613));
#156294=CARTESIAN_POINT('Ctrl Pts',(-19.12336528706,-21.4823054789026,16.7861434679553));
#156295=CARTESIAN_POINT('Ctrl Pts',(-19.1443308019265,-21.4789009939035,
16.7872064819493));
#156296=CARTESIAN_POINT('Ctrl Pts',(-19.226863125181,-21.4654989831134,
16.7913911163424));
#156297=CARTESIAN_POINT('Ctrl Pts',(-19.3088917529366,-21.4480243381486,
16.7955757507354));
#156298=CARTESIAN_POINT('Ctrl Pts',(-19.3899836880773,-21.4265273085938,
16.7997603851285));
#156299=CARTESIAN_POINT('Ctrl Pts',(-19.4709601988853,-21.4050608773999,
16.8039390632124));
#156300=CARTESIAN_POINT('Ctrl Pts',(-19.5510022244941,-21.3795835508679,
16.8081177412964));
#156301=CARTESIAN_POINT('Ctrl Pts',(-19.6296848716226,-21.3501969499494,
16.8122964193803));
#156302=CARTESIAN_POINT('Ctrl Pts',(-19.7097778486527,-21.3202836153291,
16.8165499972657));
#156303=CARTESIAN_POINT('Ctrl Pts',(-19.7884617582359,-21.2863195576314,
16.8208035751512));
#156304=CARTESIAN_POINT('Ctrl Pts',(-19.8653024038482,-21.2484657347862,
16.8250571530366));
#156305=CARTESIAN_POINT('Ctrl Pts',(-19.9406533436032,-21.2113457821626,
16.8292282670146));
#156306=CARTESIAN_POINT('Ctrl Pts',(-20.0142314204538,-21.1704857525211,
16.8333993809925));
#156307=CARTESIAN_POINT('Ctrl Pts',(-20.0856470518143,-21.1260860717372,
16.8375704949705));
#156308=CARTESIAN_POINT('Ctrl Pts',(-20.15703871897,-21.081701289695,16.8417402092909));
#156309=CARTESIAN_POINT('Ctrl Pts',(-20.2262689913883,-21.0337794581181,
16.8459099236112));
#156310=CARTESIAN_POINT('Ctrl Pts',(-20.2929745824341,-20.9825659928514,
16.8500796379316));
#156311=CARTESIAN_POINT('Ctrl Pts',(-20.3596777998085,-20.9313543499797,
16.8542492038756));
#156312=CARTESIAN_POINT('Ctrl Pts',(-20.4238561500589,-20.8768515871279,
16.8584187698197));
#156313=CARTESIAN_POINT('Ctrl Pts',(-20.4851780435301,-20.8193444941569,
16.8625883357637));
#156314=CARTESIAN_POINT('Ctrl Pts',(-20.5486559391271,-20.7598155227396,
16.8669044985026));
#156315=CARTESIAN_POINT('Ctrl Pts',(-20.6090723898813,-20.6970673867193,
16.8712206612416));
#156316=CARTESIAN_POINT('Ctrl Pts',(-20.6661012016726,-20.6314597186284,
16.8755368239805));
#156317=CARTESIAN_POINT('Ctrl Pts',(-20.7212723059182,-20.5679892134248,
16.8797123881722));
#156318=CARTESIAN_POINT('Ctrl Pts',(-20.7732728325614,-20.5018430132074,
16.8838879523639));
#156319=CARTESIAN_POINT('Ctrl Pts',(-20.8218497444837,-20.4333788996943,
16.8880635165556));
#156320=CARTESIAN_POINT('Ctrl Pts',(-20.8728801607464,-20.3614568265657,
16.8924499785681));
#156321=CARTESIAN_POINT('Ctrl Pts',(-20.9201317067406,-20.2869770238507,
16.8968364405806));
#156322=CARTESIAN_POINT('Ctrl Pts',(-20.9633649162028,-20.2103847068381,
16.9012229025932));
#156323=CARTESIAN_POINT('Ctrl Pts',(-21.0065981256651,-20.1337923898255,
16.9056093646057));
#156324=CARTESIAN_POINT('Ctrl Pts',(-21.0458128079223,-20.0550881117615,
16.9099958266183));
#156325=CARTESIAN_POINT('Ctrl Pts',(-21.0808281256648,-19.9747403133684,
16.9143822886308));
#156326=CARTESIAN_POINT('Ctrl Pts',(-21.1176528956138,-19.890240460661,
16.9189954255354));
#156327=CARTESIAN_POINT('Ctrl Pts',(-21.1499518315865,-19.8036540013275,
16.9236085624399));
#156328=CARTESIAN_POINT('Ctrl Pts',(-21.1775079602931,-19.7154584782318,
16.9282216993445));
#156329=CARTESIAN_POINT('Ctrl Pts',(-21.2049852187145,-19.6275153855896,
16.9328216326736));
#156330=CARTESIAN_POINT('Ctrl Pts',(-21.2277466226989,-19.5379726851093,
16.9374215660027));
#156331=CARTESIAN_POINT('Ctrl Pts',(-21.2456232056933,-19.4473270360306,
16.9420214993319));
#156332=CARTESIAN_POINT('Ctrl Pts',(-21.2634117418665,-19.3571278403517,
16.9465987767929));
#156333=CARTESIAN_POINT('Ctrl Pts',(-21.2763633328304,-19.2658368103367,
16.9511760542538));
#156334=CARTESIAN_POINT('Ctrl Pts',(-21.2843593339855,-19.1739623111095,
16.9557533317148));
#156335=CARTESIAN_POINT('Ctrl Pts',(-21.2907392715843,-19.1006564722762,
16.9594055003435));
#156336=CARTESIAN_POINT('Ctrl Pts',(-21.2939652250916,-19.0269796001108,
16.9630576689721));
#156337=CARTESIAN_POINT('Ctrl Pts',(-21.2939997202205,-18.9531968587605,
16.9667098376008));
#156338=CARTESIAN_POINT('Ctrl Pts',(-21.290325207156,-18.9531940791588,
16.9667098902285));
#156339=CARTESIAN_POINT('Ctrl Pts',(-21.2882101978943,-18.4498774972589,
16.9916592919231));
#156340=CARTESIAN_POINT('Ctrl Pts',(-20.9008594754591,-17.088363994255,
17.0590006291781));
#156341=CARTESIAN_POINT('Ctrl Pts',(-18.6858816908488,-15.9252896642242,
17.1687339019936));
#156342=CARTESIAN_POINT('Ctrl Pts',(-16.1629700668002,-17.3541589844551,
17.2959097086751));
#156343=CARTESIAN_POINT('Ctrl Pts',(-16.0276178903722,-19.7410799583894,
17.4007735074215));
#156344=CARTESIAN_POINT('Ctrl Pts',(-16.8552506915702,-20.7323953231713,
17.4632453706075));
#156345=CARTESIAN_POINT('Ctrl Pts',(-17.1769969312964,-20.9788274605145,
17.483325298233));
#156346=CARTESIAN_POINT('Origin',(-18.734,-18.952,-1.76670989022851));
#156347=CARTESIAN_POINT('',(-17.1744641402401,-20.9821349467765,18.3499540410247));
#156348=CARTESIAN_POINT('',(-17.1744641402402,-20.9821349467765,18.2832318482317));
#156349=CARTESIAN_POINT('',(-17.1744641402401,-20.9821349467765,-1.76670989022851));
#156350=CARTESIAN_POINT('',(-21.2939989159607,-18.9543559031924,17.8332901097715));
#156351=CARTESIAN_POINT('Ctrl Pts',(-21.2939989159607,-18.9543559031924,
17.8332901097715));
#156352=CARTESIAN_POINT('Ctrl Pts',(-21.2940751741219,-18.8714913735434,
17.837412174938));
#156353=CARTESIAN_POINT('Ctrl Pts',(-21.290123839502,-18.7885152466555,
17.8415342401044));
#156354=CARTESIAN_POINT('Ctrl Pts',(-21.2821391268744,-18.7058557534859,
17.8456563052709));
#156355=CARTESIAN_POINT('Ctrl Pts',(-21.2741597741335,-18.6232517470386,
17.8497756034244));
#156356=CARTESIAN_POINT('Ctrl Pts',(-21.262152459652,-18.5409644216312,
17.8538949015779));
#156357=CARTESIAN_POINT('Ctrl Pts',(-21.2461634417033,-18.4594202174576,
17.8580141997315));
#156358=CARTESIAN_POINT('Ctrl Pts',(-21.2301800733889,-18.3779048264943,
17.862132042353));
#156359=CARTESIAN_POINT('Ctrl Pts',(-21.2102178848107,-18.2971324990613,
17.8662498849744));
#156360=CARTESIAN_POINT('Ctrl Pts',(-21.1863745538874,-18.217521240984,
17.8703677275959));
#156361=CARTESIAN_POINT('Ctrl Pts',(-21.1625320679642,-18.1379128043046,
17.8744854242823));
#156362=CARTESIAN_POINT('Ctrl Pts',(-21.1348088500427,-18.0594658076282,
17.8786031209688));
#156363=CARTESIAN_POINT('Ctrl Pts',(-21.103352505349,-17.9825833169393,
17.8827208176552));
#156364=CARTESIAN_POINT('Ctrl Pts',(-21.071866121991,-17.905627408714,17.8868424464612));
#156365=CARTESIAN_POINT('Ctrl Pts',(-21.0366396717683,-17.8302394286303,
17.8909640752672));
#156366=CARTESIAN_POINT('Ctrl Pts',(-20.9978687619911,-17.7568020128526,
17.8950857040732));
#156367=CARTESIAN_POINT('Ctrl Pts',(-20.9590794967265,-17.683329829267,
17.8992092842005));
#156368=CARTESIAN_POINT('Ctrl Pts',(-20.9167426732498,-17.6118104548626,
17.9033328643279));
#156369=CARTESIAN_POINT('Ctrl Pts',(-20.8710983794442,-17.5425992349311,
17.9074564444553));
#156370=CARTESIAN_POINT('Ctrl Pts',(-20.8253741239691,-17.4732667677585,
17.9115872484506));
#156371=CARTESIAN_POINT('Ctrl Pts',(-20.776331105883,-17.4062509123682,
17.9157180524459));
#156372=CARTESIAN_POINT('Ctrl Pts',(-20.724250792007,-17.3418752269108,
17.9198488564413));
#156373=CARTESIAN_POINT('Ctrl Pts',(-20.6800170723894,-17.2871985975131,
17.9233572996922));
#156374=CARTESIAN_POINT('Ctrl Pts',(-20.6335931281536,-17.2344260450368,
17.9268657429431));
#156375=CARTESIAN_POINT('Ctrl Pts',(-20.5851713910723,-17.1837340469049,
17.930374186194));
#156376=CARTESIAN_POINT('Ctrl Pts',(-20.5274172101246,-17.1232720517519,
17.934558820587));
#156377=CARTESIAN_POINT('Ctrl Pts',(-20.4665902688467,-17.0655300202436,
17.93874345498));
#156378=CARTESIAN_POINT('Ctrl Pts',(-20.4029770272299,-17.0108365131759,
17.942928089373));
#156379=CARTESIAN_POINT('Ctrl Pts',(-20.3394543311886,-16.9562208555457,
17.9471067674569));
#156380=CARTESIAN_POINT('Ctrl Pts',(-20.2731535582845,-16.9046454006956,
17.9512854455408));
#156381=CARTESIAN_POINT('Ctrl Pts',(-20.2043989371765,-16.8564029572577,
17.9554641236247));
#156382=CARTESIAN_POINT('Ctrl Pts',(-20.1344119388971,-16.8072958026916,
17.9597177015102));
#156383=CARTESIAN_POINT('Ctrl Pts',(-20.0618825897098,-16.7616426719214,
17.9639712793956));
#156384=CARTESIAN_POINT('Ctrl Pts',(-19.9871893049686,-16.7197104654834,
17.9682248572811));
#156385=CARTESIAN_POINT('Ctrl Pts',(-19.9139440953053,-16.6785911966919,
17.972395971259));
#156386=CARTESIAN_POINT('Ctrl Pts',(-19.8386185251851,-16.6410501005271,
17.9765670852369));
#156387=CARTESIAN_POINT('Ctrl Pts',(-19.7615983036833,-16.6072949596448,
17.9807381992148));
#156388=CARTESIAN_POINT('Ctrl Pts',(-19.6846039270607,-16.573551145626,
17.9849079135351));
#156389=CARTESIAN_POINT('Ctrl Pts',(-19.6059164494111,-16.5435909483338,
17.9890776278554));
#156390=CARTESIAN_POINT('Ctrl Pts',(-19.5259437923517,-16.5175750104479,
17.9932473421758));
#156391=CARTESIAN_POINT('Ctrl Pts',(-19.4459739810627,-16.4915599983208,
17.9974169081197));
#156392=CARTESIAN_POINT('Ctrl Pts',(-19.3647195190219,-16.4694891080429,
18.0015864740637));
#156393=CARTESIAN_POINT('Ctrl Pts',(-19.2826045027052,-16.4514734355317,
18.0057560400077));
#156394=CARTESIAN_POINT('Ctrl Pts',(-19.1976024237123,-16.4328243541992,
18.0100722027467));
#156395=CARTESIAN_POINT('Ctrl Pts',(-19.1116786655142,-16.4185210722995,
18.0143883654857));
#156396=CARTESIAN_POINT('Ctrl Pts',(-19.0253143284881,-16.4086290160463,
18.0187045282247));
#156397=CARTESIAN_POINT('Ctrl Pts',(-18.941763300659,-16.3990591924853,
18.0228800924163));
#156398=CARTESIAN_POINT('Ctrl Pts',(-18.8578004300247,-16.3936175999791,
18.027055656608));
#156399=CARTESIAN_POINT('Ctrl Pts',(-18.7738638919263,-16.3923103957471,
18.0312312207996));
#156400=CARTESIAN_POINT('Ctrl Pts',(-18.6856879188252,-16.3909371677368,
18.0356176828123));
#156401=CARTESIAN_POINT('Ctrl Pts',(-18.5975415917826,-16.3941269389876,
18.0400041448249));
#156402=CARTESIAN_POINT('Ctrl Pts',(-18.5099274935592,-16.4018251997447,
18.0443906068376));
#156403=CARTESIAN_POINT('Ctrl Pts',(-18.4223133953358,-16.4095234605017,
18.0487770688502));
#156404=CARTESIAN_POINT('Ctrl Pts',(-18.3352320899718,-16.4217300548923,
18.0531635308629));
#156405=CARTESIAN_POINT('Ctrl Pts',(-18.249172131343,-16.4383289917387,
18.0575499928756));
#156406=CARTESIAN_POINT('Ctrl Pts',(-18.1670719189866,-16.4541641868944,
18.0617346272685));
#156407=CARTESIAN_POINT('Ctrl Pts',(-18.0855955387245,-16.4740553519455,
18.0659192616615));
#156408=CARTESIAN_POINT('Ctrl Pts',(-18.0051743135503,-16.4979394630998,
18.0701038960544));
#156409=CARTESIAN_POINT('Ctrl Pts',(-17.924867558036,-16.5217895781781,
18.0742825741382));
#156410=CARTESIAN_POINT('Ctrl Pts',(-17.8456134116216,-16.5496212203606,
18.0784612522221));
#156411=CARTESIAN_POINT('Ctrl Pts',(-17.7678335788524,-16.5813202564144,
18.0826399303059));
#156412=CARTESIAN_POINT('Ctrl Pts',(-17.6886595984777,-16.6135874749089,
18.0868935081914));
#156413=CARTESIAN_POINT('Ctrl Pts',(-17.6110137791771,-16.6498620057512,
18.0911470860768));
#156414=CARTESIAN_POINT('Ctrl Pts',(-17.5353253711178,-16.6899701297122,
18.0954006639623));
#156415=CARTESIAN_POINT('Ctrl Pts',(-17.4611043305451,-16.7293006794244,
18.0995717779401));
#156416=CARTESIAN_POINT('Ctrl Pts',(-17.3887659072351,-16.7723172800339,
18.103742891918));
#156417=CARTESIAN_POINT('Ctrl Pts',(-17.318693590526,-16.818808080059,18.1079140058958));
#156418=CARTESIAN_POINT('Ctrl Pts',(-17.2486447872595,-16.8652832796471,
18.1120837202161));
#156419=CARTESIAN_POINT('Ctrl Pts',(-17.1808609634159,-16.9152301092319,
18.1162534345363));
#156420=CARTESIAN_POINT('Ctrl Pts',(-17.1156979943011,-16.968392524124,
18.1204231488566));
#156421=CARTESIAN_POINT('Ctrl Pts',(-17.0505373439644,-17.0215530472694,
18.1245927148005));
#156422=CARTESIAN_POINT('Ctrl Pts',(-16.9879977188453,-17.0779286367475,
18.1287622807445));
#156423=CARTESIAN_POINT('Ctrl Pts',(-16.928402088408,-17.1372228286496,
18.1329318466884));
#156424=CARTESIAN_POINT('Ctrl Pts',(-16.8667111491201,-17.1986017311952,
18.1372480094274));
#156425=CARTESIAN_POINT('Ctrl Pts',(-16.8081754519449,-17.263107918902,
18.1415641721665));
#156426=CARTESIAN_POINT('Ctrl Pts',(-16.7531104204836,-17.330372276457,
18.1458803349055));
#156427=CARTESIAN_POINT('Ctrl Pts',(-16.6998391266334,-17.3954455046358,
18.1500558990971));
#156428=CARTESIAN_POINT('Ctrl Pts',(-16.6498160990941,-17.4630995606101,
18.1542314632887));
#156429=CARTESIAN_POINT('Ctrl Pts',(-16.6032836911145,-17.5329693410468,
18.1584070274802));
#156430=CARTESIAN_POINT('Ctrl Pts',(-16.5544010418239,-17.6063680779999,
18.162793489493));
#156431=CARTESIAN_POINT('Ctrl Pts',(-16.509371199651,-17.6822117522655,
18.1671799515058));
#156432=CARTESIAN_POINT('Ctrl Pts',(-16.4684203690346,-17.7600482661808,
18.1715664135186));
#156433=CARTESIAN_POINT('Ctrl Pts',(-16.4274695384181,-17.8378847800961,
18.1759528755314));
#156434=CARTESIAN_POINT('Ctrl Pts',(-16.390597893598,-17.9177135750216,
18.1803393375442));
#156435=CARTESIAN_POINT('Ctrl Pts',(-16.3579723492966,-17.9990610706384,
18.184725799557));
#156436=CARTESIAN_POINT('Ctrl Pts',(-16.3268479546497,-18.0766656473996,
18.1889104339505));
#156437=CARTESIAN_POINT('Ctrl Pts',(-16.2994716572955,-18.1559410996701,
18.193095068344));
#156438=CARTESIAN_POINT('Ctrl Pts',(-16.2760239311543,-18.236490639487,
18.1972797027375));
#156439=CARTESIAN_POINT('Ctrl Pts',(-16.2526095799489,-18.3169255270041,
18.2014583808218));
#156440=CARTESIAN_POINT('Ctrl Pts',(-16.2331128202904,-18.398630461953,
18.2056370589062));
#156441=CARTESIAN_POINT('Ctrl Pts',(-16.217665944864,-18.4811890793931,
18.2098157369906));
#156442=CARTESIAN_POINT('Ctrl Pts',(-16.201942195299,-18.565227500706,18.2140693148759));
#156443=CARTESIAN_POINT('Ctrl Pts',(-16.1904151258529,-18.6501500625611,
18.2183228927612));
#156444=CARTESIAN_POINT('Ctrl Pts',(-16.1831710111198,-18.7355018025745,
18.2225764706466));
#156445=CARTESIAN_POINT('Ctrl Pts',(-16.1760673376856,-18.8191988325684,
18.226747584625));
#156446=CARTESIAN_POINT('Ctrl Pts',(-16.1730820747445,-18.9033080688141,
18.2309186986034));
#156447=CARTESIAN_POINT('Ctrl Pts',(-16.1742446642318,-18.9873923862777,
18.2350898125817));
#156448=CARTESIAN_POINT('Ctrl Pts',(-16.1754068636011,-19.0714484884366,
18.2392595269026));
#156449=CARTESIAN_POINT('Ctrl Pts',(-16.180714144804,-19.1554792288139,
18.2434292412234));
#156450=CARTESIAN_POINT('Ctrl Pts',(-16.1901438433303,-19.2390467804617,
18.2475989555442));
#156451=CARTESIAN_POINT('Ctrl Pts',(-16.1995732063073,-19.3226113584171,
18.2517685214886));
#156452=CARTESIAN_POINT('Ctrl Pts',(-16.2131246425145,-19.4057123233777,
18.2559380874331));
#156453=CARTESIAN_POINT('Ctrl Pts',(-16.2307236899664,-19.4879176388443,
18.2601076533776));
#156454=CARTESIAN_POINT('Ctrl Pts',(-16.2489414982118,-19.5730131917728,
18.264423816116));
#156455=CARTESIAN_POINT('Ctrl Pts',(-16.2714967310845,-19.6571484255567,
18.2687399788544));
#156456=CARTESIAN_POINT('Ctrl Pts',(-16.2982497538328,-19.7398583237465,
18.2730561415928));
#156457=CARTESIAN_POINT('Ctrl Pts',(-16.3241312996848,-19.81987395572,18.2772317057849));
#156458=CARTESIAN_POINT('Ctrl Pts',(-16.3539411382348,-19.8985552629114,
18.281407269977));
#156459=CARTESIAN_POINT('Ctrl Pts',(-16.3875034565753,-19.9755008410822,
18.2855828341691));
#156460=CARTESIAN_POINT('Ctrl Pts',(-16.4227609278168,-20.0563327574592,
18.2899692961806));
#156461=CARTESIAN_POINT('Ctrl Pts',(-16.4621596558346,-20.1352484709666,
18.2943557581922));
#156462=CARTESIAN_POINT('Ctrl Pts',(-16.5054419382129,-20.2118130675793,
18.2987422202037));
#156463=CARTESIAN_POINT('Ctrl Pts',(-16.5487242205912,-20.2883776641921,
18.3031286822153));
#156464=CARTESIAN_POINT('Ctrl Pts',(-16.5958896819153,-20.362590695021,
18.3075151442268));
#156465=CARTESIAN_POINT('Ctrl Pts',(-16.6466304638568,-20.4340554711552,
18.3119016062384));
#156466=CARTESIAN_POINT('Ctrl Pts',(-16.6950307331533,-20.5022238019884,
18.3160857345568));
#156467=CARTESIAN_POINT('Ctrl Pts',(-16.7468638869254,-20.5681455333867,
18.3202698628752));
#156468=CARTESIAN_POINT('Ctrl Pts',(-16.801894064722,-20.6314542729302,
18.3244539911936));
#156469=CARTESIAN_POINT('Ctrl Pts',(-16.8577907043263,-20.69575982199,18.3287039994988));
#156470=CARTESIAN_POINT('Ctrl Pts',(-16.9169857078822,-20.7573689488297,
18.3329540078039));
#156471=CARTESIAN_POINT('Ctrl Pts',(-16.9791857141597,-20.8159277942589,
18.3372040161091));
#156472=CARTESIAN_POINT('Ctrl Pts',(-17.0413857204372,-20.8744866396881,
18.3414540244143));
#156473=CARTESIAN_POINT('Ctrl Pts',(-17.1065904145128,-20.9299948122621,
18.3457040327195));
#156474=CARTESIAN_POINT('Ctrl Pts',(-17.1744641402401,-20.9821349467765,
18.3499540410247));
#156475=CARTESIAN_POINT('Ctrl Pts',(-17.1718942801479,-20.9854857634355,
17.5498940685532));
#156476=CARTESIAN_POINT('Ctrl Pts',(-17.8395944672753,-21.4975646458316,
17.5919369033125));
#156477=CARTESIAN_POINT('Ctrl Pts',(-19.7363287145451,-21.8042998984821,
17.6763716736323));
#156478=CARTESIAN_POINT('Ctrl Pts',(-21.1817725818657,-20.2077259866878,
17.7708370079975));
#156479=CARTESIAN_POINT('Ctrl Pts',(-21.2957663888719,-19.1559927477998,
17.8232595076033));
#156480=CARTESIAN_POINT('Ctrl Pts',(-21.2939116922138,-18.9543565892689,
17.8332900716486));
#156481=CARTESIAN_POINT('',(-21.2939990418858,-18.9497851537328,17.7667099127498));
#156482=CARTESIAN_POINT('Ctrl Pts',(-17.1769969312964,-20.9788274605145,
17.483325298233));
#156483=CARTESIAN_POINT('Ctrl Pts',(-17.5345084118012,-21.2526529396887,
17.505637306168));
#156484=CARTESIAN_POINT('Ctrl Pts',(-18.7708036860181,-21.788223221189,
17.5703412496634));
#156485=CARTESIAN_POINT('Ctrl Pts',(-20.7784813047341,-21.0089843504267,
17.6648027803286));
#156486=CARTESIAN_POINT('Ctrl Pts',(-21.2874612586096,-19.5488856065476,
17.7369523030588));
#156487=CARTESIAN_POINT('Ctrl Pts',(-21.2923872581368,-18.9497870016169,
17.7667098902285));
#156488=CARTESIAN_POINT('Ctrl Pts',(-21.2939990418858,-18.9497851537328,
17.7667099127498));
#156489=CARTESIAN_POINT('Ctrl Pts',(-21.2939112972755,-18.8483667746996,
17.7717442924651));
#156490=CARTESIAN_POINT('Ctrl Pts',(-21.2877929815452,-18.7472123213116,
17.7767786721804));
#156491=CARTESIAN_POINT('Ctrl Pts',(-21.275760552819,-18.64695362298,17.7818130518957));
#156492=CARTESIAN_POINT('Ctrl Pts',(-21.2635573150894,-18.54527168012,17.7869188982619));
#156493=CARTESIAN_POINT('Ctrl Pts',(-21.245270932926,-18.4445110968148,
17.792024744628));
#156494=CARTESIAN_POINT('Ctrl Pts',(-21.2210717431372,-18.345308855769,
17.7971305909941));
#156495=CARTESIAN_POINT('Ctrl Pts',(-21.2092508709201,-18.2968503319384,
17.7996247057963));
#156496=CARTESIAN_POINT('Ctrl Pts',(-21.1960198419216,-18.2487633198847,
17.8021188205986));
#156497=CARTESIAN_POINT('Ctrl Pts',(-21.1814026084241,-18.201120201178,
17.8046129354008));
#156498=CARTESIAN_POINT('Ctrl Pts',(-21.1568777637899,-18.121184412756,
17.8087975697939));
#156499=CARTESIAN_POINT('Ctrl Pts',(-21.1283869296254,-18.0423026572185,
17.8129822041869));
#156500=CARTESIAN_POINT('Ctrl Pts',(-21.0960388974778,-17.9648970434641,
17.8171668385799));
#156501=CARTESIAN_POINT('Ctrl Pts',(-21.0637369087501,-17.88760160702,17.8213455166639));
#156502=CARTESIAN_POINT('Ctrl Pts',(-21.0275888032569,-17.8117785597318,
17.8255241947478));
#156503=CARTESIAN_POINT('Ctrl Pts',(-20.9877531601769,-17.7378349811526,
17.8297028728318));
#156504=CARTESIAN_POINT('Ctrl Pts',(-20.947203491824,-17.6625660170697,
17.8339564507172));
#156505=CARTESIAN_POINT('Ctrl Pts',(-20.9028329287837,-17.5892450243181,
17.8382100286026));
#156506=CARTESIAN_POINT('Ctrl Pts',(-20.8548601014715,-17.5182802121801,
17.8424636064881));
#156507=CARTESIAN_POINT('Ctrl Pts',(-20.8078173210281,-17.448691191402,
17.846634720466));
#156508=CARTESIAN_POINT('Ctrl Pts',(-20.7573109732373,-17.3813682068563,
17.850805834444));
#156509=CARTESIAN_POINT('Ctrl Pts',(-20.7035927080245,-17.3166698912767,
17.8549769484219));
#156510=CARTESIAN_POINT('Ctrl Pts',(-20.6498924684943,-17.2519932858418,
17.8591466627423));
#156511=CARTESIAN_POINT('Ctrl Pts',(-20.5929827456749,-17.1899399538653,
17.8633163770627));
#156512=CARTESIAN_POINT('Ctrl Pts',(-20.533156175962,-17.1308363460419,
17.867486091383));
#156513=CARTESIAN_POINT('Ctrl Pts',(-20.4733317351351,-17.0717348413785,
17.8716556573271));
#156514=CARTESIAN_POINT('Ctrl Pts',(-20.4105909816463,-17.015583174876,
17.8758252232711));
#156515=CARTESIAN_POINT('Ctrl Pts',(-20.345263220069,-16.9626707573524,
17.8799947892151));
#156516=CARTESIAN_POINT('Ctrl Pts',(-20.2776386149851,-16.9078980045031,
17.8843109519541));
#156517=CARTESIAN_POINT('Ctrl Pts',(-20.2072421084912,-16.8565968547186,
17.888627114693));
#156518=CARTESIAN_POINT('Ctrl Pts',(-20.134474432863,-16.8090414462951,
17.8929432774319));
#156519=CARTESIAN_POINT('Ctrl Pts',(-20.0640771566148,-16.7630351502991,
17.8971188416236));
#156520=CARTESIAN_POINT('Ctrl Pts',(-19.9914612509379,-16.7205345053977,
17.9012944058153));
#156521=CARTESIAN_POINT('Ctrl Pts',(-19.9170156443953,-16.6817414276968,
17.905469970007));
#156522=CARTESIAN_POINT('Ctrl Pts',(-19.8388099672436,-16.640989003863,
17.9098564320195));
#156523=CARTESIAN_POINT('Ctrl Pts',(-19.7585854263165,-16.604328771398,
17.9142428940321));
#156524=CARTESIAN_POINT('Ctrl Pts',(-19.6768157184724,-16.5719372863302,
17.9186293560446));
#156525=CARTESIAN_POINT('Ctrl Pts',(-19.5950460106283,-16.5395458012623,
17.9230158180572));
#156526=CARTESIAN_POINT('Ctrl Pts',(-19.5117317099373,-16.5114231770868,
17.9274022800697));
#156527=CARTESIAN_POINT('Ctrl Pts',(-19.427361531773,-16.4876847226344,
17.9317887420823));
#156528=CARTESIAN_POINT('Ctrl Pts',(-19.3468733505732,-16.4650385096604,
17.9359733764753));
#156529=CARTESIAN_POINT('Ctrl Pts',(-19.265124729313,-16.4462975942589,
17.9401580108683));
#156530=CARTESIAN_POINT('Ctrl Pts',(-19.1825294815773,-16.4315989794963,
17.9443426452613));
#156531=CARTESIAN_POINT('Ctrl Pts',(-19.1000517979535,-16.4169212863925,
17.9485213233453));
#156532=CARTESIAN_POINT('Ctrl Pts',(-19.0167303305415,-16.4062745451513,
17.9527000014292));
#156533=CARTESIAN_POINT('Ctrl Pts',(-18.9329932047253,-16.3997457602204,
17.9568786795131));
#156534=CARTESIAN_POINT('Ctrl Pts',(-18.8477551511091,-16.3930999515116,
17.9611322573986));
#156535=CARTESIAN_POINT('Ctrl Pts',(-18.7620868552842,-16.3907213105009,
17.965385835284));
#156536=CARTESIAN_POINT('Ctrl Pts',(-18.6764498971536,-16.3926469595497,
17.9696394131694));
#156537=CARTESIAN_POINT('Ctrl Pts',(-18.5924731785637,-16.394535276134,
17.9738105271474));
#156538=CARTESIAN_POINT('Ctrl Pts',(-18.5085270745237,-16.40056246717,17.9779816411253));
#156539=CARTESIAN_POINT('Ctrl Pts',(-18.4250493517398,-16.4107110559915,
17.9821527551032));
#156540=CARTESIAN_POINT('Ctrl Pts',(-18.341599640712,-16.4208562393561,
17.9863224694236));
#156541=CARTESIAN_POINT('Ctrl Pts',(-18.2586184550888,-16.4351200184238,
17.9904921837439));
#156542=CARTESIAN_POINT('Ctrl Pts',(-18.1765386867733,-16.4534330338661,
17.9946618980643));
#156543=CARTESIAN_POINT('Ctrl Pts',(-18.0944618392082,-16.4717453976528,
17.9988314640083));
#156544=CARTESIAN_POINT('Ctrl Pts',(-18.0132867939826,-16.4941066103199,
18.0030010299523));
#156545=CARTESIAN_POINT('Ctrl Pts',(-17.9334351461144,-16.5203964314216,
18.0071705958963));
#156546=CARTESIAN_POINT('Ctrl Pts',(-17.8507760128139,-16.5476105702015,
18.0114867586353));
#156547=CARTESIAN_POINT('Ctrl Pts',(-17.7695355706378,-16.5790345522992,
18.0158029213742));
#156548=CARTESIAN_POINT('Ctrl Pts',(-17.6901612352904,-16.6144798111482,
18.0201190841132));
#156549=CARTESIAN_POINT('Ctrl Pts',(-17.613372510569,-16.6487704444181,
18.0242946483048));
#156550=CARTESIAN_POINT('Ctrl Pts',(-17.5383305816066,-16.6868241363793,
18.0284702124965));
#156551=CARTESIAN_POINT('Ctrl Pts',(-17.4654157475491,-16.7284231530182,
18.0326457766881));
#156552=CARTESIAN_POINT('Ctrl Pts',(-17.3888181585608,-16.7721232370958,
18.0370322387007));
#156553=CARTESIAN_POINT('Ctrl Pts',(-17.3145686822397,-16.81973589169,18.0414187007133));
#156554=CARTESIAN_POINT('Ctrl Pts',(-17.2430721773899,-16.8709583791363,
18.0458051627259));
#156555=CARTESIAN_POINT('Ctrl Pts',(-17.1715756725401,-16.9221808665826,
18.0501916247385));
#156556=CARTESIAN_POINT('Ctrl Pts',(-17.1028325453263,-16.9770127656117,
18.0545780867511));
#156557=CARTESIAN_POINT('Ctrl Pts',(-17.03720428459,-17.0351055584185,18.0589645487636));
#156558=CARTESIAN_POINT('Ctrl Pts',(-16.9745956774142,-17.0905254157143,
18.0631491831567));
#156559=CARTESIAN_POINT('Ctrl Pts',(-16.9145885551718,-17.1491189671382,
18.0673338175499));
#156560=CARTESIAN_POINT('Ctrl Pts',(-16.8575221052052,-17.2106124181141,
18.071518451943));
#156561=CARTESIAN_POINT('Ctrl Pts',(-16.8005368822667,-17.2720183407739,
18.075697130027));
#156562=CARTESIAN_POINT('Ctrl Pts',(-16.7464843277719,-17.3363156298582,
18.079875808111));
#156563=CARTESIAN_POINT('Ctrl Pts',(-16.6956693348428,-17.4031913935286,
18.084054486195));
#156564=CARTESIAN_POINT('Ctrl Pts',(-16.6439435196865,-17.4712658571988,
18.0883080640804));
#156565=CARTESIAN_POINT('Ctrl Pts',(-16.5955728353228,-17.5420118234209,
18.0925616419658));
#156566=CARTESIAN_POINT('Ctrl Pts',(-16.5508383402301,-17.6150612701733,
18.0968152198512));
#156567=CARTESIAN_POINT('Ctrl Pts',(-16.5069711106161,-17.6866945108574,
18.1009863338293));
#156568=CARTESIAN_POINT('Ctrl Pts',(-16.4666005905003,-17.7605423037905,
18.1051574478073));
#156569=CARTESIAN_POINT('Ctrl Pts',(-16.4299490395872,-17.836227096663,
18.1093285617853));
#156570=CARTESIAN_POINT('Ctrl Pts',(-16.3933097874561,-17.9118864927724,
18.1134982761057));
#156571=CARTESIAN_POINT('Ctrl Pts',(-16.3603872264447,-17.989381250901,
18.1176679904261));
#156572=CARTESIAN_POINT('Ctrl Pts',(-16.331357352511,-18.0683098345761,
18.1218377047466));
#156573=CARTESIAN_POINT('Ctrl Pts',(-16.3023285115847,-18.1472356096334,
18.1260072706907));
#156574=CARTESIAN_POINT('Ctrl Pts',(-16.2771922403253,-18.227594676743,
18.1301768366348));
#156575=CARTESIAN_POINT('Ctrl Pts',(-16.2560756369329,-18.3089674573409,
18.1343464025789));
#156576=CARTESIAN_POINT('Ctrl Pts',(-16.2342165998161,-18.393201204518,
18.1386625653177));
#156577=CARTESIAN_POINT('Ctrl Pts',(-16.2166652853052,-18.478520765314,
18.1429787280566));
#156578=CARTESIAN_POINT('Ctrl Pts',(-16.203505316394,-18.5644478664209,
18.1472948907955));
#156579=CARTESIAN_POINT('Ctrl Pts',(-16.1907740320855,-18.6475759012497,
18.1514704549872));
#156580=CARTESIAN_POINT('Ctrl Pts',(-16.1821523920334,-18.7312720295791,
18.1556460191789));
#156581=CARTESIAN_POINT('Ctrl Pts',(-16.177663165104,-18.8150986247193,
18.1598215833707));
#156582=CARTESIAN_POINT('Ctrl Pts',(-16.1729471979947,-18.9031591018972,
18.1642080453831));
#156583=CARTESIAN_POINT('Ctrl Pts',(-16.172792072363,-18.9913629881318,
18.1685945073955));
#156584=CARTESIAN_POINT('Ctrl Pts',(-16.1771623761344,-19.0792059950832,
18.1729809694079));
#156585=CARTESIAN_POINT('Ctrl Pts',(-16.1815326799057,-19.1670490020346,
18.1773674314203));
#156586=CARTESIAN_POINT('Ctrl Pts',(-16.1904282787085,-19.2545305601574,
18.1817538934327));
#156587=CARTESIAN_POINT('Ctrl Pts',(-16.2037517912765,-19.3411580684653,
18.1861403554451));
#156588=CARTESIAN_POINT('Ctrl Pts',(-16.2164587426292,-19.4237767869345,
18.1903238287685));
#156589=CARTESIAN_POINT('Ctrl Pts',(-16.2332401386084,-19.5059261893906,
18.1945073020919));
#156590=CARTESIAN_POINT('Ctrl Pts',(-16.2540494029908,-19.587173233373,
18.1986907754153));
#156591=CARTESIAN_POINT('Ctrl Pts',(-16.2748315365081,-19.6683143484509,
18.2028687943773));
#156592=CARTESIAN_POINT('Ctrl Pts',(-16.2996310005511,-19.7485549992219,
18.2070468133392));
#156593=CARTESIAN_POINT('Ctrl Pts',(-16.3283498001384,-19.8274696544744,
18.2112248323011));
#156594=CARTESIAN_POINT('Ctrl Pts',(-16.3570397744387,-19.9063051024616,
18.2153986577523));
#156595=CARTESIAN_POINT('Ctrl Pts',(-16.3896411161759,-19.9838167680114,
18.2195724832034));
#156596=CARTESIAN_POINT('Ctrl Pts',(-16.4260056863287,-20.0595929974775,
18.2237463086546));
#156597=CARTESIAN_POINT('Ctrl Pts',(-16.4623446674756,-20.1353159047572,
18.22791719707));
#156598=CARTESIAN_POINT('Ctrl Pts',(-16.5024414177659,-20.2093053885233,
18.2320880854853));
#156599=CARTESIAN_POINT('Ctrl Pts',(-16.5460997340582,-20.2811698259785,
18.2362589739007));
#156600=CARTESIAN_POINT('Ctrl Pts',(-16.5897512956127,-20.3530231446947,
18.2404292170036));
#156601=CARTESIAN_POINT('Ctrl Pts',(-16.6369631004863,-20.4227516709472,
18.2445994601065));
#156602=CARTESIAN_POINT('Ctrl Pts',(-16.6874935461469,-20.4899893804372,
18.2487697032093));
#156603=CARTESIAN_POINT('Ctrl Pts',(-16.7380175638218,-20.5572185366079,
18.2529394158149));
#156604=CARTESIAN_POINT('Ctrl Pts',(-16.7918591019332,-20.6219571415253,
18.2571091284205));
#156605=CARTESIAN_POINT('Ctrl Pts',(-16.8487348978594,-20.68387051902,18.2612788410261));
#156606=CARTESIAN_POINT('Ctrl Pts',(-16.9056490538446,-20.7458256541865,
18.2654513659075));
#156607=CARTESIAN_POINT('Ctrl Pts',(-16.9656012405057,-20.8049514194522,
18.2696238907889));
#156608=CARTESIAN_POINT('Ctrl Pts',(-17.0282702917711,-20.8609489680097,
18.2737964156702));
#156609=CARTESIAN_POINT('Ctrl Pts',(-17.0755086445449,-20.9031585100375,
18.2769415598574));
#156610=CARTESIAN_POINT('Ctrl Pts',(-17.1242898505219,-20.9435913986356,
18.2800867040446));
#156611=CARTESIAN_POINT('Ctrl Pts',(-17.1744641402402,-20.9821349467765,
18.2832318482317));
#156612=CARTESIAN_POINT('Origin',(-18.734,-18.952,-1.76670989022851));
#156613=CARTESIAN_POINT('',(-17.1767158074852,-20.9792339848999,19.149828714141));
#156614=CARTESIAN_POINT('',(-17.1744641402401,-20.9821349467764,19.0833436902736));
#156615=CARTESIAN_POINT('',(-17.1744641402401,-20.9821349467765,-1.76670989022851));
#156616=CARTESIAN_POINT('',(-21.2936055493641,-18.9516176052657,18.6332901348852));
#156617=CARTESIAN_POINT('Ctrl Pts',(-21.2898370902887,-18.9516133246636,
18.6332903748308));
#156618=CARTESIAN_POINT('Ctrl Pts',(-21.2903731169848,-18.5470182197254,
18.6533365919814));
#156619=CARTESIAN_POINT('Ctrl Pts',(-21.0089153450218,-17.2875283998103,
18.7157747446925));
#156620=CARTESIAN_POINT('Ctrl Pts',(-19.0350903615485,-15.9399184014086,
18.8206048329642));
#156621=CARTESIAN_POINT('Ctrl Pts',(-16.3642905510741,-17.0684480147839,
18.9477806396456));
#156622=CARTESIAN_POINT('Ctrl Pts',(-15.9356498827334,-19.5334126702652,
19.0575219333712));
#156623=CARTESIAN_POINT('Ctrl Pts',(-16.7788811058708,-20.6706543117871,
19.1248712915363));
#156624=CARTESIAN_POINT('Ctrl Pts',(-17.1767158074852,-20.9792339848999,
19.149828714141));
#156625=CARTESIAN_POINT('Ctrl Pts',(-17.1744641402401,-20.9821349467765,
18.3499540410247));
#156626=CARTESIAN_POINT('Ctrl Pts',(-17.2410773843612,-21.033306787893,
18.3541251225104));
#156627=CARTESIAN_POINT('Ctrl Pts',(-17.3102609913822,-21.0812343275469,
18.3582962039961));
#156628=CARTESIAN_POINT('Ctrl Pts',(-17.3816628382274,-21.1256568728502,
18.3624672854819));
#156629=CARTESIAN_POINT('Ctrl Pts',(-17.4530410707598,-21.1700647265463,
18.3666369874904));
#156630=CARTESIAN_POINT('Ctrl Pts',(-17.5266356958207,-21.2109696452565,
18.3708066894989));
#156631=CARTESIAN_POINT('Ctrl Pts',(-17.602065883165,-21.2481544275473,
18.3749763915074));
#156632=CARTESIAN_POINT('Ctrl Pts',(-17.6774937511192,-21.2853380664494,
18.3791459653024));
#156633=CARTESIAN_POINT('Ctrl Pts',(-17.754756656113,-21.3188015937751,
18.3833155390974));
#156634=CARTESIAN_POINT('Ctrl Pts',(-17.8334506937448,-21.3483745423041,
18.3874851128924));
#156635=CARTESIAN_POINT('Ctrl Pts',(-17.9145942070361,-21.3788679953565,
18.391784471228));
#156636=CARTESIAN_POINT('Ctrl Pts',(-17.9972589386759,-21.4052244645523,
18.3960838295637));
#156637=CARTESIAN_POINT('Ctrl Pts',(-18.0809835220192,-21.4273119963927,
18.4003831878993));
#156638=CARTESIAN_POINT('Ctrl Pts',(-18.1622979460154,-21.4487636997919,
18.4045587816455));
#156639=CARTESIAN_POINT('Ctrl Pts',(-18.244611554837,-21.4661888816975,
18.4087343753917));
#156640=CARTESIAN_POINT('Ctrl Pts',(-18.3274915789467,-21.4795187246809,
18.412909969138));
#156641=CARTESIAN_POINT('Ctrl Pts',(-18.4140564486528,-21.4934412124391,
18.4172712097683));
#156642=CARTESIAN_POINT('Ctrl Pts',(-18.5012387072319,-21.502895666993,
18.4216324503986));
#156643=CARTESIAN_POINT('Ctrl Pts',(-18.5885418386308,-21.5078642223896,
18.4259936910289));
#156644=CARTESIAN_POINT('Ctrl Pts',(-18.6758449700296,-21.5128327777861,
18.4303549316592));
#156645=CARTESIAN_POINT('Ctrl Pts',(-18.7632684101765,-21.5133155051365,
18.4347161722895));
#156646=CARTESIAN_POINT('Ctrl Pts',(-18.8503205710794,-21.5093559636358,
18.4390774129198));
#156647=CARTESIAN_POINT('Ctrl Pts',(-18.9338475986689,-21.5055567617696,
18.4432620473123));
#156648=CARTESIAN_POINT('Ctrl Pts',(-19.0173437395027,-21.4976540121366,
18.4474466817047));
#156649=CARTESIAN_POINT('Ctrl Pts',(-19.1003730904689,-21.4856477179317,
18.4516313160972));
#156650=CARTESIAN_POINT('Ctrl Pts',(-19.1832842594309,-21.4736585132005,
18.4558099941805));
#156651=CARTESIAN_POINT('Ctrl Pts',(-19.2657295068645,-21.4575774310127,
18.4599886722639));
#156652=CARTESIAN_POINT('Ctrl Pts',(-19.3472750579131,-21.437456437627,
18.4641673503472));
#156653=CARTESIAN_POINT('Ctrl Pts',(-19.4302822543734,-21.4169747898919,
18.4684209282328));
#156654=CARTESIAN_POINT('Ctrl Pts',(-19.5123567014418,-21.3923069974992,
18.4726745061184));
#156655=CARTESIAN_POINT('Ctrl Pts',(-19.5930485432779,-21.3635628957778,
18.476928084004));
#156656=CARTESIAN_POINT('Ctrl Pts',(-19.6721760162886,-21.3353760545629,
18.4810991979813));
#156657=CARTESIAN_POINT('Ctrl Pts',(-19.7499735613546,-21.3032697094725,
18.4852703119587));
#156658=CARTESIAN_POINT('Ctrl Pts',(-19.8260310897304,-21.2673980433313,
18.489441425936));
#156659=CARTESIAN_POINT('Ctrl Pts',(-19.9020630962678,-21.2315384142742,
18.4936111402558));
#156660=CARTESIAN_POINT('Ctrl Pts',(-19.9763558299771,-21.1919161695522,
18.4977808545756));
#156661=CARTESIAN_POINT('Ctrl Pts',(-20.0485201368017,-21.1487332131925,
18.5019505688953));
#156662=CARTESIAN_POINT('Ctrl Pts',(-20.1206818757106,-21.1055517934676,
18.5061201348388));
#156663=CARTESIAN_POINT('Ctrl Pts',(-20.1907149440062,-21.058810150979,
18.5102897007822));
#156664=CARTESIAN_POINT('Ctrl Pts',(-20.2582569041575,-21.0087549416807,
18.5144592667256));
#156665=CARTESIAN_POINT('Ctrl Pts',(-20.3281735563277,-20.9569398529571,
18.5187754294653));
#156666=CARTESIAN_POINT('Ctrl Pts',(-20.3954202425923,-20.9015741660665,
18.5230915922049));
#156667=CARTESIAN_POINT('Ctrl Pts',(-20.4596314884386,-20.8429775160242,
18.5274077549445));
#156668=CARTESIAN_POINT('Ctrl Pts',(-20.5217510596858,-20.7862896457116,
18.5315833191356));
#156669=CARTESIAN_POINT('Ctrl Pts',(-20.5810296141589,-20.7265784444846,
18.5357588833267));
#156670=CARTESIAN_POINT('Ctrl Pts',(-20.6371745600421,-20.6641701416649,
18.5399344475178));
#156671=CARTESIAN_POINT('Ctrl Pts',(-20.6961552536971,-20.5986097438011,
18.5443209095317));
#156672=CARTESIAN_POINT('Ctrl Pts',(-20.7516770948084,-20.5300730764183,
18.5487073715456));
#156673=CARTESIAN_POINT('Ctrl Pts',(-20.8034508935152,-20.4589747839062,
18.5530938335595));
#156674=CARTESIAN_POINT('Ctrl Pts',(-20.8552246922221,-20.387876491394,
18.5574802955735));
#156675=CARTESIAN_POINT('Ctrl Pts',(-20.9032501953501,-20.3142171013321,
18.5618667575874));
#156676=CARTESIAN_POINT('Ctrl Pts',(-20.9472937739973,-20.238441086869,
18.5662532196013));
#156677=CARTESIAN_POINT('Ctrl Pts',(-20.9909726387703,-20.1632925546555,
18.5706033584189));
#156678=CARTESIAN_POINT('Ctrl Pts',(-21.0308877830082,-20.0858014915382,
18.5749534972364));
#156679=CARTESIAN_POINT('Ctrl Pts',(-21.066791372662,-20.0063644586356,
18.579303636054));
#156680=CARTESIAN_POINT('Ctrl Pts',(-21.1039225287105,-19.9242114234328,
18.5838025088638));
#156681=CARTESIAN_POINT('Ctrl Pts',(-21.1367625751618,-19.839977276334,
18.5883013816736));
#156682=CARTESIAN_POINT('Ctrl Pts',(-21.1650869626509,-19.7541322709059,
18.5928002544834));
#156683=CARTESIAN_POINT('Ctrl Pts',(-21.1923645588308,-19.6714598603191,
18.5971328613515));
#156684=CARTESIAN_POINT('Ctrl Pts',(-21.2154541944231,-19.5872939815202,
18.6014654682196));
#156685=CARTESIAN_POINT('Ctrl Pts',(-21.2342029378176,-19.5020775124729,
18.6057980750877));
#156686=CARTESIAN_POINT('Ctrl Pts',(-21.252927481766,-19.4169710343355,
18.6101250897577));
#156687=CARTESIAN_POINT('Ctrl Pts',(-21.267322189726,-19.330817060707,18.6144521044277));
#156688=CARTESIAN_POINT('Ctrl Pts',(-21.2772839154191,-19.2440734934402,
18.6187791190978));
#156689=CARTESIAN_POINT('Ctrl Pts',(-21.2872318317731,-19.1574501735453,
18.6231001354886));
#156690=CARTESIAN_POINT('Ctrl Pts',(-21.2927589555484,-19.0702392928319,
18.6274211518793));
#156691=CARTESIAN_POINT('Ctrl Pts',(-21.2938134141943,-18.9829076772209,
18.6317421682701));
#156692=CARTESIAN_POINT('Ctrl Pts',(-21.2939393290371,-18.9724792486627,
18.6322581487706));
#156693=CARTESIAN_POINT('Ctrl Pts',(-21.2940015277989,-18.9620491070299,
18.632774129271));
#156694=CARTESIAN_POINT('Ctrl Pts',(-21.2939999715072,-18.9516180532908,
18.6332901097715));
#156695=CARTESIAN_POINT('',(-21.2939999971965,-18.9518801919504,18.5667098901964));
#156696=CARTESIAN_POINT('Ctrl Pts',(-17.1744641402402,-20.9821349467765,
18.2832318482317));
#156697=CARTESIAN_POINT('Ctrl Pts',(-17.2411082793406,-21.0333305212062,
18.2874093946978));
#156698=CARTESIAN_POINT('Ctrl Pts',(-17.3102108974908,-21.0811910583105,
18.2915869411639));
#156699=CARTESIAN_POINT('Ctrl Pts',(-17.3813969214214,-21.1254914105696,
18.29576448763));
#156700=CARTESIAN_POINT('Ctrl Pts',(-17.4526989816651,-21.1698639743284,
18.2999488436784));
#156701=CARTESIAN_POINT('Ctrl Pts',(-17.5260908238986,-21.2106645484754,
18.3041331997268));
#156702=CARTESIAN_POINT('Ctrl Pts',(-17.601173651747,-21.2477143691461,
18.3083175557752));
#156703=CARTESIAN_POINT('Ctrl Pts',(-17.6310714819674,-21.2624675328168,
18.3099837578923));
#156704=CARTESIAN_POINT('Ctrl Pts',(-17.6612372295859,-21.2766265133864,
18.3116499600094));
#156705=CARTESIAN_POINT('Ctrl Pts',(-17.6916449845513,-21.2901822045702,
18.3133161621265));
#156706=CARTESIAN_POINT('Ctrl Pts',(-17.7680134730656,-21.3242270608135,
18.3175007965194));
#156707=CARTESIAN_POINT('Ctrl Pts',(-17.8461937671324,-21.3545898770089,
18.3216854309123));
#156708=CARTESIAN_POINT('Ctrl Pts',(-17.925796207947,-21.3810752624221,
18.3258700653053));
#156709=CARTESIAN_POINT('Ctrl Pts',(-18.0052853445399,-21.4075229491675,
18.3300487433891));
#156710=CARTESIAN_POINT('Ctrl Pts',(-18.0861921743113,-21.4301040236941,
18.3342274214729));
#156711=CARTESIAN_POINT('Ctrl Pts',(-18.1681056484756,-21.4486704994678,
18.3384060995568));
#156712=CARTESIAN_POINT('Ctrl Pts',(-18.251487362797,-21.4675697659769,
18.3426596774422));
#156713=CARTESIAN_POINT('Ctrl Pts',(-18.3359117243118,-21.4823088984315,
18.3469132553277));
#156714=CARTESIAN_POINT('Ctrl Pts',(-18.4209273694976,-21.4927844316333,
18.3511668332132));
#156715=CARTESIAN_POINT('Ctrl Pts',(-18.5042948205042,-21.5030568761823,
18.355337947191));
#156716=CARTESIAN_POINT('Ctrl Pts',(-18.5882303557904,-21.5092295037566,
18.3595090611688));
#156717=CARTESIAN_POINT('Ctrl Pts',(-18.6722982811996,-21.5112563173502,
18.3636801751467));
#156718=CARTESIAN_POINT('Ctrl Pts',(-18.7563379968046,-21.513282450827,
18.3678498894669));
#156719=CARTESIAN_POINT('Ctrl Pts',(-18.8405095547876,-21.5111655221263,
18.3720196037872));
#156720=CARTESIAN_POINT('Ctrl Pts',(-18.9243745836511,-21.5049115765924,
18.3761893181074));
#156721=CARTESIAN_POINT('Ctrl Pts',(-19.0082366282369,-21.4986578536008,
18.3803588840514));
#156722=CARTESIAN_POINT('Ctrl Pts',(-19.0917917066946,-21.4882674415332,
18.3845284499953));
#156723=CARTESIAN_POINT('Ctrl Pts',(-19.1746052695948,-21.4737983655331,
18.3886980159392));
#156724=CARTESIAN_POINT('Ctrl Pts',(-19.2603304552102,-21.4588205746695,
18.3930141786783));
#156725=CARTESIAN_POINT('Ctrl Pts',(-19.3452604921636,-21.4394720625983,
18.3973303414173));
#156726=CARTESIAN_POINT('Ctrl Pts',(-19.4289254033754,-21.4158747297181,
18.4016465041564));
#156727=CARTESIAN_POINT('Ctrl Pts',(-19.5098649388997,-21.3930460774759,
18.405822068348));
#156728=CARTESIAN_POINT('Ctrl Pts',(-19.5896200744145,-21.3662413589924,
18.4099976325395));
#156729=CARTESIAN_POINT('Ctrl Pts',(-19.6677830273837,-21.3356210390434,
18.4141731967311));
#156730=CARTESIAN_POINT('Ctrl Pts',(-19.7498938052997,-21.3034541595238,
18.4185596587439));
#156731=CARTESIAN_POINT('Ctrl Pts',(-19.8302467994652,-21.2670763374215,
18.4229461207567));
#156732=CARTESIAN_POINT('Ctrl Pts',(-19.9083976363218,-21.226728597394,
18.4273325827695));
#156733=CARTESIAN_POINT('Ctrl Pts',(-19.9865484731783,-21.1863808573664,
18.4317190447823));
#156734=CARTESIAN_POINT('Ctrl Pts',(-20.0624966899234,-21.1420635575359,
18.4361055067951));
#156735=CARTESIAN_POINT('Ctrl Pts',(-20.1358342086536,-21.0940692919344,
18.4404919688079));
#156736=CARTESIAN_POINT('Ctrl Pts',(-20.2057039471169,-21.0483444454524,
18.4446710160258));
#156737=CARTESIAN_POINT('Ctrl Pts',(-20.2734659150701,-20.9991112651902,
18.4488500632436));
#156738=CARTESIAN_POINT('Ctrl Pts',(-20.3387454860835,-20.9465906660001,
18.4530291104615));
#156739=CARTESIAN_POINT('Ctrl Pts',(-20.4039320790896,-20.8941448721524,
18.4572022054423));
#156740=CARTESIAN_POINT('Ctrl Pts',(-20.46664294125,-20.8384212459577,18.461375300423));
#156741=CARTESIAN_POINT('Ctrl Pts',(-20.5265316718116,-20.7796843834624,
18.4655483954038));
#156742=CARTESIAN_POINT('Ctrl Pts',(-20.5870226816093,-20.7203568256503,
18.4697634576868));
#156743=CARTESIAN_POINT('Ctrl Pts',(-20.6446340707897,-20.6579553356914,
18.4739785199699));
#156744=CARTESIAN_POINT('Ctrl Pts',(-20.6990425114804,-20.5927949073771,
18.4781935822529));
#156745=CARTESIAN_POINT('Ctrl Pts',(-20.7528122887531,-20.528399352699,
18.4823591668069));
#156746=CARTESIAN_POINT('Ctrl Pts',(-20.803453612438,-20.4613096522777,
18.4865247513609));
#156747=CARTESIAN_POINT('Ctrl Pts',(-20.8506921231955,-20.3918661241943,
18.4906903359149));
#156748=CARTESIAN_POINT('Ctrl Pts',(-20.8979149500345,-20.3224456524396,
18.4948545374302));
#156749=CARTESIAN_POINT('Ctrl Pts',(-20.9417369482816,-20.2506732862343,
18.4990187389455));
#156750=CARTESIAN_POINT('Ctrl Pts',(-20.9819260328718,-20.1769198140031,
18.5031829404608));
#156751=CARTESIAN_POINT('Ctrl Pts',(-21.0221139173366,-20.1031685441961,
18.5073470176248));
#156752=CARTESIAN_POINT('Ctrl Pts',(-21.0586688839111,-20.0274366916314,
18.5115110947889));
#156753=CARTESIAN_POINT('Ctrl Pts',(-21.0914046022627,-19.9501200034218,
18.5156751719529));
#156754=CARTESIAN_POINT('Ctrl Pts',(-21.1248385440614,-19.8711542197507,
18.5199280651399));
#156755=CARTESIAN_POINT('Ctrl Pts',(-21.1542882228969,-19.7905356687051,
18.5241809583268));
#156756=CARTESIAN_POINT('Ctrl Pts',(-21.1796074785074,-19.7087060598863,
18.5284338515138));
#156757=CARTESIAN_POINT('Ctrl Pts',(-21.2044336791703,-19.6284699613236,
18.5326039259141));
#156758=CARTESIAN_POINT('Ctrl Pts',(-21.2252888283687,-19.5470700198229,
18.5367740003145));
#156759=CARTESIAN_POINT('Ctrl Pts',(-21.2420864983913,-19.4649348073461,
18.5409440747148));
#156760=CARTESIAN_POINT('Ctrl Pts',(-21.2593845777048,-19.3803527541243,
18.5452383772951));
#156761=CARTESIAN_POINT('Ctrl Pts',(-21.2723795196075,-19.294991452669,
18.5495326798753));
#156762=CARTESIAN_POINT('Ctrl Pts',(-21.2810343673868,-19.2093245642189,
18.5538269824556));
#156763=CARTESIAN_POINT('Ctrl Pts',(-21.2896892151661,-19.1236576757689,
18.5581212850359));
#156764=CARTESIAN_POINT('Ctrl Pts',(-21.2940040128973,-19.0376857298059,
18.5624155876161));
#156765=CARTESIAN_POINT('Ctrl Pts',(-21.2939999971965,-18.9518801919504,
18.5667098901964));
#156766=CARTESIAN_POINT('Ctrl Pts',(-21.2939999971965,-18.9518801913084,
18.5667098902285));
#156767=CARTESIAN_POINT('Ctrl Pts',(-21.2939996986147,-18.945500276023,
18.5670291853155));
#156768=CARTESIAN_POINT('Ctrl Pts',(-21.2939755504833,-18.939120426077,
18.5673484804024));
#156769=CARTESIAN_POINT('Ctrl Pts',(-21.2939275539577,-18.9327407557766,
18.5676677754894));
#156770=CARTESIAN_POINT('Ctrl Pts',(-21.2932985185608,-18.84912973624,18.5718524098819));
#156771=CARTESIAN_POINT('Ctrl Pts',(-21.2885677156651,-18.7653939703417,
18.5760370442745));
#156772=CARTESIAN_POINT('Ctrl Pts',(-21.2797186185528,-18.6819690477864,
18.580221678667));
#156773=CARTESIAN_POINT('Ctrl Pts',(-21.2708821170351,-18.5986628702825,
18.5844003567505));
#156774=CARTESIAN_POINT('Ctrl Pts',(-21.2579390129528,-18.5156671108363,
18.5885790348339));
#156775=CARTESIAN_POINT('Ctrl Pts',(-21.2409247859828,-18.4334172029223,
18.5927577129174));
#156776=CARTESIAN_POINT('Ctrl Pts',(-21.2236055912197,-18.3496930245084,
18.5970112908029));
#156777=CARTESIAN_POINT('Ctrl Pts',(-21.2020678918843,-18.2667421815314,
18.6012648686885));
#156778=CARTESIAN_POINT('Ctrl Pts',(-21.1764043852929,-18.1850183713399,
18.605518446574));
#156779=CARTESIAN_POINT('Ctrl Pts',(-21.1512384158586,-18.1048789366916,
18.6096895605515));
#156780=CARTESIAN_POINT('Ctrl Pts',(-21.1221053294157,-18.02591984166,18.613860674529));
#156781=CARTESIAN_POINT('Ctrl Pts',(-21.0891436468891,-17.9485567268061,
18.6180317885064));
#156782=CARTESIAN_POINT('Ctrl Pts',(-21.0561930249733,-17.8712195718925,
18.6222015028263));
#156783=CARTESIAN_POINT('Ctrl Pts',(-21.0194165386218,-17.7954777564205,
18.6263712171462));
#156784=CARTESIAN_POINT('Ctrl Pts',(-20.9790011895035,-17.721727810959,
18.6305409314661));
#156785=CARTESIAN_POINT('Ctrl Pts',(-20.9385872785368,-17.6479804898368,
18.6347104974097));
#156786=CARTESIAN_POINT('Ctrl Pts',(-20.8945349840831,-17.5762253008168,
18.6388800633532));
#156787=CARTESIAN_POINT('Ctrl Pts',(-20.8470770406693,-17.5068337741989,
18.6430496292968));
#156788=CARTESIAN_POINT('Ctrl Pts',(-20.7979505344986,-17.4350025270909,
18.6473657920363));
#156789=CARTESIAN_POINT('Ctrl Pts',(-20.7451747360216,-17.3657046830186,
18.6516819547758));
#156790=CARTESIAN_POINT('Ctrl Pts',(-20.6890551911698,-17.2993175745231,
18.6559981175153));
#156791=CARTESIAN_POINT('Ctrl Pts',(-20.6347637346021,-17.23509301912,18.6601736817065));
#156792=CARTESIAN_POINT('Ctrl Pts',(-20.5773433873059,-17.173592789127,
18.6643492458977));
#156793=CARTESIAN_POINT('Ctrl Pts',(-20.5171090485652,-17.1151216368728,
18.668524810089));
#156794=CARTESIAN_POINT('Ctrl Pts',(-20.4538324165453,-17.0536972456979,
18.6729112721026));
#156795=CARTESIAN_POINT('Ctrl Pts',(-20.3874504923529,-16.9956163559344,
18.6772977341163));
#156796=CARTESIAN_POINT('Ctrl Pts',(-20.3183666557521,-16.9411836731962,
18.6816841961299));
#156797=CARTESIAN_POINT('Ctrl Pts',(-20.2492828191514,-16.886750990458,
18.6860706581436));
#156798=CARTESIAN_POINT('Ctrl Pts',(-20.1774975877418,-16.835966787744,
18.6904571201572));
#156799=CARTESIAN_POINT('Ctrl Pts',(-20.1034462555221,-16.7890813808105,
18.6948435821709));
#156800=CARTESIAN_POINT('Ctrl Pts',(-20.0328021348959,-16.7443532409684,
18.6990282165633));
#156801=CARTESIAN_POINT('Ctrl Pts',(-19.9598329133702,-16.703006515634,
18.7032128509558));
#156802=CARTESIAN_POINT('Ctrl Pts',(-19.8848959073542,-16.665290877607,
18.7073974853483));
#156803=CARTESIAN_POINT('Ctrl Pts',(-19.810065564891,-16.6276289231225,
18.7115761634316));
#156804=CARTESIAN_POINT('Ctrl Pts',(-19.7332734088094,-16.5935879949175,
18.715754841515));
#156805=CARTESIAN_POINT('Ctrl Pts',(-19.6549047742285,-16.5633739520798,
18.7199335195983));
#156806=CARTESIAN_POINT('Ctrl Pts',(-19.5751314381812,-16.5326183442331,
18.7241870974839));
#156807=CARTESIAN_POINT('Ctrl Pts',(-19.4937249583384,-16.5058284229432,
18.7284406753695));
#156808=CARTESIAN_POINT('Ctrl Pts',(-19.4111169976703,-16.4831718222068,
18.7326942532551));
#156809=CARTESIAN_POINT('Ctrl Pts',(-19.3301105535305,-16.4609544638903,
18.7368653672324));
#156810=CARTESIAN_POINT('Ctrl Pts',(-19.247949263021,-16.4427117186153,
18.7410364812098));
#156811=CARTESIAN_POINT('Ctrl Pts',(-19.1650575928263,-16.4285520905581,
18.7452075951871));
#156812=CARTESIAN_POINT('Ctrl Pts',(-19.0821937377322,-16.4143972139008,
18.7493773095069));
#156813=CARTESIAN_POINT('Ctrl Pts',(-18.9986004427846,-16.4043228107593,
18.7535470238266));
#156814=CARTESIAN_POINT('Ctrl Pts',(-18.9147123478962,-16.3983862767995,
18.7577167381464));
#156815=CARTESIAN_POINT('Ctrl Pts',(-18.8308272381063,-16.3924499540871,
18.7618863040898));
#156816=CARTESIAN_POINT('Ctrl Pts',(-18.7466478081782,-16.3906512394234,
18.7660558700333));
#156817=CARTESIAN_POINT('Ctrl Pts',(-18.6626124310835,-16.3929955422071,
18.7702254359767));
#156818=CARTESIAN_POINT('Ctrl Pts',(-18.5756224737719,-16.3954222677853,
18.7745415987163));
#156819=CARTESIAN_POINT('Ctrl Pts',(-18.4887874147824,-16.4022887536938,
18.778857761456));
#156820=CARTESIAN_POINT('Ctrl Pts',(-18.4025899172854,-16.4135423271059,
18.7831739241956));
#156821=CARTESIAN_POINT('Ctrl Pts',(-18.319200294229,-16.4244293165443,
18.7873494883867));
#156822=CARTESIAN_POINT('Ctrl Pts',(-18.2364077885012,-16.439421833601,
18.7915250525777));
#156823=CARTESIAN_POINT('Ctrl Pts',(-18.1546390975922,-16.4584200544676,
18.7957006167688));
#156824=CARTESIAN_POINT('Ctrl Pts',(-18.0687404644525,-16.4783778303154,
18.8000870787827));
#156825=CARTESIAN_POINT('Ctrl Pts',(-17.9839723511228,-16.5027564393572,
18.8044735407966));
#156826=CARTESIAN_POINT('Ctrl Pts',(-17.9008093086194,-16.5313816344172,
18.8088600028106));
#156827=CARTESIAN_POINT('Ctrl Pts',(-17.8176462661159,-16.5600068294773,
18.8132464648245));
#156828=CARTESIAN_POINT('Ctrl Pts',(-17.7360888041544,-16.5928783231054,
18.8176329268384));
#156829=CARTESIAN_POINT('Ctrl Pts',(-17.6565830150583,-16.6297655931067,
18.8220193888523));
#156830=CARTESIAN_POINT('Ctrl Pts',(-17.5807354051422,-16.6649556251501,
18.8262040232484));
#156831=CARTESIAN_POINT('Ctrl Pts',(-17.5064724966934,-16.70393099464,18.8303886576446));
#156832=CARTESIAN_POINT('Ctrl Pts',(-17.4341976336204,-16.7465263981734,
18.8345732920407));
#156833=CARTESIAN_POINT('Ctrl Pts',(-17.3620256448689,-16.7890611724222,
18.8387519701277));
#156834=CARTESIAN_POINT('Ctrl Pts',(-17.2918364736807,-16.8352055143126,
18.8429306482147));
#156835=CARTESIAN_POINT('Ctrl Pts',(-17.2240117895626,-16.8847468456089,
18.8471093263018));
#156836=CARTESIAN_POINT('Ctrl Pts',(-17.1549713967899,-16.9351761696176,
18.8513629041864));
#156837=CARTESIAN_POINT('Ctrl Pts',(-17.0883815290666,-16.9891252600227,
18.8556164820711));
#156838=CARTESIAN_POINT('Ctrl Pts',(-17.0246167910329,-17.0463218936816,
18.8598700599558));
#156839=CARTESIAN_POINT('Ctrl Pts',(-16.9620882568152,-17.1024096590385,
18.8640411739368));
#156840=CARTESIAN_POINT('Ctrl Pts',(-16.9022766467381,-17.1616198500931,
18.8682122879178));
#156841=CARTESIAN_POINT('Ctrl Pts',(-16.8455029514086,-17.223654288789,
18.8723834018988));
#156842=CARTESIAN_POINT('Ctrl Pts',(-16.7887483070409,-17.2856679112298,
18.8765531162223));
#156843=CARTESIAN_POINT('Ctrl Pts',(-16.7350298631989,-17.3505035600764,
18.8807228305457));
#156844=CARTESIAN_POINT('Ctrl Pts',(-16.6846311428961,-17.4178268391304,
18.8848925448692));
#156845=CARTESIAN_POINT('Ctrl Pts',(-16.6342342159962,-17.4851477225331,
18.8890621108163));
#156846=CARTESIAN_POINT('Ctrl Pts',(-16.5871570527719,-17.5549556913587,
18.8932316767634));
#156847=CARTESIAN_POINT('Ctrl Pts',(-16.5436414846469,-17.6268850713165,
18.8974012427105));
#156848=CARTESIAN_POINT('Ctrl Pts',(-16.4985959629,-17.7013433994214,18.9017174054458));
#156849=CARTESIAN_POINT('Ctrl Pts',(-16.4573674204997,-17.7780746406049,
18.906033568181));
#156850=CARTESIAN_POINT('Ctrl Pts',(-16.4201728243532,-17.8566444407234,
18.9103497309163));
#156851=CARTESIAN_POINT('Ctrl Pts',(-16.3841898382076,-17.9326548379861,
18.914525295111));
#156852=CARTESIAN_POINT('Ctrl Pts',(-16.3519821593661,-18.0103853983063,
18.9187008593057));
#156853=CARTESIAN_POINT('Ctrl Pts',(-16.3236968150621,-18.0894233038864,
18.9228764235003));
#156854=CARTESIAN_POINT('Ctrl Pts',(-16.293982845328,-18.1724532259908,
18.9272628855059));
#156855=CARTESIAN_POINT('Ctrl Pts',(-16.2685980256123,-18.2569254729983,
18.9316493475114));
#156856=CARTESIAN_POINT('Ctrl Pts',(-16.2476527070797,-18.3423467059155,
18.936035809517));
#156857=CARTESIAN_POINT('Ctrl Pts',(-16.2267073885472,-18.4277679388328,
18.9404222715226));
#156858=CARTESIAN_POINT('Ctrl Pts',(-16.210201605397,-18.5141375734783,
18.9448087335281));
#156859=CARTESIAN_POINT('Ctrl Pts',(-16.1981829862585,-18.6009557395151,
18.9491951955337));
#156860=CARTESIAN_POINT('Ctrl Pts',(-16.1867173615959,-18.6837792730849,
18.9533798299225));
#156861=CARTESIAN_POINT('Ctrl Pts',(-16.1792923755172,-18.7673192548711,
18.9575644643113));
#156862=CARTESIAN_POINT('Ctrl Pts',(-16.1759873564286,-18.8511470608817,
18.9617490987001));
#156863=CARTESIAN_POINT('Ctrl Pts',(-16.1726870416255,-18.9348555483864,
18.9659277767798));
#156864=CARTESIAN_POINT('Ctrl Pts',(-16.173495063509,-19.0188505906136,
18.9701064548595));
#156865=CARTESIAN_POINT('Ctrl Pts',(-16.1784392678898,-19.1026961993429,
18.9742851329392));
#156866=CARTESIAN_POINT('Ctrl Pts',(-16.1834720935871,-19.1880446804576,
18.9785387108257));
#156867=CARTESIAN_POINT('Ctrl Pts',(-16.1927909085455,-19.2732378406053,
18.9827922887122));
#156868=CARTESIAN_POINT('Ctrl Pts',(-16.2063695825694,-19.3578133473402,
18.9870458665987));
#156869=CARTESIAN_POINT('Ctrl Pts',(-16.219685007484,-19.4407491927378,
18.9912169805725));
#156870=CARTESIAN_POINT('Ctrl Pts',(-16.2370965177702,-19.5230906447079,
18.9953880945462));
#156871=CARTESIAN_POINT('Ctrl Pts',(-16.2585271389983,-19.6044064028225,
18.99955920852));
#156872=CARTESIAN_POINT('Ctrl Pts',(-16.2799505689745,-19.6856948746497,
19.0037289228362));
#156873=CARTESIAN_POINT('Ctrl Pts',(-16.3053903143092,-19.7659578916982,
19.0078986371525));
#156874=CARTESIAN_POINT('Ctrl Pts',(-16.3347186663492,-19.8447760536633,
19.0120683514687));
#156875=CARTESIAN_POINT('Ctrl Pts',(-16.3640459747607,-19.9235914109407,
19.0162379174086));
#156876=CARTESIAN_POINT('Ctrl Pts',(-16.3972614535251,-20.0009615845047,
19.0204074833485));
#156877=CARTESIAN_POINT('Ctrl Pts',(-16.4341885271963,-20.0764852998419,
19.0245770492885));
#156878=CARTESIAN_POINT('Ctrl Pts',(-16.472413911305,-20.1546643360088,
19.0288932120324));
#156879=CARTESIAN_POINT('Ctrl Pts',(-16.5146165141598,-20.2308641813283,
19.0332093747763));
#156880=CARTESIAN_POINT('Ctrl Pts',(-16.5605485527334,-20.3046672933041,
19.0375255375201));
#156881=CARTESIAN_POINT('Ctrl Pts',(-16.6049843598882,-20.3760662765199,
19.0417011017078));
#156882=CARTESIAN_POINT('Ctrl Pts',(-16.6529100541809,-20.4452219153924,
19.0458766658955));
#156883=CARTESIAN_POINT('Ctrl Pts',(-16.7040581042264,-20.5117871328431,
19.0500522300832));
#156884=CARTESIAN_POINT('Ctrl Pts',(-16.7577895208536,-20.5817144014006,
19.0544386921052));
#156885=CARTESIAN_POINT('Ctrl Pts',(-16.815076991294,-20.6487822429872,
19.0588251541272));
#156886=CARTESIAN_POINT('Ctrl Pts',(-16.8755654265139,-20.7126308346929,
19.0632116161492));
#156887=CARTESIAN_POINT('Ctrl Pts',(-16.9360538617338,-20.7764794263986,
19.0675980781712));
#156888=CARTESIAN_POINT('Ctrl Pts',(-16.9997427890403,-20.8371084232607,
19.0719845401931));
#156889=CARTESIAN_POINT('Ctrl Pts',(-17.066237677054,-20.8942072068041,
19.0763710022151));
#156890=CARTESIAN_POINT('Ctrl Pts',(-17.1014709401622,-20.9244618101855,
19.078695231568));
#156891=CARTESIAN_POINT('Ctrl Pts',(-17.1375640758584,-20.9537885682649,
19.0810194609208));
#156892=CARTESIAN_POINT('Ctrl Pts',(-17.1744641402401,-20.9821349467764,
19.0833436902736));
#156893=CARTESIAN_POINT('Origin',(-18.734,-18.952,-1.76670989022851));
#156894=CARTESIAN_POINT('',(-17.1744641402401,-20.9821349467765,19.9498236254873));
#156895=CARTESIAN_POINT('',(-17.1744641402401,-20.9821349467765,19.8833624839903));
#156896=CARTESIAN_POINT('',(-17.1744641402401,-20.9821349467765,-1.76670989022851));
#156897=CARTESIAN_POINT('',(-21.2939990581247,-18.9498040034555,19.4332901097715));
#156898=CARTESIAN_POINT('Ctrl Pts',(-21.2939990581247,-18.9498040034555,
19.4332901097715));
#156899=CARTESIAN_POINT('Ctrl Pts',(-21.2938905873826,-18.8233534412897,
19.4395926510315));
#156900=CARTESIAN_POINT('Ctrl Pts',(-21.2844099378408,-18.6972910724131,
19.4458951922915));
#156901=CARTESIAN_POINT('Ctrl Pts',(-21.2657470116111,-18.5727150554023,
19.4521977335515));
#156902=CARTESIAN_POINT('Ctrl Pts',(-21.2615163488077,-18.544475158032,
19.4536264444915));
#156903=CARTESIAN_POINT('Ctrl Pts',(-21.25681399964,-18.5163115073431,19.4550551554314));
#156904=CARTESIAN_POINT('Ctrl Pts',(-21.2516424693647,-18.4882367021301,
19.4564838663713));
#156905=CARTESIAN_POINT('Ctrl Pts',(-21.2364952751732,-18.4060067810402,
19.4606685004929));
#156906=CARTESIAN_POINT('Ctrl Pts',(-21.2172870302558,-18.3243667083798,
19.4648531346144));
#156907=CARTESIAN_POINT('Ctrl Pts',(-21.1940771445919,-18.2437483196936,
19.469037768736));
#156908=CARTESIAN_POINT('Ctrl Pts',(-21.1709002953281,-18.1632446813081,
19.4732164465487));
#156909=CARTESIAN_POINT('Ctrl Pts',(-21.1437332452338,-18.0837602766129,
19.4773951243614));
#156910=CARTESIAN_POINT('Ctrl Pts',(-21.112686592475,-18.0057177509962,
19.4815738021741));
#156911=CARTESIAN_POINT('Ctrl Pts',(-21.0810834482228,-17.9262763627721,
19.4858273801273));
#156912=CARTESIAN_POINT('Ctrl Pts',(-21.0454603362217,-17.8483295278292,
19.4900809580806));
#156913=CARTESIAN_POINT('Ctrl Pts',(-21.0059873754064,-17.7723079359452,
19.4943345360339));
#156914=CARTESIAN_POINT('Ctrl Pts',(-20.967279678073,-17.697760176956,19.4985056497431));
#156915=CARTESIAN_POINT('Ctrl Pts',(-20.9248702958461,-17.6250641047766,
19.5026767634523));
#156916=CARTESIAN_POINT('Ctrl Pts',(-20.8789678617061,-17.5546049691487,
19.5068478771615));
#156917=CARTESIAN_POINT('Ctrl Pts',(-20.8330808305555,-17.4841694767402,
19.5110175912147));
#156918=CARTESIAN_POINT('Ctrl Pts',(-20.7837033262562,-17.4159698152611,
19.5151873052678));
#156919=CARTESIAN_POINT('Ctrl Pts',(-20.7310884046656,-17.3503639914293,
19.519357019321));
#156920=CARTESIAN_POINT('Ctrl Pts',(-20.6784753553166,-17.2847605021054,
19.5235265849996));
#156921=CARTESIAN_POINT('Ctrl Pts',(-20.6226254062025,-17.2217510252597,
19.5276961506783));
#156922=CARTESIAN_POINT('Ctrl Pts',(-20.5638323065115,-17.1616610013612,
19.5318657163569));
#156923=CARTESIAN_POINT('Ctrl Pts',(-20.5029721055919,-17.0994582777943,
19.5361818794149));
#156924=CARTESIAN_POINT('Ctrl Pts',(-20.4389583090022,-17.0403845006845,
19.5404980424729));
#156925=CARTESIAN_POINT('Ctrl Pts',(-20.3721573781207,-16.9847581733532,
19.5448142055309));
#156926=CARTESIAN_POINT('Ctrl Pts',(-20.3075324893086,-16.9309438750886,
19.5489897694644));
#156927=CARTESIAN_POINT('Ctrl Pts',(-20.2402996649794,-16.8803561190116,
19.553165333398));
#156928=CARTESIAN_POINT('Ctrl Pts',(-20.1708219663603,-16.8332403069284,
19.5573408973316));
#156929=CARTESIAN_POINT('Ctrl Pts',(-20.0978350997288,-16.7837447772679,
19.5617273599518));
#156930=CARTESIAN_POINT('Ctrl Pts',(-20.0223711203466,-16.738081448703,
19.566113822572));
#156931=CARTESIAN_POINT('Ctrl Pts',(-19.9448802162024,-16.6964803033426,
19.5705002851921));
#156932=CARTESIAN_POINT('Ctrl Pts',(-19.8673893120582,-16.6548791579822,
19.5748867478123));
#156933=CARTESIAN_POINT('Ctrl Pts',(-19.7878720403135,-16.6173403747379,
19.5792732104325));
#156934=CARTESIAN_POINT('Ctrl Pts',(-19.706800567316,-16.5840348279103,
19.5836596730527));
#156935=CARTESIAN_POINT('Ctrl Pts',(-19.6294593229195,-16.5522617227512,
19.587844307487));
#156936=CARTESIAN_POINT('Ctrl Pts',(-19.5504158778324,-16.5242225928466,
19.5920289419213));
#156937=CARTESIAN_POINT('Ctrl Pts',(-19.4700654949528,-16.500101228203,
19.5962135763556));
#156938=CARTESIAN_POINT('Ctrl Pts',(-19.3898294809444,-16.4760141973502,
19.6003922544784));
#156939=CARTESIAN_POINT('Ctrl Pts',(-19.3082906610536,-16.4558339863015,
19.6045709326011));
#156940=CARTESIAN_POINT('Ctrl Pts',(-19.2258642779044,-16.4396963694407,
19.6087496107238));
#156941=CARTESIAN_POINT('Ctrl Pts',(-19.1419604620519,-16.4232694975866,
19.6130031885992));
#156942=CARTESIAN_POINT('Ctrl Pts',(-19.0571373968203,-16.4110317555328,
19.6172567664746));
#156943=CARTESIAN_POINT('Ctrl Pts',(-18.9718493062316,-16.4030732243697,
19.6215103443501));
#156944=CARTESIAN_POINT('Ctrl Pts',(-18.8882146908572,-16.3952689847839,
19.6256814583605));
#156945=CARTESIAN_POINT('Ctrl Pts',(-18.8041333991978,-16.391579559832,
19.6298525723709));
#156946=CARTESIAN_POINT('Ctrl Pts',(-18.7200422944405,-16.3920380505844,
19.6340236863813));
#156947=CARTESIAN_POINT('Ctrl Pts',(-18.6359794073137,-16.3924963874856,
19.6381934007318));
#156948=CARTESIAN_POINT('Ctrl Pts',(-18.551907173272,-16.397099873298,19.6423631150822));
#156949=CARTESIAN_POINT('Ctrl Pts',(-18.4682635936936,-16.4058295103502,
19.6465328294327));
#156950=CARTESIAN_POINT('Ctrl Pts',(-18.3846229905612,-16.4145588367595,
19.6507023954044));
#156951=CARTESIAN_POINT('Ctrl Pts',(-18.3014114690234,-16.4274139738751,
19.6548719613761));
#156952=CARTESIAN_POINT('Ctrl Pts',(-18.2190616739277,-16.4443240798816,
19.6590415273478));
#156953=CARTESIAN_POINT('Ctrl Pts',(-18.1338165629824,-16.4618287240758,
19.6633576900466));
#156954=CARTESIAN_POINT('Ctrl Pts',(-18.0494954191543,-16.4836786817452,
19.6676738527455));
#156955=CARTESIAN_POINT('Ctrl Pts',(-17.9665644117748,-16.5097382167496,
19.6719900154444));
#156956=CARTESIAN_POINT('Ctrl Pts',(-17.8863348720819,-16.5349488655054,
19.6761655796575));
#156957=CARTESIAN_POINT('Ctrl Pts',(-17.8074067178225,-16.5640988419262,
19.6803411438706));
#156958=CARTESIAN_POINT('Ctrl Pts',(-17.7301828112974,-16.5970157003357,
19.6845167080837));
#156959=CARTESIAN_POINT('Ctrl Pts',(-17.6490585105613,-16.6315951102757,
19.6889031700254));
#156960=CARTESIAN_POINT('Ctrl Pts',(-17.5698156696774,-16.6703316765449,
19.6932896319672));
#156961=CARTESIAN_POINT('Ctrl Pts',(-17.4928913452169,-16.7129713474315,
19.6976760939089));
#156962=CARTESIAN_POINT('Ctrl Pts',(-17.4159670207564,-16.7556110183182,
19.7020625558507));
#156963=CARTESIAN_POINT('Ctrl Pts',(-17.3413616647363,-16.8021534221795,
19.7064490177924));
#156964=CARTESIAN_POINT('Ctrl Pts',(-17.2694745299275,-16.8522940330825,
19.7108354797342));
#156965=CARTESIAN_POINT('Ctrl Pts',(-17.2008950125392,-16.900127611461,
19.7150201150491));
#156966=CARTESIAN_POINT('Ctrl Pts',(-17.1345338099061,-16.9514136024644,
19.719204750364));
#156967=CARTESIAN_POINT('Ctrl Pts',(-17.0707594087139,-17.0059191343887,
19.7233893856789));
#156968=CARTESIAN_POINT('Ctrl Pts',(-17.0070757824026,-17.0603470845079,
19.727568064689));
#156969=CARTESIAN_POINT('Ctrl Pts',(-16.9459719906649,-17.1179851767066,
19.731746743699));
#156970=CARTESIAN_POINT('Ctrl Pts',(-16.8877869612783,-17.1785577495577,
19.7359254227091));
#156971=CARTESIAN_POINT('Ctrl Pts',(-16.8285590234002,-17.2402160252302,
19.7401790003636));
#156972=CARTESIAN_POINT('Ctrl Pts',(-16.7723559084922,-17.3049147399376,
19.744432578018));
#156973=CARTESIAN_POINT('Ctrl Pts',(-16.7194992231336,-17.3723207224235,
19.7486861556724));
#156974=CARTESIAN_POINT('Ctrl Pts',(-16.6676672533913,-17.4384199267333,
19.7528572705803));
#156975=CARTESIAN_POINT('Ctrl Pts',(-16.6190534156957,-17.5071219869974,
19.7570283854882));
#156976=CARTESIAN_POINT('Ctrl Pts',(-16.5739220086077,-17.5780774872276,
19.7611995003961));
#156977=CARTESIAN_POINT('Ctrl Pts',(-16.5288057458024,-17.6490091776496,
19.7653692156459));
#156978=CARTESIAN_POINT('Ctrl Pts',(-16.4871698395077,-17.722192418441,
19.7695389308956));
#156979=CARTESIAN_POINT('Ctrl Pts',(-16.4492353975645,-17.7972486365204,
19.7737086461453));
#156980=CARTESIAN_POINT('Ctrl Pts',(-16.4113023055078,-17.8723021837454,
19.7778782130169));
#156981=CARTESIAN_POINT('Ctrl Pts',(-16.3770706226668,-17.9492281647853,
19.7820477798885));
#156982=CARTESIAN_POINT('Ctrl Pts',(-16.3467149647707,-18.0276244483055,
19.7862173467601));
#156983=CARTESIAN_POINT('Ctrl Pts',(-16.3152920543962,-18.1087770096893,
19.790533508398));
#156984=CARTESIAN_POINT('Ctrl Pts',(-16.288022988789,-18.1915046955782,
19.794849670036));
#156985=CARTESIAN_POINT('Ctrl Pts',(-16.2650459638136,-18.2753420604184,
19.799165831674));
#156986=CARTESIAN_POINT('Ctrl Pts',(-16.2428174024766,-18.3564484703507,
19.8033413967792));
#156987=CARTESIAN_POINT('Ctrl Pts',(-16.2246056091634,-18.4385929047702,
19.8075169618844));
#156988=CARTESIAN_POINT('Ctrl Pts',(-16.2104836461321,-18.5213432785139,
19.8116925269897));
#156989=CARTESIAN_POINT('Ctrl Pts',(-16.1956484266957,-18.6082731161156,
19.816078986894));
#156990=CARTESIAN_POINT('Ctrl Pts',(-16.1853271121021,-18.6958711329071,
19.8204654467983));
#156991=CARTESIAN_POINT('Ctrl Pts',(-16.1795426555428,-18.7836323209494,
19.8248519067027));
#156992=CARTESIAN_POINT('Ctrl Pts',(-16.1737581989836,-18.8713935089917,
19.829238366607));
#156993=CARTESIAN_POINT('Ctrl Pts',(-16.1725105326347,-18.9593172870491,
19.8336248265113));
#156994=CARTESIAN_POINT('Ctrl Pts',(-16.1757597065439,-19.0469031134252,
19.8380112864157));
#156995=CARTESIAN_POINT('Ctrl Pts',(-16.1788596427641,-19.1304660383847,
19.8421962719891));
#156996=CARTESIAN_POINT('Ctrl Pts',(-16.1860639312553,-19.2140324391989,
19.8463812575626));
#156997=CARTESIAN_POINT('Ctrl Pts',(-16.1973762176809,-19.2971663178426,
19.850566243136));
#156998=CARTESIAN_POINT('Ctrl Pts',(-16.208669157137,-19.3801580158035,
19.8547440712892));
#156999=CARTESIAN_POINT('Ctrl Pts',(-16.2240560627403,-19.4627182105596,
19.8589218994425));
#157000=CARTESIAN_POINT('Ctrl Pts',(-16.2434886326561,-19.5444129717781,
19.8630997275957));
#157001=CARTESIAN_POINT('Ctrl Pts',(-16.2629022923872,-19.6260282343488,
19.8672734902288));
#157002=CARTESIAN_POINT('Ctrl Pts',(-16.2863536946398,-19.7067792904715,
19.871447252862));
#157003=CARTESIAN_POINT('Ctrl Pts',(-16.3137431277316,-19.7862401765904,
19.8756210154952));
#157004=CARTESIAN_POINT('Ctrl Pts',(-16.3411141246999,-19.865647576728,
19.8797919687236));
#157005=CARTESIAN_POINT('Ctrl Pts',(-16.3724177386845,-19.9437660979487,
19.8839629219521));
#157006=CARTESIAN_POINT('Ctrl Pts',(-16.4075041942595,-20.0201840973689,
19.8881338751805));
#157007=CARTESIAN_POINT('Ctrl Pts',(-16.4425775582141,-20.0965735833524,
19.8923032721236));
#157008=CARTESIAN_POINT('Ctrl Pts',(-16.4814307670068,-20.1712633909202,
19.8964726690667));
#157009=CARTESIAN_POINT('Ctrl Pts',(-16.5238661301382,-20.2438623290775,
19.9006420660098));
#157010=CARTESIAN_POINT('Ctrl Pts',(-16.5663181358782,-20.3164897396133,
19.9048130981373));
#157011=CARTESIAN_POINT('Ctrl Pts',(-16.612354878163,-20.3870242402789,
19.9089841302648));
#157012=CARTESIAN_POINT('Ctrl Pts',(-16.661733317948,-20.4551003953353,
19.9131551623922));
#157013=CARTESIAN_POINT('Ctrl Pts',(-16.7111193613354,-20.5231870331858,
19.9173268368015));
#157014=CARTESIAN_POINT('Ctrl Pts',(-16.7638478466874,-20.5888142060546,
19.9214985112107));
#157015=CARTESIAN_POINT('Ctrl Pts',(-16.8196343574744,-20.6516482538212,
19.9256701856199));
#157016=CARTESIAN_POINT('Ctrl Pts',(-16.8754895074255,-20.7145596119709,
19.9298469928155));
#157017=CARTESIAN_POINT('Ctrl Pts',(-16.9344098847018,-20.774670642438,
19.9340238000111));
#157018=CARTESIAN_POINT('Ctrl Pts',(-16.9960732526694,-20.8316836491582,
19.9382006072068));
#157019=CARTESIAN_POINT('Ctrl Pts',(-17.0532712047221,-20.8845680006338,
19.9420749466336));
#157020=CARTESIAN_POINT('Ctrl Pts',(-17.1128286535666,-20.9347869850788,
19.9459492860605));
#157021=CARTESIAN_POINT('Ctrl Pts',(-17.1744641402401,-20.9821349467765,
19.9498236254873));
#157022=CARTESIAN_POINT('Ctrl Pts',(-17.1767158074852,-20.9792339848999,
19.149828714141));
#157023=CARTESIAN_POINT('Ctrl Pts',(-17.4546312945708,-21.1947985643844,
19.1672632270968));
#157024=CARTESIAN_POINT('Ctrl Pts',(-18.5512406568725,-21.7455419441639,
19.2270896756131));
#157025=CARTESIAN_POINT('Ctrl Pts',(-20.6359183918341,-21.202775782827,
19.3215765970986));
#157026=CARTESIAN_POINT('Ctrl Pts',(-21.2889868109407,-19.6455867711505,
19.3986290056282));
#157027=CARTESIAN_POINT('Ctrl Pts',(-21.2953147898194,-18.9498155448408,
19.4332894785973));
#157028=CARTESIAN_POINT('',(-21.2939989850553,-18.9542795868244,19.3667098901939));
#157029=CARTESIAN_POINT('Ctrl Pts',(-17.1744641402401,-20.9821349467764,
19.0833436902736));
#157030=CARTESIAN_POINT('Ctrl Pts',(-17.2408452334434,-21.0331284511368,
19.0875248451816));
#157031=CARTESIAN_POINT('Ctrl Pts',(-17.3098396878856,-21.080946991935,
19.0917060000897));
#157032=CARTESIAN_POINT('Ctrl Pts',(-17.3811105272675,-21.1253131561212,
19.0958871549977));
#157033=CARTESIAN_POINT('Ctrl Pts',(-17.4522930341336,-21.1696243332337,
19.1000631278153));
#157034=CARTESIAN_POINT('Ctrl Pts',(-17.5257459330175,-21.2104913926985,
19.1042391006329));
#157035=CARTESIAN_POINT('Ctrl Pts',(-17.6011009621195,-21.2476784988254,
19.1084150734506));
#157036=CARTESIAN_POINT('Ctrl Pts',(-17.6763877017987,-21.2848319046666,
19.1125872618523));
#157037=CARTESIAN_POINT('Ctrl Pts',(-17.7535727350803,-21.3183117817329,
19.116759450254));
#157038=CARTESIAN_POINT('Ctrl Pts',(-17.8322618834364,-21.3479274548985,
19.1209316386556));
#157039=CARTESIAN_POINT('Ctrl Pts',(-17.9109136780137,-21.3775290694889,
19.1251018465174));
#157040=CARTESIAN_POINT('Ctrl Pts',(-17.9910677400756,-21.4032699606739,
19.1292720543791));
#157041=CARTESIAN_POINT('Ctrl Pts',(-18.0723096286257,-21.4250074509452,
19.1334422622408));
#157042=CARTESIAN_POINT('Ctrl Pts',(-18.15353732237,-21.4467411431826,19.1376117414724));
#157043=CARTESIAN_POINT('Ctrl Pts',(-18.2358520206424,-21.4644727055195,
19.141781220704));
#157044=CARTESIAN_POINT('Ctrl Pts',(-18.3188251471571,-21.4781096258015,
19.1459506999355));
#157045=CARTESIAN_POINT('Ctrl Pts',(-18.4018086660397,-21.4917482541051,
19.1501207013936));
#157046=CARTESIAN_POINT('Ctrl Pts',(-18.4854503227753,-21.50129114871,19.1542907028516));
#157047=CARTESIAN_POINT('Ctrl Pts',(-18.5693137603081,-21.5066973289328,
19.1584607043096));
#157048=CARTESIAN_POINT('Ctrl Pts',(-18.6532674185104,-21.5121093251489,
19.1626351918743));
#157049=CARTESIAN_POINT('Ctrl Pts',(-18.7374428738953,-21.5133756933231,
19.1668096794389));
#157050=CARTESIAN_POINT('Ctrl Pts',(-18.821401611171,-21.5105075646487,
19.1709841670036));
#157051=CARTESIAN_POINT('Ctrl Pts',(-18.9054094707161,-21.5076377579002,
19.1751610969621));
#157052=CARTESIAN_POINT('Ctrl Pts',(-18.9891999013505,-21.5006286769763,
19.1793380269206));
#157053=CARTESIAN_POINT('Ctrl Pts',(-19.0723397717153,-21.4895433393098,
19.1835149568791));
#157054=CARTESIAN_POINT('Ctrl Pts',(-19.1556200492609,-21.4784392806494,
19.1876989408654));
#157055=CARTESIAN_POINT('Ctrl Pts',(-19.2382471205611,-21.4632453034702,
19.1918829248517));
#157056=CARTESIAN_POINT('Ctrl Pts',(-19.3197986310449,-21.4440754330208,
19.1960669088381));
#157057=CARTESIAN_POINT('Ctrl Pts',(-19.3683964228494,-21.4326518141634,
19.1985602088576));
#157058=CARTESIAN_POINT('Ctrl Pts',(-19.4166125476408,-21.4198172577591,
19.2010535088771));
#157059=CARTESIAN_POINT('Ctrl Pts',(-19.4643607861739,-21.4056041086572,
19.2035468088966));
#157060=CARTESIAN_POINT('Ctrl Pts',(-19.5444991251693,-21.3817494451991,
19.2077314433108));
#157061=CARTESIAN_POINT('Ctrl Pts',(-19.6236166763929,-21.3539201055357,
19.211916077725));
#157062=CARTESIAN_POINT('Ctrl Pts',(-19.7012904348026,-21.3222213429846,
19.2161007121391));
#157063=CARTESIAN_POINT('Ctrl Pts',(-19.778853634233,-21.2905676996977,
19.2202793902443));
#157064=CARTESIAN_POINT('Ctrl Pts',(-19.8549767005595,-21.2550557457739,
19.2244580683494));
#157065=CARTESIAN_POINT('Ctrl Pts',(-19.9292512406756,-21.215840646261,
19.2286367464546));
#157066=CARTESIAN_POINT('Ctrl Pts',(-20.0048570980657,-21.1759226445248,
19.2328903243347));
#157067=CARTESIAN_POINT('Ctrl Pts',(-20.0785470456786,-21.1321675712325,
19.2371439022148));
#157068=CARTESIAN_POINT('Ctrl Pts',(-20.1499110579027,-21.0847906311002,
19.241397480095));
#157069=CARTESIAN_POINT('Ctrl Pts',(-20.2198915399371,-21.038332185107,
19.2455685940941));
#157070=CARTESIAN_POINT('Ctrl Pts',(-20.2876350664325,-20.9883913190918,
19.2497397080933));
#157071=CARTESIAN_POINT('Ctrl Pts',(-20.3527809100999,-20.935216671243,
19.2539108220924));
#157072=CARTESIAN_POINT('Ctrl Pts',(-20.4179048934498,-20.8820598666613,
19.2580805364339));
#157073=CARTESIAN_POINT('Ctrl Pts',(-20.480432569049,-20.8256717259784,
19.2622502507755));
#157074=CARTESIAN_POINT('Ctrl Pts',(-20.5400350473299,-20.766342141884,
19.266419965117));
#157075=CARTESIAN_POINT('Ctrl Pts',(-20.5996354046978,-20.7070146689917,
19.2705895310821));
#157076=CARTESIAN_POINT('Ctrl Pts',(-20.6563104462706,-20.6447462859464,
19.2747590970472));
#157077=CARTESIAN_POINT('Ctrl Pts',(-20.709768014027,-20.5798638624738,
19.2789286630123));
#157078=CARTESIAN_POINT('Ctrl Pts',(-20.7651050833169,-20.5127002537633,
19.2832448257261));
#157079=CARTESIAN_POINT('Ctrl Pts',(-20.8169938810792,-20.4427357722886,
19.2875609884399));
#157080=CARTESIAN_POINT('Ctrl Pts',(-20.8651569232063,-20.3703688408415,
19.2918771511538));
#157081=CARTESIAN_POINT('Ctrl Pts',(-20.9117510598039,-20.3003592538204,
19.2960527153661));
#157082=CARTESIAN_POINT('Ctrl Pts',(-20.9548582452865,-20.2281017614681,
19.3002282795785));
#157083=CARTESIAN_POINT('Ctrl Pts',(-20.9942733140312,-20.1539835880237,
19.3044038437908));
#157084=CARTESIAN_POINT('Ctrl Pts',(-21.0356791435395,-20.0761218830757,
19.3087903057554));
#157085=CARTESIAN_POINT('Ctrl Pts',(-21.0730098296578,-19.9962071202703,
19.3131767677199));
#157086=CARTESIAN_POINT('Ctrl Pts',(-21.1060848561741,-19.9147115014943,
19.3175632296844));
#157087=CARTESIAN_POINT('Ctrl Pts',(-21.1391598826905,-19.8332158827183,
19.321949691649));
#157088=CARTESIAN_POINT('Ctrl Pts',(-21.1679791313071,-19.7501399810715,
19.3263361536135));
#157089=CARTESIAN_POINT('Ctrl Pts',(-21.1924232051046,-19.6659715292665,
19.330722615578));
#157090=CARTESIAN_POINT('Ctrl Pts',(-21.2214742546437,-19.56593984538,19.3359357942359));
#157091=CARTESIAN_POINT('Ctrl Pts',(-21.2444357643464,-19.4640653478474,
19.3411489728938));
#157092=CARTESIAN_POINT('Ctrl Pts',(-21.261115150052,-19.3610098023001,
19.3463621515516));
#157093=CARTESIAN_POINT('Ctrl Pts',(-21.277528721009,-19.2595966244285,
19.3514922492257));
#157094=CARTESIAN_POINT('Ctrl Pts',(-21.2878587862943,-19.1570396545895,
19.3566223468997));
#157095=CARTESIAN_POINT('Ctrl Pts',(-21.2919675308073,-19.0539907414198,
19.3617524445737));
#157096=CARTESIAN_POINT('Ctrl Pts',(-21.2932910194155,-19.020797131491,
19.3634049264471));
#157097=CARTESIAN_POINT('Ctrl Pts',(-21.2939693565913,-18.9875526505269,
19.3650574083205));
#157098=CARTESIAN_POINT('Ctrl Pts',(-21.2939989850553,-18.9542795868244,
19.3667098901939));
#157099=CARTESIAN_POINT('Ctrl Pts',(-21.2939989850559,-18.954279586128,
19.3667098902285));
#157100=CARTESIAN_POINT('Ctrl Pts',(-21.294073180434,-18.8709574030256,
19.3708480242597));
#157101=CARTESIAN_POINT('Ctrl Pts',(-21.2900751830219,-18.7875513930813,
19.3749861582908));
#157102=CARTESIAN_POINT('Ctrl Pts',(-21.2820071809341,-18.7044936245096,
19.379124292322));
#157103=CARTESIAN_POINT('Ctrl Pts',(-21.2739428344709,-18.6214734895453,
19.3832605513581));
#157104=CARTESIAN_POINT('Ctrl Pts',(-21.2618121886764,-18.5388017480938,
19.3873968103941));
#157105=CARTESIAN_POINT('Ctrl Pts',(-21.2456694473266,-18.4569074961523,
19.3915330694301));
#157106=CARTESIAN_POINT('Ctrl Pts',(-21.2295289836496,-18.3750247991451,
19.3956687448574));
#157107=CARTESIAN_POINT('Ctrl Pts',(-21.2093776397613,-18.2939198329769,
19.3998044202847));
#157108=CARTESIAN_POINT('Ctrl Pts',(-21.1853208566141,-18.214012155975,
19.403940095712));
#157109=CARTESIAN_POINT('Ctrl Pts',(-21.1612599617833,-18.1340908214908,
19.4080764779915));
#157110=CARTESIAN_POINT('Ctrl Pts',(-21.1332924395156,-18.0553676300856,
19.4122128602709));
#157111=CARTESIAN_POINT('Ctrl Pts',(-21.1015733410968,-17.9782461940883,
19.4163492425504));
#157112=CARTESIAN_POINT('Ctrl Pts',(-21.0698191717564,-17.901039487072,
19.4204901983123));
#157113=CARTESIAN_POINT('Ctrl Pts',(-21.0343053289603,-17.825438502363,
19.4246311540741));
#157114=CARTESIAN_POINT('Ctrl Pts',(-20.9952344193641,-17.7518254707406,
19.428772109836));
#157115=CARTESIAN_POINT('Ctrl Pts',(-20.9561382227283,-17.6781647961105,
19.4329157456612));
#157116=CARTESIAN_POINT('Ctrl Pts',(-20.9134806196083,-17.6064950352479,
19.4370593814864));
#157117=CARTESIAN_POINT('Ctrl Pts',(-20.8675081508587,-17.5371703387972,
19.4412030173116));
#157118=CARTESIAN_POINT('Ctrl Pts',(-20.8214607545949,-17.4677326545666,
19.4453534065774));
#157119=CARTESIAN_POINT('Ctrl Pts',(-20.7720879921757,-17.4006480348511,
19.4495037958431));
#157120=CARTESIAN_POINT('Ctrl Pts',(-20.7196769297237,-17.3362379102222,
19.4536541851088));
#157121=CARTESIAN_POINT('Ctrl Pts',(-20.7018115389434,-17.3142823918094,
19.4550689308257));
#157122=CARTESIAN_POINT('Ctrl Pts',(-20.6835934338648,-17.2926373126042,
19.4564836765426));
#157123=CARTESIAN_POINT('Ctrl Pts',(-20.6650349200515,-17.2713143846806,
19.4578984222595));
#157124=CARTESIAN_POINT('Ctrl Pts',(-20.6101412425931,-17.2082439287333,
19.4620830566462));
#157125=CARTESIAN_POINT('Ctrl Pts',(-20.552052199416,-17.1477482923966,
19.4662676910329));
#157126=CARTESIAN_POINT('Ctrl Pts',(-20.4910387353975,-17.0901689436706,
19.4704523254196));
#157127=CARTESIAN_POINT('Ctrl Pts',(-20.4301121164985,-17.0326715520257,
19.4746310034968));
#157128=CARTESIAN_POINT('Ctrl Pts',(-20.3662696766049,-16.9780825158894,
19.4788096815741));
#157129=CARTESIAN_POINT('Ctrl Pts',(-20.2998217436397,-16.9267093376147,
19.4829883596513));
#157130=CARTESIAN_POINT('Ctrl Pts',(-20.2321827790971,-16.8744153319368,
19.4872419375384));
#157131=CARTESIAN_POINT('Ctrl Pts',(-20.1618443123322,-16.8254539702931,
19.4914955154255));
#157132=CARTESIAN_POINT('Ctrl Pts',(-20.0891719990944,-16.7801093828486,
19.4957490933125));
#157133=CARTESIAN_POINT('Ctrl Pts',(-20.0179085806131,-16.7356438888117,
19.4999202072829));
#157134=CARTESIAN_POINT('Ctrl Pts',(-19.9444014087305,-16.6946564386937,
19.5040913212534));
#157135=CARTESIAN_POINT('Ctrl Pts',(-19.8690261614839,-16.6573724457448,
19.5082624352238));
#157136=CARTESIAN_POINT('Ctrl Pts',(-19.7936762071349,-16.6201009638025,
19.5124321495363));
#157137=CARTESIAN_POINT('Ctrl Pts',(-19.7164598343598,-16.5865306747405,
19.5166018638488));
#157138=CARTESIAN_POINT('Ctrl Pts',(-19.6377770918967,-16.5568409305095,
19.5207715781614));
#157139=CARTESIAN_POINT('Ctrl Pts',(-19.5590971493085,-16.527152242769,
19.5249411440973));
#157140=CARTESIAN_POINT('Ctrl Pts',(-19.4789513714909,-16.5013439869193,
19.5291107100332));
#157141=CARTESIAN_POINT('Ctrl Pts',(-19.3977582580731,-16.4795467699389,
19.5332802759692));
#157142=CARTESIAN_POINT('Ctrl Pts',(-19.3137104946165,-16.4569831896096,
19.5375964387168));
#157143=CARTESIAN_POINT('Ctrl Pts',(-19.2285408859958,-16.4387180891116,
19.5419126014644));
#157144=CARTESIAN_POINT('Ctrl Pts',(-19.1427269885612,-16.4248390932072,
19.5462287642121));
#157145=CARTESIAN_POINT('Ctrl Pts',(-19.0597084701507,-16.4114122041898,
19.5504043283951));
#157146=CARTESIAN_POINT('Ctrl Pts',(-18.9760874671123,-16.4020900585603,
19.554579892578));
#157147=CARTESIAN_POINT('Ctrl Pts',(-18.8923014001436,-16.3968990887418,
19.558755456761));
#157148=CARTESIAN_POINT('Ctrl Pts',(-18.8042834975808,-16.391445935345,
19.5631419187909));
#157149=CARTESIAN_POINT('Ctrl Pts',(-18.7160840019592,-16.3905522627805,
19.5675283808209));
#157150=CARTESIAN_POINT('Ctrl Pts',(-18.6282074804617,-16.3941868827434,
19.5719148428509));
#157151=CARTESIAN_POINT('Ctrl Pts',(-18.5403309589642,-16.3978215027064,
19.5763013048809));
#157152=CARTESIAN_POINT('Ctrl Pts',(-18.4527779822414,-16.4059842855988,
19.5806877669109));
#157153=CARTESIAN_POINT('Ctrl Pts',(-18.3660419494154,-16.4185819782338,
19.5850742289409));
#157154=CARTESIAN_POINT('Ctrl Pts',(-18.2832967675646,-16.4306000327149,
19.5892588634754));
#157155=CARTESIAN_POINT('Ctrl Pts',(-18.2009870107893,-16.4466985853957,
19.59344349801));
#157156=CARTESIAN_POINT('Ctrl Pts',(-18.1195464569871,-16.4668346446405,
19.5976281325445));
#157157=CARTESIAN_POINT('Ctrl Pts',(-18.0382218237187,-16.4869420427009,
19.6018068107705));
#157158=CARTESIAN_POINT('Ctrl Pts',(-17.9577643787149,-16.5110754227199,
19.6059854889965));
#157159=CARTESIAN_POINT('Ctrl Pts',(-17.878600657432,-16.5391402931927,
19.6101641672224));
#157160=CARTESIAN_POINT('Ctrl Pts',(-17.7980179867494,-16.5677082050898,
19.6144177450724));
#157161=CARTESIAN_POINT('Ctrl Pts',(-17.7187763529939,-16.6003498680467,
19.6186713229224));
#157162=CARTESIAN_POINT('Ctrl Pts',(-17.6413125871542,-16.6369116177112,
19.6229249007724));
#157163=CARTESIAN_POINT('Ctrl Pts',(-17.5653506043487,-16.6727645480362,
19.6270960148927));
#157164=CARTESIAN_POINT('Ctrl Pts',(-17.4910986050711,-16.712386719325,
19.631267129013));
#157165=CARTESIAN_POINT('Ctrl Pts',(-17.4189494736076,-16.7555842576973,
19.6354382431332));
#157166=CARTESIAN_POINT('Ctrl Pts',(-17.3468245524847,-16.7987673007169,
19.6396079575957));
#157167=CARTESIAN_POINT('Ctrl Pts',(-17.2768014921365,-16.845523091981,
19.6437776720582));
#157168=CARTESIAN_POINT('Ctrl Pts',(-17.2092476379827,-16.8956123335999,
19.6479473865207));
#157169=CARTESIAN_POINT('Ctrl Pts',(-17.141696187691,-16.9456997928241,
19.6521169526065));
#157170=CARTESIAN_POINT('Ctrl Pts',(-17.0766141379211,-16.9991201918754,
19.6562865186922));
#157171=CARTESIAN_POINT('Ctrl Pts',(-17.0143378344021,-17.0555923338556,
19.660456084778));
#157172=CARTESIAN_POINT('Ctrl Pts',(-16.9498719775865,-17.1140499624118,
19.6647722473484));
#157173=CARTESIAN_POINT('Ctrl Pts',(-16.8884132283207,-17.1757775704978,
19.6690884099187));
#157174=CARTESIAN_POINT('Ctrl Pts',(-16.8302937573018,-17.2404210384818,
19.6734045724891));
#157175=CARTESIAN_POINT('Ctrl Pts',(-16.7740675178662,-17.3029587568246,
19.6775801368201));
#157176=CARTESIAN_POINT('Ctrl Pts',(-16.7209666047403,-17.3682248893115,
19.6817557011511));
#157177=CARTESIAN_POINT('Ctrl Pts',(-16.6712500109568,-17.4358659417115,
19.6859312654821));
#157178=CARTESIAN_POINT('Ctrl Pts',(-16.6190223557939,-17.5069233752716,
19.6903177271722));
#157179=CARTESIAN_POINT('Ctrl Pts',(-16.5705302089911,-17.5806014599345,
19.6947041888622));
#157180=CARTESIAN_POINT('Ctrl Pts',(-16.5260204587108,-17.6564590530407,
19.6990906505522));
#157181=CARTESIAN_POINT('Ctrl Pts',(-16.4815107084305,-17.7323166461468,
19.7034771122423));
#157182=CARTESIAN_POINT('Ctrl Pts',(-16.4409835545834,-17.810353197721,
19.7078635739323));
#157183=CARTESIAN_POINT('Ctrl Pts',(-16.4046276535563,-17.8901033611394,
19.7122500356223));
#157184=CARTESIAN_POINT('Ctrl Pts',(-16.3699445411289,-17.9661841019766,
19.7164346697438));
#157185=CARTESIAN_POINT('Ctrl Pts',(-16.3389281684892,-18.0441074153348,
19.7206193038652));
#157186=CARTESIAN_POINT('Ctrl Pts',(-16.3117771822314,-18.1234852921757,
19.7248039379867));
#157187=CARTESIAN_POINT('Ctrl Pts',(-16.2846648420429,-18.2027501844311,
19.7289826157992));
#157188=CARTESIAN_POINT('Ctrl Pts',(-16.2614071073441,-18.2834650961696,
19.7331612936118));
#157189=CARTESIAN_POINT('Ctrl Pts',(-16.2421554012958,-18.3652202321922,
19.7373399714244));
#157190=CARTESIAN_POINT('Ctrl Pts',(-16.2225586206672,-18.4484407770037,
19.7415935493777));
#157191=CARTESIAN_POINT('Ctrl Pts',(-16.207113098083,-18.5327387664133,
19.745847127331));
#157192=CARTESIAN_POINT('Ctrl Pts',(-16.1959260745188,-18.617663719001,
19.7501007052843));
#157193=CARTESIAN_POINT('Ctrl Pts',(-16.1849559341181,-18.7009422289687,
19.7542718189934));
#157194=CARTESIAN_POINT('Ctrl Pts',(-16.1780807097886,-18.7848231320472,
19.7584429327025));
#157195=CARTESIAN_POINT('Ctrl Pts',(-16.1753500450965,-18.8688711345423,
19.7626140464116));
#157196=CARTESIAN_POINT('Ctrl Pts',(-16.1726202967043,-18.9528909339471,
19.7667837604647));
#157197=CARTESIAN_POINT('Ctrl Pts',(-16.1740323608325,-19.0370772620015,
19.7709534745177));
#157198=CARTESIAN_POINT('Ctrl Pts',(-16.1795838629395,-19.1209917120006,
19.7751231885707));
#157199=CARTESIAN_POINT('Ctrl Pts',(-16.1851351675026,-19.2049031760005,
19.7792927542493));
#157200=CARTESIAN_POINT('Ctrl Pts',(-16.1948255859618,-19.2885423222071,
19.7834623199278));
#157201=CARTESIAN_POINT('Ctrl Pts',(-16.2086007337952,-19.3714741306115,
19.7876318856064));
#157202=CARTESIAN_POINT('Ctrl Pts',(-16.2228602007955,-19.457321730907,
19.7919480486645));
#157203=CARTESIAN_POINT('Ctrl Pts',(-16.2414968944622,-19.5424108074415,
19.7962642117226));
#157204=CARTESIAN_POINT('Ctrl Pts',(-16.26439285385,-19.6262703787688,19.8005803747807));
#157205=CARTESIAN_POINT('Ctrl Pts',(-16.2865429767612,-19.7073982223639,
19.8047559387142));
#157206=CARTESIAN_POINT('Ctrl Pts',(-16.3126789433259,-19.7873750001408,
19.8089315026477));
#157207=CARTESIAN_POINT('Ctrl Pts',(-16.34264370885,-19.8657916002993,19.8131070665811));
#157208=CARTESIAN_POINT('Ctrl Pts',(-16.3741219297554,-19.9481688530246,
19.8174935292016));
#157209=CARTESIAN_POINT('Ctrl Pts',(-16.4098256651424,-20.0288236423437,
19.821879991822));
#157210=CARTESIAN_POINT('Ctrl Pts',(-16.4495176194985,-20.1073095919183,
19.8262664544425));
#157211=CARTESIAN_POINT('Ctrl Pts',(-16.4892095738547,-20.1857955414929,
19.8306529170629));
#157212=CARTESIAN_POINT('Ctrl Pts',(-16.532889392945,-20.2621121855376,
19.8350393796833));
#157213=CARTESIAN_POINT('Ctrl Pts',(-16.5802679097415,-20.3358490103298,
19.8394258423038));
#157214=CARTESIAN_POINT('Ctrl Pts',(-16.6254567089947,-20.4061779019541,
19.8436095735007));
#157215=CARTESIAN_POINT('Ctrl Pts',(-16.6741780301271,-20.4744218961067,
19.8477933046977));
#157216=CARTESIAN_POINT('Ctrl Pts',(-16.726213289138,-20.5402041819885,
19.8519770358946));
#157217=CARTESIAN_POINT('Ctrl Pts',(-16.7781836605675,-20.6059044378486,
19.8561555500099));
#157218=CARTESIAN_POINT('Ctrl Pts',(-16.8334594864442,-20.669148719787,
19.8603340641251));
#157219=CARTESIAN_POINT('Ctrl Pts',(-16.8917781973807,-20.729587924676,
19.8645125782403));
#157220=CARTESIAN_POINT('Ctrl Pts',(-16.9500311212365,-20.7899589504372,
19.8686863787355));
#157221=CARTESIAN_POINT('Ctrl Pts',(-17.0113197908613,-20.8475308583887,
19.8728601792307));
#157222=CARTESIAN_POINT('Ctrl Pts',(-17.0753415571519,-20.9019877358508,
19.8770339797259));
#157223=CARTESIAN_POINT('Ctrl Pts',(-17.1076991188394,-20.9295110591499,
19.8791434811473));
#157224=CARTESIAN_POINT('Ctrl Pts',(-17.1407542103651,-20.9562392078978,
19.8812529825688));
#157225=CARTESIAN_POINT('Ctrl Pts',(-17.1744641402401,-20.9821349467765,
19.8833624839903));
#157226=CARTESIAN_POINT('Origin',(-18.734,-18.952,-1.76670989022851));
#157227=CARTESIAN_POINT('',(-17.1744641402402,-20.9821349467765,20.7499611383185));
#157228=CARTESIAN_POINT('',(-17.1763037530772,-20.9797762769265,20.6832232033274));
#157229=CARTESIAN_POINT('',(-17.1744641402401,-20.9821349467765,-1.76670989022851));
#157230=CARTESIAN_POINT('',(-21.2939995273704,-18.9535555909848,20.2332901098006));
#157231=CARTESIAN_POINT('Ctrl Pts',(-21.2939995273704,-18.9535555909848,
20.2332901098006));
#157232=CARTESIAN_POINT('Ctrl Pts',(-21.294049723898,-18.870948345104,20.2374173417263));
#157233=CARTESIAN_POINT('Ctrl Pts',(-21.2900972917066,-18.7881812203374,
20.241544573652));
#157234=CARTESIAN_POINT('Ctrl Pts',(-21.2821221997477,-18.7056805830778,
20.2456718055777));
#157235=CARTESIAN_POINT('Ctrl Pts',(-21.2739869562085,-18.6215232116386,
20.2498819183928));
#157236=CARTESIAN_POINT('Ctrl Pts',(-21.2616656480612,-18.537643639815,
20.254092031208));
#157237=CARTESIAN_POINT('Ctrl Pts',(-21.2451929664636,-18.4544963465625,
20.2583021440231));
#157238=CARTESIAN_POINT('Ctrl Pts',(-21.229080068103,-18.3731650904946,
20.2624203028958));
#157239=CARTESIAN_POINT('Ctrl Pts',(-21.2089953895162,-18.2925349412607,
20.2665384617684));
#157240=CARTESIAN_POINT('Ctrl Pts',(-21.1850236976428,-18.2130258234598,
20.270656620641));
#157241=CARTESIAN_POINT('Ctrl Pts',(-21.1610629749352,-18.1335530881012,
20.2747728950923));
#157242=CARTESIAN_POINT('Ctrl Pts',(-21.1332189046361,-18.055200818656,
20.2788891695437));
#157243=CARTESIAN_POINT('Ctrl Pts',(-21.1016267121137,-17.9783759698499,
20.283005443995));
#157244=CARTESIAN_POINT('Ctrl Pts',(-21.0700389130291,-17.9015618048605,
20.2871211460075));
#157245=CARTESIAN_POINT('Ctrl Pts',(-21.0347042074052,-17.8262750760015,
20.2912368480201));
#157246=CARTESIAN_POINT('Ctrl Pts',(-20.9958062193322,-17.752903412485,
20.2953525500326));
#157247=CARTESIAN_POINT('Ctrl Pts',(-20.9553538853537,-17.6765998506772,
20.299632713625));
#157248=CARTESIAN_POINT('Ctrl Pts',(-20.9110477424172,-17.6023681210458,
20.3039128772174));
#157249=CARTESIAN_POINT('Ctrl Pts',(-20.8631463424907,-17.5306148121433,
20.3081930408098));
#157250=CARTESIAN_POINT('Ctrl Pts',(-20.817026382064,-17.4615299884816,
20.3123140263301));
#157251=CARTESIAN_POINT('Ctrl Pts',(-20.767574190865,-17.394742855338,20.3164350118505));
#157252=CARTESIAN_POINT('Ctrl Pts',(-20.7150628530422,-17.3305839607626,
20.3205559973708));
#157253=CARTESIAN_POINT('Ctrl Pts',(-20.6625158707606,-17.2663815154195,
20.3246797801975));
#157254=CARTESIAN_POINT('Ctrl Pts',(-20.6069059305284,-17.204811205117,
20.3288035630242));
#157255=CARTESIAN_POINT('Ctrl Pts',(-20.5485433980296,-17.1461671570527,
20.3329273458509));
#157256=CARTESIAN_POINT('Ctrl Pts',(-20.4900913111083,-17.0874331225942,
20.3370574564186));
#157257=CARTESIAN_POINT('Ctrl Pts',(-20.4288785613994,-17.031634616857,
20.3411875669862));
#157258=CARTESIAN_POINT('Ctrl Pts',(-20.3652483132487,-16.9790253573542,
20.3453176775539));
#157259=CARTESIAN_POINT('Ctrl Pts',(-20.3580748979454,-16.9730944034733,
20.3457832894164));
#157260=CARTESIAN_POINT('Ctrl Pts',(-20.3508707868094,-16.9672039368768,
20.3462489012788));
#157261=CARTESIAN_POINT('Ctrl Pts',(-20.3436364930174,-16.961354285578,
20.3467145131413));
#157262=CARTESIAN_POINT('Ctrl Pts',(-20.2786189220457,-16.9087810656599,
20.3508991582751));
#157263=CARTESIAN_POINT('Ctrl Pts',(-20.2109019646558,-16.8592987216113,
20.3550838034089));
#157264=CARTESIAN_POINT('Ctrl Pts',(-20.1408117772448,-16.813196450488,
20.3592684485427));
#157265=CARTESIAN_POINT('Ctrl Pts',(-20.0708213560678,-16.7671598012461,
20.3634471372609));
#157266=CARTESIAN_POINT('Ctrl Pts',(-19.9984647957972,-16.724493919034,
20.3676258259791));
#157267=CARTESIAN_POINT('Ctrl Pts',(-19.9241011351325,-16.6854477089297,
20.3718045146973));
#157268=CARTESIAN_POINT('Ctrl Pts',(-19.8484047994816,-16.6457017496864,
20.3760580899108));
#157269=CARTESIAN_POINT('Ctrl Pts',(-19.7706290892635,-16.6097067834814,
20.3803116651244));
#157270=CARTESIAN_POINT('Ctrl Pts',(-19.6911834645766,-16.5776790833712,
20.384565240338));
#157271=CARTESIAN_POINT('Ctrl Pts',(-19.6132778070226,-16.5462722054359,
20.3887363646167));
#157272=CARTESIAN_POINT('Ctrl Pts',(-19.5337668426417,-16.5186803435126,
20.3929074888954));
#157273=CARTESIAN_POINT('Ctrl Pts',(-19.4530597028474,-16.4950602075466,
20.3970786131741));
#157274=CARTESIAN_POINT('Ctrl Pts',(-19.3723796478629,-16.47144799835,20.4012483376496));
#157275=CARTESIAN_POINT('Ctrl Pts',(-19.2905046558528,-16.4518049970839,
20.4054180621252));
#157276=CARTESIAN_POINT('Ctrl Pts',(-19.2078598549769,-16.4362383185522,
20.4095877866007));
#157277=CARTESIAN_POINT('Ctrl Pts',(-19.1252179980804,-16.4206721945378,
20.4137573625421));
#157278=CARTESIAN_POINT('Ctrl Pts',(-19.0418068390792,-16.4091821888638,
20.4179269384834));
#157279=CARTESIAN_POINT('Ctrl Pts',(-18.9580612068526,-16.4018242069254,
20.4220965144247));
#157280=CARTESIAN_POINT('Ctrl Pts',(-18.8713716361879,-16.3942075673677,
20.4264126648745));
#157281=CARTESIAN_POINT('Ctrl Pts',(-18.7843241636749,-16.3910189213341,
20.4307288153244));
#157282=CARTESIAN_POINT('Ctrl Pts',(-18.6974043010312,-16.3922615846894,
20.4350449657742));
#157283=CARTESIAN_POINT('Ctrl Pts',(-18.613315412911,-16.3934637745764,
20.4392205394722));
#157284=CARTESIAN_POINT('Ctrl Pts',(-18.5293464168603,-16.3988129730352,
20.4433961131702));
#157285=CARTESIAN_POINT('Ctrl Pts',(-18.4459326746173,-16.4082592081647,
20.4475716868682));
#157286=CARTESIAN_POINT('Ctrl Pts',(-18.3583065652386,-16.4181824751278,
20.4519581256939));
#157287=CARTESIAN_POINT('Ctrl Pts',(-18.2712938422191,-16.432627374356,
20.4563445645197));
#157288=CARTESIAN_POINT('Ctrl Pts',(-18.1853859701635,-16.4514755257613,
20.4607310033455));
#157289=CARTESIAN_POINT('Ctrl Pts',(-18.099478098108,-16.4703236771666,
20.4651174421713));
#157290=CARTESIAN_POINT('Ctrl Pts',(-18.0146756164477,-16.4935748539843,
20.469503880997));
#157291=CARTESIAN_POINT('Ctrl Pts',(-17.9314482086937,-16.5210514974045,
20.4738903198228));
#157292=CARTESIAN_POINT('Ctrl Pts',(-17.8520491312121,-16.5472642583054,
20.4780749893396));
#157293=CARTESIAN_POINT('Ctrl Pts',(-17.7737878973577,-16.5774198558355,
20.4822596588565));
#157294=CARTESIAN_POINT('Ctrl Pts',(-17.6970842217394,-16.6114005748967,
20.4864443283734));
#157295=CARTESIAN_POINT('Ctrl Pts',(-17.6204897187464,-16.6453329290746,
20.4906230418346));
#157296=CARTESIAN_POINT('Ctrl Pts',(-17.545448787571,-16.6830794059288,
20.4948017552959));
#157297=CARTESIAN_POINT('Ctrl Pts',(-17.4723650615669,-16.7244728324609,
20.4989804687571));
#157298=CARTESIAN_POINT('Ctrl Pts',(-17.3979721462502,-16.7666077623972,
20.5032340378299));
#157299=CARTESIAN_POINT('Ctrl Pts',(-17.3256077070819,-16.8125214402581,
20.5074876069027));
#157300=CARTESIAN_POINT('Ctrl Pts',(-17.2556752218673,-16.8619866387128,
20.5117411759755));
#157301=CARTESIAN_POINT('Ctrl Pts',(-17.1870977846746,-16.9104933738853,
20.5159123256928));
#157302=CARTESIAN_POINT('Ctrl Pts',(-17.1208592892441,-16.9624149470776,
20.5200834754102));
#157303=CARTESIAN_POINT('Ctrl Pts',(-17.0573129609309,-17.0174921625856,
20.5242546251275));
#157304=CARTESIAN_POINT('Ctrl Pts',(-16.9937879551552,-17.0725508973092,
20.5284243752439));
#157305=CARTESIAN_POINT('Ctrl Pts',(-16.9329536697872,-17.130762870401,
20.5325941253604));
#157306=CARTESIAN_POINT('Ctrl Pts',(-16.8751302869621,-17.1918285907473,
20.5367638754768));
#157307=CARTESIAN_POINT('Ctrl Pts',(-16.8173089615946,-17.252892138268,
20.5409334772262));
#157308=CARTESIAN_POINT('Ctrl Pts',(-16.76249864144,-17.3168088965337,20.5451030789756));
#157309=CARTESIAN_POINT('Ctrl Pts',(-16.7109817002441,-17.383243499184,
20.549272680725));
#157310=CARTESIAN_POINT('Ctrl Pts',(-16.6576544669953,-17.4520125966707,
20.5535888012066));
#157311=CARTESIAN_POINT('Ctrl Pts',(-16.6078567053803,-17.5234793715945,
20.5579049216882));
#157312=CARTESIAN_POINT('Ctrl Pts',(-16.561853993216,-17.5972373915654,
20.5622210421698));
#157313=CARTESIAN_POINT('Ctrl Pts',(-16.5173490008796,-17.6685940564038,
20.566396641823));
#157314=CARTESIAN_POINT('Ctrl Pts',(-16.4763959254939,-17.7420946281061,
20.5705722414761));
#157315=CARTESIAN_POINT('Ctrl Pts',(-16.439188403649,-17.8173459834589,
20.5747478411293));
#157316=CARTESIAN_POINT('Ctrl Pts',(-16.4001026730812,-17.8963959726636,
20.5791342220251));
#157317=CARTESIAN_POINT('Ctrl Pts',(-16.3651508237527,-17.9773776173555,
20.5835206029209));
#157318=CARTESIAN_POINT('Ctrl Pts',(-16.3344993304474,-18.0598136199109,
20.5879069838167));
#157319=CARTESIAN_POINT('Ctrl Pts',(-16.303847837142,-18.1422496224663,
20.5922933647126));
#157320=CARTESIAN_POINT('Ctrl Pts',(-16.2774968011627,-18.2261394066298,
20.5966797456084));
#157321=CARTESIAN_POINT('Ctrl Pts',(-16.2555511525118,-18.3109919576289,
20.6010661265042));
#157322=CARTESIAN_POINT('Ctrl Pts',(-16.2346154345157,-18.3919396255348,
20.6052506477694));
#157323=CARTESIAN_POINT('Ctrl Pts',(-16.2176106157921,-18.4740647181833,
20.6094351690347));
#157324=CARTESIAN_POINT('Ctrl Pts',(-16.2046649096203,-18.5569506352697,
20.6136196902999));
#157325=CARTESIAN_POINT('Ctrl Pts',(-16.1917376309692,-18.6397185686836,
20.6177982551227));
#157326=CARTESIAN_POINT('Ctrl Pts',(-16.1828580584881,-18.7232447247141,
20.6219768199456));
#157327=CARTESIAN_POINT('Ctrl Pts',(-16.1781041153419,-18.8070992519427,
20.6261553847685));
#157328=CARTESIAN_POINT('Ctrl Pts',(-16.1732647978195,-18.8924596928357,
20.6304089909525));
#157329=CARTESIAN_POINT('Ctrl Pts',(-16.1727008779273,-18.9781599489879,
20.6346625971366));
#157330=CARTESIAN_POINT('Ctrl Pts',(-16.1764397017154,-19.0637377314902,
20.6389162033206));
#157331=CARTESIAN_POINT('Ctrl Pts',(-16.1801059175876,-19.1476535944187,
20.6430872045204));
#157332=CARTESIAN_POINT('Ctrl Pts',(-16.1879092316882,-19.2314512172152,
20.6472582057202));
#157333=CARTESIAN_POINT('Ctrl Pts',(-16.1998229036826,-19.3146933201762,
20.65142920692));
#157334=CARTESIAN_POINT('Ctrl Pts',(-16.2117325790265,-19.3979074981112,
20.6555988088842));
#157335=CARTESIAN_POINT('Ctrl Pts',(-16.2277498086426,-19.480566071281,
20.6597684108483));
#157336=CARTESIAN_POINT('Ctrl Pts',(-16.2477960843791,-19.5622377323235,
20.6639380128125));
#157337=CARTESIAN_POINT('Ctrl Pts',(-16.267841649488,-19.6439064981583,
20.668107466967));
#157338=CARTESIAN_POINT('Ctrl Pts',(-16.2919158662461,-19.7245879748305,
20.6722769211214));
#157339=CARTESIAN_POINT('Ctrl Pts',(-16.3198895960845,-19.8038632271128,
20.6764463752759));
#157340=CARTESIAN_POINT('Ctrl Pts',(-16.3488485215243,-19.8859304427941,
20.6807626717684));
#157341=CARTESIAN_POINT('Ctrl Pts',(-16.3819865838885,-19.9664900366012,
20.6850789682608));
#157342=CARTESIAN_POINT('Ctrl Pts',(-16.419105751819,-20.0450986322096,
20.6893952647533));
#157343=CARTESIAN_POINT('Ctrl Pts',(-16.4550137144481,-20.1211422148331,
20.6935707196945));
#157344=CARTESIAN_POINT('Ctrl Pts',(-16.494646706784,-20.1953597704703,
20.6977461746357));
#157345=CARTESIAN_POINT('Ctrl Pts',(-16.5377789910434,-20.2673757181192,
20.7019216295769));
#157346=CARTESIAN_POINT('Ctrl Pts',(-16.5830936067771,-20.3430354020531,
20.7063083468451));
#157347=CARTESIAN_POINT('Ctrl Pts',(-16.6322706296986,-20.4162643312086,
20.7106950641132));
#157348=CARTESIAN_POINT('Ctrl Pts',(-16.6849987382266,-20.4866640770054,
20.7150817813813));
#157349=CARTESIAN_POINT('Ctrl Pts',(-16.7377268467545,-20.5570638228022,
20.7194684986494));
#157350=CARTESIAN_POINT('Ctrl Pts',(-16.7940056108791,-20.6246339879283,
20.7238552159176));
#157351=CARTESIAN_POINT('Ctrl Pts',(-16.8534788452301,-20.689020491089,
20.7282419331857));
#157352=CARTESIAN_POINT('Ctrl Pts',(-16.9102019255006,-20.7504296413894,
20.7324258004066));
#157353=CARTESIAN_POINT('Ctrl Pts',(-16.9700416973334,-20.8091716375129,
20.7366096676276));
#157354=CARTESIAN_POINT('Ctrl Pts',(-17.0327174072577,-20.8649133643822,
20.7407935348485));
#157355=CARTESIAN_POINT('Ctrl Pts',(-17.0784953144305,-20.9056267380537,
20.7438494026718));
#157356=CARTESIAN_POINT('Ctrl Pts',(-17.1257851938307,-20.944740111196,
20.7469052704952));
#157357=CARTESIAN_POINT('Ctrl Pts',(-17.1744641402402,-20.9821349467765,
20.7499611383185));
#157358=CARTESIAN_POINT('Ctrl Pts',(-17.1744641402401,-20.9821349467765,
19.9498236254873));
#157359=CARTESIAN_POINT('Ctrl Pts',(-17.2410374779127,-21.0332761320307,
19.9540083528391));
#157360=CARTESIAN_POINT('Ctrl Pts',(-17.3100350925294,-21.0810671210711,
19.9581930801908));
#157361=CARTESIAN_POINT('Ctrl Pts',(-17.3810772332865,-21.125292430233,
19.9623778075426));
#157362=CARTESIAN_POINT('Ctrl Pts',(-17.396974538177,-21.1351888553144,
19.9633142360608));
#157363=CARTESIAN_POINT('Ctrl Pts',(-17.4129741317038,-21.1449069178138,
19.9642506645789));
#157364=CARTESIAN_POINT('Ctrl Pts',(-17.4290716122084,-21.1544445288669,
19.965187093097));
#157365=CARTESIAN_POINT('Ctrl Pts',(-17.5010067187011,-21.1970654263791,
19.9693717283979));
#157366=CARTESIAN_POINT('Ctrl Pts',(-17.5751659818923,-21.2362376725991,
19.9735563636989));
#157367=CARTESIAN_POINT('Ctrl Pts',(-17.6511848628853,-21.2717222632969,
19.9777409989998));
#157368=CARTESIAN_POINT('Ctrl Pts',(-17.7270955401341,-21.307156345943,
19.9819196779751));
#157369=CARTESIAN_POINT('Ctrl Pts',(-17.8048601642346,-21.3389130061849,
19.9860983569504));
#157370=CARTESIAN_POINT('Ctrl Pts',(-17.8840874846203,-21.3667978623895,
19.9902770359257));
#157371=CARTESIAN_POINT('Ctrl Pts',(-17.9647348763174,-21.3951825270456,
19.9945306135862));
#157372=CARTESIAN_POINT('Ctrl Pts',(-18.0468975021298,-21.4195549745919,
19.9987841912467));
#157373=CARTESIAN_POINT('Ctrl Pts',(-18.1301389338575,-21.4397604010027,
20.0030377689073));
#157374=CARTESIAN_POINT('Ctrl Pts',(-18.211766588852,-21.4595741108567,
20.0072088837303));
#157375=CARTESIAN_POINT('Ctrl Pts',(-18.294431126417,-21.4753808138487,
20.0113799985532));
#157376=CARTESIAN_POINT('Ctrl Pts',(-18.3777050585878,-21.4870845971533,
20.0155511133762));
#157377=CARTESIAN_POINT('Ctrl Pts',(-18.4609510470138,-21.4987844530881,
20.0197208285227));
#157378=CARTESIAN_POINT('Ctrl Pts',(-18.544805568747,-21.5063840596946,
20.0238905436692));
#157379=CARTESIAN_POINT('Ctrl Pts',(-18.6288324774106,-21.5098388909766,
20.0280602588157));
#157380=CARTESIAN_POINT('Ctrl Pts',(-18.7128563956357,-21.5132935993045,
20.0322298255659));
#157381=CARTESIAN_POINT('Ctrl Pts',(-18.7970522289137,-21.5126038075458,
20.0363993923161));
#157382=CARTESIAN_POINT('Ctrl Pts',(-18.8809816357491,-21.5077770635861,
20.0405689590663));
#157383=CARTESIAN_POINT('Ctrl Pts',(-18.9678618598034,-21.5027806194017,
20.0448851207924));
#157384=CARTESIAN_POINT('Ctrl Pts',(-19.0544560474151,-21.4933509339533,
20.0492012825184));
#157385=CARTESIAN_POINT('Ctrl Pts',(-19.1402833032842,-21.4795549207629,
20.0535174442444));
#157386=CARTESIAN_POINT('Ctrl Pts',(-19.2233147796994,-21.466208305725,
20.057693009185));
#157387=CARTESIAN_POINT('Ctrl Pts',(-19.3056280710303,-21.4487756011034,
20.0618685741256));
#157388=CARTESIAN_POINT('Ctrl Pts',(-19.3867996160279,-21.4273691969712,
20.0660441390663));
#157389=CARTESIAN_POINT('Ctrl Pts',(-19.472070890686,-21.4048816199976,
20.070430599185));
#157390=CARTESIAN_POINT('Ctrl Pts',(-19.5560814940463,-21.3780085540522,
20.0748170593037));
#157391=CARTESIAN_POINT('Ctrl Pts',(-19.6383622324208,-21.3469381938937,
20.0792035194224));
#157392=CARTESIAN_POINT('Ctrl Pts',(-19.7206429707954,-21.3158678337352,
20.0835899795411));
#157393=CARTESIAN_POINT('Ctrl Pts',(-19.8011933431874,-21.2806004817501,
20.0879764396598));
#157394=CARTESIAN_POINT('Ctrl Pts',(-19.8795742651246,-21.2413797420009,
20.0923628997785));
#157395=CARTESIAN_POINT('Ctrl Pts',(-19.9543489008138,-21.2039635384947,
20.0965475399847));
#157396=CARTESIAN_POINT('Ctrl Pts',(-20.0274276531195,-21.162810473499,
20.100732180191));
#157397=CARTESIAN_POINT('Ctrl Pts',(-20.0984122388012,-21.11809769923,20.1049168203972));
#157398=CARTESIAN_POINT('Ctrl Pts',(-20.1692957874189,-21.0734485676151,
20.1090955043278));
#157399=CARTESIAN_POINT('Ctrl Pts',(-20.2380907042344,-21.0252500340151,
20.1132741882584));
#157400=CARTESIAN_POINT('Ctrl Pts',(-20.3044217681325,-20.9737258642496,
20.117452872189));
#157401=CARTESIAN_POINT('Ctrl Pts',(-20.371941651073,-20.9212782521244,
20.1217064486169));
#157402=CARTESIAN_POINT('Ctrl Pts',(-20.4369080609029,-20.865384834865,
20.1259600250449));
#157403=CARTESIAN_POINT('Ctrl Pts',(-20.4989546028882,-20.8063287868509,
20.1302136014728));
#157404=CARTESIAN_POINT('Ctrl Pts',(-20.5597983582893,-20.7484175540028,
20.1343847213367));
#157405=CARTESIAN_POINT('Ctrl Pts',(-20.6178340917841,-20.6874655447192,
20.1385558412007));
#157406=CARTESIAN_POINT('Ctrl Pts',(-20.6727497644134,-20.6237802938745,
20.1427269610646));
#157407=CARTESIAN_POINT('Ctrl Pts',(-20.7276470096087,-20.5601164131724,
20.1468966812728));
#157408=CARTESIAN_POINT('Ctrl Pts',(-20.7794259730566,-20.4937214605129,
20.151066401481));
#157409=CARTESIAN_POINT('Ctrl Pts',(-20.827813137392,-20.4249380658006,
20.1552361216892));
#157410=CARTESIAN_POINT('Ctrl Pts',(-20.8761985798384,-20.3561571187907,
20.1594056935151));
#157411=CARTESIAN_POINT('Ctrl Pts',(-20.921192199164,-20.2849882754667,
20.1635752653411));
#157412=CARTESIAN_POINT('Ctrl Pts',(-20.9625630757428,-20.2118041980546,
20.167744837167));
#157413=CARTESIAN_POINT('Ctrl Pts',(-21.0053883717902,-20.1360472878725,
20.1720609929414));
#157414=CARTESIAN_POINT('Ctrl Pts',(-21.044331197893,-20.0581312678785,
20.1763771487158));
#157415=CARTESIAN_POINT('Ctrl Pts',(-21.0791875194638,-19.9784967114177,
20.1806933044902));
#157416=CARTESIAN_POINT('Ctrl Pts',(-21.1129085013345,-19.9014560108021,
20.184868874489));
#157417=CARTESIAN_POINT('Ctrl Pts',(-21.1428049796707,-19.8228074643854,
20.1890444444878));
#157418=CARTESIAN_POINT('Ctrl Pts',(-21.1687421906793,-19.7429680555664,
20.1932200144866));
#157419=CARTESIAN_POINT('Ctrl Pts',(-21.1959893077345,-19.6590965199184,
20.1976064631488));
#157420=CARTESIAN_POINT('Ctrl Pts',(-21.2188665683597,-19.5739112349382,
20.201992911811));
#157421=CARTESIAN_POINT('Ctrl Pts',(-21.2372782494394,-19.4879085797817,
20.2063793604732));
#157422=CARTESIAN_POINT('Ctrl Pts',(-21.2556899305191,-19.4019059246253,
20.2107658091355));
#157423=CARTESIAN_POINT('Ctrl Pts',(-21.2696360151318,-19.3150864842148,
20.2151522577977));
#157424=CARTESIAN_POINT('Ctrl Pts',(-21.2790836671994,-19.2279513126528,
20.2195387064599));
#157425=CARTESIAN_POINT('Ctrl Pts',(-21.2889563823072,-19.136895808223,
20.2241225075637));
#157426=CARTESIAN_POINT('Ctrl Pts',(-21.2939437779019,-19.0453011468624,
20.2287063086676));
#157427=CARTESIAN_POINT('Ctrl Pts',(-21.2939995273701,-18.9535555915677,
20.2332901097715));
#157428=CARTESIAN_POINT('',(-21.2937660523048,-18.9509923322678,20.1667099325986));
#157429=CARTESIAN_POINT('Ctrl Pts',(-17.1744641402401,-20.9821349467765,
19.8833624839903));
#157430=CARTESIAN_POINT('Ctrl Pts',(-17.2411053585891,-21.0333282775047,
19.8875327609786));
#157431=CARTESIAN_POINT('Ctrl Pts',(-17.3103076802409,-21.0812658121085,
19.8917030379669));
#157432=CARTESIAN_POINT('Ctrl Pts',(-17.3817163438391,-21.1256901603679,
19.8958733149552));
#157433=CARTESIAN_POINT('Ctrl Pts',(-17.4531114624803,-21.1701060821163,
19.9000428009159));
#157434=CARTESIAN_POINT('Ctrl Pts',(-17.5267117010556,-21.211009898609,
19.9042122868766));
#157435=CARTESIAN_POINT('Ctrl Pts',(-17.6021341277255,-21.2481880687741,
19.9083817728373));
#157436=CARTESIAN_POINT('Ctrl Pts',(-17.6775648727756,-21.2853703393396,
19.9125517186529));
#157437=CARTESIAN_POINT('Ctrl Pts',(-17.754817791772,-21.3188259454625,
19.9167216644685));
#157438=CARTESIAN_POINT('Ctrl Pts',(-17.833487460302,-21.3483883587279,
19.920891610284));
#157439=CARTESIAN_POINT('Ctrl Pts',(-17.9122410721742,-21.3779823161427,
19.9250660055805));
#157440=CARTESIAN_POINT('Ctrl Pts',(-17.9924140202009,-21.4036746249937,
19.929240400877));
#157441=CARTESIAN_POINT('Ctrl Pts',(-18.0735835869046,-21.4253479660804,
19.9334147961735));
#157442=CARTESIAN_POINT('Ctrl Pts',(-18.1547995551522,-21.4470336969892,
19.9375915778125));
#157443=CARTESIAN_POINT('Ctrl Pts',(-18.2370128265568,-21.464695789383,
19.9417683594515));
#157444=CARTESIAN_POINT('Ctrl Pts',(-18.3197906755089,-21.4782681242308,
19.9459451410904));
#157445=CARTESIAN_POINT('Ctrl Pts',(-18.4027095772105,-21.4918635862215,
19.9501290399297));
#157446=CARTESIAN_POINT('Ctrl Pts',(-18.4861945203917,-21.5013553226401,
19.9543129387691));
#157447=CARTESIAN_POINT('Ctrl Pts',(-18.5698081482532,-21.5067291511665,
19.9584968376084));
#157448=CARTESIAN_POINT('Ctrl Pts',(-18.6237986730703,-21.5101991097108,
19.9611984414006));
#157449=CARTESIAN_POINT('Ctrl Pts',(-18.6778428224662,-21.5119531844675,
19.9639000451929));
#157450=CARTESIAN_POINT('Ctrl Pts',(-18.7318236815561,-21.5119990749291,
19.9666016489852));
#157451=CARTESIAN_POINT('Ctrl Pts',(-18.8154370559313,-21.5120701567239,
19.9707862843005));
#157452=CARTESIAN_POINT('Ctrl Pts',(-18.8992095169516,-21.508040657495,
19.9749709196158));
#157453=CARTESIAN_POINT('Ctrl Pts',(-18.9827056283928,-21.4998904039236,
19.9791555549311));
#157454=CARTESIAN_POINT('Ctrl Pts',(-19.0660828935662,-21.4917517512183,
19.9833342339415));
#157455=CARTESIAN_POINT('Ctrl Pts',(-19.149184136535,-21.4795040389676,
19.987512912952));
#157456=CARTESIAN_POINT('Ctrl Pts',(-19.2315736418543,-21.4631790997322,
19.9916915919625));
#157457=CARTESIAN_POINT('Ctrl Pts',(-19.3154398966918,-21.446561552281,
19.9959451696169));
#157458=CARTESIAN_POINT('Ctrl Pts',(-19.3985681653821,-21.4257191734759,
20.0001987472712));
#157459=CARTESIAN_POINT('Ctrl Pts',(-19.4805039905309,-21.400740858507,
20.0044523249255));
#157460=CARTESIAN_POINT('Ctrl Pts',(-19.560851352111,-21.3762467901208,
20.0086234398338));
#157461=CARTESIAN_POINT('Ctrl Pts',(-19.6400516322992,-21.3477758589918,
20.0127945547421));
#157462=CARTESIAN_POINT('Ctrl Pts',(-19.7176880451009,-21.315463101029,
20.0169656696504));
#157463=CARTESIAN_POINT('Ctrl Pts',(-19.7952984062491,-21.2831611859264,
20.0211353849005));
#157464=CARTESIAN_POINT('Ctrl Pts',(-19.8713455178527,-21.247020180909,
20.0253051001507));
#157465=CARTESIAN_POINT('Ctrl Pts',(-19.9454312973038,-21.207223760941,
20.0294748154008));
#157466=CARTESIAN_POINT('Ctrl Pts',(-20.0195144404333,-21.1674287571174,
20.0336443822728));
#157467=CARTESIAN_POINT('Ctrl Pts',(-20.0916359853166,-21.1239788154148,
20.0378139491447));
#157468=CARTESIAN_POINT('Ctrl Pts',(-20.1614224658083,-21.0771035513842,
20.0419835160167));
#157469=CARTESIAN_POINT('Ctrl Pts',(-20.2336625183512,-21.0285802340787,
20.0462996776542));
#157470=CARTESIAN_POINT('Ctrl Pts',(-20.3033998142158,-20.9763865417844,
20.0506158392917));
#157471=CARTESIAN_POINT('Ctrl Pts',(-20.3702544760718,-20.9208248498876,
20.0549320009292));
#157472=CARTESIAN_POINT('Ctrl Pts',(-20.4349313850112,-20.8670730487781,
20.0591075660348));
#157473=CARTESIAN_POINT('Ctrl Pts',(-20.4969102618753,-20.8101696539257,
20.0632831311405));
#157474=CARTESIAN_POINT('Ctrl Pts',(-20.555883728143,-20.7504270018902,
20.0674586962461));
#157475=CARTESIAN_POINT('Ctrl Pts',(-20.6178357606473,-20.6876669344389,
20.0718451561495));
#157476=CARTESIAN_POINT('Ctrl Pts',(-20.6764704135552,-20.6217736908107,
20.0762316160529));
#157477=CARTESIAN_POINT('Ctrl Pts',(-20.7314796147868,-20.5531480845041,
20.0806180759564));
#157478=CARTESIAN_POINT('Ctrl Pts',(-20.7864888160183,-20.4845224781975,
20.0850045358598));
#157479=CARTESIAN_POINT('Ctrl Pts',(-20.8378722882511,-20.4131650245059,
20.0893909957632));
#157480=CARTESIAN_POINT('Ctrl Pts',(-20.8853760799667,-20.3395089053938,
20.0937774556666));
#157481=CARTESIAN_POINT('Ctrl Pts',(-20.93172083375,-20.2676499109516,20.0980568909888));
#157482=CARTESIAN_POINT('Ctrl Pts',(-20.9745398784111,-20.1933453659579,
20.1023363263109));
#157483=CARTESIAN_POINT('Ctrl Pts',(-21.0135728621542,-20.1169667661055,
20.1066157616331));
#157484=CARTESIAN_POINT('Ctrl Pts',(-21.0525424988234,-20.0407121219527,
20.1108882518109));
#157485=CARTESIAN_POINT('Ctrl Pts',(-21.0877380945303,-19.9623904961899,
20.1151607419887));
#157486=CARTESIAN_POINT('Ctrl Pts',(-21.1189429603293,-19.8824015670536,
20.1194332321666));
#157487=CARTESIAN_POINT('Ctrl Pts',(-21.1500944336146,-19.8025495015083,
20.1236984119784));
#157488=CARTESIAN_POINT('Ctrl Pts',(-21.1772686126578,-19.7210362114978,
20.1279635917902));
#157489=CARTESIAN_POINT('Ctrl Pts',(-21.2002957121622,-19.6382838043918,
20.132228771602));
#157490=CARTESIAN_POINT('Ctrl Pts',(-21.2232995983466,-19.5556148189128,
20.1364896517415));
#157491=CARTESIAN_POINT('Ctrl Pts',(-21.242164599727,-19.4717096138904,
20.1407505318809));
#157492=CARTESIAN_POINT('Ctrl Pts',(-21.2567699769455,-19.3870076360505,
20.1450114120204));
#157493=CARTESIAN_POINT('Ctrl Pts',(-21.2713627640963,-19.3023786726647,
20.1492686192133));
#157494=CARTESIAN_POINT('Ctrl Pts',(-21.2817031592285,-19.2169547278876,
20.1535258264062));
#157495=CARTESIAN_POINT('Ctrl Pts',(-21.2877212407691,-19.1311865632376,
20.1577830335991));
#157496=CARTESIAN_POINT('Ctrl Pts',(-21.2919276409326,-19.0712380199392,
20.1607586524755));
#157497=CARTESIAN_POINT('Ctrl Pts',(-21.2940234518483,-19.0111215769093,
20.163734271352));
#157498=CARTESIAN_POINT('Ctrl Pts',(-21.293999801981,-18.9509930952203,
20.1667098902285));
#157499=CARTESIAN_POINT('Ctrl Pts',(-21.2901593135592,-18.9509805599729,
20.1667105863666));
#157500=CARTESIAN_POINT('Ctrl Pts',(-21.2914430747328,-18.5861666271369,
20.1847914783605));
#157501=CARTESIAN_POINT('Ctrl Pts',(-21.0477247281039,-17.3676608534593,
20.2452643059147));
#157502=CARTESIAN_POINT('Ctrl Pts',(-19.1741877080397,-15.9570837783716,
20.3481290690295));
#157503=CARTESIAN_POINT('Ctrl Pts',(-16.4540143744161,-16.9607794391954,
20.4753048757109));
#157504=CARTESIAN_POINT('Ctrl Pts',(-15.9020682314716,-19.4468144996336,
20.5870029204769));
#157505=CARTESIAN_POINT('Ctrl Pts',(-16.7482596976323,-20.6463211842255,
20.6563090296824));
#157506=CARTESIAN_POINT('Ctrl Pts',(-17.1763037530771,-20.9797762769264,
20.6832232033273));
#157507=CARTESIAN_POINT('Origin',(-18.734,-18.952,-1.76670989022851));
#157508=CARTESIAN_POINT('',(-17.176996236551,-20.9788220778502,21.5499224931685));
#157509=CARTESIAN_POINT('',(-17.1722616776481,-20.9849677398537,21.4832513321535));
#157510=CARTESIAN_POINT('',(-17.1744641402401,-20.9821349467765,-1.76670989022851));
#157511=CARTESIAN_POINT('',(-21.293894749231,-18.9533416782113,21.033290082045));
#157512=CARTESIAN_POINT('Ctrl Pts',(-21.2904839170199,-18.9533393312605,
21.0332901097715));
#157513=CARTESIAN_POINT('Ctrl Pts',(-21.2880301337774,-18.4391275099938,
21.0587831909243));
#157514=CARTESIAN_POINT('Ctrl Pts',(-20.8878308621683,-17.0663417376224,
21.1266682076376));
#157515=CARTESIAN_POINT('Ctrl Pts',(-18.6471935206347,-15.9262791991665,
21.2369451599114));
#157516=CARTESIAN_POINT('Ctrl Pts',(-16.142559944897,-17.3869838835127,
21.3641209665928));
#157517=CARTESIAN_POINT('Ctrl Pts',(-16.0386998683022,-19.7637662988606,
21.4684467443452));
#157518=CARTESIAN_POINT('Ctrl Pts',(-16.8637710355043,-20.7393377348947,
21.5303805865371));
#157519=CARTESIAN_POINT('Ctrl Pts',(-17.176996236551,-20.9788220778502,
21.5499224931685));
#157520=CARTESIAN_POINT('Ctrl Pts',(-17.1744641402402,-20.9821349467765,
20.7499611383185));
#157521=CARTESIAN_POINT('Ctrl Pts',(-17.2444594813357,-21.0359048917883,
20.754355163383));
#157522=CARTESIAN_POINT('Ctrl Pts',(-17.317328415444,-21.0861194210246,
20.7587491884476));
#157523=CARTESIAN_POINT('Ctrl Pts',(-17.3926684715169,-21.1324654848672,
20.7631432135121));
#157524=CARTESIAN_POINT('Ctrl Pts',(-17.4641970336474,-21.1764668764227,
20.7673149424862));
#157525=CARTESIAN_POINT('Ctrl Pts',(-17.5379523384401,-21.2169813963177,
20.7714866714603));
#157526=CARTESIAN_POINT('Ctrl Pts',(-17.6135584513473,-21.2537842505441,
20.7756584004345));
#157527=CARTESIAN_POINT('Ctrl Pts',(-17.6891338306681,-21.2905721445555,
20.7798284336172));
#157528=CARTESIAN_POINT('Ctrl Pts',(-17.7665581109874,-21.3236511679191,
20.7839984668));
#157529=CARTESIAN_POINT('Ctrl Pts',(-17.8454309959992,-21.3528425864952,
20.7881684999828));
#157530=CARTESIAN_POINT('Ctrl Pts',(-17.9242954765414,-21.382030894517,
20.7923380888187));
#157531=CARTESIAN_POINT('Ctrl Pts',(-18.0046078235079,-21.4073322617217,
20.7965076776546));
#157532=CARTESIAN_POINT('Ctrl Pts',(-18.0859492963724,-21.4286167013746,
20.8006772664906));
#157533=CARTESIAN_POINT('Ctrl Pts',(-18.1673064987639,-21.4499052569374,
20.8048476616269));
#157534=CARTESIAN_POINT('Ctrl Pts',(-18.2496927769265,-21.4671752273624,
20.8090180567632));
#157535=CARTESIAN_POINT('Ctrl Pts',(-18.3326771588405,-21.4803472817561,
20.8131884518995));
#157536=CARTESIAN_POINT('Ctrl Pts',(-18.4157540106533,-21.4935340138339,
20.8173634941273));
#157537=CARTESIAN_POINT('Ctrl Pts',(-18.4994298412268,-21.502613645428,
20.8215385363551));
#157538=CARTESIAN_POINT('Ctrl Pts',(-18.583267037094,-21.5075585639726,
20.825713578583));
#157539=CARTESIAN_POINT('Ctrl Pts',(-18.6671584017786,-21.5125066775237,
20.8298913183855));
#157540=CARTESIAN_POINT('Ctrl Pts',(-18.7512108797419,-21.5133147567839,
20.834069058188));
#157541=CARTESIAN_POINT('Ctrl Pts',(-18.8349877178507,-21.5100073261903,
20.8382467979905));
#157542=CARTESIAN_POINT('Ctrl Pts',(-18.9189003229372,-21.5066945356444,
20.8424313081501));
#157543=CARTESIAN_POINT('Ctrl Pts',(-19.0025359395193,-21.4992529664416,
20.8466158183097));
#157544=CARTESIAN_POINT('Ctrl Pts',(-19.0854642865313,-21.487758832242,
20.8508003284693));
#157545=CARTESIAN_POINT('Ctrl Pts',(-19.1159668049541,-21.4835310856051,
20.8523394656019));
#157546=CARTESIAN_POINT('Ctrl Pts',(-19.1463737547783,-21.478755563272,
20.8538786027345));
#157547=CARTESIAN_POINT('Ctrl Pts',(-19.1766642018011,-21.4734377653323,
20.8554177398671));
#157548=CARTESIAN_POINT('Ctrl Pts',(-19.2590223589629,-21.4589789480642,
20.8596025740416));
#157549=CARTESIAN_POINT('Ctrl Pts',(-19.3408245084339,-21.4404538839632,
20.8637874082161));
#157550=CARTESIAN_POINT('Ctrl Pts',(-19.4216382989709,-21.4179184029056,
20.8679722423906));
#157551=CARTESIAN_POINT('Ctrl Pts',(-19.5023371028523,-21.3954149866674,
20.8721511221348));
#157552=CARTESIAN_POINT('Ctrl Pts',(-19.5820499018622,-21.3689126104334,
20.8763300018789));
#157553=CARTESIAN_POINT('Ctrl Pts',(-19.6603531104248,-21.338518366744,
20.8805088816231));
#157554=CARTESIAN_POINT('Ctrl Pts',(-19.7400550610479,-21.3075811860814,
20.8847624093283));
#157555=CARTESIAN_POINT('Ctrl Pts',(-19.8182960912148,-21.2726118104529,
20.8890159370335));
#157556=CARTESIAN_POINT('Ctrl Pts',(-19.8946441530214,-21.2337767528961,
20.8932694647388));
#157557=CARTESIAN_POINT('Ctrl Pts',(-19.9695166174632,-21.195692269843,
20.8974407834904));
#157558=CARTESIAN_POINT('Ctrl Pts',(-20.0425682056166,-21.1538904198174,
20.901612102242));
#157559=CARTESIAN_POINT('Ctrl Pts',(-20.1134119104384,-21.1085766347016,
20.9057834209936));
#157560=CARTESIAN_POINT('Ctrl Pts',(-20.1842318561761,-21.0632780466174,
20.9099533407964));
#157561=CARTESIAN_POINT('Ctrl Pts',(-20.2528450019901,-21.0144701102459,
20.9141232605992));
#157562=CARTESIAN_POINT('Ctrl Pts',(-20.3188912127324,-20.9624029058384,
20.9182931804021));
#157563=CARTESIAN_POINT('Ctrl Pts',(-20.3849350802549,-20.9103375486967,
20.9224629522624));
#157564=CARTESIAN_POINT('Ctrl Pts',(-20.448411833077,-20.8550134388734,
20.9266327241228));
#157565=CARTESIAN_POINT('Ctrl Pts',(-20.5089935615136,-20.7967216203496,
20.9308024959832));
#157566=CARTESIAN_POINT('Ctrl Pts',(-20.5716986579763,-20.7363866943274,
20.9351184168636));
#157567=CARTESIAN_POINT('Ctrl Pts',(-20.6313016391124,-20.6728725241964,
20.9394343377441));
#157568=CARTESIAN_POINT('Ctrl Pts',(-20.687481020985,-20.6065428071378,
20.9437502586245));
#157569=CARTESIAN_POINT('Ctrl Pts',(-20.7418360778663,-20.5423670290593,
20.9479260276902));
#157570=CARTESIAN_POINT('Ctrl Pts',(-20.79298623453,-20.4755561680757,20.9521017967558));
#157571=CARTESIAN_POINT('Ctrl Pts',(-20.8406830326348,-20.4064712441326,
20.9562775658215));
#157572=CARTESIAN_POINT('Ctrl Pts',(-20.8907811103752,-20.333908262383,
20.9606635626093));
#157573=CARTESIAN_POINT('Ctrl Pts',(-20.9370686806316,-20.2588367305564,
20.9650495593971));
#157574=CARTESIAN_POINT('Ctrl Pts',(-20.9793120741947,-20.1817047163753,
20.969435556185));
#157575=CARTESIAN_POINT('Ctrl Pts',(-21.0215554677577,-20.1045727021941,
20.9738215529728));
#157576=CARTESIAN_POINT('Ctrl Pts',(-21.0597545011784,-20.025380760798,
20.9782075497606));
#157577=CARTESIAN_POINT('Ctrl Pts',(-21.0937343889893,-19.9445994224366,
20.9825935465485));
#157578=CARTESIAN_POINT('Ctrl Pts',(-21.1297844964522,-19.8588964929525,
20.9872467595436));
#157579=CARTESIAN_POINT('Ctrl Pts',(-21.1612011352353,-19.7711341998165,
20.9918999725387));
#157580=CARTESIAN_POINT('Ctrl Pts',(-21.187770405969,-19.6818018873577,
20.9965531855338));
#157581=CARTESIAN_POINT('Ctrl Pts',(-21.2142564631891,-19.5927493588517,
21.0011918249184));
#157582=CARTESIAN_POINT('Ctrl Pts',(-21.2359253189815,-19.5021368713044,
21.005830464303));
#157583=CARTESIAN_POINT('Ctrl Pts',(-21.2526114126831,-19.410471975046,
21.0104691036876));
#157584=CARTESIAN_POINT('Ctrl Pts',(-21.269207206213,-19.3193031419175,
21.0150826401368));
#157585=CARTESIAN_POINT('Ctrl Pts',(-21.2808739033347,-19.2270935185721,
21.019696176586));
#157586=CARTESIAN_POINT('Ctrl Pts',(-21.2874964963647,-19.1343612981233,
21.0243097130352));
#157587=CARTESIAN_POINT('Ctrl Pts',(-21.2917935126354,-19.074192742048,
21.0273031690875));
#157588=CARTESIAN_POINT('Ctrl Pts',(-21.2939679585382,-19.0138045492422,
21.0302966251399));
#157589=CARTESIAN_POINT('Ctrl Pts',(-21.29399964838,-18.9533417503911,21.0332900811922));
#157590=CARTESIAN_POINT('',(-21.2964370555865,-18.950145562236,20.9667098902285));
#157591=CARTESIAN_POINT('Ctrl Pts',(-17.1763037530771,-20.9797762769264,
20.6832232033273));
#157592=CARTESIAN_POINT('Ctrl Pts',(-17.4224626753946,-21.171539122868,
20.6987009652428));
#157593=CARTESIAN_POINT('Ctrl Pts',(-18.4657781128202,-21.7248573720238,
20.7565706627188));
#157594=CARTESIAN_POINT('Ctrl Pts',(-20.5735369035609,-21.279131873543,
20.8510662250192));
#157595=CARTESIAN_POINT('Ctrl Pts',(-21.2904547875037,-19.6845342581055,
20.9300840254041));
#157596=CARTESIAN_POINT('Ctrl Pts',(-21.2964370555865,-18.950145562236,
20.9667098902285));
#157597=CARTESIAN_POINT('Ctrl Pts',(-21.2964370555865,-18.950145562236,
20.9667098902285));
#157598=CARTESIAN_POINT('Ctrl Pts',(-21.2973788539875,-18.8345295300019,
20.9724759609645));
#157599=CARTESIAN_POINT('Ctrl Pts',(-21.2376962631739,-17.8698878407826,
21.0206339672611));
#157600=CARTESIAN_POINT('Ctrl Pts',(-20.0126665202556,-16.2082458119612,
21.1111839091181));
#157601=CARTESIAN_POINT('Ctrl Pts',(-17.1190397035347,-16.3916499423084,
21.2383597157995));
#157602=CARTESIAN_POINT('Ctrl Pts',(-15.7420434390129,-18.8613631757064,
21.3623821901447));
#157603=CARTESIAN_POINT('Ctrl Pts',(-16.5519397204913,-20.5025265151668,
21.4440127289293));
#157604=CARTESIAN_POINT('Ctrl Pts',(-17.1722616776481,-20.9849677398537,
21.4832513321535));
#157605=CARTESIAN_POINT('Origin',(23.734,10.1295,7.));
#157606=CARTESIAN_POINT('',(18.1138504785695,10.1294996219627,11.263));
#157607=CARTESIAN_POINT('',(17.7339525131034,10.1295,11.263));
#157608=CARTESIAN_POINT('',(23.734,10.1295,11.263));
#157609=CARTESIAN_POINT('',(17.733926103998,5.86728159109872,6.91639119716989));
#157610=CARTESIAN_POINT('Ctrl Pts',(17.7339050262067,5.86731958600617,6.91641101407837));
#157611=CARTESIAN_POINT('Ctrl Pts',(17.7472715260208,5.8626834471393,7.15280651591456));
#157612=CARTESIAN_POINT('Ctrl Pts',(17.7606427200251,5.87772229287975,7.38918410650487));
#157613=CARTESIAN_POINT('Ctrl Pts',(17.786815786871,5.94601267161834,7.851385147275));
#157614=CARTESIAN_POINT('Ctrl Pts',(17.7995827838462,5.99822391915381,8.07656087620677));
#157615=CARTESIAN_POINT('Ctrl Pts',(17.835119220085,6.19309530208892,8.6870119457575));
#157616=CARTESIAN_POINT('Ctrl Pts',(17.8583297454841,6.37348892203968,9.05758417879396));
#157617=CARTESIAN_POINT('Ctrl Pts',(17.8967844976297,6.75793497537115,9.62310813562425));
#157618=CARTESIAN_POINT('Ctrl Pts',(17.9119480496723,6.93333891295104,9.83420296144228));
#157619=CARTESIAN_POINT('Ctrl Pts',(17.9585777026362,7.53054826773672,10.4264221396266));
#157620=CARTESIAN_POINT('Ctrl Pts',(17.9907447985597,8.0090078993714,10.7414473723924));
#157621=CARTESIAN_POINT('Ctrl Pts',(18.0356178403253,8.75695927515788,11.0430860995625));
#157622=CARTESIAN_POINT('Ctrl Pts',(18.0487834108318,8.98598833752505,11.1137320441811));
#157623=CARTESIAN_POINT('Ctrl Pts',(18.079255259419,9.51889849517406,11.230142863414));
#157624=CARTESIAN_POINT('Ctrl Pts',(18.0966641306137,9.82391712323077,11.2629999729013));
#157625=CARTESIAN_POINT('Ctrl Pts',(18.1138504785695,10.1294996219628,11.263));
#157626=CARTESIAN_POINT('Origin',(17.734,10.1295,7.));
#157627=CARTESIAN_POINT('Origin',(23.734,10.1295,7.));
#157628=CARTESIAN_POINT('',(19.613681670589,10.1293184243372,11.262999996133));
#157629=CARTESIAN_POINT('',(19.2041804397712,10.1295003962013,11.263));
#157630=CARTESIAN_POINT('',(23.734,10.1295,11.263));
#157631=CARTESIAN_POINT('Ctrl Pts',(18.1138504785695,10.1294996219628,11.263));
#157632=CARTESIAN_POINT('Ctrl Pts',(18.1201665818489,10.2418033311226,11.2630000099589));
#157633=CARTESIAN_POINT('Ctrl Pts',(18.1264604938674,10.3541827562155,11.2585622688176));
#157634=CARTESIAN_POINT('Ctrl Pts',(18.1471940248053,10.7247867279603,11.2291842636932));
#157635=CARTESIAN_POINT('Ctrl Pts',(18.1614507417818,10.9807896977882,11.185172584425));
#157636=CARTESIAN_POINT('Ctrl Pts',(18.1906782807484,11.4871350383031,11.0497141872492));
#157637=CARTESIAN_POINT('Ctrl Pts',(18.2057216972168,11.736119762744,10.957539975328));
#157638=CARTESIAN_POINT('Ctrl Pts',(18.2521519575592,12.4777159151984,10.6014088470678));
#157639=CARTESIAN_POINT('Ctrl Pts',(18.2823429382786,12.9282578663991,10.263620068643));
#157640=CARTESIAN_POINT('Ctrl Pts',(18.3296538137456,13.4877135786547,9.64077045992482));
#157641=CARTESIAN_POINT('Ctrl Pts',(18.3454517805426,13.6535680656264,9.41499876952407));
#157642=CARTESIAN_POINT('Ctrl Pts',(18.3746150682435,13.9198075223705,8.96609205758119));
#157643=CARTESIAN_POINT('Ctrl Pts',(18.3879846661531,14.0254683231313,8.74739252579659));
#157644=CARTESIAN_POINT('Ctrl Pts',(18.4231226715518,14.2511090924869,8.15655366404959));
#157645=CARTESIAN_POINT('Ctrl Pts',(18.4453003814799,14.3395929517634,7.77484194259151));
#157646=CARTESIAN_POINT('Ctrl Pts',(18.4823917739119,14.3994905024371,7.11683170769568));
#157647=CARTESIAN_POINT('Ctrl Pts',(18.4973546022919,14.3982932618793,6.8454803979011));
#157648=CARTESIAN_POINT('Ctrl Pts',(18.5347942990784,14.331175004687,6.17388033575934));
#157649=CARTESIAN_POINT('Ctrl Pts',(18.5577058604119,14.2339831082639,5.77944841219729));
#157650=CARTESIAN_POINT('Ctrl Pts',(18.6118397199921,13.8735896061126,4.88640953402182));
#157651=CARTESIAN_POINT('Ctrl Pts',(18.6422259846235,13.564577504846,4.41432857678637));
#157652=CARTESIAN_POINT('Ctrl Pts',(18.7055321258339,12.7810679852525,3.61529247979986));
#157653=CARTESIAN_POINT('Ctrl Pts',(18.7359957101013,12.313775454571,3.29648891512936));
#157654=CARTESIAN_POINT('Ctrl Pts',(18.7812347552267,11.5729279137528,2.98133967923363));
#157655=CARTESIAN_POINT('Ctrl Pts',(18.7951387469876,11.3397888762334,2.90508645340095));
#157656=CARTESIAN_POINT('Ctrl Pts',(18.8352464587369,10.6462678184755,2.74269823580172));
#157657=CARTESIAN_POINT('Ctrl Pts',(18.8606341833889,10.1767051841473,2.71170941449449));
#157658=CARTESIAN_POINT('Ctrl Pts',(18.9034984090833,9.41910717160332,2.78634983706026));
#157659=CARTESIAN_POINT('Ctrl Pts',(18.9201726621107,9.1304431930615,2.84531616915589));
#157660=CARTESIAN_POINT('Ctrl Pts',(18.9522997376604,8.58351430917128,3.01738452781976));
#157661=CARTESIAN_POINT('Ctrl Pts',(18.9677031918578,8.32577932626899,3.12728891895167));
#157662=CARTESIAN_POINT('Ctrl Pts',(19.0109367485974,7.64338159504519,3.50128156788361));
#157663=CARTESIAN_POINT('Ctrl Pts',(19.0393158831965,7.25153182153395,3.81580315655779));
#157664=CARTESIAN_POINT('Ctrl Pts',(19.0795493216095,6.77548652527038,4.3591967363062));
#157665=CARTESIAN_POINT('Ctrl Pts',(19.0918810594698,6.64150701319289,4.53887176488872));
#157666=CARTESIAN_POINT('Ctrl Pts',(19.1230560174742,6.34314182400765,5.01263327675107));
#157667=CARTESIAN_POINT('Ctrl Pts',(19.1421738225493,6.19829725781291,5.31721393769373));
#157668=CARTESIAN_POINT('Ctrl Pts',(19.1853171399678,5.95271794430234,6.04416714316602));
#157669=CARTESIAN_POINT('Ctrl Pts',(19.2087798990235,5.8774910195126,6.47128620995645));
#157670=CARTESIAN_POINT('Ctrl Pts',(19.2466843093111,5.86205261143494,7.14537690669814));
#157671=CARTESIAN_POINT('Ctrl Pts',(19.2604937503701,5.87727780168091,7.3883930320663));
#157672=CARTESIAN_POINT('Ctrl Pts',(19.3005707743551,5.98219667984587,8.09193506062706));
#157673=CARTESIAN_POINT('Ctrl Pts',(19.3260125741856,6.12710547128438,8.54054648012738));
#157674=CARTESIAN_POINT('Ctrl Pts',(19.3678816644823,6.46864618458046,9.20168746218623));
#157675=CARTESIAN_POINT('Ctrl Pts',(19.3835202161449,6.61876411563961,9.43393026367854));
#157676=CARTESIAN_POINT('Ctrl Pts',(19.414638151997,6.96381222178052,9.8687156698808));
#157677=CARTESIAN_POINT('Ctrl Pts',(19.4300392252702,7.15842094953444,10.0698209042673));
#157678=CARTESIAN_POINT('Ctrl Pts',(19.473442030871,7.75442043537448,10.5755628582299));
#157679=CARTESIAN_POINT('Ctrl Pts',(19.5020877234821,8.19201943815246,10.8303801925215));
#157680=CARTESIAN_POINT('Ctrl Pts',(19.5439781330779,8.89730494092279,11.0886021060379));
#157681=CARTESIAN_POINT('Ctrl Pts',(19.5576540928679,9.13777911174077,11.1534877285564));
#157682=CARTESIAN_POINT('Ctrl Pts',(19.5854375418345,9.6290530629089,11.2409219828863));
#157683=CARTESIAN_POINT('Ctrl Pts',(19.5996142344451,9.8789470933161,11.2629891261597));
#157684=CARTESIAN_POINT('Ctrl Pts',(19.6137437552536,10.1293149200936,11.2629999959823));
#157685=CARTESIAN_POINT('',(17.734,10.6581555755053,11.2300936493755));
#157686=CARTESIAN_POINT('Origin',(17.734,10.1295,7.));
#157687=CARTESIAN_POINT('Ctrl Pts',(17.734,10.6581555755053,11.2300936493755));
#157688=CARTESIAN_POINT('Ctrl Pts',(17.7616949897363,11.1488824019432,11.1687651081304));
#157689=CARTESIAN_POINT('Ctrl Pts',(17.7887411547574,11.6252164816622,11.0225101169825));
#157690=CARTESIAN_POINT('Ctrl Pts',(17.8283704905734,12.2488459039359,10.7045581296159));
#157691=CARTESIAN_POINT('Ctrl Pts',(17.840040605835,12.4248958275708,10.5981298986797));
#157692=CARTESIAN_POINT('Ctrl Pts',(17.8641028867666,12.77549500137,10.3499403602549));
#157693=CARTESIAN_POINT('Ctrl Pts',(17.8764490032863,12.9479121974887,10.206235555167));
#157694=CARTESIAN_POINT('Ctrl Pts',(17.9199030297306,13.5074194414442,9.65973748271246));
#157695=CARTESIAN_POINT('Ctrl Pts',(17.9515980360201,13.8261895030659,9.19522934563977));
#157696=CARTESIAN_POINT('Ctrl Pts',(17.9980916364257,14.1567255204859,8.42573715427207));
#157697=CARTESIAN_POINT('Ctrl Pts',(18.0135132032873,14.2415069949429,8.15873529814874));
#157698=CARTESIAN_POINT('Ctrl Pts',(18.0446456785229,14.356767835986,7.61585955813702));
#157699=CARTESIAN_POINT('Ctrl Pts',(18.0602767788215,14.3877260386578,7.34144189889881));
#157700=CARTESIAN_POINT('Ctrl Pts',(18.0972674830967,14.3978911621874,6.68465423453746));
#157701=CARTESIAN_POINT('Ctrl Pts',(18.1180690129512,14.3525994780205,6.30427024344823));
#157702=CARTESIAN_POINT('Ctrl Pts',(18.1543442829001,14.1906202473075,5.67645811688825));
#157703=CARTESIAN_POINT('Ctrl Pts',(18.16944942413,14.0997743614236,5.42476163756622));
#157704=CARTESIAN_POINT('Ctrl Pts',(18.2068329217642,13.8178295802788,4.82627311027319));
#157705=CARTESIAN_POINT('Ctrl Pts',(18.2284118162708,13.6009250725321,4.49439078429331));
#157706=CARTESIAN_POINT('Ctrl Pts',(18.2655893604534,13.1629216798711,3.99246341933803));
#157707=CARTESIAN_POINT('Ctrl Pts',(18.2809099585374,12.9652186480114,3.80537710443323));
#157708=CARTESIAN_POINT('Ctrl Pts',(18.3192591952197,12.4304752860569,3.38835543633559));
#157709=CARTESIAN_POINT('Ctrl Pts',(18.3415514937179,12.0757504454465,3.18547745510687));
#157710=CARTESIAN_POINT('Ctrl Pts',(18.3794657800805,11.4433735390018,2.93531061625104));
#157711=CARTESIAN_POINT('Ctrl Pts',(18.3948739914762,11.1799788566158,2.85941435868902));
#157712=CARTESIAN_POINT('Ctrl Pts',(18.4424275943522,10.3536066845282,2.70528145186069));
#157713=CARTESIAN_POINT('Ctrl Pts',(18.4731668243514,9.78087981819454,2.71359051196341));
#157714=CARTESIAN_POINT('Ctrl Pts',(18.518505973483,8.99449974862713,2.88401448716478));
#157715=CARTESIAN_POINT('Ctrl Pts',(18.5319909201975,8.76702457031755,2.95361613557958));
#157716=CARTESIAN_POINT('Ctrl Pts',(18.5686141586478,8.16162068842985,3.19572972788208));
#157717=CARTESIAN_POINT('Ctrl Pts',(18.5911937657581,7.80121566223636,3.40498683764839));
#157718=CARTESIAN_POINT('Ctrl Pts',(18.6291066957715,7.2730386993043,3.82486380705621));
#157719=CARTESIAN_POINT('Ctrl Pts',(18.6438750234105,7.08462699739337,4.0050699100077));
#157720=CARTESIAN_POINT('Ctrl Pts',(18.6734339719351,6.73987280833042,4.40119196250021));
#157721=CARTESIAN_POINT('Ctrl Pts',(18.6880123692262,6.58493645837877,4.61684085395999));
#157722=CARTESIAN_POINT('Ctrl Pts',(18.7336162491048,6.16995756759497,5.32534722466218));
#157723=CARTESIAN_POINT('Ctrl Pts',(18.7652059626455,5.98549365249281,5.85560035998954));
#157724=CARTESIAN_POINT('Ctrl Pts',(18.8116030190859,5.86912190868235,6.68305429248612));
#157725=CARTESIAN_POINT('Ctrl Pts',(18.8270172348669,5.85750963450242,6.96296049691824));
#157726=CARTESIAN_POINT('Ctrl Pts',(18.8583521429971,5.88922794992203,7.5208417297993));
#157727=CARTESIAN_POINT('Ctrl Pts',(18.8741990497534,5.9324506783649,7.79746776882433));
#157728=CARTESIAN_POINT('Ctrl Pts',(18.9167047062517,6.12147134216349,8.52799592711725));
#157729=CARTESIAN_POINT('Ctrl Pts',(18.9425081610268,6.31664167906196,8.96498829608126));
#157730=CARTESIAN_POINT('Ctrl Pts',(18.9829337727668,6.71411921308159,9.56264230070435));
#157731=CARTESIAN_POINT('Ctrl Pts',(18.9967032709609,6.86537344567519,9.75271471476632));
#157732=CARTESIAN_POINT('Ctrl Pts',(19.0341600899032,7.3234092395884,10.2371236706298));
#157733=CARTESIAN_POINT('Ctrl Pts',(19.0572543340028,7.65923372746821,10.5001293577879));
#157734=CARTESIAN_POINT('Ctrl Pts',(19.0957939377919,8.25570526069354,10.8380136743055));
#157735=CARTESIAN_POINT('Ctrl Pts',(19.1106329303094,8.49443402195775,10.9456320449966));
#157736=CARTESIAN_POINT('Ctrl Pts',(19.1519247463186,9.18867344018609,11.1846962566353));
#157737=CARTESIAN_POINT('Ctrl Pts',(19.1775909397056,9.65778711534599,11.263000043841));
#157738=CARTESIAN_POINT('Ctrl Pts',(19.2041804397713,10.1295003962029,11.263));
#157739=CARTESIAN_POINT('Origin',(23.734,10.1295,7.));
#157740=CARTESIAN_POINT('',(21.113681670589,10.1298201264287,11.2629999879802));
#157741=CARTESIAN_POINT('',(20.7043183294109,10.1330470789259,11.2629985243055));
#157742=CARTESIAN_POINT('',(23.734,10.1295,11.263));
#157743=CARTESIAN_POINT('Ctrl Pts',(19.613681670589,10.1293184243372,11.262999996133));
#157744=CARTESIAN_POINT('Ctrl Pts',(19.6210623037642,10.2610687195736,11.263005607826));
#157745=CARTESIAN_POINT('Ctrl Pts',(19.6284429369393,10.3928267771473,11.2568991564636));
#157746=CARTESIAN_POINT('Ctrl Pts',(19.6358235701145,10.5240278125494,11.2447045604052));
#157747=CARTESIAN_POINT('Ctrl Pts',(19.6432028342893,10.6552045120622,11.2325122262675));
#157748=CARTESIAN_POINT('Ctrl Pts',(19.650582098464,10.7858240783452,11.2142340323102));
#157749=CARTESIAN_POINT('Ctrl Pts',(19.6579613626388,10.9153264213143,11.1899458034161));
#157750=CARTESIAN_POINT('Ctrl Pts',(19.6653396985726,11.044812474126,11.1656606297492));
#157751=CARTESIAN_POINT('Ctrl Pts',(19.6727180345064,11.1731812706445,11.1353669878975));
#157752=CARTESIAN_POINT('Ctrl Pts',(19.6800963704403,11.2998820511657,11.0991919757812));
#157753=CARTESIAN_POINT('Ctrl Pts',(19.6849288196367,11.382864866059,11.0754991119973));
#157754=CARTESIAN_POINT('Ctrl Pts',(19.6897612688331,11.4651323638681,11.0492844183613));
#157755=CARTESIAN_POINT('Ctrl Pts',(19.6945937180296,11.5465329042847,11.0205953226076));
#157756=CARTESIAN_POINT('Ctrl Pts',(19.7016231773756,11.6649411412557,10.9788631027588));
#157757=CARTESIAN_POINT('Ctrl Pts',(19.7086526367216,11.7815525661295,10.9318790465684));
#157758=CARTESIAN_POINT('Ctrl Pts',(19.7156820960676,11.8958854944383,10.8798261926326));
#157759=CARTESIAN_POINT('Ctrl Pts',(19.722709782053,12.0101895793458,10.8277864703587));
#157760=CARTESIAN_POINT('Ctrl Pts',(19.7297374680383,12.1222159630139,10.7706806571767));
#157761=CARTESIAN_POINT('Ctrl Pts',(19.7367651540237,12.2315037832726,10.7087395561171));
#157762=CARTESIAN_POINT('Ctrl Pts',(19.7437942650805,12.3408137648732,10.6467858946649));
#157763=CARTESIAN_POINT('Ctrl Pts',(19.7508233761373,12.4473837362772,10.5799951717423));
#157764=CARTESIAN_POINT('Ctrl Pts',(19.7578524871941,12.5507782076321,10.5086437324479));
#157765=CARTESIAN_POINT('Ctrl Pts',(19.7648822673835,12.6541825215712,10.4372855008895));
#157766=CARTESIAN_POINT('Ctrl Pts',(19.771912047573,12.7544104201016,10.3613659117439));
#157767=CARTESIAN_POINT('Ctrl Pts',(19.7789418277624,12.8510567997471,10.2812036794065));
#157768=CARTESIAN_POINT('Ctrl Pts',(19.7859761861195,12.947766120667,10.20098924115));
#157769=CARTESIAN_POINT('Ctrl Pts',(19.7930105444766,13.0408889712832,10.116526891086));
#157770=CARTESIAN_POINT('Ctrl Pts',(19.8000449028336,13.1300544842105,10.0281746626118));
#157771=CARTESIAN_POINT('Ctrl Pts',(19.803676389535,13.176086170113,9.9825628347157));
#157772=CARTESIAN_POINT('Ctrl Pts',(19.8073078762364,13.2210637677684,9.93591490652767));
#157773=CARTESIAN_POINT('Ctrl Pts',(19.8109393629378,13.2649402640227,9.88828380716734));
#157774=CARTESIAN_POINT('Ctrl Pts',(19.8185510511639,13.3569065129464,9.788447814911));
#157775=CARTESIAN_POINT('Ctrl Pts',(19.82616273939,13.4440921851538,9.68422623732347));
#157776=CARTESIAN_POINT('Ctrl Pts',(19.8337744276161,13.5261126987745,9.57608058385672));
#157777=CARTESIAN_POINT('Ctrl Pts',(19.8415669759686,13.6100820889147,9.46536529853304));
#157778=CARTESIAN_POINT('Ctrl Pts',(19.8493595243211,13.6886375971267,9.350537337596));
#157779=CARTESIAN_POINT('Ctrl Pts',(19.8571520726736,13.7614114960694,9.23212631468719));
#157780=CARTESIAN_POINT('Ctrl Pts',(19.8647577752929,13.8324404597364,9.11655449063818));
#157781=CARTESIAN_POINT('Ctrl Pts',(19.8723634779121,13.8979617722854,8.99756971412403));
#157782=CARTESIAN_POINT('Ctrl Pts',(19.8799691805314,13.9576776738065,8.87569312462606));
#157783=CARTESIAN_POINT('Ctrl Pts',(19.8878551517505,14.0195940941942,8.74932540750959));
#157784=CARTESIAN_POINT('Ctrl Pts',(19.8957411229696,14.0752688994055,8.61984891580091));
#157785=CARTESIAN_POINT('Ctrl Pts',(19.9036270941887,14.1244221857155,8.48787288774221));
#157786=CARTESIAN_POINT('Ctrl Pts',(19.9115130654078,14.1735754720254,8.35589685968352));
#157787=CARTESIAN_POINT('Ctrl Pts',(19.9193990366269,14.2162070893851,8.22142157961869));
#157788=CARTESIAN_POINT('Ctrl Pts',(19.9272850078459,14.2520924147731,8.08508100234748));
#157789=CARTESIAN_POINT('Ctrl Pts',(19.9343239536661,14.2841233281666,7.9633846494403));
#157790=CARTESIAN_POINT('Ctrl Pts',(19.9413628994862,14.3107676181272,7.8402454199408));
#157791=CARTESIAN_POINT('Ctrl Pts',(19.9484018453063,14.3319126474473,7.71616823482706));
#157792=CARTESIAN_POINT('Ctrl Pts',(19.9554405817332,14.3530570477492,7.59209474073655));
#157793=CARTESIAN_POINT('Ctrl Pts',(19.9624793181602,14.3687024503286,7.4670837237731));
#157794=CARTESIAN_POINT('Ctrl Pts',(19.9695180545871,14.3787875954937,7.34164884133137));
#157795=CARTESIAN_POINT('Ctrl Pts',(19.976560483799,14.3888780317039,7.21614815104951));
#157796=CARTESIAN_POINT('Ctrl Pts',(19.9836029130109,14.3934023507515,7.09022353254098));
#157797=CARTESIAN_POINT('Ctrl Pts',(19.9906453422228,14.3923512886368,6.96439254336727));
#157798=CARTESIAN_POINT('Ctrl Pts',(19.9976897288499,14.3912999343835,6.83852657996872));
#157799=CARTESIAN_POINT('Ctrl Pts',(20.0047341154771,14.384670122848,6.71275468020004));
#157800=CARTESIAN_POINT('Ctrl Pts',(20.0117785021043,14.3725046893258,6.58759218441076));
#157801=CARTESIAN_POINT('Ctrl Pts',(20.0188293217025,14.3603281462655,6.46231538956881));
#157802=CARTESIAN_POINT('Ctrl Pts',(20.0258801413008,14.3426059296771,6.33764949029167));
#157803=CARTESIAN_POINT('Ctrl Pts',(20.032930960899,14.3194325420246,6.21410287360031));
#157804=CARTESIAN_POINT('Ctrl Pts',(20.0364975248507,14.3077105900036,6.15160844961165));
#157805=CARTESIAN_POINT('Ctrl Pts',(20.0400640888024,14.2945946542908,6.08940024916908));
#157806=CARTESIAN_POINT('Ctrl Pts',(20.043630652754,14.2801018815878,6.02754279242752));
#157807=CARTESIAN_POINT('Ctrl Pts',(20.0506540757907,14.2515621231407,5.9057305685185));
#157808=CARTESIAN_POINT('Ctrl Pts',(20.0576774988273,14.2176287610004,5.78506067889005));
#157809=CARTESIAN_POINT('Ctrl Pts',(20.064700921864,14.178413687597,5.66603337733305));
#157810=CARTESIAN_POINT('Ctrl Pts',(20.0717185186296,14.1392311450044,5.54710481471211));
#157811=CARTESIAN_POINT('Ctrl Pts',(20.0787361153952,14.0947757355895,5.42981649293811));
#157812=CARTESIAN_POINT('Ctrl Pts',(20.0857537121608,14.0452096568303,5.31465526274116));
#157813=CARTESIAN_POINT('Ctrl Pts',(20.0927670515899,13.9956736481201,5.19956389693379));
#157814=CARTESIAN_POINT('Ctrl Pts',(20.0997803910189,13.9410332971071,5.08659740716836));
#157815=CARTESIAN_POINT('Ctrl Pts',(20.106793730448,13.8814994526977,4.97622404724333));
#157816=CARTESIAN_POINT('Ctrl Pts',(20.1138574059531,13.821538322521,4.86505851664211));
#157817=CARTESIAN_POINT('Ctrl Pts',(20.1209210814582,13.7566133174844,4.75652385852162));
#157818=CARTESIAN_POINT('Ctrl Pts',(20.1279847569633,13.6869877988477,4.65107480726828));
#157819=CARTESIAN_POINT('Ctrl Pts',(20.1349957098057,13.6178819590572,4.54641281860872));
#157820=CARTESIAN_POINT('Ctrl Pts',(20.1420066626481,13.5441457768754,4.4447908421696));
#157821=CARTESIAN_POINT('Ctrl Pts',(20.1490176154904,13.4660808058284,4.34662525711552));
#157822=CARTESIAN_POINT('Ctrl Pts',(20.1560292419106,13.3880083346838,4.24845024079589));
#157823=CARTESIAN_POINT('Ctrl Pts',(20.1630408683308,13.3056064871499,4.15373257998509));
#157824=CARTESIAN_POINT('Ctrl Pts',(20.1700524947509,13.2192173973556,4.06285591016064));
#157825=CARTESIAN_POINT('Ctrl Pts',(20.1770662121528,13.1328025449214,3.97195213942652));
#157826=CARTESIAN_POINT('Ctrl Pts',(20.1840799295547,13.0423983490892,3.8848919206958));
#157827=CARTESIAN_POINT('Ctrl Pts',(20.1910936469566,12.9483838509154,3.80202207089415));
#157828=CARTESIAN_POINT('Ctrl Pts',(20.1981960049244,12.8531811813556,3.71810489768801));
#157829=CARTESIAN_POINT('Ctrl Pts',(20.2052983628922,12.7542766304511,3.63848501133126));
#157830=CARTESIAN_POINT('Ctrl Pts',(20.2124007208601,12.6520974127302,3.56347976969624));
#157831=CARTESIAN_POINT('Ctrl Pts',(20.2194266380452,12.5510179226514,3.48928178945322));
#157832=CARTESIAN_POINT('Ctrl Pts',(20.2264525552303,12.4467342673697,3.41959977243168));
#157833=CARTESIAN_POINT('Ctrl Pts',(20.2334784724154,12.3396876781542,3.35469625033312));
#157834=CARTESIAN_POINT('Ctrl Pts',(20.2406190507746,12.2308941159415,3.28873351932974));
#157835=CARTESIAN_POINT('Ctrl Pts',(20.2477596291338,12.1192470170137,3.22770681705742));
#157836=CARTESIAN_POINT('Ctrl Pts',(20.254900207493,12.0052331387805,3.17184193219762));
#157837=CARTESIAN_POINT('Ctrl Pts',(20.2620407858522,11.8912192605474,3.11597704733782));
#157838=CARTESIAN_POINT('Ctrl Pts',(20.2691813642114,11.7748390041325,3.06527409536859));
#157839=CARTESIAN_POINT('Ctrl Pts',(20.2763219425706,11.6565970046819,3.01990656663797));
#157840=CARTESIAN_POINT('Ctrl Pts',(20.2831124368812,11.5441521039813,2.97676329024846));
#157841=CARTESIAN_POINT('Ctrl Pts',(20.2899029311918,11.4296496272437,2.93830180029273));
#157842=CARTESIAN_POINT('Ctrl Pts',(20.2966934255024,11.3135242806343,2.90472766438319));
#157843=CARTESIAN_POINT('Ctrl Pts',(20.3034747086535,11.1975564555602,2.87119907106695));
#157844=CARTESIAN_POINT('Ctrl Pts',(20.3102559918046,11.0799705337984,2.84254477101641));
#157845=CARTESIAN_POINT('Ctrl Pts',(20.3170372749558,10.9612220024664,2.81892268540592));
#157846=CARTESIAN_POINT('Ctrl Pts',(20.3238112366047,10.8426016795597,2.79532610369315));
#157847=CARTESIAN_POINT('Ctrl Pts',(20.3305851982536,10.7228216505048,2.77675101741854));
#157848=CARTESIAN_POINT('Ctrl Pts',(20.3373591599025,10.602352688061,2.76330561222627));
#157849=CARTESIAN_POINT('Ctrl Pts',(20.3441276801126,10.48198049683,2.74987100756003));
#157850=CARTESIAN_POINT('Ctrl Pts',(20.3508962003228,10.3609208876254,2.74155793704571));
#157851=CARTESIAN_POINT('Ctrl Pts',(20.3576647205329,10.2396542166227,2.73842340810819));
#157852=CARTESIAN_POINT('Ctrl Pts',(20.3644304116747,10.1184382319863,2.73529018932358));
#157853=CARTESIAN_POINT('Ctrl Pts',(20.3711961028166,9.99701577598613,2.73733122414958));
#157854=CARTESIAN_POINT('Ctrl Pts',(20.3779617939584,9.8758711148973,2.74455156433055));
#157855=CARTESIAN_POINT('Ctrl Pts',(20.3847262515225,9.7547485419237,2.75177058803827));
#157856=CARTESIAN_POINT('Ctrl Pts',(20.3914907090865,9.63390408190446,2.76416701590755));
#157857=CARTESIAN_POINT('Ctrl Pts',(20.3982551666505,9.51381996728511,2.78169381181069));
#157858=CARTESIAN_POINT('Ctrl Pts',(20.4050200814275,9.39372773612192,2.79922179235852));
#157859=CARTESIAN_POINT('Ctrl Pts',(20.4117849962045,9.27439636769387,2.82188076925702));
#157860=CARTESIAN_POINT('Ctrl Pts',(20.4185499109815,9.15630016132667,2.8495721818099));
#157861=CARTESIAN_POINT('Ctrl Pts',(20.4253169740298,9.03816645224213,2.87727238806794));
#157862=CARTESIAN_POINT('Ctrl Pts',(20.4320840370781,8.92126909293508,2.91000810994903));
#157863=CARTESIAN_POINT('Ctrl Pts',(20.4388511001264,8.8060686569394,2.94763051040446));
#157864=CARTESIAN_POINT('Ctrl Pts',(20.4456261525318,8.69073221254255,2.98529732876934));
#157865=CARTESIAN_POINT('Ctrl Pts',(20.4524012049372,8.57709708877692,3.02786220934678));
#157866=CARTESIAN_POINT('Ctrl Pts',(20.4591762573426,8.46560533251585,3.07512757716664));
#157867=CARTESIAN_POINT('Ctrl Pts',(20.465955865875,8.3540385996251,3.12242473027806));
#157868=CARTESIAN_POINT('Ctrl Pts',(20.4727354744074,8.24461847941592,3.17442847978152));
#157869=CARTESIAN_POINT('Ctrl Pts',(20.4795150829397,8.13776210427539,3.23089544391052));
#157870=CARTESIAN_POINT('Ctrl Pts',(20.4863055094517,8.03073522222619,3.28745251036128));
#157871=CARTESIAN_POINT('Ctrl Pts',(20.4930959359638,7.92628060892515,3.34848679214083));
#157872=CARTESIAN_POINT('Ctrl Pts',(20.4998863624758,7.82478626913523,3.41371172118535));
#157873=CARTESIAN_POINT('Ctrl Pts',(20.5029286524462,7.77931413105292,3.44293420774036));
#157874=CARTESIAN_POINT('Ctrl Pts',(20.5059709424165,7.73443575525086,3.4729973349816));
#157875=CARTESIAN_POINT('Ctrl Pts',(20.5090132323869,7.69018375192213,3.50387282241288));
#157876=CARTESIAN_POINT('Ctrl Pts',(20.5160528480572,7.58778815547792,3.57531623091908));
#157877=CARTESIAN_POINT('Ctrl Pts',(20.5230924637274,7.48839576824068,3.65135791091549));
#157878=CARTESIAN_POINT('Ctrl Pts',(20.5301320793977,7.39243615095284,3.73172056178803));
#157879=CARTESIAN_POINT('Ctrl Pts',(20.5371627089137,7.29659902727188,3.81198062876912));
#157880=CARTESIAN_POINT('Ctrl Pts',(20.5441933384298,7.20418624476916,3.89655044007299));
#157881=CARTESIAN_POINT('Ctrl Pts',(20.5512239679459,7.11559764941311,3.98511001508732));
#157882=CARTESIAN_POINT('Ctrl Pts',(20.5582471924636,7.0271023598425,4.07357631488181));
#157883=CARTESIAN_POINT('Ctrl Pts',(20.5652704169812,6.94242351009667,4.16602373977542));
#157884=CARTESIAN_POINT('Ctrl Pts',(20.5722936414989,6.86192690158119,4.26209294414699));
#157885=CARTESIAN_POINT('Ctrl Pts',(20.5793524281949,6.78102269755993,4.3586485960431));
#157886=CARTESIAN_POINT('Ctrl Pts',(20.5864112148909,6.70434351288937,4.45886255685475));
#157887=CARTESIAN_POINT('Ctrl Pts',(20.5934700015869,6.63222286897191,4.56233274034623));
#157888=CARTESIAN_POINT('Ctrl Pts',(20.6004830794517,6.56056923879038,4.66513290767694));
#157889=CARTESIAN_POINT('Ctrl Pts',(20.6074961573164,6.49341550627245,4.77114692695205));
#157890=CARTESIAN_POINT('Ctrl Pts',(20.6145092351811,6.4310476922353,4.87994822535157));
#157891=CARTESIAN_POINT('Ctrl Pts',(20.6215200654578,6.36869986616283,4.9887146545394));
#157892=CARTESIAN_POINT('Ctrl Pts',(20.6285308957345,6.31113509680343,5.10026624921301));
#157893=CARTESIAN_POINT('Ctrl Pts',(20.6355417260111,6.25859484105923,5.21414943220723));
#157894=CARTESIAN_POINT('Ctrl Pts',(20.6425517265455,6.20606080353314,5.32801913695587));
#157895=CARTESIAN_POINT('Ctrl Pts',(20.6495617270799,6.15855025661158,5.44421952922821));
#157896=CARTESIAN_POINT('Ctrl Pts',(20.6565717276143,6.11625749444774,5.56227485532575));
#157897=CARTESIAN_POINT('Ctrl Pts',(20.6636661271634,6.07345553582416,5.68175154411103));
#157898=CARTESIAN_POINT('Ctrl Pts',(20.6707605267125,6.0359979916284,5.80312775504321));
#157899=CARTESIAN_POINT('Ctrl Pts',(20.6778549262616,6.00403488298935,5.92589266442861));
#157900=CARTESIAN_POINT('Ctrl Pts',(20.6848699695753,5.97242930594331,6.04728435526654));
#157901=CARTESIAN_POINT('Ctrl Pts',(20.691885012889,5.94619591700699,6.17003344375839));
#157902=CARTESIAN_POINT('Ctrl Pts',(20.6989000562027,5.92542852701159,6.29363462004067));
#157903=CARTESIAN_POINT('Ctrl Pts',(20.7060341338695,5.90430874677111,6.41933311566898));
#157904=CARTESIAN_POINT('Ctrl Pts',(20.7131682115363,5.88884222559255,6.54591246948119));
#157905=CARTESIAN_POINT('Ctrl Pts',(20.720302289203,5.87907269796409,6.67283528596788));
#157906=CARTESIAN_POINT('Ctrl Pts',(20.7274363668698,5.86930317033562,6.79975810245456));
#157907=CARTESIAN_POINT('Ctrl Pts',(20.7345704445365,5.86523062067719,6.92702396271638));
#157908=CARTESIAN_POINT('Ctrl Pts',(20.7417045222033,5.86684324052786,7.05409575700999));
#157909=CARTESIAN_POINT('Ctrl Pts',(20.7487555408127,5.86843708532577,7.17968810799774));
#157910=CARTESIAN_POINT('Ctrl Pts',(20.7558065594222,5.87558719238043,7.30531726205016));
#157911=CARTESIAN_POINT('Ctrl Pts',(20.7628575780316,5.88828942330491,7.43046700701646));
#157912=CARTESIAN_POINT('Ctrl Pts',(20.7699032665315,5.90098205217249,7.55552214695005));
#157913=CARTESIAN_POINT('Ctrl Pts',(20.7769489550314,5.91921840902034,7.68009822009394));
#157914=CARTESIAN_POINT('Ctrl Pts',(20.7839946435314,5.94294234854903,7.80368154829967));
#157915=CARTESIAN_POINT('Ctrl Pts',(20.7910363483395,5.96665287436202,7.92719500144824));
#157916=CARTESIAN_POINT('Ctrl Pts',(20.7980780531477,5.99584473055009,8.04971645279611));
#157917=CARTESIAN_POINT('Ctrl Pts',(20.8051197579558,6.03041028946687,8.17074016972232));
#157918=CARTESIAN_POINT('Ctrl Pts',(20.8121590390629,6.06496395118215,8.29172223120907));
#157919=CARTESIAN_POINT('Ctrl Pts',(20.81919832017,6.10488752575289,8.41120721791972));
#157920=CARTESIAN_POINT('Ctrl Pts',(20.8262376012772,6.15002298728712,8.528702621601));
#157921=CARTESIAN_POINT('Ctrl Pts',(20.8332767281295,6.19515745974894,8.64619545055594));
#157922=CARTESIAN_POINT('Ctrl Pts',(20.8403158549819,6.24550345864841,8.76169842478665));
#157923=CARTESIAN_POINT('Ctrl Pts',(20.8473549818343,6.30085412572507,8.87473725342982));
#157924=CARTESIAN_POINT('Ctrl Pts',(20.8509200435934,6.32888722566361,8.93198730925843));
#157925=CARTESIAN_POINT('Ctrl Pts',(20.8544851053524,6.35820328570989,8.98860562121714));
#157926=CARTESIAN_POINT('Ctrl Pts',(20.8580501671115,6.38877083910759,9.04453279378179));
#157927=CARTESIAN_POINT('Ctrl Pts',(20.8656419313286,6.45386414569605,9.16362916184931));
#157928=CARTESIAN_POINT('Ctrl Pts',(20.8732336955456,6.52461037034493,9.27954435589301));
#157929=CARTESIAN_POINT('Ctrl Pts',(20.8808254597627,6.60067979658225,9.39177694862015));
#157930=CARTESIAN_POINT('Ctrl Pts',(20.8886229891175,6.67881098811066,9.50705146338693));
#157931=CARTESIAN_POINT('Ctrl Pts',(20.8964205184722,6.7625578532525,9.61844067454016));
#157932=CARTESIAN_POINT('Ctrl Pts',(20.904218047827,6.85151803388108,9.72543633750618));
#157933=CARTESIAN_POINT('Ctrl Pts',(20.9118262952094,6.93831874095385,9.82983472264376));
#157934=CARTESIAN_POINT('Ctrl Pts',(20.9194345425919,7.03008237539708,9.93005022576152));
#157935=CARTESIAN_POINT('Ctrl Pts',(20.9270427899744,7.12639604911989,10.0256463210706));
#157936=CARTESIAN_POINT('Ctrl Pts',(20.9349349603153,7.22630393604349,10.1248098511419));
#157937=CARTESIAN_POINT('Ctrl Pts',(20.9428271306562,7.3311078117208,10.219002308715));
#157938=CARTESIAN_POINT('Ctrl Pts',(20.950719300997,7.4403062336633,10.3077796007437));
#157939=CARTESIAN_POINT('Ctrl Pts',(20.9586114713379,7.5495046556058,10.3965568927723));
#157940=CARTESIAN_POINT('Ctrl Pts',(20.9665036416788,7.66309737480791,10.4799188219024));
#157941=CARTESIAN_POINT('Ctrl Pts',(20.9743958120197,7.78054523318155,10.5574682716));
#157942=CARTESIAN_POINT('Ctrl Pts',(20.9814302636453,7.88522889338838,10.6265896702683));
#157943=CARTESIAN_POINT('Ctrl Pts',(20.9884647152709,7.99303771031586,10.6911341334027));
#157944=CARTESIAN_POINT('Ctrl Pts',(20.9954991668964,8.10354027043256,10.750820733409));
#157945=CARTESIAN_POINT('Ctrl Pts',(21.0025297316031,8.2139817718456,10.8104743533069));
#157946=CARTESIAN_POINT('Ctrl Pts',(21.0095602963097,8.32711371454162,10.8652752730648));
#157947=CARTESIAN_POINT('Ctrl Pts',(21.0165908610163,8.44247818970125,10.9149874088656));
#157948=CARTESIAN_POINT('Ctrl Pts',(21.0236196792195,8.55781400650079,10.9646871953857));
#157949=CARTESIAN_POINT('Ctrl Pts',(21.0306484974226,8.67538089984565,11.0093005597809));
#157950=CARTESIAN_POINT('Ctrl Pts',(21.0376773156258,8.79469914404457,11.0486387434471));
#157951=CARTESIAN_POINT('Ctrl Pts',(21.0447049946651,8.91399805027931,11.0879705515553));
#157952=CARTESIAN_POINT('Ctrl Pts',(21.0517326737043,9.03504737574514,11.1220287644151));
#157953=CARTESIAN_POINT('Ctrl Pts',(21.0587603527436,9.15735080920185,11.1506740357237));
#157954=CARTESIAN_POINT('Ctrl Pts',(21.0657898849612,9.27968649371527,11.1793268607063));
#157955=CARTESIAN_POINT('Ctrl Pts',(21.0728194171789,9.40327657205448,11.2025638053603));
#157956=CARTESIAN_POINT('Ctrl Pts',(21.0798489493965,9.52761306300916,11.220296330245));
#157957=CARTESIAN_POINT('Ctrl Pts',(21.0834797852403,9.59183431900078,11.2294553873429));
#157958=CARTESIAN_POINT('Ctrl Pts',(21.0871106210841,9.65625455719416,11.2371467896353));
#157959=CARTESIAN_POINT('Ctrl Pts',(21.0907414569279,9.7208031090756,11.2433637425218));
#157960=CARTESIAN_POINT('Ctrl Pts',(21.0983881948149,9.8567458722469,11.2564569836444));
#157961=CARTESIAN_POINT('Ctrl Pts',(21.106034932702,9.99328288766813,11.2630102411303));
#157962=CARTESIAN_POINT('Ctrl Pts',(21.113681670589,10.1298201264287,11.2629999879802));
#157963=CARTESIAN_POINT('Ctrl Pts',(19.2041804397713,10.1295003962029,11.263));
#157964=CARTESIAN_POINT('Ctrl Pts',(19.2091555282883,10.2177613759535,11.262999991797));
#157965=CARTESIAN_POINT('Ctrl Pts',(19.2141496156627,10.3061141204568,11.2602590201419));
#157966=CARTESIAN_POINT('Ctrl Pts',(19.2344704543066,10.6646652801004,11.2379329571964));
#157967=CARTESIAN_POINT('Ctrl Pts',(19.2496908524141,10.9326920234655,11.1953988307096));
#157968=CARTESIAN_POINT('Ctrl Pts',(19.2797046258122,11.4565285457862,11.0601954318409));
#157969=CARTESIAN_POINT('Ctrl Pts',(19.2946346817085,11.7111627636934,10.9679378982786));
#157970=CARTESIAN_POINT('Ctrl Pts',(19.3315996560539,12.3063541787618,10.6858325829712));
#157971=CARTESIAN_POINT('Ctrl Pts',(19.3536978982461,12.6329899403981,10.4722627163212));
#157972=CARTESIAN_POINT('Ctrl Pts',(19.3877230669708,13.0950538749999,10.0706235651989));
#157973=CARTESIAN_POINT('Ctrl Pts',(19.4000640296122,13.2521141818841,9.91075924709942));
#157974=CARTESIAN_POINT('Ctrl Pts',(19.4357312298586,13.6630070448086,9.4208033139932));
#157975=CARTESIAN_POINT('Ctrl Pts',(19.4593953461805,13.8820913705074,9.06494763762778));
#157976=CARTESIAN_POINT('Ctrl Pts',(19.4958359772684,14.1395982420948,8.46569002107918));
#157977=CARTESIAN_POINT('Ctrl Pts',(19.5088553757794,14.2147436659343,8.24093608349154));
#157978=CARTESIAN_POINT('Ctrl Pts',(19.5535545931509,14.4053393872225,7.46028346490425));
#157979=CARTESIAN_POINT('Ctrl Pts',(19.5857136184606,14.4285872270892,6.88812837299951));
#157980=CARTESIAN_POINT('Ctrl Pts',(19.6323168676482,14.2961534186914,6.05824455511635));
#157981=CARTESIAN_POINT('Ctrl Pts',(19.6474533909766,14.2272056986917,5.79305876366753));
#157982=CARTESIAN_POINT('Ctrl Pts',(19.6857684809327,13.9932393926121,5.15305688632271));
#157983=CARTESIAN_POINT('Ctrl Pts',(19.7088876903985,13.7988236342008,4.79188655028604));
#157984=CARTESIAN_POINT('Ctrl Pts',(19.7465531814489,13.3946263547052,4.24577739348952));
#157985=CARTESIAN_POINT('Ctrl Pts',(19.7615465917255,13.2127536149457,4.04359417204778));
#157986=CARTESIAN_POINT('Ctrl Pts',(19.798491640212,12.7280248607654,3.59846612441179));
#157987=CARTESIAN_POINT('Ctrl Pts',(19.8204785529977,12.408856941812,3.37683700633801));
#157988=CARTESIAN_POINT('Ctrl Pts',(19.8566610655473,11.8289531070741,3.08149027174962));
#157989=CARTESIAN_POINT('Ctrl Pts',(19.8712342531552,11.58309787199,2.98379394328921));
#157990=CARTESIAN_POINT('Ctrl Pts',(19.9082163625415,10.9497473469888,2.7979489841858));
#157991=CARTESIAN_POINT('Ctrl Pts',(19.9307842906331,10.5560084986188,2.73993671915285));
#157992=CARTESIAN_POINT('Ctrl Pts',(19.9695236866791,9.85941229810532,2.73496282863175));
#157993=CARTESIAN_POINT('Ctrl Pts',(19.9860035798403,9.55950248987418,2.76460233010767));
#157994=CARTESIAN_POINT('Ctrl Pts',(20.0229371076307,8.91280204416998,2.8984967389742));
#157995=CARTESIAN_POINT('Ctrl Pts',(20.0434322172209,8.57105887634374,3.01578895256602));
#157996=CARTESIAN_POINT('Ctrl Pts',(20.0769000040484,8.03479136220468,3.27953142000264));
#157997=CARTESIAN_POINT('Ctrl Pts',(20.0900163507226,7.83060149372497,3.40211734388238));
#157998=CARTESIAN_POINT('Ctrl Pts',(20.1338095512129,7.19270610888212,3.86165767663712));
#157999=CARTESIAN_POINT('Ctrl Pts',(20.1648930200309,6.81373218408336,4.26510658271138));
#158000=CARTESIAN_POINT('Ctrl Pts',(20.2103643554928,6.37698899278802,4.95903584802513));
#158001=CARTESIAN_POINT('Ctrl Pts',(20.2253878983731,6.25466168325506,5.20208544273264));
#158002=CARTESIAN_POINT('Ctrl Pts',(20.265076338985,5.99911605061139,5.85930905056656));
#158003=CARTESIAN_POINT('Ctrl Pts',(20.2897711795976,5.90453976302446,6.28515777739997));
#158004=CARTESIAN_POINT('Ctrl Pts',(20.3258939710697,5.86107099681106,6.94068417744711));
#158005=CARTESIAN_POINT('Ctrl Pts',(20.3380665169335,5.86381992540913,7.16424877544068));
#158006=CARTESIAN_POINT('Ctrl Pts',(20.371741745925,5.91913743472679,7.77176835866281));
#158007=CARTESIAN_POINT('Ctrl Pts',(20.3934865621156,6.00647306353156,8.15038990357501));
#158008=CARTESIAN_POINT('Ctrl Pts',(20.4455102960916,6.33112460849197,9.0062184383894));
#158009=CARTESIAN_POINT('Ctrl Pts',(20.4764801611693,6.60887478254657,9.46123463933842));
#158010=CARTESIAN_POINT('Ctrl Pts',(20.5119580174849,7.02483927015239,9.92281955521915));
#158011=CARTESIAN_POINT('Ctrl Pts',(20.5172006914584,7.08924585716699,9.98975731009913));
#158012=CARTESIAN_POINT('Ctrl Pts',(20.5267183602449,7.2124004403559,10.1096529137158));
#158013=CARTESIAN_POINT('Ctrl Pts',(20.5310107442253,7.27052964225416,10.1631789130787));
#158014=CARTESIAN_POINT('Ctrl Pts',(20.5484386539012,7.51696918442732,10.3777554714386));
#158015=CARTESIAN_POINT('Ctrl Pts',(20.5609307880345,7.71765784539843,10.523859312996));
#158016=CARTESIAN_POINT('Ctrl Pts',(20.5854393461132,8.12956102938122,10.7719668847095));
#158017=CARTESIAN_POINT('Ctrl Pts',(20.5974044794598,8.33871786847911,10.8756388895332));
#158018=CARTESIAN_POINT('Ctrl Pts',(20.6150536709055,8.64443499427547,10.9971180667588));
#158019=CARTESIAN_POINT('Ctrl Pts',(20.6202822909967,8.73474679395746,11.0295201389533));
#158020=CARTESIAN_POINT('Ctrl Pts',(20.6304484270141,8.90909128553992,11.0855079059924));
#158021=CARTESIAN_POINT('Ctrl Pts',(20.635366617745,8.99290606745967,11.1096137248184));
#158022=CARTESIAN_POINT('Ctrl Pts',(20.6478456224131,9.20384891131824,11.1633359546457));
#158023=CARTESIAN_POINT('Ctrl Pts',(20.6555008505231,9.3317021745655,11.1897147616175));
#158024=CARTESIAN_POINT('Ctrl Pts',(20.6767866376051,9.68298663275184,11.245529383248));
#158025=CARTESIAN_POINT('Ctrl Pts',(20.6907029872948,9.90784737756346,11.26318471361));
#158026=CARTESIAN_POINT('Ctrl Pts',(20.7046814563364,10.1330245361105,11.2629985430029));
#158027=CARTESIAN_POINT('Origin',(23.734,10.1295,7.));
#158028=CARTESIAN_POINT('',(22.6135314140065,10.129499907926,11.263));
#158029=CARTESIAN_POINT('',(22.2043183294109,10.1294634642048,11.2629999998434));
#158030=CARTESIAN_POINT('',(23.734,10.1295,11.263));
#158031=CARTESIAN_POINT('Ctrl Pts',(22.6135314140065,10.129499907926,11.263));
#158032=CARTESIAN_POINT('Ctrl Pts',(22.6114428647833,10.0924740380264,11.2629999992003));
#158033=CARTESIAN_POINT('Ctrl Pts',(22.609356796018,10.0554407197264,11.2625176221842));
#158034=CARTESIAN_POINT('Ctrl Pts',(22.5828597608454,9.58418469426959,11.2502328609711));
#158035=CARTESIAN_POINT('Ctrl Pts',(22.5592247311594,9.15423404753517,11.1726142704355));
#158036=CARTESIAN_POINT('Ctrl Pts',(22.5159780879935,8.4271237417952,10.9226239895735));
#158037=CARTESIAN_POINT('Ctrl Pts',(22.4969475017253,8.12468288507274,10.7770071894103));
#158038=CARTESIAN_POINT('Ctrl Pts',(22.4658536990385,7.65343574173953,10.4774133220202));
#158039=CARTESIAN_POINT('Ctrl Pts',(22.4535162590206,7.4742482739064,10.342594339537));
#158040=CARTESIAN_POINT('Ctrl Pts',(22.4257158867594,7.10019293920917,10.0120189258201));
#158041=CARTESIAN_POINT('Ctrl Pts',(22.4102301496065,6.91205649731029,9.81016156506494));
#158042=CARTESIAN_POINT('Ctrl Pts',(22.3707596858084,6.48790867091137,9.25619448374488));
#158043=CARTESIAN_POINT('Ctrl Pts',(22.3475308352618,6.28237905215565,8.88448259158381));
#158044=CARTESIAN_POINT('Ctrl Pts',(22.2991991321215,5.97940150598051,8.07147339738871));
#158045=CARTESIAN_POINT('Ctrl Pts',(22.2738562761949,5.8902452696974,7.63252148027423));
#158046=CARTESIAN_POINT('Ctrl Pts',(22.2344286972258,5.85912360595505,6.92661403257636));
#158047=CARTESIAN_POINT('Ctrl Pts',(22.2200564830558,5.87165432098166,6.66495841673331));
#158048=CARTESIAN_POINT('Ctrl Pts',(22.1818399371025,5.96714508365989,5.98621167170793));
#158049=CARTESIAN_POINT('Ctrl Pts',(22.1577019805083,6.08853236073664,5.57748960160242));
#158050=CARTESIAN_POINT('Ctrl Pts',(22.1204989350787,6.37080733470024,4.97416663593735));
#158051=CARTESIAN_POINT('Ctrl Pts',(22.1071797556236,6.49188676873379,4.76403391951975));
#158052=CARTESIAN_POINT('Ctrl Pts',(22.0671855771246,6.90231042658895,4.17413546742915));
#158053=CARTESIAN_POINT('Ctrl Pts',(22.040060765781,7.23814240904191,3.83135520777246));
#158054=CARTESIAN_POINT('Ctrl Pts',(21.9978279990004,7.85152801401269,3.3856746636728));
#158055=CARTESIAN_POINT('Ctrl Pts',(21.9823406925833,8.09524200760288,3.24309973310937));
#158056=CARTESIAN_POINT('Ctrl Pts',(21.9509679532618,8.60524270089143,3.00901993289245));
#158057=CARTESIAN_POINT('Ctrl Pts',(21.935159201254,8.87009885346302,2.91769874568505));
#158058=CARTESIAN_POINT('Ctrl Pts',(21.8880351083181,9.6816113240163,2.7244544592365));
#158059=CARTESIAN_POINT('Ctrl Pts',(21.8580076368599,10.2411734304136,2.70250958797326));
#158060=CARTESIAN_POINT('Ctrl Pts',(21.8117338739207,11.0510219152431,2.82936601039102));
#158061=CARTESIAN_POINT('Ctrl Pts',(21.7966910548133,11.3084374918958,2.89469785587851));
#158062=CARTESIAN_POINT('Ctrl Pts',(21.7658118326499,11.8304223071756,3.08036229437963));
#158063=CARTESIAN_POINT('Ctrl Pts',(21.749931542416,12.0921668051575,3.20465583637065));
#158064=CARTESIAN_POINT('Ctrl Pts',(21.7181459700998,12.5783576346297,3.49937142960535));
#158065=CARTESIAN_POINT('Ctrl Pts',(21.7023349255994,12.8025617882264,3.6674278171189));
#158066=CARTESIAN_POINT('Ctrl Pts',(21.6552251732102,13.4175836166178,4.23068582269741));
#158067=CARTESIAN_POINT('Ctrl Pts',(21.6252026270812,13.7495122674209,4.68135672108846));
#158068=CARTESIAN_POINT('Ctrl Pts',(21.5789375005714,14.0988020859468,5.42264915317206));
#158069=CARTESIAN_POINT('Ctrl Pts',(21.5638953347234,14.1891620494996,5.67239014673362));
#158070=CARTESIAN_POINT('Ctrl Pts',(21.5345432819917,14.3215256214276,6.1823040533484));
#158071=CARTESIAN_POINT('Ctrl Pts',(21.520151853032,14.3638210107639,6.44122196721935));
#158072=CARTESIAN_POINT('Ctrl Pts',(21.4828334512866,14.4105356040433,7.10871520996769));
#158073=CARTESIAN_POINT('Ctrl Pts',(21.4596547429648,14.3805895699774,7.5170209498503));
#158074=CARTESIAN_POINT('Ctrl Pts',(21.4235520815382,14.2420611454006,8.14749736915591));
#158075=CARTESIAN_POINT('Ctrl Pts',(21.4104286147913,14.1715322789947,8.37545902069937));
#158076=CARTESIAN_POINT('Ctrl Pts',(21.3655784812187,13.8699134766247,9.12232448644817));
#158077=CARTESIAN_POINT('Ctrl Pts',(21.3333941001527,13.5546316931928,9.60066090863966));
#158078=CARTESIAN_POINT('Ctrl Pts',(21.2868974827202,12.9628157617956,10.1968584796758));
#158079=CARTESIAN_POINT('Ctrl Pts',(21.2718286027191,12.7525036562347,10.3715618333134));
#158080=CARTESIAN_POINT('Ctrl Pts',(21.2355758124263,12.2187529997089,10.7345835549968));
#158081=CARTESIAN_POINT('Ctrl Pts',(21.2143759062964,11.8843871977691,10.9028804360248));
#158082=CARTESIAN_POINT('Ctrl Pts',(21.1804532628206,11.3089988116208,11.1034041201438));
#158083=CARTESIAN_POINT('Ctrl Pts',(21.167375361928,11.0794965174539,11.1625291571328));
#158084=CARTESIAN_POINT('Ctrl Pts',(21.1407216241085,10.609585791639,11.2426807155862));
#158085=CARTESIAN_POINT('Ctrl Pts',(21.127186528019,10.3699147472305,11.2629817564361));
#158086=CARTESIAN_POINT('Ctrl Pts',(21.1136182667127,10.1298237102038,11.2629999877096));
#158087=CARTESIAN_POINT('Ctrl Pts',(22.2043183294109,10.1294634642048,11.2629999998434));
#158088=CARTESIAN_POINT('Ctrl Pts',(22.1969189590874,9.99730152393924,11.2629988671572));
#158089=CARTESIAN_POINT('Ctrl Pts',(22.189519588764,9.86515952805542,11.2568474502169));
#158090=CARTESIAN_POINT('Ctrl Pts',(22.1821202184405,9.73360519517336,11.2445772820755));
#158091=CARTESIAN_POINT('Ctrl Pts',(22.174718676944,9.60201226073265,11.2323035135386));
#158092=CARTESIAN_POINT('Ctrl Pts',(22.1673171354475,9.4710076462198,11.2139074381013));
#158093=CARTESIAN_POINT('Ctrl Pts',(22.1599155939509,9.34115385194505,11.1894724430227));
#158094=CARTESIAN_POINT('Ctrl Pts',(22.1583218981377,9.31319380492495,11.184211113424));
#158095=CARTESIAN_POINT('Ctrl Pts',(22.1567282023245,9.2852870817884,11.1786699942204));
#158096=CARTESIAN_POINT('Ctrl Pts',(22.1551345065113,9.25743924154365,11.1728502289874));
#158097=CARTESIAN_POINT('Ctrl Pts',(22.1478859733478,9.13078019414404,11.1463804591948));
#158098=CARTESIAN_POINT('Ctrl Pts',(22.1406374401844,9.00530415852921,11.1141348765338));
#158099=CARTESIAN_POINT('Ctrl Pts',(22.1333889070209,8.88154079800544,11.0762442063936));
#158100=CARTESIAN_POINT('Ctrl Pts',(22.1261417954377,8.75780170991764,11.0383609673611));
#158101=CARTESIAN_POINT('Ctrl Pts',(22.1188946838546,8.63577495772857,10.9948349505913));
#158102=CARTESIAN_POINT('Ctrl Pts',(22.1116475722714,8.51597534149411,10.9458468262711));
#158103=CARTESIAN_POINT('Ctrl Pts',(22.1044001904397,8.39617125786865,10.8968568751578));
#158104=CARTESIAN_POINT('Ctrl Pts',(22.0971528086079,8.27859479795234,10.8424045371221));
#158105=CARTESIAN_POINT('Ctrl Pts',(22.0899054267761,8.16374135476003,10.7827188566776));
#158106=CARTESIAN_POINT('Ctrl Pts',(22.0826583545769,8.04889281849421,10.7230357262067));
#158107=CARTESIAN_POINT('Ctrl Pts',(22.0754112823778,7.93676737253154,10.6581198618939));
#158108=CARTESIAN_POINT('Ctrl Pts',(22.0681642101786,7.82783617158518,10.5882464548811));
#158109=CARTESIAN_POINT('Ctrl Pts',(22.0609155607501,7.71888126320527,10.5183578408465));
#158110=CARTESIAN_POINT('Ctrl Pts',(22.0536669113216,7.61312227946226,10.4435097165584));
#158111=CARTESIAN_POINT('Ctrl Pts',(22.0464182618931,7.51100202624902,10.3640210108532));
#158112=CARTESIAN_POINT('Ctrl Pts',(22.0438751284631,7.47517391338621,10.336133004021));
#158113=CARTESIAN_POINT('Ctrl Pts',(22.0413319950331,7.43979341525656,10.3076741642416));
#158114=CARTESIAN_POINT('Ctrl Pts',(22.0387888616031,7.40487871978231,10.2786594637725));
#158115=CARTESIAN_POINT('Ctrl Pts',(22.0315394209714,7.30535110199038,10.1959503357274));
#158116=CARTESIAN_POINT('Ctrl Pts',(22.0242899803397,7.20957401612299,10.1086907026288));
#158117=CARTESIAN_POINT('Ctrl Pts',(22.017040539708,7.11795438636582,10.0172441096141));
#158118=CARTESIAN_POINT('Ctrl Pts',(22.0097925532381,7.02635313454589,9.9258158598272));
#158119=CARTESIAN_POINT('Ctrl Pts',(22.0025445667682,6.93890792009219,9.83020256976117));
#158120=CARTESIAN_POINT('Ctrl Pts',(21.9952965802982,6.85598915380836,9.73080496188683));
#158121=CARTESIAN_POINT('Ctrl Pts',(21.9880483796479,6.77306793724778,9.63140441678055));
#158122=CARTESIAN_POINT('Ctrl Pts',(21.9808001789976,6.6946736606481,9.52821959371692));
#158123=CARTESIAN_POINT('Ctrl Pts',(21.9735519783473,6.62113693951177,9.4216848754125));
#158124=CARTESIAN_POINT('Ctrl Pts',(21.9663041219354,6.54760371085105,9.31515521675584));
#158125=CARTESIAN_POINT('Ctrl Pts',(21.9590562655236,6.47892777135026,9.20527626682615));
#158126=CARTESIAN_POINT('Ctrl Pts',(21.9518084091117,6.41539671901959,9.09251184422229));
#158127=CARTESIAN_POINT('Ctrl Pts',(21.9445590323089,6.35185233970934,8.97972376689994));
#158128=CARTESIAN_POINT('Ctrl Pts',(21.9373096555061,6.2934551725897,8.86404930972835));
#158129=CARTESIAN_POINT('Ctrl Pts',(21.9300602787033,6.24044729171342,8.74597767229963));
#158130=CARTESIAN_POINT('Ctrl Pts',(21.9275212580338,6.22188181928051,8.70462427930307));
#158131=CARTESIAN_POINT('Ctrl Pts',(21.9249822373644,6.20397701830358,8.66297703249349));
#158132=CARTESIAN_POINT('Ctrl Pts',(21.922443216695,6.18674190960378,8.62105756856911));
#158133=CARTESIAN_POINT('Ctrl Pts',(21.9151754459718,6.13740760526893,8.50106600792267));
#158134=CARTESIAN_POINT('Ctrl Pts',(21.9079076752487,6.09354713243275,8.37880167535367));
#158135=CARTESIAN_POINT('Ctrl Pts',(21.9006399045255,6.05534999136786,8.25477914676757));
#158136=CARTESIAN_POINT('Ctrl Pts',(21.8933734613687,6.01715982757829,8.13077927273893));
#158137=CARTESIAN_POINT('Ctrl Pts',(21.8861070182118,5.98463103242785,8.00502217048947));
#158138=CARTESIAN_POINT('Ctrl Pts',(21.878840575055,5.95790341045558,7.87803809376438));
#158139=CARTESIAN_POINT('Ctrl Pts',(21.871573922425,5.93117501799356,7.75105035640947));
#158140=CARTESIAN_POINT('Ctrl Pts',(21.8643072697949,5.91024820677359,7.6228359082289));
#158141=CARTESIAN_POINT('Ctrl Pts',(21.8570406171649,5.89521184619667,7.49393605918256));
#158142=CARTESIAN_POINT('Ctrl Pts',(21.8497743641547,5.8801763125242,7.36504329881022));
#158143=CARTESIAN_POINT('Ctrl Pts',(21.8425081111445,5.8710306198732,7.23546555319564));
#158144=CARTESIAN_POINT('Ctrl Pts',(21.8352418581342,5.86781184389181,7.10574998859196));
#158145=CARTESIAN_POINT('Ctrl Pts',(21.8279743223649,5.8645924996789,6.9760115244532));
#158146=CARTESIAN_POINT('Ctrl Pts',(21.8207067865956,5.86730217015556,6.84613553506541));
#158147=CARTESIAN_POINT('Ctrl Pts',(21.8134392508263,5.87592582273696,6.7166703006725));
#158148=CARTESIAN_POINT('Ctrl Pts',(21.8109920244798,5.878829699714,6.67307495520454));
#158149=CARTESIAN_POINT('Ctrl Pts',(21.8085447981333,5.88240372517832,6.62952616917805));
#158150=CARTESIAN_POINT('Ctrl Pts',(21.8060975717868,5.88664599746917,6.58604479323473));
#158151=CARTESIAN_POINT('Ctrl Pts',(21.7989003324876,5.89912242773205,6.45816701512477));
#158152=CARTESIAN_POINT('Ctrl Pts',(21.7917030931884,5.9173874845122,6.33082262933598));
#158153=CARTESIAN_POINT('Ctrl Pts',(21.7845058538891,5.94137144353383,6.20454529072198));
#158154=CARTESIAN_POINT('Ctrl Pts',(21.777310240048,5.96534998590645,6.07829647117027));
#158155=CARTESIAN_POINT('Ctrl Pts',(21.7701146262068,5.9950447885472,5.95311456770553));
#158156=CARTESIAN_POINT('Ctrl Pts',(21.7629190123656,6.03033483538351,5.82952404843386));
#158157=CARTESIAN_POINT('Ctrl Pts',(21.7557229447161,6.06562710786945,5.705925734636));
#158158=CARTESIAN_POINT('Ctrl Pts',(21.7485268770667,6.10651523595494,5.58391934900157));
#158159=CARTESIAN_POINT('Ctrl Pts',(21.7413308094172,6.15282797750728,5.46401542145645));
#158160=CARTESIAN_POINT('Ctrl Pts',(21.7341348236115,6.199140192326,5.34411285762736));
#158161=CARTESIAN_POINT('Ctrl Pts',(21.7269388378059,6.25087676563492,5.22631303483247));
#158162=CARTESIAN_POINT('Ctrl Pts',(21.7197428520002,6.3078179577087,5.11110737001062));
#158163=CARTESIAN_POINT('Ctrl Pts',(21.7125445442252,6.36477752331817,4.99586453112694));
#158164=CARTESIAN_POINT('Ctrl Pts',(21.7053462364502,6.42694490292231,4.88321784067244));
#158165=CARTESIAN_POINT('Ctrl Pts',(21.6981479286752,6.49405382499079,4.77363522561758));
#158166=CARTESIAN_POINT('Ctrl Pts',(21.6953492614097,6.52014544947959,4.73103003461787));
#158167=CARTESIAN_POINT('Ctrl Pts',(21.6925505941441,6.54698356415018,4.68888773294117));
#158168=CARTESIAN_POINT('Ctrl Pts',(21.6897519268785,6.57455071884714,4.64723468904552));
#158169=CARTESIAN_POINT('Ctrl Pts',(21.6823654767811,6.64730799692895,4.53730088807892));
#158170=CARTESIAN_POINT('Ctrl Pts',(21.6749790266836,6.72517120219222,4.43074005094906));
#158171=CARTESIAN_POINT('Ctrl Pts',(21.6675925765861,6.8078078071312,4.32801010933154));
#158172=CARTESIAN_POINT('Ctrl Pts',(21.6602070407686,6.89043418347741,4.22529288341958));
#158173=CARTESIAN_POINT('Ctrl Pts',(21.652821504951,6.97783258068516,4.12640585384117));
#158174=CARTESIAN_POINT('Ctrl Pts',(21.6454359691335,7.06962978046818,4.03177439543045));
#158175=CARTESIAN_POINT('Ctrl Pts',(21.6380510733541,7.16141902501109,3.93715113787961));
#158176=CARTESIAN_POINT('Ctrl Pts',(21.6306661775747,7.2576060910435,3.84678294446063));
#158177=CARTESIAN_POINT('Ctrl Pts',(21.6232812817953,7.3577801678109,3.76105909719711));
#158178=CARTESIAN_POINT('Ctrl Pts',(21.6158977417591,7.45793585429648,3.67535098739542));
#158179=CARTESIAN_POINT('Ctrl Pts',(21.6085142017228,7.56207684856391,3.59428572780241));
#158180=CARTESIAN_POINT('Ctrl Pts',(21.6011306616865,7.66975832511667,3.51821311783129));
#158181=CARTESIAN_POINT('Ctrl Pts',(21.5937483307954,7.77742216750874,3.4421529656818));
#158182=CARTESIAN_POINT('Ctrl Pts',(21.5863659999042,7.88862507567842,3.3710840148624));
#158183=CARTESIAN_POINT('Ctrl Pts',(21.5789836690131,8.0028919322252,3.30531366337072));
#158184=CARTESIAN_POINT('Ctrl Pts',(21.5771245399989,8.03166832162039,3.28875038944878));
#158185=CARTESIAN_POINT('Ctrl Pts',(21.5752654109847,8.06063888910807,3.27252294045707));
#158186=CARTESIAN_POINT('Ctrl Pts',(21.5734062819705,8.08979577177236,3.25663578296871));
#158187=CARTESIAN_POINT('Ctrl Pts',(21.5663766750943,8.20004171021903,3.19656438896128));
#158188=CARTESIAN_POINT('Ctrl Pts',(21.5593470682181,8.31298831198066,3.14134266250149));
#158189=CARTESIAN_POINT('Ctrl Pts',(21.5523174613419,8.42817722338396,3.0912060926972));
#158190=CARTESIAN_POINT('Ctrl Pts',(21.5452896275042,8.54333708133278,3.04108216855934));
#158191=CARTESIAN_POINT('Ctrl Pts',(21.5382617936664,8.6607377697407,2.99604099920424));
#158192=CARTESIAN_POINT('Ctrl Pts',(21.5312339598286,8.7798993723283,2.95627063890421));
#158193=CARTESIAN_POINT('Ctrl Pts',(21.5242047012697,8.89908513201198,2.9164922161378));
#158194=CARTESIAN_POINT('Ctrl Pts',(21.5171754427108,9.02003215567398,2.88198686387374));
#158195=CARTESIAN_POINT('Ctrl Pts',(21.5101461841518,9.14224366034339,2.85289330739999));
#158196=CARTESIAN_POINT('Ctrl Pts',(21.5031162567188,9.26446679413621,2.82379698250799));
#158197=CARTESIAN_POINT('Ctrl Pts',(21.4960863292857,9.38795427288864,2.80011356232756));
#158198=CARTESIAN_POINT('Ctrl Pts',(21.4890564018526,9.5121981594764,2.78193084010158));
#158199=CARTESIAN_POINT('Ctrl Pts',(21.4820218975376,9.63652293588892,2.76373627989101));
#158200=CARTESIAN_POINT('Ctrl Pts',(21.4749873932226,9.76160472207926,2.75104962078328));
#158201=CARTESIAN_POINT('Ctrl Pts',(21.4679528889076,9.88692926940032,2.74390690413657));
#158202=CARTESIAN_POINT('Ctrl Pts',(21.4643221382925,9.95161359638359,2.74022030139992));
#158203=CARTESIAN_POINT('Ctrl Pts',(21.4606913876774,10.0163625427089,2.73800972683479));
#158204=CARTESIAN_POINT('Ctrl Pts',(21.4570606370622,10.0811053611285,2.737274702854));
#158205=CARTESIAN_POINT('Ctrl Pts',(21.4494491623812,10.216831654508,2.73573380483792));
#158206=CARTESIAN_POINT('Ctrl Pts',(21.4418376877003,10.3526182676046,2.74067973952619));
#158207=CARTESIAN_POINT('Ctrl Pts',(21.4342262130193,10.4878649307102,2.75208950465796));
#158208=CARTESIAN_POINT('Ctrl Pts',(21.4264336112805,10.6263300017054,2.76377078316592));
#158209=CARTESIAN_POINT('Ctrl Pts',(21.4186410095417,10.764228814435,2.78222738393882));
#158210=CARTESIAN_POINT('Ctrl Pts',(21.410848407803,10.9009217006177,2.80737819976378));
#158211=CARTESIAN_POINT('Ctrl Pts',(21.4032429171247,11.0343324030374,2.83192510998959));
#158212=CARTESIAN_POINT('Ctrl Pts',(21.3956374264465,11.1665941568544,2.86284837110384));
#158213=CARTESIAN_POINT('Ctrl Pts',(21.3880319357682,11.2971204731094,2.90002055727401));
#158214=CARTESIAN_POINT('Ctrl Pts',(21.3801457784992,11.4324636220633,2.93856451434043));
#158215=CARTESIAN_POINT('Ctrl Pts',(21.3722596212301,11.5659405054026,2.98382740162559));
#158216=CARTESIAN_POINT('Ctrl Pts',(21.3643734639611,11.6969110187463,3.03560954265189));
#158217=CARTESIAN_POINT('Ctrl Pts',(21.3564873066921,11.8278815320899,3.08739168367819));
#158218=CARTESIAN_POINT('Ctrl Pts',(21.3486011494231,11.956345363596,3.14569299962129));
#158219=CARTESIAN_POINT('Ctrl Pts',(21.340714992154,12.0816810369674,3.21025618294525));
#158220=CARTESIAN_POINT('Ctrl Pts',(21.3336759604758,12.1935532384943,3.26788403351437));
#158221=CARTESIAN_POINT('Ctrl Pts',(21.3266369287976,12.3028932792345,3.33048051016728));
#158222=CARTESIAN_POINT('Ctrl Pts',(21.3195978971194,12.40925055225,3.39779145252306));
#158223=CARTESIAN_POINT('Ctrl Pts',(21.3125590744663,12.5156046669697,3.46510039606998));
#158224=CARTESIAN_POINT('Ctrl Pts',(21.3055202518132,12.6189758680056,3.53712332086819));
#158225=CARTESIAN_POINT('Ctrl Pts',(21.2984814291601,12.7189414344944,3.61356203994173));
#158226=CARTESIAN_POINT('Ctrl Pts',(21.2914389136867,12.8189594465259,3.69004086152499));
#158227=CARTESIAN_POINT('Ctrl Pts',(21.2843963982133,12.9155679496317,3.77093987410838));
#158228=CARTESIAN_POINT('Ctrl Pts',(21.2773538827399,13.0083761165701,3.85591964074671));
#158229=CARTESIAN_POINT('Ctrl Pts',(21.2703094098651,13.1012100786724,3.94092302671816));
#158230=CARTESIAN_POINT('Ctrl Pts',(21.2632649369902,13.1902413235328,4.03000916216276));
#158231=CARTESIAN_POINT('Ctrl Pts',(21.2562204641154,13.2751155328051,4.12280137637754));
#158232=CARTESIAN_POINT('Ctrl Pts',(21.2491695588495,13.3600672417159,4.21567832025411));
#158233=CARTESIAN_POINT('Ctrl Pts',(21.2421186535837,13.4408540813723,4.31226781405213));
#158234=CARTESIAN_POINT('Ctrl Pts',(21.2350677483178,13.5171614727389,4.41215944345081));
#158235=CARTESIAN_POINT('Ctrl Pts',(21.2315016146271,13.5557554332217,4.46268159508693));
#158236=CARTESIAN_POINT('Ctrl Pts',(21.2279354809365,13.5932042061302,4.51404795176234));
#158237=CARTESIAN_POINT('Ctrl Pts',(21.2243693472458,13.6294713302574,4.56620261990112));
#158238=CARTESIAN_POINT('Ctrl Pts',(21.2173459273525,13.7008986134619,4.66892006279847));
#158239=CARTESIAN_POINT('Ctrl Pts',(21.2103225074592,13.7678679518273,4.77488136034603));
#158240=CARTESIAN_POINT('Ctrl Pts',(21.2032990875659,13.8300824556287,4.88366862493296));
#158241=CARTESIAN_POINT('Ctrl Pts',(21.1962814937663,13.8922453510204,4.99236564789809));
#158242=CARTESIAN_POINT('Ctrl Pts',(21.1892638999668,13.9496610740247,5.10388363594717));
#158243=CARTESIAN_POINT('Ctrl Pts',(21.1822463061672,14.0020763560252,5.21777628599693));
#158244=CARTESIAN_POINT('Ctrl Pts',(21.1752329695233,14.0544598407996,5.33159984416752));
#158245=CARTESIAN_POINT('Ctrl Pts',(21.1682196328795,14.1018487643949,5.44779484503741));
#158246=CARTESIAN_POINT('Ctrl Pts',(21.1612062962356,14.1440362326073,5.5658912743158));
#158247=CARTESIAN_POINT('Ctrl Pts',(21.1541426196187,14.1865265118952,5.68483537017137));
#158248=CARTESIAN_POINT('Ctrl Pts',(21.1470789430017,14.223740187332,5.80570794539113));
#158249=CARTESIAN_POINT('Ctrl Pts',(21.1400152663848,14.2555155490246,5.92800900693764));
#158250=CARTESIAN_POINT('Ctrl Pts',(21.1330043158592,14.2870537267815,6.04939716472518));
#158251=CARTESIAN_POINT('Ctrl Pts',(21.1259933653335,14.3132344332075,6.17219216889758));
#158252=CARTESIAN_POINT('Ctrl Pts',(21.1189824148079,14.3339500177816,6.29589130954337));
#158253=CARTESIAN_POINT('Ctrl Pts',(21.1119707905225,14.3546675931453,6.41960233780791));
#158254=CARTESIAN_POINT('Ctrl Pts',(21.104959166237,14.3699189367607,6.54421729408242));
#158255=CARTESIAN_POINT('Ctrl Pts',(21.0979475419516,14.3796478851492,6.66922522109208));
#158256=CARTESIAN_POINT('Ctrl Pts',(21.0909338264986,14.3893797351281,6.79427043083558));
#158257=CARTESIAN_POINT('Ctrl Pts',(21.0839201110456,14.3935858804475,6.91970845912758));
#158258=CARTESIAN_POINT('Ctrl Pts',(21.0769063955927,14.3922622147059,7.04502555802502));
#158259=CARTESIAN_POINT('Ctrl Pts',(21.069804034079,14.3909218192076,7.17192653457186));
#158260=CARTESIAN_POINT('Ctrl Pts',(21.0627016725654,14.3839108701113,7.29870309586766));
#158261=CARTESIAN_POINT('Ctrl Pts',(21.0555993110518,14.37127938786,7.42482540499111));
#158262=CARTESIAN_POINT('Ctrl Pts',(21.0485733953341,14.358783863728,7.54959020502676));
#158263=CARTESIAN_POINT('Ctrl Pts',(21.0415474796164,14.3407883237577,7.67371439178308));
#158264=CARTESIAN_POINT('Ctrl Pts',(21.0345215638987,14.3173929110686,7.79669439901484));
#158265=CARTESIAN_POINT('Ctrl Pts',(21.0273809794871,14.2936156660999,7.92168154059925));
#158266=CARTESIAN_POINT('Ctrl Pts',(21.0202403950756,14.264260841247,8.04548642037499));
#158267=CARTESIAN_POINT('Ctrl Pts',(21.013099810664,14.2294863484673,8.16759622403539));
#158268=CARTESIAN_POINT('Ctrl Pts',(21.0059592262525,14.1947118556876,8.28970602769578));
#158269=CARTESIAN_POINT('Ctrl Pts',(20.9988186418409,14.1545178775712,8.41012037987649));
#158270=CARTESIAN_POINT('Ctrl Pts',(20.9916780574294,14.1091131539846,8.52834817519842));
#158271=CARTESIAN_POINT('Ctrl Pts',(20.9848875792511,14.0659346454851,8.64077920575989));
#158272=CARTESIAN_POINT('Ctrl Pts',(20.9780971010728,14.0179001275206,8.75160660314064));
#158273=CARTESIAN_POINT('Ctrl Pts',(20.9713066228945,13.9651477064359,8.86036976757665));
#158274=CARTESIAN_POINT('Ctrl Pts',(20.9645253559579,13.9124668436842,8.96898539545253));
#158275=CARTESIAN_POINT('Ctrl Pts',(20.9577440890213,13.8550809778343,9.07554198259683));
#158276=CARTESIAN_POINT('Ctrl Pts',(20.9509628220846,13.793177528671,9.17959536747338));
#158277=CARTESIAN_POINT('Ctrl Pts',(20.9441888767195,13.7313409151793,9.28353640840212));
#158278=CARTESIAN_POINT('Ctrl Pts',(20.9374149313544,13.6649966269885,9.38497926183249));
#158279=CARTESIAN_POINT('Ctrl Pts',(20.9306409859893,13.5943792727532,9.48350168617723));
#158280=CARTESIAN_POINT('Ctrl Pts',(20.9238724821202,13.5238186452894,9.58194496766671));
#158281=CARTESIAN_POINT('Ctrl Pts',(20.9171039782511,13.4489920202032,9.67747214528359));
#158282=CARTESIAN_POINT('Ctrl Pts',(20.910335474382,13.370178451617,9.76968810035086));
#158283=CARTESIAN_POINT('Ctrl Pts',(20.903569799622,13.2913978256411,9.8618655108588));
#158284=CARTESIAN_POINT('Ctrl Pts',(20.896804124862,13.2086338378673,9.95073412927473));
#158285=CARTESIAN_POINT('Ctrl Pts',(20.890038450102,13.1222067694605,10.0359306961828));
#158286=CARTESIAN_POINT('Ctrl Pts',(20.8832740089491,13.035795459577,10.1211117289289));
#158287=CARTESIAN_POINT('Ctrl Pts',(20.8765095677961,12.9457226947661,10.2026217459866));
#158288=CARTESIAN_POINT('Ctrl Pts',(20.8697451266432,12.8523461041995,10.2801338528855));
#158289=CARTESIAN_POINT('Ctrl Pts',(20.8629802282965,12.7589632025141,10.3576511986577));
#158290=CARTESIAN_POINT('Ctrl Pts',(20.8562153299499,12.6622763543278,10.4311698294127));
#158291=CARTESIAN_POINT('Ctrl Pts',(20.8494504316032,12.5626761707932,10.5004032227565));
#158292=CARTESIAN_POINT('Ctrl Pts',(20.8426833849945,12.4630443582094,10.5696586018671));
#158293=CARTESIAN_POINT('Ctrl Pts',(20.8359163383857,12.3604977161624,10.6346258000381));
#158294=CARTESIAN_POINT('Ctrl Pts',(20.8291492917769,12.2554550341066,10.6950621365488));
#158295=CARTESIAN_POINT('Ctrl Pts',(20.8223742557459,12.1502883348272,10.7555698264038));
#158296=CARTESIAN_POINT('Ctrl Pts',(20.815599219715,12.0426200781834,10.8115357695555));
#158297=CARTESIAN_POINT('Ctrl Pts',(20.808824183684,11.9328928762342,10.8627636652982));
#158298=CARTESIAN_POINT('Ctrl Pts',(20.8020445915196,11.8230918840095,10.9140260112088));
#158299=CARTESIAN_POINT('Ctrl Pts',(20.7952649993552,11.7112295779413,10.9605438102634));
#158300=CARTESIAN_POINT('Ctrl Pts',(20.7884854071908,11.5977659401151,11.002169927564));
#158301=CARTESIAN_POINT('Ctrl Pts',(20.7816949968921,11.4841212493811,11.0438624672861));
#158302=CARTESIAN_POINT('Ctrl Pts',(20.7749045865934,11.3688705257193,11.0806476224473));
#158303=CARTESIAN_POINT('Ctrl Pts',(20.7681141762946,11.2524863546908,11.1124288014722));
#158304=CARTESIAN_POINT('Ctrl Pts',(20.7650717067341,11.2003399773581,11.1266684814808));
#158305=CARTESIAN_POINT('Ctrl Pts',(20.7620292371736,11.1479661589978,11.1399042936374));
#158306=CARTESIAN_POINT('Ctrl Pts',(20.7589867676131,11.0954077443162,11.1521309263401));
#158307=CARTESIAN_POINT('Ctrl Pts',(20.7486384526106,10.9166414426865,11.193717224612));
#158308=CARTESIAN_POINT('Ctrl Pts',(20.7382901376082,10.7352286283145,11.223745455636));
#158309=CARTESIAN_POINT('Ctrl Pts',(20.7279418226057,10.5523855434177,11.2419732221183));
#158310=CARTESIAN_POINT('Ctrl Pts',(20.7200673248741,10.4132520268103,11.2558435484257));
#158311=CARTESIAN_POINT('Ctrl Pts',(20.7121928271425,10.2732902767665,11.2628818332749));
#158312=CARTESIAN_POINT('Ctrl Pts',(20.7043183294109,10.1330470789259,11.2629985243055));
#158313=CARTESIAN_POINT('Origin',(-23.734,10.1295,7.));
#158314=CARTESIAN_POINT('',(-22.2043183294109,10.1295365081804,11.2629999998437));
#158315=CARTESIAN_POINT('',(-22.6135314280912,10.1295000920819,11.263));
#158316=CARTESIAN_POINT('',(-23.734,10.1295,11.263));
#158317=CARTESIAN_POINT('',(-23.533999981871,12.9193850840203,10.2235360174615));
#158318=CARTESIAN_POINT('Ctrl Pts',(-23.533999981871,12.9193850840203,10.2235360174615));
#158319=CARTESIAN_POINT('Ctrl Pts',(-23.5009788547478,13.3648360859832,
9.83730561563166));
#158320=CARTESIAN_POINT('Ctrl Pts',(-23.4291758459887,14.1588395586771,
8.79502344007021));
#158321=CARTESIAN_POINT('Ctrl Pts',(-23.3185909555933,14.5604905826756,
6.80076298861617));
#158322=CARTESIAN_POINT('Ctrl Pts',(-23.2022453106852,13.9513208636606,
4.74899583476332));
#158323=CARTESIAN_POINT('Ctrl Pts',(-23.0858996657769,12.452270995998,3.22136570469558));
#158324=CARTESIAN_POINT('Ctrl Pts',(-22.9695540208687,10.4123750626855,
2.57356516157568));
#158325=CARTESIAN_POINT('Ctrl Pts',(-22.8532083759605,8.30661439543301,
2.9564333045403));
#158326=CARTESIAN_POINT('Ctrl Pts',(-22.7368627310523,6.62530205950465,
4.28082127060911));
#158327=CARTESIAN_POINT('Ctrl Pts',(-22.6205170861441,5.75991783379543,
6.23835174036327));
#158328=CARTESIAN_POINT('Ctrl Pts',(-22.5041714412359,5.9119701463398,8.37323075593554));
#158329=CARTESIAN_POINT('Ctrl Pts',(-22.3878257963277,7.04603468702391,
10.1883540588533));
#158330=CARTESIAN_POINT('Ctrl Pts',(-22.2878747590527,8.63711446750853,
11.1099400088585));
#158331=CARTESIAN_POINT('Ctrl Pts',(-22.2267056034138,9.72970022779226,
11.2625492465514));
#158332=CARTESIAN_POINT('Ctrl Pts',(-22.2043183294109,10.1295365056039,
11.2626991438894));
#158333=CARTESIAN_POINT('',(-23.534,12.9193325810254,3.77664721604209));
#158334=CARTESIAN_POINT('Origin',(-23.534,10.1295,7.));
#158335=CARTESIAN_POINT('Ctrl Pts',(-23.534,12.9193325810254,3.77664721604209));
#158336=CARTESIAN_POINT('Ctrl Pts',(-23.5168586580598,12.6878910637622,
3.57633309322055));
#158337=CARTESIAN_POINT('Ctrl Pts',(-23.5000542450407,12.4355456847612,
3.40152546405373));
#158338=CARTESIAN_POINT('Ctrl Pts',(-23.4666881757483,11.9114783876185,
3.11643078784149));
#158339=CARTESIAN_POINT('Ctrl Pts',(-23.4502450241458,11.6427807725919,
3.0040609018805));
#158340=CARTESIAN_POINT('Ctrl Pts',(-23.4112911491467,10.984032226903,2.80462331559761));
#158341=CARTESIAN_POINT('Ctrl Pts',(-23.3895178715562,10.5890392288408,
2.74321227034389));
#158342=CARTESIAN_POINT('Ctrl Pts',(-23.3521339750897,9.91912682473691,
2.73350346552896));
#158343=CARTESIAN_POINT('Ctrl Pts',(-23.3367839960271,9.64723138241095,
2.75563212128445));
#158344=CARTESIAN_POINT('Ctrl Pts',(-23.2981650012946,8.97514813831931,
2.87577736451175));
#158345=CARTESIAN_POINT('Ctrl Pts',(-23.275645081719,8.58352778228038,3.00603949148055));
#158346=CARTESIAN_POINT('Ctrl Pts',(-23.2375083553902,7.972206472833,3.31299050935889));
#158347=CARTESIAN_POINT('Ctrl Pts',(-23.2221028377029,7.74019526512778,
3.45893107422773));
#158348=CARTESIAN_POINT('Ctrl Pts',(-23.1745609982425,7.07494413186754,
3.97271405519828));
#158349=CARTESIAN_POINT('Ctrl Pts',(-23.1438258283781,6.6997624203252,4.40545139686439));
#158350=CARTESIAN_POINT('Ctrl Pts',(-23.0985113983711,6.30345136697088,
5.1050910847094));
#158351=CARTESIAN_POINT('Ctrl Pts',(-23.08505282655,6.20404911848136,5.32066599727039));
#158352=CARTESIAN_POINT('Ctrl Pts',(-23.048506070219,5.9817503616778,5.93209744180422));
#158353=CARTESIAN_POINT('Ctrl Pts',(-23.0259779563819,5.89774520043703,
6.33931806570632));
#158354=CARTESIAN_POINT('Ctrl Pts',(-22.9878332334974,5.85828446543936,
7.01713139920122));
#158355=CARTESIAN_POINT('Ctrl Pts',(-22.9727696608249,5.86762836053496,
7.28288238713844));
#158356=CARTESIAN_POINT('Ctrl Pts',(-22.9429381658152,5.93554297343332,
7.80873923758166));
#158357=CARTESIAN_POINT('Ctrl Pts',(-22.9283693246464,5.99388207497819,
8.06770856547383));
#158358=CARTESIAN_POINT('Ctrl Pts',(-22.8916881242178,6.19827579788421,
8.69558095527337));
#158359=CARTESIAN_POINT('Ctrl Pts',(-22.8693946085137,6.3723902759301,9.05271068927232));
#158360=CARTESIAN_POINT('Ctrl Pts',(-22.8320450352526,6.74201792090859,
9.60175977677851));
#158361=CARTESIAN_POINT('Ctrl Pts',(-22.8173301696315,6.91124320118273,
9.80838308598632));
#158362=CARTESIAN_POINT('Ctrl Pts',(-22.7769127817254,7.42355106280853,
10.3263283873352));
#158363=CARTESIAN_POINT('Ctrl Pts',(-22.7508487154543,7.79969368267197,
10.599803533184));
#158364=CARTESIAN_POINT('Ctrl Pts',(-22.6994967655324,8.61502871430095,
11.010342875459));
#158365=CARTESIAN_POINT('Ctrl Pts',(-22.6749853207843,9.04737808066313,
11.1479500333799));
#158366=CARTESIAN_POINT('Ctrl Pts',(-22.6376180791365,9.70387868628257,
11.2470462297682));
#158367=CARTESIAN_POINT('Ctrl Pts',(-22.625542538647,9.91656672784588,11.2630000045994));
#158368=CARTESIAN_POINT('Ctrl Pts',(-22.6135314280911,10.1295000920819,
11.263));
#158369=CARTESIAN_POINT('Origin',(-23.734,10.1295,7.));
#158370=CARTESIAN_POINT('',(-20.7043183294109,10.1259540174844,11.2629985252177));
#158371=CARTESIAN_POINT('',(-21.113681670589,10.1291791134783,11.262999987923));
#158372=CARTESIAN_POINT('',(-23.734,10.1295,11.263));
#158373=CARTESIAN_POINT('Ctrl Pts',(-22.2043183294109,10.1295365081804,
11.2629999998437));
#158374=CARTESIAN_POINT('Ctrl Pts',(-22.1969189537551,10.2616985400649,
11.2629988680127));
#158375=CARTESIAN_POINT('Ctrl Pts',(-22.1895195780993,10.3938406290833,
11.2568474434062));
#158376=CARTESIAN_POINT('Ctrl Pts',(-22.1821202024435,10.5253950557853,
11.2445772586684));
#158377=CARTESIAN_POINT('Ctrl Pts',(-22.1747186558373,10.6569880800865,
11.2323034739021));
#158378=CARTESIAN_POINT('Ctrl Pts',(-22.1673171092311,10.7879927851824,
11.2139073736701));
#158379=CARTESIAN_POINT('Ctrl Pts',(-22.159915562625,10.917846669891,11.1894723448272));
#158380=CARTESIAN_POINT('Ctrl Pts',(-22.1583218772537,10.9458065338851,
11.184211046063));
#158381=CARTESIAN_POINT('Ctrl Pts',(-22.1567281918825,10.9737130747608,
11.1786699613311));
#158382=CARTESIAN_POINT('Ctrl Pts',(-22.1551345065113,11.0015607336212,
11.1728502341776));
#158383=CARTESIAN_POINT('Ctrl Pts',(-22.1478859815791,11.1282196420853,
11.146380494207));
#158384=CARTESIAN_POINT('Ctrl Pts',(-22.1406374566469,11.2536955421307,
11.1141349538837));
#158385=CARTESIAN_POINT('Ctrl Pts',(-22.1333889317147,11.3774587715464,
11.076244338177));
#158386=CARTESIAN_POINT('Ctrl Pts',(-22.1261418283556,11.5011977286471,
11.0383611535383));
#158387=CARTESIAN_POINT('Ctrl Pts',(-22.1188947249966,11.6232243543046,
10.9948352032451));
#158388=CARTESIAN_POINT('Ctrl Pts',(-22.1116476216375,11.7430238495479,
10.9458471570678));
#158389=CARTESIAN_POINT('Ctrl Pts',(-22.1044002479377,11.8628278137052,
10.8968572834758));
#158390=CARTESIAN_POINT('Ctrl Pts',(-22.0971528742379,11.980404159636,10.8424050344898));
#158391=CARTESIAN_POINT('Ctrl Pts',(-22.0899055005381,12.0952574954049,
10.7827194542101));
#158392=CARTESIAN_POINT('Ctrl Pts',(-22.0826584363958,12.2101059254377,
10.7230364232835));
#158393=CARTESIAN_POINT('Ctrl Pts',(-22.0754113722534,12.3222312716713,
10.6581206695218));
#158394=CARTESIAN_POINT('Ctrl Pts',(-22.068164308111,12.4311623804912,10.5882473836445));
#158395=CARTESIAN_POINT('Ctrl Pts',(-22.0609156665626,12.5401171994071,
10.518358889051));
#158396=CARTESIAN_POINT('Ctrl Pts',(-22.0536670250143,12.6458761011336,
10.44351089455));
#158397=CARTESIAN_POINT('Ctrl Pts',(-22.0464183834659,12.7479962808951,
10.3640223285434));
#158398=CARTESIAN_POINT('Ctrl Pts',(-22.0438752095116,12.7838249778501,
10.3361338960173));
#158399=CARTESIAN_POINT('Ctrl Pts',(-22.0413320355574,12.8192060458866,
10.3076746123286));
#158400=CARTESIAN_POINT('Ctrl Pts',(-22.0387888616031,12.8541212962082,
10.2786594504841));
#158401=CARTESIAN_POINT('Ctrl Pts',(-22.031539428324,12.9536488087519,10.1959504090815));
#158402=CARTESIAN_POINT('Ctrl Pts',(-22.0242899950448,13.0494257988114,
10.1086908709218));
#158403=CARTESIAN_POINT('Ctrl Pts',(-22.0170405617656,13.1410453426988,
10.0172443800378));
#158404=CARTESIAN_POINT('Ctrl Pts',(-22.0097925827507,13.2326465073522,
9.92581623367245));
#158405=CARTESIAN_POINT('Ctrl Pts',(-22.0025446037358,13.3200916446912,
9.83020305433749));
#158406=CARTESIAN_POINT('Ctrl Pts',(-21.995296624721,13.403010344373,9.73080556343414));
#158407=CARTESIAN_POINT('Ctrl Pts',(-21.9880484316003,13.4859314934781,
9.63140513632307));
#158408=CARTESIAN_POINT('Ctrl Pts',(-21.9808002384797,13.5643257132272,
9.52822043757356));
#158409=CARTESIAN_POINT('Ctrl Pts',(-21.9735520453591,13.6378623885564,
9.42168584885883));
#158410=CARTESIAN_POINT('Ctrl Pts',(-21.9663041964995,13.7113955711792,
9.31515632012311));
#158411=CARTESIAN_POINT('Ctrl Pts',(-21.9590563476399,13.7800714757143,
9.20527750541175));
#158412=CARTESIAN_POINT('Ctrl Pts',(-21.9518084987802,13.8436025045761,
9.09251322230027));
#158413=CARTESIAN_POINT('Ctrl Pts',(-21.944559129499,13.9071468606959,8.97972528399669));
#158414=CARTESIAN_POINT('Ctrl Pts',(-21.9373097602177,13.9655440160801,
8.86405097009525));
#158415=CARTESIAN_POINT('Ctrl Pts',(-21.9300603909365,14.0185518970943,
8.74597947917691));
#158416=CARTESIAN_POINT('Ctrl Pts',(-21.927521332856,14.0371176623904,8.70462548526887));
#158417=CARTESIAN_POINT('Ctrl Pts',(-21.9249822747754,14.0550227368446,
8.66297762867509));
#158418=CARTESIAN_POINT('Ctrl Pts',(-21.9224432166949,14.072258099233,8.62105754707614));
#158419=CARTESIAN_POINT('Ctrl Pts',(-21.9151753922206,14.1215927676882,
8.50106509895149));
#158420=CARTESIAN_POINT('Ctrl Pts',(-21.9079075677462,14.1654535201482,
8.37879985409838));
#158421=CARTESIAN_POINT('Ctrl Pts',(-21.9006397432719,14.2036508556539,
8.25477639656434));
#158422=CARTESIAN_POINT('Ctrl Pts',(-21.8933732460253,14.2418412156796,
8.13077558781263));
#158423=CARTESIAN_POINT('Ctrl Pts',(-21.8861067487787,14.2743701213767,
8.0050175340044));
#158424=CARTESIAN_POINT('Ctrl Pts',(-21.8788402515321,14.3010977675838,
7.87803249683022));
#158425=CARTESIAN_POINT('Ctrl Pts',(-21.8715735448853,14.3278261840071,
7.75104380030113));
#158426=CARTESIAN_POINT('Ctrl Pts',(-21.8643068382385,14.3487529329938,
7.6228283840705));
#158427=CARTESIAN_POINT('Ctrl Pts',(-21.8570401315917,14.3637891445478,
7.49392756590881));
#158428=CARTESIAN_POINT('Ctrl Pts',(-21.8497738247676,14.3788245287919,
7.36503384002021));
#158429=CARTESIAN_POINT('Ctrl Pts',(-21.8425075179435,14.3879699855593,
7.23545512785121));
#158430=CARTESIAN_POINT('Ctrl Pts',(-21.8352412111193,14.3911884386049,
7.10573860345731));
#158431=CARTESIAN_POINT('Ctrl Pts',(-21.8279736222961,14.3944074594842,
6.97599919309588));
#158432=CARTESIAN_POINT('Ctrl Pts',(-21.8207060334729,14.3916973798453,
6.84612226427044));
#158433=CARTESIAN_POINT('Ctrl Pts',(-21.8134384446498,14.3830732316722,
6.71665610505596));
#158434=CARTESIAN_POINT('Ctrl Pts',(-21.8109914870288,14.3801695278977,
6.67306555354588));
#158435=CARTESIAN_POINT('Ctrl Pts',(-21.8085445294078,14.3765958228007,
6.62952155223097));
#158436=CARTESIAN_POINT('Ctrl Pts',(-21.8060975717868,14.3723540173125,
6.58604494473972));
#158437=CARTESIAN_POINT('Ctrl Pts',(-21.7989004737786,14.35987783482,6.45816965891825));
#158438=CARTESIAN_POINT('Ctrl Pts',(-21.7917033757704,14.3416132490332,
6.33082772123226));
#158439=CARTESIAN_POINT('Ctrl Pts',(-21.7845062777622,14.3176299764922,
6.20455276730157));
#158440=CARTESIAN_POINT('Ctrl Pts',(-21.7773108057981,14.2936521225045,
6.07830634273716));
#158441=CARTESIAN_POINT('Ctrl Pts',(-21.770115333834,14.2639582246201,5.95312677071234));
#158442=CARTESIAN_POINT('Ctrl Pts',(-21.7629198618699,14.2286692912606,
5.82953850059646));
#158443=CARTESIAN_POINT('Ctrl Pts',(-21.7557239357197,14.1933781304247,
5.70594242945247));
#158444=CARTESIAN_POINT('Ctrl Pts',(-21.7485280095695,14.1524913221394,
5.5839382043744));
#158445=CARTESIAN_POINT('Ctrl Pts',(-21.7413320834193,14.1061801009768,
5.46403633685718));
#158446=CARTESIAN_POINT('Ctrl Pts',(-21.7341362386062,14.0598694032798,
5.34413582461646));
#158447=CARTESIAN_POINT('Ctrl Pts',(-21.7269403937931,14.0081345469274,
5.22633795320274));
#158448=CARTESIAN_POINT('Ctrl Pts',(-21.7197445489799,13.951195264075,5.11113412108044));
#158449=CARTESIAN_POINT('Ctrl Pts',(-21.7125463803664,13.8942375934544,
4.9958930854447));
#158450=CARTESIAN_POINT('Ctrl Pts',(-21.7053482117529,13.8320722985288,
4.8832480808549));
#158451=CARTESIAN_POINT('Ctrl Pts',(-21.6981500431394,13.7649656431987,
4.77366701566866));
#158452=CARTESIAN_POINT('Ctrl Pts',(-21.6953506710525,13.7388678247307,
4.73105087375697));
#158453=CARTESIAN_POINT('Ctrl Pts',(-21.6925512989656,13.7120231386475,
4.68889785170956));
#158454=CARTESIAN_POINT('Ctrl Pts',(-21.6897519268786,13.6844490489701,
4.64723433822518));
#158455=CARTESIAN_POINT('Ctrl Pts',(-21.6823651612314,13.6116886826953,
4.53729589467605));
#158456=CARTESIAN_POINT('Ctrl Pts',(-21.6749783955841,13.5338219832499,
4.43073073882055));
#158457=CARTESIAN_POINT('Ctrl Pts',(-21.6675916299368,13.4511815146991,
4.32799683478733));
#158458=CARTESIAN_POINT('Ctrl Pts',(-21.6602057767909,13.3685512548839,
4.2252756216705));
#158459=CARTESIAN_POINT('Ctrl Pts',(-21.652819923645,13.281148602485,4.12638496293451));
#158460=CARTESIAN_POINT('Ctrl Pts',(-21.645434070499,13.1893468117984,4.03175026516851));
#158461=CARTESIAN_POINT('Ctrl Pts',(-21.6380488592528,13.0975529995455,
3.93712379204228));
#158462=CARTESIAN_POINT('Ctrl Pts',(-21.6306636480065,13.0013610322878,
3.84675277061771));
#158463=CARTESIAN_POINT('Ctrl Pts',(-21.6232784367602,12.9011817562969,
3.76102651418525));
#158464=CARTESIAN_POINT('Ctrl Pts',(-21.6158945838923,12.8010209065034,
3.67531602557404));
#158465=CARTESIAN_POINT('Ctrl Pts',(-21.6085107310244,12.6968744537646,
3.59424880257396));
#158466=CARTESIAN_POINT('Ctrl Pts',(-21.6011268781565,12.5891872591908,
3.51817467598181));
#158467=CARTESIAN_POINT('Ctrl Pts',(-21.5937442414511,12.4815178013097,
3.44211307923043));
#158468=CARTESIAN_POINT('Ctrl Pts',(-21.5863616047457,12.3703090248018,
3.37104312100045));
#158469=CARTESIAN_POINT('Ctrl Pts',(-21.5789789680403,12.2560360828037,
3.30527223079506));
#158470=CARTESIAN_POINT('Ctrl Pts',(-21.577121406017,12.2272836077984,3.2887234674252));
#158471=CARTESIAN_POINT('Ctrl Pts',(-21.5752638439937,12.1983372842333,
3.27250996499309));
#158472=CARTESIAN_POINT('Ctrl Pts',(-21.5734062819704,12.1692049547297,
3.25663617882909));
#158473=CARTESIAN_POINT('Ctrl Pts',(-21.5663770387532,12.0589646359696,
3.19656781915905));
#158474=CARTESIAN_POINT('Ctrl Pts',(-21.5593477955361,11.9460238764199,
3.14134860569491));
#158475=CARTESIAN_POINT('Ctrl Pts',(-21.5523185523189,11.8308409812737,
3.09121401641908));
#158476=CARTESIAN_POINT('Ctrl Pts',(-21.5452910829351,11.7156871525937,
3.04109207863409));
#158477=CARTESIAN_POINT('Ctrl Pts',(-21.5382636135512,11.598292668025,2.99605236218513));
#158478=CARTESIAN_POINT('Ctrl Pts',(-21.5312361441674,11.4791373964743,
2.95628291073201));
#158479=CARTESIAN_POINT('Ctrl Pts',(-21.5242072492004,11.3599579532428,
2.91650539170054));
#158480=CARTESIAN_POINT('Ctrl Pts',(-21.5171783542334,11.2390173728664,
2.88200040031871));
#158481=CARTESIAN_POINT('Ctrl Pts',(-21.5101494592664,11.1168123916017,
2.85290665147386));
#158482=CARTESIAN_POINT('Ctrl Pts',(-21.5031198947892,10.9945957701737,
2.82381013141641));
#158483=CARTESIAN_POINT('Ctrl Pts',(-21.496090330312,10.8711148837365,2.80012596375325));
#158484=CARTESIAN_POINT('Ctrl Pts',(-21.4890607658348,10.7468776224925,
2.78194193126202));
#158485=CARTESIAN_POINT('Ctrl Pts',(-21.4820266213085,10.6225594155855,
2.76374605112903));
#158486=CARTESIAN_POINT('Ctrl Pts',(-21.4749924767822,10.4974842312982,
2.75105751390997));
#158487=CARTESIAN_POINT('Ctrl Pts',(-21.4679583322559,10.3721662707993,
2.7439123504072));
#158488=CARTESIAN_POINT('Ctrl Pts',(-21.4643257671913,10.3074497095221,
2.74022245304675));
#158489=CARTESIAN_POINT('Ctrl Pts',(-21.4606932021268,10.2426684536507,
2.73801005930991));
#158490=CARTESIAN_POINT('Ctrl Pts',(-21.4570606370622,10.1778933606384,
2.73727468834243));
#158491=CARTESIAN_POINT('Ctrl Pts',(-21.4494486360556,10.0421578502062,
2.73573372639261));
#158492=CARTESIAN_POINT('Ctrl Pts',(-21.4418366350489,9.90636208137426,
2.74068047835051));
#158493=CARTESIAN_POINT('Ctrl Pts',(-21.4342246340423,9.77110640803279,
2.75209192269456));
#158494=CARTESIAN_POINT('Ctrl Pts',(-21.4264321638849,9.63264402511851,
2.76377391530407));
#158495=CARTESIAN_POINT('Ctrl Pts',(-21.4186396937276,9.49474795528324,
2.78223096696343));
#158496=CARTESIAN_POINT('Ctrl Pts',(-21.4108472235702,9.35805779034524,
2.80738197337714));
#158497=CARTESIAN_POINT('Ctrl Pts',(-21.4032412105133,9.22463832793057,
2.83193117014216));
#158498=CARTESIAN_POINT('Ctrl Pts',(-21.3956351974563,9.09236799004524,
2.86285756196605));
#158499=CARTESIAN_POINT('Ctrl Pts',(-21.3880291843993,8.96183334801938,
2.90003370869316));
#158500=CARTESIAN_POINT('Ctrl Pts',(-21.3801434856918,8.82649873181441,
2.93857688367882));
#158501=CARTESIAN_POINT('Ctrl Pts',(-21.3722577869842,8.69303018501617,
2.98383817560741));
#158502=CARTESIAN_POINT('Ctrl Pts',(-21.3643720882767,8.56206766416862,
3.03561797090767));
#158503=CARTESIAN_POINT('Ctrl Pts',(-21.3564863895691,8.43110514332108,
3.08739776620794));
#158504=CARTESIAN_POINT('Ctrl Pts',(-21.3486006908616,8.30264895994336,
3.14569598622589));
#158505=CARTESIAN_POINT('Ctrl Pts',(-21.340714992154,8.17732045741597,3.2102554131556));
#158506=CARTESIAN_POINT('Ctrl Pts',(-21.3336761719785,8.06545151277584,
3.26788153021242));
#158507=CARTESIAN_POINT('Ctrl Pts',(-21.3266373518029,7.95611455042713,
3.33047599778825));
#158508=CARTESIAN_POINT('Ctrl Pts',(-21.3195985316273,7.84976015631307,
3.39778467535514));
#158509=CARTESIAN_POINT('Ctrl Pts',(-21.3125599213837,7.74340893420629,
3.46509134544864));
#158510=CARTESIAN_POINT('Ctrl Pts',(-21.3055213111402,7.6400404255637,3.53711173986184));
#158511=CARTESIAN_POINT('Ctrl Pts',(-21.2984827008966,7.54007733081936,
3.61354769111783));
#158512=CARTESIAN_POINT('Ctrl Pts',(-21.2914403979205,7.44006179149318,
3.69002374368832));
#158513=CARTESIAN_POINT('Ctrl Pts',(-21.2843980949443,7.34345554026389,
3.77091974958848));
#158514=CARTESIAN_POINT('Ctrl Pts',(-21.2773557919682,7.25064938419331,
3.85589629117145));
#158515=CARTESIAN_POINT('Ctrl Pts',(-21.270311531557,7.15781743229572,3.94089645231006));
#158516=CARTESIAN_POINT('Ctrl Pts',(-21.2632672711458,7.06878795662045,
4.02997914451082));
#158517=CARTESIAN_POINT('Ctrl Pts',(-21.2562230107345,6.98391525521804,
4.12276771646865));
#158518=CARTESIAN_POINT('Ctrl Pts',(-21.2491723165041,6.89896503600872,
4.21564103613083));
#158519=CARTESIAN_POINT('Ctrl Pts',(-21.2421216222736,6.8181794261953,4.31222670801673));
#158520=CARTESIAN_POINT('Ctrl Pts',(-21.2350709280432,6.74187298426385,
4.41211433748425));
#158521=CARTESIAN_POINT('Ctrl Pts',(-21.2315037344441,6.70326687792428,
4.46265099399217));
#158522=CARTESIAN_POINT('Ctrl Pts',(-21.2279365408449,6.6658066369646,4.51403236253905));
#158523=CARTESIAN_POINT('Ctrl Pts',(-21.2243693472458,6.62952875518707,
4.56620249702597));
#158524=CARTESIAN_POINT('Ctrl Pts',(-21.2173459196766,6.55810143621733,
4.66891998366267));
#158525=CARTESIAN_POINT('Ctrl Pts',(-21.2103224921073,6.49113206267362,
4.77488133278218));
#158526=CARTESIAN_POINT('Ctrl Pts',(-21.203299064538,6.42891752586231,4.88366865729751));
#158527=CARTESIAN_POINT('Ctrl Pts',(-21.1962814635001,6.3667546013078,4.99236573346224));
#158528=CARTESIAN_POINT('Ctrl Pts',(-21.1892638624622,6.30933885072374,
5.10388378270884));
#158529=CARTESIAN_POINT('Ctrl Pts',(-21.1822462614242,6.25692354442136,
5.21777650231572));
#158530=CARTESIAN_POINT('Ctrl Pts',(-21.1752329179883,6.20454003866059,
5.33160012282876));
#158531=CARTESIAN_POINT('Ctrl Pts',(-21.1682195745524,6.15715109672532,
5.44779519409355));
#158532=CARTESIAN_POINT('Ctrl Pts',(-21.1612062311164,6.11496361461179,
5.5658917019994));
#158533=CARTESIAN_POINT('Ctrl Pts',(-21.1541425572128,6.07247337879379,
5.6848357161669));
#158534=CARTESIAN_POINT('Ctrl Pts',(-21.1470788833092,6.03525973704695,
5.80570821283149));
#158535=CARTESIAN_POINT('Ctrl Pts',(-21.1400152094056,6.00348440058743,
5.92800920087711));
#158536=CARTESIAN_POINT('Ctrl Pts',(-21.133004253243,5.97194621040375,6.04939742993803));
#158537=CARTESIAN_POINT('Ctrl Pts',(-21.1259932970804,5.94576549596376,
6.17219251371173));
#158538=CARTESIAN_POINT('Ctrl Pts',(-21.1189823409179,5.925049909777,6.29589174211361));
#158539=CARTESIAN_POINT('Ctrl Pts',(-21.1119707114441,5.90433233412748,
6.41960285021839));
#158540=CARTESIAN_POINT('Ctrl Pts',(-21.1049590819704,5.88908099593137,
6.54421789437491));
#158541=CARTESIAN_POINT('Ctrl Pts',(-21.0979474524966,5.87935206069904,
6.66922591689215));
#158542=CARTESIAN_POINT('Ctrl Pts',(-21.0909337323132,5.86962022451783,
6.79427121398003));
#158543=CARTESIAN_POINT('Ctrl Pts',(-21.0839200121298,5.86541410001686,
6.91970933719594));
#158544=CARTESIAN_POINT('Ctrl Pts',(-21.0769062919464,5.86673779564441,
7.04502653792429));
#158545=CARTESIAN_POINT('Ctrl Pts',(-21.06980393907,5.8680782188723,7.17192737767607));
#158546=CARTESIAN_POINT('Ctrl Pts',(-21.0627015861936,5.87508918354248,
7.29870380973344));
#158547=CARTESIAN_POINT('Ctrl Pts',(-21.0555992333171,5.88772067164072,
7.42482599909129));
#158548=CARTESIAN_POINT('Ctrl Pts',(-21.0485733140547,5.90021622305687,
7.54959089532375));
#158549=CARTESIAN_POINT('Ctrl Pts',(-21.0415473947922,5.9182117997394,7.67371518534136));
#158550=CARTESIAN_POINT('Ctrl Pts',(-21.0345214755298,5.9416072606581,7.79669530171039));
#158551=CARTESIAN_POINT('Ctrl Pts',(-21.0273809058464,5.96538449360439,
7.92168223335618));
#158552=CARTESIAN_POINT('Ctrl Pts',(-21.020240336163,5.99473928967706,8.04548691534146));
#158553=CARTESIAN_POINT('Ctrl Pts',(-21.0130997664796,6.02951374026827,
8.16759653562821));
#158554=CARTESIAN_POINT('Ctrl Pts',(-21.0059591967962,6.06428819085948,
8.28970615591497));
#158555=CARTESIAN_POINT('Ctrl Pts',(-20.9988186271128,6.10448211338605,
8.41012033914232));
#158556=CARTESIAN_POINT('Ctrl Pts',(-20.9916780574294,6.14988677165161,
8.52834798156522));
#158557=CARTESIAN_POINT('Ctrl Pts',(-20.9848875394138,6.19306556040558,
8.6407797582169));
#158558=CARTESIAN_POINT('Ctrl Pts',(-20.9780970213983,6.24110041539954,
8.75160786112374));
#158559=CARTESIAN_POINT('Ctrl Pts',(-20.9713065033827,6.29385322449215,
8.86037168693147));
#158560=CARTESIAN_POINT('Ctrl Pts',(-20.964525196406,6.34653447672102,8.96898797939648));
#158561=CARTESIAN_POINT('Ctrl Pts',(-20.9577438894292,6.40392078324138,
9.07554518694513));
#158562=CARTESIAN_POINT('Ctrl Pts',(-20.9509625824525,6.46582471863268,
9.17959914495719));
#158563=CARTESIAN_POINT('Ctrl Pts',(-20.9441885968762,6.52766181978393,
9.28354076169135));
#158564=CARTESIAN_POINT('Ctrl Pts',(-20.9374146112999,6.59400664137681,
9.38498414360832));
#158565=CARTESIAN_POINT('Ctrl Pts',(-20.9306406257236,6.66462456931131,
9.48350704645866));
#158566=CARTESIAN_POINT('Ctrl Pts',(-20.923872081502,6.73518577182298,9.58195080859381));
#158567=CARTESIAN_POINT('Ctrl Pts',(-20.9171035372804,6.81001301240761,
9.67747841681211));
#158568=CARTESIAN_POINT('Ctrl Pts',(-20.9103349930588,6.88882723169973,
9.76969475011184));
#158569=CARTESIAN_POINT('Ctrl Pts',(-20.9035692778455,6.96760850947957,
9.8618725402971));
#158570=CARTESIAN_POINT('Ctrl Pts',(-20.8968035626323,7.05037318437453,
9.9507414859558));
#158571=CARTESIAN_POINT('Ctrl Pts',(-20.890037847419,7.13680097017415,10.0359383256054));
#158572=CARTESIAN_POINT('Ctrl Pts',(-20.8832733657405,7.2232129983373,10.1211196320463));
#158573=CARTESIAN_POINT('Ctrl Pts',(-20.8765088840621,7.31328651177657,
10.2026298682361));
#158574=CARTESIAN_POINT('Ctrl Pts',(-20.8697444023836,7.40666387645209,
10.28014213782));
#158575=CARTESIAN_POINT('Ctrl Pts',(-20.8629794634639,7.50004755291707,
10.3576596468014));
#158576=CARTESIAN_POINT('Ctrl Pts',(-20.8562145245441,7.59673520141363,
10.4311783842624));
#158577=CARTESIAN_POINT('Ctrl Pts',(-20.8494495856244,7.6963362060632,10.5004118260392));
#158578=CARTESIAN_POINT('Ctrl Pts',(-20.8426824984199,7.79596884016584,
10.5696672536977));
#158579=CARTESIAN_POINT('Ctrl Pts',(-20.8359154112155,7.8985163245618,10.6346344420979));
#158580=CARTESIAN_POINT('Ctrl Pts',(-20.829148324011,8.00355986516484,10.6950707088088));
#158581=CARTESIAN_POINT('Ctrl Pts',(-20.8223732475449,8.10872742076868,
10.7555783269196));
#158582=CARTESIAN_POINT('Ctrl Pts',(-20.8155981710788,8.21639654982388,
10.8115441384382));
#158583=CARTESIAN_POINT('Ctrl Pts',(-20.8088230946128,8.3261246357037,10.8627718409776));
#158584=CARTESIAN_POINT('Ctrl Pts',(-20.8020434620293,8.43592651175376,
10.9140339932283));
#158585=CARTESIAN_POINT('Ctrl Pts',(-20.7952638294458,8.54778971316061,
10.9605515370318));
#158586=CARTESIAN_POINT('Ctrl Pts',(-20.7884841968622,8.66125425324206,
11.002177335792));
#158587=CARTESIAN_POINT('Ctrl Pts',(-20.7816937465263,8.77489984020051,
11.0438695537248));
#158588=CARTESIAN_POINT('Ctrl Pts',(-20.7749032961903,8.89015146681934,
11.0806543242509));
#158589=CARTESIAN_POINT('Ctrl Pts',(-20.7681128458544,9.00653654290877,
11.1124350540814));
#158590=CARTESIAN_POINT('Ctrl Pts',(-20.7650708197739,9.05867541725731,
11.1266723732895));
#158591=CARTESIAN_POINT('Ctrl Pts',(-20.7620287936935,9.11104166406988,
11.1399061162083));
#158592=CARTESIAN_POINT('Ctrl Pts',(-20.7589867676131,9.16359245771118,
11.1521309733376));
#158593=CARTESIAN_POINT('Ctrl Pts',(-20.7486393029828,9.34234420543419,
11.1937138767748));
#158594=CARTESIAN_POINT('Ctrl Pts',(-20.7382918383526,9.5237420713755,11.2237406026673));
#158595=CARTESIAN_POINT('Ctrl Pts',(-20.7279443737223,9.70657007694164,
11.2419687976436));
#158596=CARTESIAN_POINT('Ctrl Pts',(-20.7200690256185,9.84571857741016,
11.2558420879492));
#158597=CARTESIAN_POINT('Ctrl Pts',(-20.7121936775147,9.9856955507432,11.2628818575557));
#158598=CARTESIAN_POINT('Ctrl Pts',(-20.7043183294109,10.1259540174844,
11.2629985252177));
#158599=CARTESIAN_POINT('Ctrl Pts',(-22.6135314280912,10.1295000920819,
11.263));
#158600=CARTESIAN_POINT('Ctrl Pts',(-22.6114426391579,10.1665302112095,
11.2629999992001));
#158601=CARTESIAN_POINT('Ctrl Pts',(-22.6093563312962,10.2035677796465,
11.262517511459));
#158602=CARTESIAN_POINT('Ctrl Pts',(-22.5828596258304,10.6748181369334,
11.250231487439));
#158603=CARTESIAN_POINT('Ctrl Pts',(-22.5592251208326,11.1047589224831,
11.172614884571));
#158604=CARTESIAN_POINT('Ctrl Pts',(-22.5159786266063,11.83186799329,10.9226282195187));
#158605=CARTESIAN_POINT('Ctrl Pts',(-22.4969476089091,12.1343159013056,
10.777008501496));
#158606=CARTESIAN_POINT('Ctrl Pts',(-22.4658534516122,12.6055680940911,
10.4774105216325));
#158607=CARTESIAN_POINT('Ctrl Pts',(-22.4535160694584,12.7847545671071,
10.3425920108082));
#158608=CARTESIAN_POINT('Ctrl Pts',(-22.4257157609656,13.1588088195395,
10.0120171476607));
#158609=CARTESIAN_POINT('Ctrl Pts',(-22.4102300281437,13.3469450757265,
9.81015975406352));
#158610=CARTESIAN_POINT('Ctrl Pts',(-22.3707596136098,13.7710920754039,
9.25619313536883));
#158611=CARTESIAN_POINT('Ctrl Pts',(-22.3475308067559,13.9766212163167,
8.88448187132161));
#158612=CARTESIAN_POINT('Ctrl Pts',(-22.2991991860079,14.2795982494886,
8.07147405339804));
#158613=CARTESIAN_POINT('Ctrl Pts',(-22.2738563707513,14.3687544511833,
7.63252285753962));
#158614=CARTESIAN_POINT('Ctrl Pts',(-22.2344289353595,14.3998763445003,
6.92661806501799));
#158615=CARTESIAN_POINT('Ctrl Pts',(-22.2200568265937,14.3873460295288,
6.66496438588235));
#158616=CARTESIAN_POINT('Ctrl Pts',(-22.1818402111224,14.2918563360692,
5.98621612201307));
#158617=CARTESIAN_POINT('Ctrl Pts',(-22.1577020672557,14.1704683909691,
5.57749075443616));
#158618=CARTESIAN_POINT('Ctrl Pts',(-22.1204988010786,13.8881914365572,
4.97416426877736));
#158619=CARTESIAN_POINT('Ctrl Pts',(-22.1071795825062,13.7671114862297,
4.76403100142559));
#158620=CARTESIAN_POINT('Ctrl Pts',(-22.0671856153995,13.356689442883,4.174136086842));
#158621=CARTESIAN_POINT('Ctrl Pts',(-22.040061063534,13.0208609312589,3.83135894128661));
#158622=CARTESIAN_POINT('Ctrl Pts',(-21.997829069187,12.4074877547101,3.38568534891367));
#158623=CARTESIAN_POINT('Ctrl Pts',(-21.982342286845,12.1637828884393,3.24311393211752));
#158624=CARTESIAN_POINT('Ctrl Pts',(-21.9509701153768,11.6537930500623,
3.0090335913358));
#158625=CARTESIAN_POINT('Ctrl Pts',(-21.9351613841381,11.3889377721737,
2.91771004900118));
#158626=CARTESIAN_POINT('Ctrl Pts',(-21.8880369349077,10.5774214126253,
2.72445713079606));
#158627=CARTESIAN_POINT('Ctrl Pts',(-21.8580091533467,10.0178534544547,
2.702508135162));
#158628=CARTESIAN_POINT('Ctrl Pts',(-21.8117350925593,9.20799888551045,
2.82936143448262));
#158629=CARTESIAN_POINT('Ctrl Pts',(-21.7966922808976,8.9505832899176,2.89469190842999));
#158630=CARTESIAN_POINT('Ctrl Pts',(-21.7658144070032,8.42862069443619,
3.08034542418168));
#158631=CARTESIAN_POINT('Ctrl Pts',(-21.7499354473133,8.16689659842979,
3.20462489799745));
#158632=CARTESIAN_POINT('Ctrl Pts',(-21.7181513147124,7.68071999843214,
3.49931712327065));
#158633=CARTESIAN_POINT('Ctrl Pts',(-21.7023403176168,7.456512124172,3.66736853387015));
#158634=CARTESIAN_POINT('Ctrl Pts',(-21.6552296339294,6.84146664781248,
4.23062311346996));
#158635=CARTESIAN_POINT('Ctrl Pts',(-21.6252062531605,6.50952114646976,
4.68130093424691));
#158636=CARTESIAN_POINT('Ctrl Pts',(-21.5789403259214,6.16021652511212,
5.42260242657841));
#158637=CARTESIAN_POINT('Ctrl Pts',(-21.5638981717868,6.06985381932021,
5.67234174953908));
#158638=CARTESIAN_POINT('Ctrl Pts',(-21.5345482489233,5.93749382557748,
6.18221655998195));
#158639=CARTESIAN_POINT('Ctrl Pts',(-21.5201589270318,5.89519802892576,
6.44109555311767));
#158640=CARTESIAN_POINT('Ctrl Pts',(-21.4828396833504,5.84845620697068,
7.10860567556486));
#158641=CARTESIAN_POINT('Ctrl Pts',(-21.4596577911668,5.87839873192986,
7.51696953547816));
#158642=CARTESIAN_POINT('Ctrl Pts',(-21.423550649416,6.01694477422831,8.14752324270353));
#158643=CARTESIAN_POINT('Ctrl Pts',(-21.4104259251066,6.08748232390585,
8.37550581925328));
#158644=CARTESIAN_POINT('Ctrl Pts',(-21.3655742102444,6.38912305546613,
9.12238960843889));
#158645=CARTESIAN_POINT('Ctrl Pts',(-21.3333897070469,6.70441487023999,
9.60072283825932));
#158646=CARTESIAN_POINT('Ctrl Pts',(-21.2868929381845,7.29624627282401,
10.1969137484751));
#158647=CARTESIAN_POINT('Ctrl Pts',(-21.2718238897837,7.50656447427855,
10.3716151107222));
#158648=CARTESIAN_POINT('Ctrl Pts',(-21.2355726264431,8.04030007418018,
10.7346101683361));
#158649=CARTESIAN_POINT('Ctrl Pts',(-21.2143744670667,8.3746396975226,10.9028895836668));
#158650=CARTESIAN_POINT('Ctrl Pts',(-21.1804533596015,8.9500000326423,11.10340386045));
#158651=CARTESIAN_POINT('Ctrl Pts',(-21.1673753465103,9.17950354419723,
11.1625292427343));
#158652=CARTESIAN_POINT('Ctrl Pts',(-21.1407215400377,9.6494148452743,11.2426807480191));
#158653=CARTESIAN_POINT('Ctrl Pts',(-21.1271864912783,9.88908519110593,
11.2629817136974));
#158654=CARTESIAN_POINT('Ctrl Pts',(-21.1136182899058,10.1291755310197,
11.2629999876519));
#158655=CARTESIAN_POINT('Origin',(-23.734,10.1295,7.));
#158656=CARTESIAN_POINT('',(-19.2041804192452,10.1294996037974,11.263));
#158657=CARTESIAN_POINT('',(-19.613681670589,10.1296816520865,11.2629999961298));
#158658=CARTESIAN_POINT('',(-23.734,10.1295,11.263));
#158659=CARTESIAN_POINT('Ctrl Pts',(-19.2041804192453,10.1294996037957,
11.263));
#158660=CARTESIAN_POINT('Ctrl Pts',(-19.2091555077248,10.0412386223353,
11.262999991797));
#158661=CARTESIAN_POINT('Ctrl Pts',(-19.2141495951209,9.95288587610765,
11.2602590200357));
#158662=CARTESIAN_POINT('Ctrl Pts',(-19.2344704309081,9.594334766552,11.2379329597718));
#158663=CARTESIAN_POINT('Ctrl Pts',(-19.2496908269967,9.32630807408874,
11.195398846032));
#158664=CARTESIAN_POINT('Ctrl Pts',(-19.2797045996433,8.80247160325071,
11.0601954801443));
#158665=CARTESIAN_POINT('Ctrl Pts',(-19.2946346564539,8.54783738766795,
10.9679379581973));
#158666=CARTESIAN_POINT('Ctrl Pts',(-19.3315996706072,7.95264534116758,
10.6858323724252));
#158667=CARTESIAN_POINT('Ctrl Pts',(-19.3536979505227,7.62600903500464,
10.4722620550939));
#158668=CARTESIAN_POINT('Ctrl Pts',(-19.3877232763041,7.16394309676322,
10.0706208008373));
#158669=CARTESIAN_POINT('Ctrl Pts',(-19.4000643592666,7.00688143635039,
9.91075471545546));
#158670=CARTESIAN_POINT('Ctrl Pts',(-19.4357313461682,6.59599208944473,
9.4208009938086));
#158671=CARTESIAN_POINT('Ctrl Pts',(-19.4593951127358,6.37691098361786,
9.06495067689065));
#158672=CARTESIAN_POINT('Ctrl Pts',(-19.4958348981863,6.11940880274535,
8.46570780361107));
#158673=CARTESIAN_POINT('Ctrl Pts',(-19.5088537924435,6.04426507456067,
8.24096309539799));
#158674=CARTESIAN_POINT('Ctrl Pts',(-19.5535524077618,5.85366486086651,
7.46032192478212));
#158675=CARTESIAN_POINT('Ctrl Pts',(-19.5857113991186,5.83041185246494,
6.88816788272283));
#158676=CARTESIAN_POINT('Ctrl Pts',(-19.6323145553016,5.96283750508647,
6.05828516392695));
#158677=CARTESIAN_POINT('Ctrl Pts',(-19.6474509864785,6.03178219950232,
5.79310020348745));
#158678=CARTESIAN_POINT('Ctrl Pts',(-19.6857655215158,6.26573850417946,
5.15310490708459));
#158679=CARTESIAN_POINT('Ctrl Pts',(-19.7088843434601,6.46014558211258,
4.79193919500421));
#158680=CARTESIAN_POINT('Ctrl Pts',(-19.7465491137239,6.86432665940929,
4.24583352824216));
#158681=CARTESIAN_POINT('Ctrl Pts',(-19.7615422170789,7.04619287785323,
4.04365037828345));
#158682=CARTESIAN_POINT('Ctrl Pts',(-19.7984847782363,7.53088218012923,
3.59854141372588));
#158683=CARTESIAN_POINT('Ctrl Pts',(-19.8204696525764,7.85001162023237,
3.37692371205805));
#158684=CARTESIAN_POINT('Ctrl Pts',(-19.8566369314541,8.42965415314089,
3.08167682554085));
#158685=CARTESIAN_POINT('Ctrl Pts',(-19.8711968764263,8.67527171508076,
2.98403797096035));
#158686=CARTESIAN_POINT('Ctrl Pts',(-19.9081683831554,9.30841328477263,
2.7981068549328));
#158687=CARTESIAN_POINT('Ctrl Pts',(-19.9307401674725,9.70220546686087,
2.74000951869332));
#158688=CARTESIAN_POINT('Ctrl Pts',(-19.9694380892079,10.3980406039924,
2.73492315147449));
#158689=CARTESIAN_POINT('Ctrl Pts',(-19.9858727647485,10.6971367123354,
2.76434369637872));
#158690=CARTESIAN_POINT('Ctrl Pts',(-20.0227662733845,11.3432954392777,
2.89762198974648));
#158691=CARTESIAN_POINT('Ctrl Pts',(-20.0432699897383,11.6852809105655,
3.01473420416989));
#158692=CARTESIAN_POINT('Ctrl Pts',(-20.076651410723,12.2202683677404,3.27742892102962));
#158693=CARTESIAN_POINT('Ctrl Pts',(-20.0896708823895,12.4230772446439,
3.39883984538454));
#158694=CARTESIAN_POINT('Ctrl Pts',(-20.1334004236417,13.060990745914,3.85657432071279));
#158695=CARTESIAN_POINT('Ctrl Pts',(-20.1645279866838,13.441139920168,4.25996144938882));
#158696=CARTESIAN_POINT('Ctrl Pts',(-20.2100247655609,13.8790518431926,
4.95364727143574));
#158697=CARTESIAN_POINT('Ctrl Pts',(-20.2250273884282,14.0015916712933,
5.19622618956876));
#158698=CARTESIAN_POINT('Ctrl Pts',(-20.260882647435,14.2334407076506,5.789709985387));
#158699=CARTESIAN_POINT('Ctrl Pts',(-20.2818214487302,14.322168679465,6.14637236301619));
#158700=CARTESIAN_POINT('Ctrl Pts',(-20.3135537072225,14.3880112771085,
6.71538442436535));
#158701=CARTESIAN_POINT('Ctrl Pts',(-20.3248315747683,14.3968038232362,
6.9222480698235));
#158702=CARTESIAN_POINT('Ctrl Pts',(-20.3546688285941,14.380365048869,7.46552067577716));
#158703=CARTESIAN_POINT('Ctrl Pts',(-20.3733100925241,14.3303361250923,
7.79969984624028));
#158704=CARTESIAN_POINT('Ctrl Pts',(-20.417539114031,14.1239496172783,8.55441328809823));
#158705=CARTESIAN_POINT('Ctrl Pts',(-20.4428344074042,13.939685282225,8.96323388419608));
#158706=CARTESIAN_POINT('Ctrl Pts',(-20.4837268841908,13.5544044546243,
9.55136430710921));
#158707=CARTESIAN_POINT('Ctrl Pts',(-20.4987792036827,13.3941307270601,
9.75347485757442));
#158708=CARTESIAN_POINT('Ctrl Pts',(-20.5178127710289,13.161755636317,9.99748555588612));
#158709=CARTESIAN_POINT('Ctrl Pts',(-20.522248843943,13.1053061725239,10.0535344672164));
#158710=CARTESIAN_POINT('Ctrl Pts',(-20.5321349407436,12.9736042138546,
10.1771785327503));
#158711=CARTESIAN_POINT('Ctrl Pts',(-20.5375188011386,12.8974492660982,
10.2437401275997));
#158712=CARTESIAN_POINT('Ctrl Pts',(-20.558580141542,12.5853323786389,10.4975358412307));
#158713=CARTESIAN_POINT('Ctrl Pts',(-20.5735495753211,12.3321844091471,
10.6622488002918));
#158714=CARTESIAN_POINT('Ctrl Pts',(-20.5972520006835,11.923575169114,10.8702994496326));
#158715=CARTESIAN_POINT('Ctrl Pts',(-20.6055199827159,11.7795335659103,
10.9338666400614));
#158716=CARTESIAN_POINT('Ctrl Pts',(-20.618904508283,11.5481062279498,11.0210475063173));
#158717=CARTESIAN_POINT('Ctrl Pts',(-20.6238506098718,11.4629173548294,
11.0500942269107));
#158718=CARTESIAN_POINT('Ctrl Pts',(-20.6339717950465,11.2898491377814,
11.1030527573785));
#158719=CARTESIAN_POINT('Ctrl Pts',(-20.6391462195046,11.2019957859215,
11.1268878189299));
#158720=CARTESIAN_POINT('Ctrl Pts',(-20.6537883564757,10.9555454474256,
11.1853500835783));
#158721=CARTESIAN_POINT('Ctrl Pts',(-20.6634370025332,10.7956451865527,
11.2137569600568));
#158722=CARTESIAN_POINT('Ctrl Pts',(-20.6836076701493,10.4657507135338,
11.2531160154837));
#158723=CARTESIAN_POINT('Ctrl Pts',(-20.6941318382673,10.2959301957534,
11.2631390120574));
#158724=CARTESIAN_POINT('Ctrl Pts',(-20.7046820180537,10.1259765948704,
11.2629985439379));
#158725=CARTESIAN_POINT('Ctrl Pts',(-19.613681670589,10.1296816520865,11.2629999961298));
#158726=CARTESIAN_POINT('Ctrl Pts',(-19.6210625559268,9.99792696780947,
11.2630056103717));
#158727=CARTESIAN_POINT('Ctrl Pts',(-19.6284434412646,9.86616452721088,
11.2568987546168));
#158728=CARTESIAN_POINT('Ctrl Pts',(-19.6358243266025,9.73495915245449,
11.2447033488358));
#158729=CARTESIAN_POINT('Ctrl Pts',(-19.6432038414137,9.60377814069074,
11.2325102075702));
#158730=CARTESIAN_POINT('Ctrl Pts',(-19.6505833562249,9.47315430553389,
11.2142308037361));
#158731=CARTESIAN_POINT('Ctrl Pts',(-19.6579628710361,9.34364777489142,
11.1899409638194));
#158732=CARTESIAN_POINT('Ctrl Pts',(-19.665341452104,9.21415763094539,11.1656541973403));
#158733=CARTESIAN_POINT('Ctrl Pts',(-19.6727200331718,9.0857848227637,11.1353585705236));
#158734=CARTESIAN_POINT('Ctrl Pts',(-19.6800986142396,8.95908014795422,
11.0991811828629));
#158735=CARTESIAN_POINT('Ctrl Pts',(-19.6849303155029,8.87611038293851,
11.0754912175352));
#158736=CARTESIAN_POINT('Ctrl Pts',(-19.6897620167663,8.79385571635695,
11.049280203234));
#158737=CARTESIAN_POINT('Ctrl Pts',(-19.6945937180296,8.71246771439215,
11.0205955406563));
#158738=CARTESIAN_POINT('Ctrl Pts',(-19.7016228891401,8.59406424510147,
10.9788650216284));
#158739=CARTESIAN_POINT('Ctrl Pts',(-19.7086520602506,8.47745739883753,
10.9318830738138));
#158740=CARTESIAN_POINT('Ctrl Pts',(-19.7156812313611,8.36312882780601,
10.8798327131517));
#158741=CARTESIAN_POINT('Ctrl Pts',(-19.7227086284805,8.24882911051486,
10.82779548873));
#158742=CARTESIAN_POINT('Ctrl Pts',(-19.7297360255998,8.13680687283187,
10.7706925591275));
#158743=CARTESIAN_POINT('Ctrl Pts',(-19.7367634227191,8.02752294555477,
10.7087547050979));
#158744=CARTESIAN_POINT('Ctrl Pts',(-19.7437922455919,7.91821684620777,
10.6468042848066));
#158745=CARTESIAN_POINT('Ctrl Pts',(-19.7508210684647,7.8116505045704,10.5800171656424));
#158746=CARTESIAN_POINT('Ctrl Pts',(-19.7578498913375,7.70825937959702,
10.5086696707029));
#158747=CARTESIAN_POINT('Ctrl Pts',(-19.7648793838462,7.60485840455196,
10.4373153784882));
#158748=CARTESIAN_POINT('Ctrl Pts',(-19.7719088763549,7.50463356199163,
10.3614000686881));
#158749=CARTESIAN_POINT('Ctrl Pts',(-19.7789383688636,7.40798992434636,
10.2812424336089));
#158750=CARTESIAN_POINT('Ctrl Pts',(-19.7859724420486,7.31128331014651,
10.2010325648618));
#158751=CARTESIAN_POINT('Ctrl Pts',(-19.7930065152336,7.21816285464981,
10.1165750994141));
#158752=CARTESIAN_POINT('Ctrl Pts',(-19.8000405884186,7.12899939384763,
10.0282280482948));
#158753=CARTESIAN_POINT('Ctrl Pts',(-19.8036735132583,7.08294867145319,
9.98259898131086));
#158754=CARTESIAN_POINT('Ctrl Pts',(-19.807306438098,7.03795286658765,9.93593298706528));
#158755=CARTESIAN_POINT('Ctrl Pts',(-19.8109393629378,6.99405904894667,
9.88828306134593));
#158756=CARTESIAN_POINT('Ctrl Pts',(-19.8185514682813,6.90208787460305,
9.78844167453286));
#158757=CARTESIAN_POINT('Ctrl Pts',(-19.8261635736248,6.81489782850554,
9.68421427120516));
#158758=CARTESIAN_POINT('Ctrl Pts',(-19.8337756789683,6.73287352582023,
9.57606242061428));
#158759=CARTESIAN_POINT('Ctrl Pts',(-19.8415681230414,6.64890598169537,
9.46534833967273));
#158760=CARTESIAN_POINT('Ctrl Pts',(-19.8493605671145,6.5703521935622,9.35052175498863));
#158761=CARTESIAN_POINT('Ctrl Pts',(-19.8571530111877,6.49757984993105,
9.23211223363054));
#158762=CARTESIAN_POINT('Ctrl Pts',(-19.8647591278018,6.42654758755655,
9.11653403772446));
#158763=CARTESIAN_POINT('Ctrl Pts',(-19.872365244416,6.36102356679838,8.99754254531327));
#158764=CARTESIAN_POINT('Ctrl Pts',(-19.8799713610301,6.30130558280906,
8.8756589519921));
#158765=CARTESIAN_POINT('Ctrl Pts',(-19.8878569688327,6.23939322668899,
8.74929667498954));
#158766=CARTESIAN_POINT('Ctrl Pts',(-19.8957425766354,6.18372190273754,
8.61982593912762));
#158767=CARTESIAN_POINT('Ctrl Pts',(-19.903628184438,6.13457147332775,8.48785586223272));
#158768=CARTESIAN_POINT('Ctrl Pts',(-19.9115137922407,6.08542104391795,
8.35588578533781));
#158769=CARTESIAN_POINT('Ctrl Pts',(-19.9193994000433,6.04279165902778,
8.22141665147341));
#158770=CARTESIAN_POINT('Ctrl Pts',(-19.927285007846,6.00690792403289,8.085082289586));
#158771=CARTESIAN_POINT('Ctrl Pts',(-19.9343237861388,5.97487771643589,
7.96338877260736));
#158772=CARTESIAN_POINT('Ctrl Pts',(-19.9413625644316,5.94823387545845,
7.8402524200153));
#158773=CARTESIAN_POINT('Ctrl Pts',(-19.9484013427244,5.92708903886797,
7.71617812990721));
#158774=CARTESIAN_POINT('Ctrl Pts',(-19.9554399109056,5.90594483346336,
7.59210754349001));
#158775=CARTESIAN_POINT('Ctrl Pts',(-19.9624784790867,5.89029936842274,
7.46709945251523));
#158776=CARTESIAN_POINT('Ctrl Pts',(-19.9695170472678,5.8802139040895,7.3416674920177));
#158777=CARTESIAN_POINT('Ctrl Pts',(-19.9765593081639,5.87012314851751,
7.21616972488726));
#158778=CARTESIAN_POINT('Ctrl Pts',(-19.9836015690599,5.86559825316507,
7.0902480255059));
#158779=CARTESIAN_POINT('Ctrl Pts',(-19.990643829956,5.86664848269717,6.96441992932841));
#158780=CARTESIAN_POINT('Ctrl Pts',(-19.9976880482936,5.86769900414732,
6.83855685842447));
#158781=CARTESIAN_POINT('Ctrl Pts',(-20.0047322666312,5.87432772657293,
6.71278782503369));
#158782=CARTESIAN_POINT('Ctrl Pts',(-20.0117764849689,5.88649181534104,
6.58762814727832));
#158783=CARTESIAN_POINT('Ctrl Pts',(-20.0188271374083,5.89866701463715,
6.46235415022382));
#158784=CARTESIAN_POINT('Ctrl Pts',(-20.0258777898477,5.91638763336263,
6.33769100055036));
#158785=CARTESIAN_POINT('Ctrl Pts',(-20.0329284422871,5.93955916974701,
6.21414706275352));
#158786=CARTESIAN_POINT('Ctrl Pts',(-20.0364958457761,5.95128322230163,
6.15163780158474));
#158787=CARTESIAN_POINT('Ctrl Pts',(-20.0400632492651,5.96440191628728,
6.08941489423676));
#158788=CARTESIAN_POINT('Ctrl Pts',(-20.0436306527542,5.97889809135828,
6.02754290789789));
#158789=CARTESIAN_POINT('Ctrl Pts',(-20.0506540818166,6.00743785637264,
5.90573064070087));
#158790=CARTESIAN_POINT('Ctrl Pts',(-20.0576775108791,6.04137122992328,
5.78506070393765));
#158791=CARTESIAN_POINT('Ctrl Pts',(-20.0647009399416,6.08058632073389,
5.6660333520467));
#158792=CARTESIAN_POINT('Ctrl Pts',(-20.0717185423857,6.11976887880798,
5.54710474493479));
#158793=CARTESIAN_POINT('Ctrl Pts',(-20.0787361448298,6.16422430917893,
5.42981637531585));
#158794=CARTESIAN_POINT('Ctrl Pts',(-20.085753747274,6.21379041548669,5.3146550947208));
#158795=CARTESIAN_POINT('Ctrl Pts',(-20.0927670920274,6.2633264492517,5.19956368430097));
#158796=CARTESIAN_POINT('Ctrl Pts',(-20.0997804367809,6.31796683139565,
5.08659714716067));
#158797=CARTESIAN_POINT('Ctrl Pts',(-20.1067937815343,6.37750071407498,
4.97622373805349));
#158798=CARTESIAN_POINT('Ctrl Pts',(-20.1138574549108,6.43746181920613,
4.86505827581068));
#158799=CARTESIAN_POINT('Ctrl Pts',(-20.1209211282873,6.5023867959048,4.75652367863071));
#158800=CARTESIAN_POINT('Ctrl Pts',(-20.1279848016638,6.57201228474143,
4.65107468067111));
#158801=CARTESIAN_POINT('Ctrl Pts',(-20.1349957589147,6.64111815923273,
4.54641264755664));
#158802=CARTESIAN_POINT('Ctrl Pts',(-20.1420067161656,6.71485438329882,
4.44479062478944));
#158803=CARTESIAN_POINT('Ctrl Pts',(-20.1490176734164,6.79291940437145,
4.34662499279219));
#158804=CARTESIAN_POINT('Ctrl Pts',(-20.1560293038896,6.87099192158304,
4.2484499345089));
#158805=CARTESIAN_POINT('Ctrl Pts',(-20.1630409343627,6.95339382288946,
4.15373223076921));
#158806=CARTESIAN_POINT('Ctrl Pts',(-20.1700525648358,7.03978297499938,
4.06285551846333));
#158807=CARTESIAN_POINT('Ctrl Pts',(-20.1770662859279,7.12619788528295,
3.97195170995291));
#158808=CARTESIAN_POINT('Ctrl Pts',(-20.1840800070199,7.21660214710082,
3.88489145349599));
#158809=CARTESIAN_POINT('Ctrl Pts',(-20.191093728112,7.3106167200912,3.80202156757576));
#158810=CARTESIAN_POINT('Ctrl Pts',(-20.1981960793168,7.4058193246704,3.71810448185337));
#158811=CARTESIAN_POINT('Ctrl Pts',(-20.2052984305217,7.50472380869981,
3.63848467191371));
#158812=CARTESIAN_POINT('Ctrl Pts',(-20.2124007817266,7.6069029600472,3.5634794960569));
#158813=CARTESIAN_POINT('Ctrl Pts',(-20.2194267016631,7.70798252029948,
3.4892814811754));
#158814=CARTESIAN_POINT('Ctrl Pts',(-20.2264526215996,7.81226625486711,
3.41959943125368));
#158815=CARTESIAN_POINT('Ctrl Pts',(-20.2334785415361,7.91931293289363,
3.3546958798482));
#158816=CARTESIAN_POINT('Ctrl Pts',(-20.2406191083752,8.02810636724196,
3.28873325131098));
#158817=CARTESIAN_POINT('Ctrl Pts',(-20.2477596752143,8.13975333669771,
3.22770663540868));
#158818=CARTESIAN_POINT('Ctrl Pts',(-20.2549002420533,8.25376708692567,
3.17184182160537));
#158819=CARTESIAN_POINT('Ctrl Pts',(-20.2620408088924,8.36778083715362,
3.11597700780207));
#158820=CARTESIAN_POINT('Ctrl Pts',(-20.2691813757315,8.48416096703565,
3.06527411157802));
#158821=CARTESIAN_POINT('Ctrl Pts',(-20.2763219425705,8.60240284429547,
3.0199066245829));
#158822=CARTESIAN_POINT('Ctrl Pts',(-20.2831124685135,8.71484833401245,
2.97676311730259));
#158823=CARTESIAN_POINT('Ctrl Pts',(-20.2899029944564,8.82935140599041,
2.93830145149597));
#158824=CARTESIAN_POINT('Ctrl Pts',(-20.2966935203994,8.94547734886698,
2.90472719326246));
#158825=CARTESIAN_POINT('Ctrl Pts',(-20.3034748353439,9.06144577288687,
2.87119847677993));
#158826=CARTESIAN_POINT('Ctrl Pts',(-20.3102561502883,9.17903229471747,
2.842544107233));
#158827=CARTESIAN_POINT('Ctrl Pts',(-20.3170374652328,9.29778142242843,
2.81892200410919));
#158828=CARTESIAN_POINT('Ctrl Pts',(-20.3238114588109,9.41640234404969,
2.79532540430932));
#158829=CARTESIAN_POINT('Ctrl Pts',(-20.330585452389,9.53618296819803,2.77675035206636));
#158830=CARTESIAN_POINT('Ctrl Pts',(-20.3373594459671,9.65665251765119,
2.76330503122583));
#158831=CARTESIAN_POINT('Ctrl Pts',(-20.3441279982186,9.77702529787156,
2.74987051056998));
#158832=CARTESIAN_POINT('Ctrl Pts',(-20.3508965504701,9.89808548802565,
2.74155757451038));
#158833=CARTESIAN_POINT('Ctrl Pts',(-20.3576651027216,10.0193527277818,
2.73842322861328));
#158834=CARTESIAN_POINT('Ctrl Pts',(-20.3644308259848,10.1405692826068,
2.73529019274934));
#158835=CARTESIAN_POINT('Ctrl Pts',(-20.371196549248,10.2619922966189,2.73733145918129));
#158836=CARTESIAN_POINT('Ctrl Pts',(-20.3779622725112,10.383137499644,2.74455207777438));
#158837=CARTESIAN_POINT('Ctrl Pts',(-20.384726762254,10.5042606155877,2.75177137991097));
#158838=CARTESIAN_POINT('Ctrl Pts',(-20.3914912519967,10.6251056025061,
2.7641681330934));
#158839=CARTESIAN_POINT('Ctrl Pts',(-20.3982557417395,10.7451902242561,
2.78169529932278));
#158840=CARTESIAN_POINT('Ctrl Pts',(-20.405020688733,10.8652829632157,2.79922365031404));
#158841=CARTESIAN_POINT('Ctrl Pts',(-20.4117856357265,10.9846148196652,
2.82188304272845));
#158842=CARTESIAN_POINT('Ctrl Pts',(-20.41855058272,11.1027114907248,2.84957491402132));
#158843=CARTESIAN_POINT('Ctrl Pts',(-20.4253176780028,11.2208456647849,
2.87727557919678));
#158844=CARTESIAN_POINT('Ctrl Pts',(-20.4320847732856,11.3377434657248,
2.91001180325871));
#158845=CARTESIAN_POINT('Ctrl Pts',(-20.4388518685683,11.4529443165418,
2.9476347473342));
#158846=CARTESIAN_POINT('Ctrl Pts',(-20.4456269530807,11.5682811734314,
2.98530210904052));
#158847=CARTESIAN_POINT('Ctrl Pts',(-20.4524020375931,11.6819166829018,
3.0278675742583));
#158848=CARTESIAN_POINT('Ctrl Pts',(-20.4591771221056,11.7934087946616,
3.07513356621555));
#158849=CARTESIAN_POINT('Ctrl Pts',(-20.4659567627322,11.9049758827261,
3.12243134364499));
#158850=CARTESIAN_POINT('Ctrl Pts',(-20.4727364033589,12.0143963278875,
3.1744357569713));
#158851=CARTESIAN_POINT('Ctrl Pts',(-20.4795160439856,12.1212529943158,
3.23090342261781));
#158852=CARTESIAN_POINT('Ctrl Pts',(-20.4863065022887,12.2282801625317,
3.28746118875372));
#158853=CARTESIAN_POINT('Ctrl Pts',(-20.4930969605919,12.3327350284989,
3.34849620756881));
#158854=CARTESIAN_POINT('Ctrl Pts',(-20.499887418895,12.434229583985,3.41372190917881));
#158855=CARTESIAN_POINT('Ctrl Pts',(-20.5029293567257,12.479696342509,3.44294122257403));
#158856=CARTESIAN_POINT('Ctrl Pts',(-20.5059712945563,12.5245694743666,
3.47300098129164));
#158857=CARTESIAN_POINT('Ctrl Pts',(-20.5090132323869,12.5688163807365,
3.50387291497142));
#158858=CARTESIAN_POINT('Ctrl Pts',(-20.5160528500654,12.6712120645548,
3.57531639021697));
#158859=CARTESIAN_POINT('Ctrl Pts',(-20.5230924677439,12.7706045269319,
3.65135814019731));
#158860=CARTESIAN_POINT('Ctrl Pts',(-20.5301320854224,12.8665642076717,
3.73172086212295));
#158861=CARTESIAN_POINT('Ctrl Pts',(-20.5371627173815,12.9624014006857,
3.81198100505939));
#158862=CARTESIAN_POINT('Ctrl Pts',(-20.5441933493406,13.0548142404394,
3.89655089391907));
#158863=CARTESIAN_POINT('Ctrl Pts',(-20.5512239812998,13.1434028817285,
3.98511054605499));
#158864=CARTESIAN_POINT('Ctrl Pts',(-20.5582472086855,13.2318982225716,
4.07357692827592));
#158865=CARTESIAN_POINT('Ctrl Pts',(-20.5652704360712,13.3165771118334,
4.16602443564554));
#158866=CARTESIAN_POINT('Ctrl Pts',(-20.5722936634569,13.3970737490667,
4.26209372066711));
#158867=CARTESIAN_POINT('Ctrl Pts',(-20.579352449238,13.477977938426,4.35864940167621));
#158868=CARTESIAN_POINT('Ctrl Pts',(-20.5864112350191,13.5546571020791,
4.45886338581479));
#158869=CARTESIAN_POINT('Ctrl Pts',(-20.5934700208002,13.6267777203579,
4.56233358584726));
#158870=CARTESIAN_POINT('Ctrl Pts',(-20.6004831025417,13.6984313739637,
4.6651338397634));
#158871=CARTESIAN_POINT('Ctrl Pts',(-20.6074961842832,13.7655851192017,
4.77114794331499));
#158872=CARTESIAN_POINT('Ctrl Pts',(-20.6145092660247,13.8279529364795,
4.87994932215142));
#158873=CARTESIAN_POINT('Ctrl Pts',(-20.6215201005457,13.8903007690717,
4.98871583747262));
#158874=CARTESIAN_POINT('Ctrl Pts',(-20.6285309350668,13.947865534977,5.10026751473464));
#158875=CARTESIAN_POINT('Ctrl Pts',(-20.6355417695879,14.000405778642,5.214150775436));
#158876=CARTESIAN_POINT('Ctrl Pts',(-20.6425517747268,14.0529398067936,
5.32802056374194));
#158877=CARTESIAN_POINT('Ctrl Pts',(-20.6495617798658,14.1004503352034,
5.44422103493076));
#158878=CARTESIAN_POINT('Ctrl Pts',(-20.6565717850048,14.1427430711648,
5.56227643416836));
#158879=CARTESIAN_POINT('Ctrl Pts',(-20.6636661797713,14.1855449463016,
5.68175303795214));
#158880=CARTESIAN_POINT('Ctrl Pts',(-20.6707605745379,14.2230024133749,
5.80312915290586));
#158881=CARTESIAN_POINT('Ctrl Pts',(-20.6778549693044,14.2549654534142,
5.92589395649855));
#158882=CARTESIAN_POINT('Ctrl Pts',(-20.6848700180614,14.2865710084581,
6.04728571875378));
#158883=CARTESIAN_POINT('Ctrl Pts',(-20.6918850668184,14.3128043681359,
6.17003487300886));
#158884=CARTESIAN_POINT('Ctrl Pts',(-20.6989001155754,14.3335717231044,
6.29363610865666));
#158885=CARTESIAN_POINT('Ctrl Pts',(-20.7060341833467,14.3546914220416,
6.41933439277077));
#158886=CARTESIAN_POINT('Ctrl Pts',(-20.713168251118,14.37015788043,6.5459135246403));
#158887=CARTESIAN_POINT('Ctrl Pts',(-20.7203023188893,14.3799273655978,
6.6728361117461));
#158888=CARTESIAN_POINT('Ctrl Pts',(-20.7274363866606,14.3896968507655,
6.79975869885191));
#158889=CARTESIAN_POINT('Ctrl Pts',(-20.7345704544319,14.3937693782952,
6.92702432229997));
#158890=CARTESIAN_POINT('Ctrl Pts',(-20.7417045222032,14.3921567579672,
7.05409587559758));
#158891=CARTESIAN_POINT('Ctrl Pts',(-20.7487553738306,14.3905629482322,
7.17968518832687));
#158892=CARTESIAN_POINT('Ctrl Pts',(-20.755806225458,14.3834131442202,7.30531135250305));
#158893=CARTESIAN_POINT('Ctrl Pts',(-20.7628570770854,14.3707114727388,
7.43045817858265));
#158894=CARTESIAN_POINT('Ctrl Pts',(-20.7699025977755,14.35801940461,7.55551038490363));
#158895=CARTESIAN_POINT('Ctrl Pts',(-20.7769481184657,14.339783866004,7.68008359541989));
#158896=CARTESIAN_POINT('Ctrl Pts',(-20.7839936391558,14.316060990687,7.80366415327441));
#158897=CARTESIAN_POINT('Ctrl Pts',(-20.7910351758234,14.2923515299169,
7.92717483017315));
#158898=CARTESIAN_POINT('Ctrl Pts',(-20.7980767124911,14.2631609851212,
8.0496935975355));
#158899=CARTESIAN_POINT('Ctrl Pts',(-20.8051182491587,14.2285969725616,
8.17071474302503));
#158900=CARTESIAN_POINT('Ctrl Pts',(-20.8121573620581,14.1940448572855,
8.29169423180984));
#158901=CARTESIAN_POINT('Ctrl Pts',(-20.8191964749575,14.1541230641496,
8.41117675831594));
#158902=CARTESIAN_POINT('Ctrl Pts',(-20.8262355878569,14.108989607831,8.52866983392907));
#158903=CARTESIAN_POINT('Ctrl Pts',(-20.8332745473014,14.0638571354359,
8.64616034815655));
#158904=CARTESIAN_POINT('Ctrl Pts',(-20.8403135067459,14.0135133592023,
8.76166113931436));
#158905=CARTESIAN_POINT('Ctrl Pts',(-20.8473524661904,13.9581651263394,
8.87469793576249));
#158906=CARTESIAN_POINT('Ctrl Pts',(-20.8509183664974,13.9301259989493,
8.93196178993535));
#158907=CARTESIAN_POINT('Ctrl Pts',(-20.8544842668044,13.9008033009508,
8.98859361159937));
#158908=CARTESIAN_POINT('Ctrl Pts',(-20.8580501671115,13.8702285225073,
9.04453396178702));
#158909=CARTESIAN_POINT('Ctrl Pts',(-20.8656423239006,13.8051317750523,
9.16363653698444));
#158910=CARTESIAN_POINT('Ctrl Pts',(-20.8732344806897,13.7343815652685,
9.27955752070515));
#158911=CARTESIAN_POINT('Ctrl Pts',(-20.8808266374789,13.6583076665164,
9.39179544542065));
#158912=CARTESIAN_POINT('Ctrl Pts',(-20.8886240686906,13.580176904863,9.50706802495553));
#158913=CARTESIAN_POINT('Ctrl Pts',(-20.8964214999023,13.4964306780399,
9.61845531819866));
#158914=CARTESIAN_POINT('Ctrl Pts',(-20.9042189311141,13.4074713236086,
9.72544913759181));
#158915=CARTESIAN_POINT('Ctrl Pts',(-20.9118275959575,13.3206655674334,
9.8298527661687));
#158916=CARTESIAN_POINT('Ctrl Pts',(-20.919436260801,13.2288963926095,9.93007301888403));
#158917=CARTESIAN_POINT('Ctrl Pts',(-20.9270449256444,13.1325767406681,
10.0256733283119));
#158918=CARTESIAN_POINT('Ctrl Pts',(-20.9349367400403,13.0326726403515,
10.1248313164367));
#158919=CARTESIAN_POINT('Ctrl Pts',(-20.9428285544362,12.9278730596348,
10.2190186506561));
#158920=CARTESIAN_POINT('Ctrl Pts',(-20.950720368832,12.8186793474327,10.3077913231251));
#158921=CARTESIAN_POINT('Ctrl Pts',(-20.9586121832279,12.7094856352306,
10.396563995594));
#158922=CARTESIAN_POINT('Ctrl Pts',(-20.9665039976238,12.5958980403162,
10.4799218091269));
#158923=CARTESIAN_POINT('Ctrl Pts',(-20.9743958120197,12.4784556130269,
10.5574677128583));
#158924=CARTESIAN_POINT('Ctrl Pts',(-20.9814299786755,12.3737763131122,
10.6265862682323));
#158925=CARTESIAN_POINT('Ctrl Pts',(-20.9884641453313,12.2659720439805,
10.6911283149499));
#158926=CARTESIAN_POINT('Ctrl Pts',(-20.9954983119871,12.1554741760127,
10.7508129303032));
#158927=CARTESIAN_POINT('Ctrl Pts',(-21.0025285897974,12.0450373968928,
10.810464548962));
#158928=CARTESIAN_POINT('Ctrl Pts',(-21.0095588676077,11.9319103223061,
10.8652639016021));
#158929=CARTESIAN_POINT('Ctrl Pts',(-21.016589145418,11.8165508198208,10.9149749081369));
#158930=CARTESIAN_POINT('Ctrl Pts',(-21.0236176753931,11.7012199974825,
10.9646735557508));
#158931=CARTESIAN_POINT('Ctrl Pts',(-21.0306462053682,11.5836582040373,
11.0092862208708));
#158932=CARTESIAN_POINT('Ctrl Pts',(-21.0376747353433,11.4643451254216,
11.0486241479221));
#158933=CARTESIAN_POINT('Ctrl Pts',(-21.0447021255488,11.345051395008,11.0879556958055));
#158934=CARTESIAN_POINT('Ctrl Pts',(-21.0517295157543,11.2240073113907,
11.1220140919123));
#158935=CARTESIAN_POINT('Ctrl Pts',(-21.0587569059598,11.1017091471191,
11.1506599926106));
#158936=CARTESIAN_POINT('Ctrl Pts',(-21.0657861500461,10.9793787196288,
11.179313450323));
#158937=CARTESIAN_POINT('Ctrl Pts',(-21.0728153941325,10.8557939254294,
11.2025514728704));
#158938=CARTESIAN_POINT('Ctrl Pts',(-21.0798446382189,10.7314627077289,
11.2202855233389));
#158939=CARTESIAN_POINT('Ctrl Pts',(-21.0834769111219,10.6672161248101,
11.2294493694347));
#158940=CARTESIAN_POINT('Ctrl Pts',(-21.0871091840249,10.6027703828996,
11.2371443975746));
#158941=CARTESIAN_POINT('Ctrl Pts',(-21.0907414569279,10.5381962379688,
11.2433638054108));
#158942=CARTESIAN_POINT('Ctrl Pts',(-21.0983881948149,10.4022533796668,
11.2564570345833));
#158943=CARTESIAN_POINT('Ctrl Pts',(-21.106034932702,10.2657163342166,11.2630102654163));
#158944=CARTESIAN_POINT('Ctrl Pts',(-21.113681670589,10.1291791134783,11.262999987923));
#158945=CARTESIAN_POINT('Origin',(-23.734,10.1295,7.));
#158946=CARTESIAN_POINT('',(-17.7339525171114,10.1295,11.263));
#158947=CARTESIAN_POINT('',(-18.1138504934428,10.1295003780334,11.263));
#158948=CARTESIAN_POINT('',(-23.734,10.1295,11.263));
#158949=CARTESIAN_POINT('',(-17.734,9.60084442449481,11.2300936493755));
#158950=CARTESIAN_POINT('Origin',(-17.734,10.1295,7.));
#158951=CARTESIAN_POINT('Ctrl Pts',(-17.734,9.60084442449481,11.2300936493755));
#158952=CARTESIAN_POINT('Ctrl Pts',(-17.7617000790389,9.11002742083171,
11.1687538382398));
#158953=CARTESIAN_POINT('Ctrl Pts',(-17.7887513666815,8.6336091385854,11.0224564453886));
#158954=CARTESIAN_POINT('Ctrl Pts',(-17.8283758438164,8.010079686466,10.7045055574008));
#158955=CARTESIAN_POINT('Ctrl Pts',(-17.8400356673621,7.83418479791178,
10.5981710316897));
#158956=CARTESIAN_POINT('Ctrl Pts',(-17.8640864842584,7.48374154752343,
10.3501251931301));
#158957=CARTESIAN_POINT('Ctrl Pts',(-17.8764309707687,7.31133675452661,
10.2064522936414));
#158958=CARTESIAN_POINT('Ctrl Pts',(-17.9198792988024,6.75185233693977,
9.6600686649743));
#158959=CARTESIAN_POINT('Ctrl Pts',(-17.9515705295498,6.43307107325946,
9.19565118676176));
#158960=CARTESIAN_POINT('Ctrl Pts',(-17.9980608413685,6.10246074027769,
8.42626318993039));
#158961=CARTESIAN_POINT('Ctrl Pts',(-18.0134821699885,6.01764435575489,
8.15927229438703));
#158962=CARTESIAN_POINT('Ctrl Pts',(-18.0446219329139,5.90228404118004,
7.61627701282578));
#158963=CARTESIAN_POINT('Ctrl Pts',(-18.0602607748556,5.87128772424761,
7.34172435081686));
#158964=CARTESIAN_POINT('Ctrl Pts',(-18.0972591962321,5.86109815311643,
6.68480301531689));
#158965=CARTESIAN_POINT('Ctrl Pts',(-18.1180605746812,5.90637601846631,
6.3044208662641));
#158966=CARTESIAN_POINT('Ctrl Pts',(-18.1543359347367,6.0683334091008,5.67659879469026));
#158967=CARTESIAN_POINT('Ctrl Pts',(-18.1694414484725,6.15917338165903,
5.42489206896729));
#158968=CARTESIAN_POINT('Ctrl Pts',(-18.2068265544821,6.44111102179745,
4.82637038093062));
#158969=CARTESIAN_POINT('Ctrl Pts',(-18.2284065883895,6.65801820869123,
4.49446631522699));
#158970=CARTESIAN_POINT('Ctrl Pts',(-18.2655853293336,7.09602773048975,
3.99251414384753));
#158971=CARTESIAN_POINT('Ctrl Pts',(-18.2809060786613,7.29373013801882,
3.80542228181663));
#158972=CARTESIAN_POINT('Ctrl Pts',(-18.3192560865802,7.82847773736109,
3.38838423076535));
#158973=CARTESIAN_POINT('Ctrl Pts',(-18.341548988857,8.18320909687546,3.18549702299022));
#158974=CARTESIAN_POINT('Ctrl Pts',(-18.3794638857893,8.81559460658373,
2.93532082146657));
#158975=CARTESIAN_POINT('Ctrl Pts',(-18.3948721589547,9.07899002309546,
2.85942216427453));
#158976=CARTESIAN_POINT('Ctrl Pts',(-18.4424258696319,9.90536277180713,
2.70528299904782));
#158977=CARTESIAN_POINT('Ctrl Pts',(-18.4731651406769,10.4780900647047,
2.71358801542172));
#158978=CARTESIAN_POINT('Ctrl Pts',(-18.5185046603243,11.2644782764602,
2.88400803732114));
#158979=CARTESIAN_POINT('Ctrl Pts',(-18.53198999126,11.4919602735929,2.95361063545592));
#158980=CARTESIAN_POINT('Ctrl Pts',(-18.5686148708944,12.0973915996452,
3.19573366261946));
#158981=CARTESIAN_POINT('Ctrl Pts',(-18.5911956664381,12.4578149803992,
3.40500412070652));
#158982=CARTESIAN_POINT('Ctrl Pts',(-18.6291092351267,12.9859944857833,
3.82489462925093));
#158983=CARTESIAN_POINT('Ctrl Pts',(-18.6438768977571,13.1743959422191,
4.00509425775862));
#158984=CARTESIAN_POINT('Ctrl Pts',(-18.6734351481004,13.5191402296173,
4.40120899021167));
#158985=CARTESIAN_POINT('Ctrl Pts',(-18.6880135235118,13.6740753746476,
4.61685847799688));
#158986=CARTESIAN_POINT('Ctrl Pts',(-18.7336176921056,14.0890532736973,
5.3253711472166));
#158987=CARTESIAN_POINT('Ctrl Pts',(-18.7652076931336,14.2735153696961,
5.85563052663519));
#158988=CARTESIAN_POINT('Ctrl Pts',(-18.8116050038436,14.3898807843215,
6.68309052149403));
#158989=CARTESIAN_POINT('Ctrl Pts',(-18.8270192336647,14.4014906778751,
6.96299679224388));
#158990=CARTESIAN_POINT('Ctrl Pts',(-18.8583536528325,14.3697681512779,
7.52086853484267));
#158991=CARTESIAN_POINT('Ctrl Pts',(-18.8742000416313,14.3265453993646,
7.79748518887851));
#158992=CARTESIAN_POINT('Ctrl Pts',(-18.9167049423928,14.1375265626357,
8.52800017652366));
#158993=CARTESIAN_POINT('Ctrl Pts',(-18.9425081846297,13.9423576196096,
8.96498868777149));
#158994=CARTESIAN_POINT('Ctrl Pts',(-18.9829336075695,13.5448823717088,
9.5626402559391));
#158995=CARTESIAN_POINT('Ctrl Pts',(-18.9967031462161,13.3936277925957,
9.75271330915583));
#158996=CARTESIAN_POINT('Ctrl Pts',(-19.034160076992,12.935590791635,10.2371238056325));
#158997=CARTESIAN_POINT('Ctrl Pts',(-19.0572543880736,12.5997652716431,
10.5001302140577));
#158998=CARTESIAN_POINT('Ctrl Pts',(-19.0957940148976,12.0032932316461,
10.8380143501432));
#158999=CARTESIAN_POINT('Ctrl Pts',(-19.1106329571733,11.7645652514517,
10.9456322875166));
#159000=CARTESIAN_POINT('Ctrl Pts',(-19.1519247247326,11.0703266384371,
11.184696243469));
#159001=CARTESIAN_POINT('Ctrl Pts',(-19.1775909176582,10.6012129243344,
11.2630000438411));
#159002=CARTESIAN_POINT('Ctrl Pts',(-19.2041804192453,10.1294996037957,
11.263));
#159003=CARTESIAN_POINT('Ctrl Pts',(-18.1138504934428,10.1295003780333,
11.263));
#159004=CARTESIAN_POINT('Ctrl Pts',(-18.1201664240278,10.0171997379224,
11.2630000099585));
#159005=CARTESIAN_POINT('Ctrl Pts',(-18.1264601646708,9.90482338535515,
11.2585625113639));
#159006=CARTESIAN_POINT('Ctrl Pts',(-18.1471939564367,9.5342147629796,11.2291849445822));
#159007=CARTESIAN_POINT('Ctrl Pts',(-18.1614510886987,9.27820419644792,
11.1851718184008));
#159008=CARTESIAN_POINT('Ctrl Pts',(-18.190679063517,8.77185199290599,11.04970983128));
#159009=CARTESIAN_POINT('Ctrl Pts',(-18.205722478305,8.52286768105405,10.9575348695707));
#159010=CARTESIAN_POINT('Ctrl Pts',(-18.2521528724009,7.78127034447633,
10.6014003031429));
#159011=CARTESIAN_POINT('Ctrl Pts',(-18.2823439987331,7.33072756467248,
10.2636080327611));
#159012=CARTESIAN_POINT('Ctrl Pts',(-18.3296550402369,6.77127318646973,
9.64075362893174));
#159013=CARTESIAN_POINT('Ctrl Pts',(-18.3454529965589,6.60541983307923,
9.41498111034329));
#159014=CARTESIAN_POINT('Ctrl Pts',(-18.3746159475739,6.33918555578304,
8.96607800534638));
#159015=CARTESIAN_POINT('Ctrl Pts',(-18.3879852293196,6.23352792098854,
8.74738335505999));
#159016=CARTESIAN_POINT('Ctrl Pts',(-18.4231228670393,6.00789011106766,
8.15655051036886));
#159017=CARTESIAN_POINT('Ctrl Pts',(-18.445300526248,5.91940671390389,7.77483965536696));
#159018=CARTESIAN_POINT('Ctrl Pts',(-18.482391861555,5.85950946605294,7.1168303996138));
#159019=CARTESIAN_POINT('Ctrl Pts',(-18.497354685792,5.86070678728025,6.84547915816173));
#159020=CARTESIAN_POINT('Ctrl Pts',(-18.5347943580174,5.92782518434814,
6.17387956069213));
#159021=CARTESIAN_POINT('Ctrl Pts',(-18.5577058978721,6.02501704398986,
5.77944802631504));
#159022=CARTESIAN_POINT('Ctrl Pts',(-18.6118397338822,6.38541040569196,
4.8864095166674));
#159023=CARTESIAN_POINT('Ctrl Pts',(-18.6422259979436,6.69442250090281,
4.4143285720778));
#159024=CARTESIAN_POINT('Ctrl Pts',(-18.7055321400725,7.47793199683672,
3.61529249690852));
#159025=CARTESIAN_POINT('Ctrl Pts',(-18.7359957244316,7.94522450923478,
3.2964889392701));
#159026=CARTESIAN_POINT('Ctrl Pts',(-18.7812347653197,8.68607200895231,
2.98133970829284));
#159027=CARTESIAN_POINT('Ctrl Pts',(-18.7951387550697,8.91921102446701,
2.90508648402335));
#159028=CARTESIAN_POINT('Ctrl Pts',(-18.8352464895255,9.61273249287762,
2.74269814882526));
#159029=CARTESIAN_POINT('Ctrl Pts',(-18.8606342384993,10.0822955872121,
2.71170935717385));
#159030=CARTESIAN_POINT('Ctrl Pts',(-18.9034985446018,10.8398949502786,
2.78635012991713));
#159031=CARTESIAN_POINT('Ctrl Pts',(-18.920172849714,11.1285598118538,2.84531682591275));
#159032=CARTESIAN_POINT('Ctrl Pts',(-18.9522999708127,11.6754893919508,
3.01738596676868));
#159033=CARTESIAN_POINT('Ctrl Pts',(-18.967703420322,11.9332242435038,3.12729058389462));
#159034=CARTESIAN_POINT('Ctrl Pts',(-19.0109361724726,12.6156088885913,
3.50127687237792));
#159035=CARTESIAN_POINT('Ctrl Pts',(-19.0393144976386,13.0074483977873,
3.81578754937372));
#159036=CARTESIAN_POINT('Ctrl Pts',(-19.0795464292398,13.4834803550414,
4.35915580258086));
#159037=CARTESIAN_POINT('Ctrl Pts',(-19.0918774504661,13.6174543555981,
4.53881822871678));
#159038=CARTESIAN_POINT('Ctrl Pts',(-19.1230581322882,13.9158838913541,
5.01266238566637));
#159039=CARTESIAN_POINT('Ctrl Pts',(-19.1421826533911,14.0607725750834,
5.31735360043846));
#159040=CARTESIAN_POINT('Ctrl Pts',(-19.1853242557598,14.3062974466496,
6.04429874103027));
#159041=CARTESIAN_POINT('Ctrl Pts',(-19.2087794214143,14.3814932447286,
6.47127597578725));
#159042=CARTESIAN_POINT('Ctrl Pts',(-19.2466684721848,14.3969497001182,
7.145096609166));
#159043=CARTESIAN_POINT('Ctrl Pts',(-19.2604707095446,14.381752049973,7.3879865648949));
#159044=CARTESIAN_POINT('Ctrl Pts',(-19.3005656529627,14.2768757074118,
8.09184703182885));
#159045=CARTESIAN_POINT('Ctrl Pts',(-19.3260305629335,14.1318180963956,
8.54087751131874));
#159046=CARTESIAN_POINT('Ctrl Pts',(-19.3679683490484,13.7896058996363,
9.20302695145331));
#159047=CARTESIAN_POINT('Ctrl Pts',(-19.3836501061341,13.6389632072953,
9.43585214398804));
#159048=CARTESIAN_POINT('Ctrl Pts',(-19.4148089165798,13.2931223158563,
9.87099362074104));
#159049=CARTESIAN_POINT('Ctrl Pts',(-19.430208841783,13.0983665680379,10.0719609623287));
#159050=CARTESIAN_POINT('Ctrl Pts',(-19.4735764674731,12.5025186741097,
10.576835535129));
#159051=CARTESIAN_POINT('Ctrl Pts',(-19.5021850689032,12.0653976838966,
10.8310913618801));
#159052=CARTESIAN_POINT('Ctrl Pts',(-19.5440264004416,11.3608570703204,
11.0888435365032));
#159053=CARTESIAN_POINT('Ctrl Pts',(-19.5576923663702,11.1205471605292,
11.1536376829205));
#159054=CARTESIAN_POINT('Ctrl Pts',(-19.5854566839399,10.6296085314679,
11.2409518821898));
#159055=CARTESIAN_POINT('Ctrl Pts',(-19.5996238369442,10.379883262343,11.262989129004));
#159056=CARTESIAN_POINT('Ctrl Pts',(-19.6137437660346,10.1296851569352,
11.262999995979));
#159057=CARTESIAN_POINT('Origin',(-18.734,-18.952,0.));
#159058=CARTESIAN_POINT('',(-20.7225805737622,-18.2258896078036,0.755484073133954));
#159059=CARTESIAN_POINT('',(-20.7225805737341,-18.2258896077265,0.534177427254549));
#159060=CARTESIAN_POINT('',(-20.7225805737622,-18.2258896078036,0.));
#159061=CARTESIAN_POINT('',(-20.8509997094771,-18.9508909130732,0.710943721022757));
#159062=CARTESIAN_POINT('Ctrl Pts',(-20.8509997094771,-18.9508909130732,
0.710943721022757));
#159063=CARTESIAN_POINT('Ctrl Pts',(-20.8509573783464,-18.8700902207682,
0.71578119702302));
#159064=CARTESIAN_POINT('Ctrl Pts',(-20.8462849658904,-18.7894513944425,
0.720618673023283));
#159065=CARTESIAN_POINT('Ctrl Pts',(-20.8370625267197,-18.7094778181125,
0.725456149023546));
#159066=CARTESIAN_POINT('Ctrl Pts',(-20.8275213698741,-18.6267404401649,
0.730460803041947));
#159067=CARTESIAN_POINT('Ctrl Pts',(-20.8131101401339,-18.5447154876357,
0.735465457060348));
#159068=CARTESIAN_POINT('Ctrl Pts',(-20.7939728278586,-18.463941654631,
0.74047011107875));
#159069=CARTESIAN_POINT('Ctrl Pts',(-20.7748355155832,-18.3831678216262,
0.745474765097151));
#159070=CARTESIAN_POINT('Ctrl Pts',(-20.7509723251239,-18.303645395105,
0.750479419115552));
#159071=CARTESIAN_POINT('Ctrl Pts',(-20.7225805737622,-18.2258896078036,
0.755484073133953));
#159072=CARTESIAN_POINT('',(-20.3539400851898,-17.5891048754966,2.1911925810487E-7));
#159073=CARTESIAN_POINT('Ctrl Pts',(-20.3539400851898,-17.5891048754966,
2.1911925810487E-7));
#159074=CARTESIAN_POINT('Ctrl Pts',(-20.3072931859159,-17.5336602703872,
0.00438523983104698));
#159075=CARTESIAN_POINT('Ctrl Pts',(-20.2577048501402,-17.4805043431566,
0.00877026054283585));
#159076=CARTESIAN_POINT('Ctrl Pts',(-20.2054284583706,-17.4299660674291,
0.0131552812546247));
#159077=CARTESIAN_POINT('Ctrl Pts',(-20.1532296863998,-17.3795028307521,
0.017533791103401));
#159078=CARTESIAN_POINT('Ctrl Pts',(-20.0983511257708,-17.3316498632894,
0.0219123009521774));
#159079=CARTESIAN_POINT('Ctrl Pts',(-20.0410859170619,-17.2867026075147,
0.0262908108009537));
#159080=CARTESIAN_POINT('Ctrl Pts',(-19.9838881021842,-17.241808248915,
0.030664167703297));
#159081=CARTESIAN_POINT('Ctrl Pts',(-19.9243095970083,-17.1998131057541,
0.0350375246056404));
#159082=CARTESIAN_POINT('Ctrl Pts',(-19.862678574843,-17.1609741278556,
0.0394108815079837));
#159083=CARTESIAN_POINT('Ctrl Pts',(-19.801086549423,-17.1221597251416,
0.0437814711888932));
#159084=CARTESIAN_POINT('Ctrl Pts',(-19.7374449915696,-17.0864977823031,
0.0481520608698027));
#159085=CARTESIAN_POINT('Ctrl Pts',(-19.6721120099387,-17.0542026302029,
0.0525226505507122));
#159086=CARTESIAN_POINT('Ctrl Pts',(-19.6067987309426,-17.0219172174345,
0.0568919221816862));
#159087=CARTESIAN_POINT('Ctrl Pts',(-19.5397954737533,-16.9929967935616,
0.0612611938126602));
#159088=CARTESIAN_POINT('Ctrl Pts',(-19.4714844671138,-16.9676094989227,
0.0656304654436342));
#159089=CARTESIAN_POINT('Ctrl Pts',(-19.4031714390129,-16.9422214530222,
0.0699998663702325));
#159090=CARTESIAN_POINT('Ctrl Pts',(-19.3335510382756,-16.9203669101752,
0.0743692672968309));
#159091=CARTESIAN_POINT('Ctrl Pts',(-19.2630233707279,-16.9021650619565,
0.0787386682234292));
#159092=CARTESIAN_POINT('Ctrl Pts',(-19.1924239083033,-16.883944684847,
0.0831125170583901));
#159093=CARTESIAN_POINT('Ctrl Pts',(-19.1209158041549,-16.8693845460032,
0.087486365893351));
#159094=CARTESIAN_POINT('Ctrl Pts',(-19.0489112989912,-16.8585531117872,
0.0918602147283118));
#159095=CARTESIAN_POINT('Ctrl Pts',(-18.9768669711113,-16.8477156871526,
0.0962364825583059));
#159096=CARTESIAN_POINT('Ctrl Pts',(-18.9043261767328,-16.8406111195394,
0.1006127503883));
#159097=CARTESIAN_POINT('Ctrl Pts',(-18.8317055633233,-16.8372558965928,
0.104989018218294));
#159098=CARTESIAN_POINT('Ctrl Pts',(-18.7589608117345,-16.8338949382048,
0.109372766870811));
#159099=CARTESIAN_POINT('Ctrl Pts',(-18.6861364519365,-16.8342961174985,
0.113756515523328));
#159100=CARTESIAN_POINT('Ctrl Pts',(-18.6136477260043,-16.8384238054558,
0.118140264175844));
#159101=CARTESIAN_POINT('Ctrl Pts',(-18.5716413935222,-16.8408157502787,
0.120680593048329));
#159102=CARTESIAN_POINT('Ctrl Pts',(-18.5297476644012,-16.8444581093918,
0.123220921920813));
#159103=CARTESIAN_POINT('Ctrl Pts',(-18.4880458342194,-16.8493360828855,
0.125761250793297));
#159104=CARTESIAN_POINT('Ctrl Pts',(-18.4158851594457,-16.8577769080795,
0.13015702538607));
#159105=CARTESIAN_POINT('Ctrl Pts',(-18.3440241643562,-16.8699525372844,
0.134552799978843));
#159106=CARTESIAN_POINT('Ctrl Pts',(-18.2728786958473,-16.8858305628878,
0.138948574571615));
#159107=CARTESIAN_POINT('Ctrl Pts',(-18.2018360533927,-16.9016856400904,
0.143337995981724));
#159108=CARTESIAN_POINT('Ctrl Pts',(-18.1315073495764,-16.9212323858817,
0.147727417391832));
#159109=CARTESIAN_POINT('Ctrl Pts',(-18.0623020683668,-16.9443867681648,
0.152116838801941));
#159110=CARTESIAN_POINT('Ctrl Pts',(-17.9931748039694,-16.9675150479445,
0.156501311909549));
#159111=CARTESIAN_POINT('Ctrl Pts',(-17.9251688996744,-16.9942427328982,
0.160885785017158));
#159112=CARTESIAN_POINT('Ctrl Pts',(-17.8586807914585,-17.0244354010414,
0.165270258124766));
#159113=CARTESIAN_POINT('Ctrl Pts',(-17.79223296666,-17.0546097762314,0.16965207479403));
#159114=CARTESIAN_POINT('Ctrl Pts',(-17.7273015495519,-17.0882447704819,
0.174033891463294));
#159115=CARTESIAN_POINT('Ctrl Pts',(-17.6642636992251,-17.1251575747196,
0.178415708132558));
#159116=CARTESIAN_POINT('Ctrl Pts',(-17.6012434550811,-17.1620600693801,
0.182796300980494));
#159117=CARTESIAN_POINT('Ctrl Pts',(-17.5401161419553,-17.2022383136031,
0.18717689382843));
#159118=CARTESIAN_POINT('Ctrl Pts',(-17.481233502117,-17.2454640051314,
0.191557486676366));
#159119=CARTESIAN_POINT('Ctrl Pts',(-17.4223480788122,-17.2886917400001,
0.19593828660119));
#159120=CARTESIAN_POINT('Ctrl Pts',(-17.3657079255823,-17.3349669223205,
0.200319086526014));
#159121=CARTESIAN_POINT('Ctrl Pts',(-17.3116336689764,-17.3840194451555,
0.204699886450838));
#159122=CARTESIAN_POINT('Ctrl Pts',(-17.2575022929462,-17.4331237828844,
0.20908531387839));
#159123=CARTESIAN_POINT('Ctrl Pts',(-17.2059425814251,-17.4850109948883,
0.213470741305941));
#159124=CARTESIAN_POINT('Ctrl Pts',(-17.1572394598231,-17.5393729441424,
0.217856168733493));
#159125=CARTESIAN_POINT('Ctrl Pts',(-17.1085090930288,-17.5937653042144,
0.222244049429123));
#159126=CARTESIAN_POINT('Ctrl Pts',(-17.0626387997765,-17.6506347838424,
0.226631930124754));
#159127=CARTESIAN_POINT('Ctrl Pts',(-17.019872504564,-17.7096409820868,
0.231019810820385));
#159128=CARTESIAN_POINT('Ctrl Pts',(-16.9770304728485,-17.7687516767129,
0.23541546218537));
#159129=CARTESIAN_POINT('Ctrl Pts',(-16.9373036781403,-17.8300062430902,
0.239811113550356));
#159130=CARTESIAN_POINT('Ctrl Pts',(-16.9008917879239,-17.8930366942999,
0.244206764915342));
#159131=CARTESIAN_POINT('Ctrl Pts',(-16.8767856560651,-17.9347653812468,
0.247116862435138));
#159132=CARTESIAN_POINT('Ctrl Pts',(-16.8541314891368,-17.9772719122011,
0.250026959954935));
#159133=CARTESIAN_POINT('Ctrl Pts',(-16.8329756005513,-18.0204447237547,
0.252937057474732));
#159134=CARTESIAN_POINT('Ctrl Pts',(-16.8011149915786,-18.0854626529992,
0.257319642435692));
#159135=CARTESIAN_POINT('Ctrl Pts',(-16.7725300877984,-18.1522470560442,
0.261702227396652));
#159136=CARTESIAN_POINT('Ctrl Pts',(-16.7474199512368,-18.2204340700553,
0.266084812357612));
#159137=CARTESIAN_POINT('Ctrl Pts',(-16.7223475943392,-18.2885184927293,
0.270460803464049));
#159138=CARTESIAN_POINT('Ctrl Pts',(-16.7007397931117,-18.3580008874103,
0.274836794570485));
#159139=CARTESIAN_POINT('Ctrl Pts',(-16.6827489310325,-18.4284944584252,
0.279212785676921));
#159140=CARTESIAN_POINT('Ctrl Pts',(-16.6647796228869,-18.4989035746903,
0.283583534131738));
#159141=CARTESIAN_POINT('Ctrl Pts',(-16.6504187653927,-18.5703209945558,
0.287954282586556));
#159142=CARTESIAN_POINT('Ctrl Pts',(-16.6397694152316,-18.6423433226608,
0.292325031041373));
#159143=CARTESIAN_POINT('Ctrl Pts',(-16.6291269614596,-18.714319009986,
0.29669294905288));
#159144=CARTESIAN_POINT('Ctrl Pts',(-16.6221913171743,-18.7868983510167,
0.301060867064387));
#159145=CARTESIAN_POINT('Ctrl Pts',(-16.6190144817355,-18.8596676788374,
0.305428785075894));
#159146=CARTESIAN_POINT('Ctrl Pts',(-16.6158386481743,-18.9324140574164,
0.309795325578371));
#159147=CARTESIAN_POINT('Ctrl Pts',(-16.616419291388,-19.0053498208129,
0.314161866080847));
#159148=CARTESIAN_POINT('Ctrl Pts',(-16.6207564193529,-19.0780577996553,
0.318528406583324));
#159149=CARTESIAN_POINT('Ctrl Pts',(-16.6250936203624,-19.1507670030232,
0.322895020625736));
#159150=CARTESIAN_POINT('Ctrl Pts',(-16.6331874009118,-19.2232479313927,
0.327261634668148));
#159151=CARTESIAN_POINT('Ctrl Pts',(-16.6449857626134,-19.2950867470421,
0.33162824871056));
#159152=CARTESIAN_POINT('Ctrl Pts',(-16.6567963363639,-19.3669999203992,
0.335999382474067));
#159153=CARTESIAN_POINT('Ctrl Pts',(-16.6723190685484,-19.4382691756095,
0.340370516237575));
#159154=CARTESIAN_POINT('Ctrl Pts',(-16.6914506293117,-19.5084899534592,
0.344741650001082));
#159155=CARTESIAN_POINT('Ctrl Pts',(-16.7105925668403,-19.578748818349,
0.349115154623362));
#159156=CARTESIAN_POINT('Ctrl Pts',(-16.7333470785608,-19.6479576138078,
0.353488659245642));
#159157=CARTESIAN_POINT('Ctrl Pts',(-16.7595614725531,-19.7157286830631,
0.357862163867922));
#159158=CARTESIAN_POINT('Ctrl Pts',(-16.7858226024992,-19.7836205769906,
0.362243465729771));
#159159=CARTESIAN_POINT('Ctrl Pts',(-16.8155557348011,-19.8500691841256,
0.36662476759162));
#159160=CARTESIAN_POINT('Ctrl Pts',(-16.8485609817509,-19.9147090466303,
0.371006069453469));
#159161=CARTESIAN_POINT('Ctrl Pts',(-16.871428766834,-19.9594949706928,
0.374041667687701));
#159162=CARTESIAN_POINT('Ctrl Pts',(-16.8958663395961,-20.0034131234881,
0.377077265921934));
#159163=CARTESIAN_POINT('Ctrl Pts',(-16.9217951774031,-20.0463503465328,
0.380112864156166));
#159164=CARTESIAN_POINT('Ctrl Pts',(-16.9592871194148,-20.108435654348,
0.384502203694482));
#159165=CARTESIAN_POINT('Ctrl Pts',(-17.0000462087351,-20.1687128298791,
0.388891543232798));
#159166=CARTESIAN_POINT('Ctrl Pts',(-17.0438726579669,-20.2268170722547,
0.393280882771114));
#159167=CARTESIAN_POINT('Ctrl Pts',(-17.0876341208282,-20.2848351569816,
0.397663713745537));
#159168=CARTESIAN_POINT('Ctrl Pts',(-17.1344536264988,-20.3406863231545,
0.402046544719961));
#159169=CARTESIAN_POINT('Ctrl Pts',(-17.1840869213948,-20.3940327488544,
0.406429375694384));
#159170=CARTESIAN_POINT('Ctrl Pts',(-17.2336619167729,-20.4473165135743,
0.410807058573494));
#159171=CARTESIAN_POINT('Ctrl Pts',(-17.2860438089119,-20.4981010311794,
0.415184741452605));
#159172=CARTESIAN_POINT('Ctrl Pts',(-17.3409477702607,-20.5460810786213,
0.419562424331716));
#159173=CARTESIAN_POINT('Ctrl Pts',(-17.3958169194766,-20.5940307040727,
0.42393733151897));
#159174=CARTESIAN_POINT('Ctrl Pts',(-17.4532046028361,-20.6391790711337,
0.428312238706224));
#159175=CARTESIAN_POINT('Ctrl Pts',(-17.5127898056829,-20.6812584136837,
0.432687145893477));
#159176=CARTESIAN_POINT('Ctrl Pts',(-17.5723568562232,-20.723324936992,
0.437060720289165));
#159177=CARTESIAN_POINT('Ctrl Pts',(-17.6341197035787,-20.7623240140802,
0.441434294684853));
#159178=CARTESIAN_POINT('Ctrl Pts',(-17.6977263244876,-20.7980297585467,
0.445807869080541));
#159179=CARTESIAN_POINT('Ctrl Pts',(-17.7613345200931,-20.8337363869733,
0.450181551751944));
#159180=CARTESIAN_POINT('Ctrl Pts',(-17.8267861585152,-20.8661492866597,
0.454555234423347));
#159181=CARTESIAN_POINT('Ctrl Pts',(-17.8937039331709,-20.8950881400676,
0.45892891709475));
#159182=CARTESIAN_POINT('Ctrl Pts',(-17.9606909349872,-20.924056931032,
0.463307124388118));
#159183=CARTESIAN_POINT('Ctrl Pts',(-18.0291466578795,-20.9495443083807,
0.467685331681485));
#159184=CARTESIAN_POINT('Ctrl Pts',(-18.0986738647242,-20.9714181592319,
0.472063538974852));
#159185=CARTESIAN_POINT('Ctrl Pts',(-18.1682389417348,-20.9933039243595,
0.476444130995642));
#159186=CARTESIAN_POINT('Ctrl Pts',(-18.2388761976446,-21.0115721233672,
0.480824723016432));
#159187=CARTESIAN_POINT('Ctrl Pts',(-18.3101759171462,-21.0261413034779,
0.485205315037221));
#159188=CARTESIAN_POINT('Ctrl Pts',(-18.3816016288558,-21.040736228475,
0.48959364790839));
#159189=CARTESIAN_POINT('Ctrl Pts',(-18.453691664747,-21.0516190094181,
0.49398198077956));
#159190=CARTESIAN_POINT('Ctrl Pts',(-18.5260294507966,-21.0587598939281,
0.498370313650729));
#159191=CARTESIAN_POINT('Ctrl Pts',(-18.5750331942104,-21.063597339078,
0.501343099379686));
#159192=CARTESIAN_POINT('Ctrl Pts',(-18.6241505410345,-21.0667186770647,
0.504315885108644));
#159193=CARTESIAN_POINT('Ctrl Pts',(-18.6732524746729,-21.0681282423725,
0.507288670837601));
#159194=CARTESIAN_POINT('Ctrl Pts',(-18.7457477477536,-21.0702093584171,
0.511677763023228));
#159195=CARTESIAN_POINT('Ctrl Pts',(-18.8184909227825,-21.068564845846,
0.516066855208855));
#159196=CARTESIAN_POINT('Ctrl Pts',(-18.8910671418926,-21.063165297398,
0.520455947394481));
#159197=CARTESIAN_POINT('Ctrl Pts',(-18.9635359951035,-21.0577737367921,
0.524838546560292));
#159198=CARTESIAN_POINT('Ctrl Pts',(-19.035837905828,-21.0486382034475,
0.529221145726103));
#159199=CARTESIAN_POINT('Ctrl Pts',(-19.1075566421874,-21.0357812829272,
0.533603744891914));
#159200=CARTESIAN_POINT('Ctrl Pts',(-19.1791915341236,-21.0229393930828,
0.537981220480296));
#159201=CARTESIAN_POINT('Ctrl Pts',(-19.2502441338016,-21.0063848432238,
0.542358696068678));
#159202=CARTESIAN_POINT('Ctrl Pts',(-19.32030366582,-20.9861919799876,0.54673617165706));
#159203=CARTESIAN_POINT('Ctrl Pts',(-19.3903190177729,-20.9660118505222,
0.551110886776558));
#159204=CARTESIAN_POINT('Ctrl Pts',(-19.4593420824552,-20.9421980932421,
0.555485601896056));
#159205=CARTESIAN_POINT('Ctrl Pts',(-19.5269740036053,-20.91487575501,0.559860317015555));
#159206=CARTESIAN_POINT('Ctrl Pts',(-19.594585560535,-20.8875616436346,
0.564233714892226));
#159207=CARTESIAN_POINT('Ctrl Pts',(-19.6608063587658,-20.8567412292126,
0.568607112768897));
#159208=CARTESIAN_POINT('Ctrl Pts',(-19.7252559833366,-20.8225882966327,
0.572980510645567));
#159209=CARTESIAN_POINT('Ctrl Pts',(-19.7897074377077,-20.7884343944112,
0.577354032688118));
#159210=CARTESIAN_POINT('Ctrl Pts',(-19.852387193486,-20.7509480137079,
0.581727554730669));
#159211=CARTESIAN_POINT('Ctrl Pts',(-19.9129394779501,-20.7103488582562,
0.58610107677322));
#159212=CARTESIAN_POINT('Ctrl Pts',(-19.9735547637542,-20.6697074616038,
0.590479149226244));
#159213=CARTESIAN_POINT('Ctrl Pts',(-20.0320377575059,-20.6259470930867,
0.594857221679268));
#159214=CARTESIAN_POINT('Ctrl Pts',(-20.0880624400643,-20.5793303009552,
0.599235294132292));
#159215=CARTESIAN_POINT('Ctrl Pts',(-20.1441178212582,-20.5326879652269,
0.603615765543133));
#159216=CARTESIAN_POINT('Ctrl Pts',(-20.1977118548978,-20.4831864169906,
0.607996236953973));
#159217=CARTESIAN_POINT('Ctrl Pts',(-20.2485543758915,-20.431126107696,
0.612376708364814));
#159218=CARTESIAN_POINT('Ctrl Pts',(-20.2994870261129,-20.3789735103839,
0.616764945096839));
#159219=CARTESIAN_POINT('Ctrl Pts',(-20.3476581043648,-20.3242534561182,
0.621153181828863));
#159220=CARTESIAN_POINT('Ctrl Pts',(-20.3928172134662,-20.2673001377284,
0.625541418560888));
#159221=CARTESIAN_POINT('Ctrl Pts',(-20.4234261206892,-20.2286970989766,
0.628515771546937));
#159222=CARTESIAN_POINT('Ctrl Pts',(-20.4526521510532,-20.189068732231,
0.631490124532986));
#159223=CARTESIAN_POINT('Ctrl Pts',(-20.4804290435443,-20.1485260531492,
0.634464477519035));
#159224=CARTESIAN_POINT('Ctrl Pts',(-20.5219871713971,-20.0878685177061,
0.638914526843781));
#159225=CARTESIAN_POINT('Ctrl Pts',(-20.5604589871816,-20.0249304539103,
0.643364576168526));
#159226=CARTESIAN_POINT('Ctrl Pts',(-20.5955899081637,-19.9600535768614,
0.647814625493272));
#159227=CARTESIAN_POINT('Ctrl Pts',(-20.6306645362352,-19.8952806569004,
0.652257544170088));
#159228=CARTESIAN_POINT('Ctrl Pts',(-20.6624086819058,-19.8285754984249,
0.656700462846903));
#159229=CARTESIAN_POINT('Ctrl Pts',(-20.6906106771651,-19.7603091351726,
0.661143381523719));
#159230=CARTESIAN_POINT('Ctrl Pts',(-20.7187693668652,-19.6921475982991,
0.665579477879059));
#159231=CARTESIAN_POINT('Ctrl Pts',(-20.7433965459121,-19.6224300506977,
0.670015574234399));
#159232=CARTESIAN_POINT('Ctrl Pts',(-20.7643269859574,-19.5515509403655,
0.674451670589739));
#159233=CARTESIAN_POINT('Ctrl Pts',(-20.7852384369126,-19.4807361349314,
0.678883742307599));
#159234=CARTESIAN_POINT('Ctrl Pts',(-20.8024596788638,-19.4087623035746,
0.683315814025459));
#159235=CARTESIAN_POINT('Ctrl Pts',(-20.8158743946738,-19.3360416706575,
0.687747885743319));
#159236=CARTESIAN_POINT('Ctrl Pts',(-20.8292815682241,-19.2633619240265,
0.692177465583092));
#159237=CARTESIAN_POINT('Ctrl Pts',(-20.8388863810041,-19.1899366656731,
0.696607045422866));
#159238=CARTESIAN_POINT('Ctrl Pts',(-20.8446233100443,-19.1161896558795,
0.70103662526264));
#159239=CARTESIAN_POINT('Ctrl Pts',(-20.8489003376003,-19.0612093709814,
0.704338990500929));
#159240=CARTESIAN_POINT('Ctrl Pts',(-20.8510286073489,-19.0060505461427,
0.707641355739218));
#159241=CARTESIAN_POINT('Ctrl Pts',(-20.8509997094775,-18.950890913829,
0.710943720977507));
#159242=CARTESIAN_POINT('',(-17.1140743056112,-17.5890877707427,0.));
#159243=CARTESIAN_POINT('Origin',(-18.734,-18.952,0.));
#159244=CARTESIAN_POINT('',(-20.8509993841888,-18.9503852727442,0.489056278967187));
#159245=CARTESIAN_POINT('Ctrl Pts',(-20.8509993841888,-18.9503852727442,
0.489056278967187));
#159246=CARTESIAN_POINT('Ctrl Pts',(-20.8510560136238,-19.0246296868351,
0.4845759098454));
#159247=CARTESIAN_POINT('Ctrl Pts',(-20.8472020786515,-19.0990185847436,
0.480095540723613));
#159248=CARTESIAN_POINT('Ctrl Pts',(-20.8394225353484,-19.1730994067089,
0.475615171601827));
#159249=CARTESIAN_POINT('Ctrl Pts',(-20.8319236706916,-19.2445074619042,
0.471296450007534));
#159250=CARTESIAN_POINT('Ctrl Pts',(-20.8207776586562,-19.315628743596,
0.466977728413241));
#159251=CARTESIAN_POINT('Ctrl Pts',(-20.8060239434695,-19.3860573437798,
0.462659006818948));
#159252=CARTESIAN_POINT('Ctrl Pts',(-20.7912800569942,-19.4564390254502,
0.458343162294427));
#159253=CARTESIAN_POINT('Ctrl Pts',(-20.7729333335852,-19.5261284557063,
0.454027317769906));
#159254=CARTESIAN_POINT('Ctrl Pts',(-20.7510747167063,-19.5947274595226,
0.449711473245385));
#159255=CARTESIAN_POINT('Ctrl Pts',(-20.729222990825,-19.6633048372874,
0.445396989304411));
#159256=CARTESIAN_POINT('Ctrl Pts',(-20.703861718916,-19.7307919977793,
0.441082505363437));
#159257=CARTESIAN_POINT('Ctrl Pts',(-20.6751318649418,-19.7968053520828,
0.436768021422464));
#159258=CARTESIAN_POINT('Ctrl Pts',(-20.6464009865417,-19.8628210602368,
0.43245338363913));
#159259=CARTESIAN_POINT('Ctrl Pts',(-20.6143014889206,-19.9273624038596,
0.428138745855796));
#159260=CARTESIAN_POINT('Ctrl Pts',(-20.5790219450864,-19.9900669641933,
0.423824108072462));
#159261=CARTESIAN_POINT('Ctrl Pts',(-20.5437075127064,-20.052833534142,
0.419505203469831));
#159262=CARTESIAN_POINT('Ctrl Pts',(-20.5052070056352,-20.1137592644334,
0.4151862988672));
#159263=CARTESIAN_POINT('Ctrl Pts',(-20.4637537424931,-20.1725084966239,
0.410867394264568));
#159264=CARTESIAN_POINT('Ctrl Pts',(-20.4222758241251,-20.2312926711924,
0.406545920899905));
#159265=CARTESIAN_POINT('Ctrl Pts',(-20.377841965069,-20.2878973842407,
0.402224447535242));
#159266=CARTESIAN_POINT('Ctrl Pts',(-20.3307256528942,-20.3420202118637,
0.397902974170579));
#159267=CARTESIAN_POINT('Ctrl Pts',(-20.2835347523397,-20.3962287196649,
0.393574659614792));
#159268=CARTESIAN_POINT('Ctrl Pts',(-20.2336532763038,-20.4479471527698,
0.389246345059005));
#159269=CARTESIAN_POINT('Ctrl Pts',(-20.1813905761972,-20.4969108453033,
0.384918030503218));
#159270=CARTESIAN_POINT('Ctrl Pts',(-20.1677438125197,-20.5096961767043,
0.383787827016913));
#159271=CARTESIAN_POINT('Ctrl Pts',(-20.153934855464,-20.5222939030973,
0.382657623530608));
#159272=CARTESIAN_POINT('Ctrl Pts',(-20.1399695482849,-20.534699791273,
0.381527420044303));
#159273=CARTESIAN_POINT('Ctrl Pts',(-20.0856805306588,-20.5829266919206,
0.37713384414925));
#159274=CARTESIAN_POINT('Ctrl Pts',(-20.0288042210984,-20.628448612849,
0.372740268254198));
#159275=CARTESIAN_POINT('Ctrl Pts',(-19.9696409341315,-20.6709765797994,
0.368346692359146));
#159276=CARTESIAN_POINT('Ctrl Pts',(-19.9105639454999,-20.7134425134696,
0.363959525139228));
#159277=CARTESIAN_POINT('Ctrl Pts',(-19.8492069897093,-20.7529228848839,
0.359572357919309));
#159278=CARTESIAN_POINT('Ctrl Pts',(-19.7859047362902,-20.7891677728967,
0.355185190699391));
#159279=CARTESIAN_POINT('Ctrl Pts',(-19.7226749495449,-20.8253711687614,
0.350803045787509));
#159280=CARTESIAN_POINT('Ctrl Pts',(-19.6575047045699,-20.8583462016275,
0.346420900875626));
#159281=CARTESIAN_POINT('Ctrl Pts',(-19.5907576513136,-20.8878861864571,
0.342038755963743));
#159282=CARTESIAN_POINT('Ctrl Pts',(-19.5240517390544,-20.9174079636751,
0.337659312082127));
#159283=CARTESIAN_POINT('Ctrl Pts',(-19.4557713858206,-20.9434987000513,
0.333279868200511));
#159284=CARTESIAN_POINT('Ctrl Pts',(-19.3863035870799,-20.9659982696822,
0.328900424318895));
#159285=CARTESIAN_POINT('Ctrl Pts',(-19.3168558633837,-20.9884913373096,
0.324522246024112));
#159286=CARTESIAN_POINT('Ctrl Pts',(-19.2462218327664,-21.0073951506619,
0.320144067729329));
#159287=CARTESIAN_POINT('Ctrl Pts',(-19.1748055877231,-21.0225988104488,
0.315765889434546));
#159288=CARTESIAN_POINT('Ctrl Pts',(-19.1033866007396,-21.0378030539619,
0.311387543044908));
#159289=CARTESIAN_POINT('Ctrl Pts',(-19.0311858104647,-21.0493067636484,
0.307009196655271));
#159290=CARTESIAN_POINT('Ctrl Pts',(-18.9586178566869,-21.0570500750475,
0.302630850265634));
#159291=CARTESIAN_POINT('Ctrl Pts',(-18.8859739522814,-21.0648014907037,
0.298247921437894));
#159292=CARTESIAN_POINT('Ctrl Pts',(-18.8129625963384,-21.0687845992062,
0.293864992610155));
#159293=CARTESIAN_POINT('Ctrl Pts',(-18.7400030989875,-21.0689914885995,
0.289482063782416));
#159294=CARTESIAN_POINT('Ctrl Pts',(-18.6670032476659,-21.0691984924235,
0.285096710752373));
#159295=CARTESIAN_POINT('Ctrl Pts',(-18.5940557926885,-21.0656251419751,
0.280711357722329));
#159296=CARTESIAN_POINT('Ctrl Pts',(-18.5215768813658,-21.0583156028169,
0.276326004692286));
#159297=CARTESIAN_POINT('Ctrl Pts',(-18.4489698822543,-21.0509931459328,
0.271932901681422));
#159298=CARTESIAN_POINT('Ctrl Pts',(-18.3768335560972,-21.039921387774,
0.267539798670557));
#159299=CARTESIAN_POINT('Ctrl Pts',(-18.3055752234049,-21.0251958930114,
0.263146695659693));
#159300=CARTESIAN_POINT('Ctrl Pts',(-18.258021675733,-21.0153689788707,
0.260215001560752));
#159301=CARTESIAN_POINT('Ctrl Pts',(-18.2108588965979,-21.0039159582902,
0.25728330746181));
#159302=CARTESIAN_POINT('Ctrl Pts',(-18.164203666426,-20.9908774210937,
0.254351613362869));
#159303=CARTESIAN_POINT('Ctrl Pts',(-18.0951064200439,-20.9715671098208,
0.250009720959284));
#159304=CARTESIAN_POINT('Ctrl Pts',(-18.0268407868783,-20.9486978630522,
0.245667828555699));
#159305=CARTESIAN_POINT('Ctrl Pts',(-17.9598054524231,-20.922358292926,
0.241325936152114));
#159306=CARTESIAN_POINT('Ctrl Pts',(-17.8928710627946,-20.8960583861112,
0.236990581965715));
#159307=CARTESIAN_POINT('Ctrl Pts',(-17.8271637514137,-20.8662987014601,
0.232655227779317));
#159308=CARTESIAN_POINT('Ctrl Pts',(-17.763068724128,-20.8332180781434,
0.228319873592918));
#159309=CARTESIAN_POINT('Ctrl Pts',(-17.699047363678,-20.8001754756366,
0.223989502192827));
#159310=CARTESIAN_POINT('Ctrl Pts',(-17.6366350451716,-20.7638197356247,
0.219659130792735));
#159311=CARTESIAN_POINT('Ctrl Pts',(-17.5761969042586,-20.7243377193672,
0.215328759392644));
#159312=CARTESIAN_POINT('Ctrl Pts',(-17.5157959073165,-20.6848799679007,
0.211001049344912));
#159313=CARTESIAN_POINT('Ctrl Pts',(-17.457367094634,-20.6423000184136,
0.206673339297181));
#159314=CARTESIAN_POINT('Ctrl Pts',(-17.4012494835622,-20.5968297969501,
0.202345629249449));
#159315=CARTESIAN_POINT('Ctrl Pts',(-17.3451469193491,-20.5513717674523,
0.198019079593976));
#159316=CARTESIAN_POINT('Ctrl Pts',(-17.2913547105839,-20.5030253137849,
0.193692529938503));
#159317=CARTESIAN_POINT('Ctrl Pts',(-17.2401799611388,-20.4520635624855,
0.18936598028303));
#159318=CARTESIAN_POINT('Ctrl Pts',(-17.1890012037485,-20.4010978199226,
0.185039091777358));
#159319=CARTESIAN_POINT('Ctrl Pts',(-17.1404406606225,-20.3475167229364,
0.180712203271685));
#159320=CARTESIAN_POINT('Ctrl Pts',(-17.0947683110377,-20.2916299749938,
0.176385314766013));
#159321=CARTESIAN_POINT('Ctrl Pts',(-17.0490411502534,-20.2356761575941,
0.172053233579186));
#159322=CARTESIAN_POINT('Ctrl Pts',(-17.0062094147358,-20.1774115489121,
0.167721152392358));
#159323=CARTESIAN_POINT('Ctrl Pts',(-16.9665019464716,-20.1171779395326,
0.16338907120553));
#159324=CARTESIAN_POINT('Ctrl Pts',(-16.9267699714228,-20.0569071549778,
0.159054316330717));
#159325=CARTESIAN_POINT('Ctrl Pts',(-16.8901663478009,-19.9946653786934,
0.154719561455904));
#159326=CARTESIAN_POINT('Ctrl Pts',(-16.8568742859376,-19.9308197247736,
0.150384806581091));
#159327=CARTESIAN_POINT('Ctrl Pts',(-16.8235151748393,-19.8668454875814,
0.146041321637236));
#159328=CARTESIAN_POINT('Ctrl Pts',(-16.793481145719,-19.8012613727176,
0.141697836693382));
#159329=CARTESIAN_POINT('Ctrl Pts',(-16.7669073048299,-19.7344546815047,
0.137354351749528));
#159330=CARTESIAN_POINT('Ctrl Pts',(-16.7461495461317,-19.6822696330047,
0.133961503393496));
#159331=CARTESIAN_POINT('Ctrl Pts',(-16.7275021235515,-19.6293390357121,
0.130568655037465));
#159332=CARTESIAN_POINT('Ctrl Pts',(-16.7110078198973,-19.5758522575445,
0.127175806681434));
#159333=CARTESIAN_POINT('Ctrl Pts',(-16.6890805816263,-19.5047478718232,
0.122665413525099));
#159334=CARTESIAN_POINT('Ctrl Pts',(-16.670871275646,-19.4323727566685,
0.118155020368764));
#159335=CARTESIAN_POINT('Ctrl Pts',(-16.6565191765188,-19.3591393226743,
0.113644627212429));
#159336=CARTESIAN_POINT('Ctrl Pts',(-16.641451763523,-19.2822559075513,
0.108909434411911));
#159337=CARTESIAN_POINT('Ctrl Pts',(-16.6306362897029,-19.2044268305763,
0.104174241611394));
#159338=CARTESIAN_POINT('Ctrl Pts',(-16.6241750766647,-19.1261487664996,
0.0994390488108757));
#159339=CARTESIAN_POINT('Ctrl Pts',(-16.618041066305,-19.0518347865785,
0.0949436511940506));
#159340=CARTESIAN_POINT('Ctrl Pts',(-16.6158311203138,-18.9771167035359,
0.0904482535772255));
#159341=CARTESIAN_POINT('Ctrl Pts',(-16.6175804393308,-18.9024294117756,
0.0859528559604003));
#159342=CARTESIAN_POINT('Ctrl Pts',(-16.6193281134804,-18.8278123477383,
0.0814616853215709));
#159343=CARTESIAN_POINT('Ctrl Pts',(-16.6250276422425,-18.7532264655291,
0.0769705146827415));
#159344=CARTESIAN_POINT('Ctrl Pts',(-16.6346622154624,-18.6791083247648,
0.0724793440439121));
#159345=CARTESIAN_POINT('Ctrl Pts',(-16.6442902465126,-18.6050405124837,
0.0679912230472238));
#159346=CARTESIAN_POINT('Ctrl Pts',(-16.6578479512151,-18.5314402553688,
0.0635031020505355));
#159347=CARTESIAN_POINT('Ctrl Pts',(-16.6752666606882,-18.458739381659,
0.0590149810538472));
#159348=CARTESIAN_POINT('Ctrl Pts',(-16.6926780888339,-18.3860688981953,
0.0545287361708016));
#159349=CARTESIAN_POINT('Ctrl Pts',(-16.7139472060124,-18.3142974872696,
0.0500424912877559));
#159350=CARTESIAN_POINT('Ctrl Pts',(-16.738954437569,-18.2438459180203,
0.0455562464047103));
#159351=CARTESIAN_POINT('Ctrl Pts',(-16.7639647762088,-18.1733855953477,
0.0410694441174684));
#159352=CARTESIAN_POINT('Ctrl Pts',(-16.7927140135935,-18.1042458686283,
0.0365826418302264));
#159353=CARTESIAN_POINT('Ctrl Pts',(-16.8250332584604,-18.0368306278641,
0.0320958395429845));
#159354=CARTESIAN_POINT('Ctrl Pts',(-16.8573540573157,-17.9694121456102,
0.0276088215193051));
#159355=CARTESIAN_POINT('Ctrl Pts',(-16.893245003916,-17.9037187169574,
0.0231218034956257));
#159356=CARTESIAN_POINT('Ctrl Pts',(-16.9324905209222,-17.8401310343422,
0.0186347854719464));
#159357=CARTESIAN_POINT('Ctrl Pts',(-16.971763121732,-17.776499469102,0.0141446709031355));
#159358=CARTESIAN_POINT('Ctrl Pts',(-17.0143946720501,-17.7149769304511,
0.00965455633432465));
#159359=CARTESIAN_POINT('Ctrl Pts',(-17.0601258387639,-17.65591578501,0.00516444176551379));
#159360=CARTESIAN_POINT('Ctrl Pts',(-17.0776588692871,-17.6332721277373,
0.00344296117700913));
#159361=CARTESIAN_POINT('Ctrl Pts',(-17.0956470822643,-17.6109899387145,
0.00172148058850446));
#159362=CARTESIAN_POINT('Ctrl Pts',(-17.1140743056112,-17.5890877707427,
-2.02192933296002E-16));
#159363=CARTESIAN_POINT('Ctrl Pts',(-20.8509994311265,-18.9504480302426,
0.490010487033197));
#159364=CARTESIAN_POINT('Ctrl Pts',(-20.8509485264066,-18.8810102963088,
0.494577353552967));
#159365=CARTESIAN_POINT('Ctrl Pts',(-20.8474812861683,-18.8116101392654,
0.499099022991477));
#159366=CARTESIAN_POINT('Ctrl Pts',(-20.8382974724733,-18.7192631654625,
0.504962284114916));
#159367=CARTESIAN_POINT('Ctrl Pts',(-20.835602182128,-18.6960651320075,
0.506421988151869));
#159368=CARTESIAN_POINT('Ctrl Pts',(-20.831714710083,-18.6668340267685,
0.508240727451452));
#159369=CARTESIAN_POINT('Ctrl Pts',(-20.8308795002837,-18.6607561149905,
0.508617762711525));
#159370=CARTESIAN_POINT('Ctrl Pts',(-20.8294396311101,-18.6506054014144,
0.509245465875726));
#159371=CARTESIAN_POINT('Ctrl Pts',(-20.8288494962058,-18.6465306225147,
0.509496908631013));
#159372=CARTESIAN_POINT('Ctrl Pts',(-20.8277537529322,-18.6391172367348,
0.509953361381631));
#159373=CARTESIAN_POINT('Ctrl Pts',(-20.8272520391161,-18.6357780801865,
0.510158586227083));
#159374=CARTESIAN_POINT('Ctrl Pts',(-20.8262054025295,-18.6289238385501,
0.510579064774858));
#159375=CARTESIAN_POINT('Ctrl Pts',(-20.8256596119141,-18.6254089394044,
0.510794262175057));
#159376=CARTESIAN_POINT('Ctrl Pts',(-20.8244066763097,-18.6174720023468,
0.511279232147259));
#159377=CARTESIAN_POINT('Ctrl Pts',(-20.8236943601969,-18.6130508365728,
0.511548707398385));
#159378=CARTESIAN_POINT('Ctrl Pts',(-20.821498981492,-18.5996946857722,
0.512360842528697));
#159379=CARTESIAN_POINT('Ctrl Pts',(-20.8199725808866,-18.590766791922,
0.512901088674201));
#159380=CARTESIAN_POINT('Ctrl Pts',(-20.8078179693633,-18.5223219602975,
0.517024578341899));
#159381=CARTESIAN_POINT('Ctrl Pts',(-20.7947008199896,-18.4632692387237,
0.520476395378648));
#159382=CARTESIAN_POINT('Ctrl Pts',(-20.7741834180103,-18.3865812121723,
0.524914225206502));
#159383=CARTESIAN_POINT('Ctrl Pts',(-20.7690499488155,-18.3683746774345,
0.525964408236979));
#159384=CARTESIAN_POINT('Ctrl Pts',(-20.7520366525769,-18.3109907112767,
0.52927032329694));
#159385=CARTESIAN_POINT('Ctrl Pts',(-20.7392639646607,-18.2720871905213,
0.53150561845119));
#159386=CARTESIAN_POINT('Ctrl Pts',(-20.7244457869367,-18.231013174881,
0.533880934072488));
#159387=CARTESIAN_POINT('Ctrl Pts',(-20.7235156490763,-18.2284504754409,
0.534029198950805));
#159388=CARTESIAN_POINT('Ctrl Pts',(-20.7225805737341,-18.2258896077265,
0.534177427254548));
#159389=CARTESIAN_POINT('Origin',(-18.734,-18.952,0.));
#159390=CARTESIAN_POINT('',(-20.7225805817976,-18.2258896298098,1.55576077259463));
#159391=CARTESIAN_POINT('',(-20.7225805737606,-18.2258896077991,1.33163200235201));
#159392=CARTESIAN_POINT('',(-20.7225805737622,-18.2258896078036,0.));
#159393=CARTESIAN_POINT('',(-20.8509996091575,-18.9507135992268,1.51094372094299));
#159394=CARTESIAN_POINT('Ctrl Pts',(-20.7225805817976,-18.2258896298098,
1.55576077259462));
#159395=CARTESIAN_POINT('Ctrl Pts',(-20.7518710589646,-18.3061067380035,
1.55012867077602));
#159396=CARTESIAN_POINT('Ctrl Pts',(-20.7762853815704,-18.38803479713,1.54445865839829));
#159397=CARTESIAN_POINT('Ctrl Pts',(-20.8019773168351,-18.4982088405443,
1.53708130683603));
#159398=CARTESIAN_POINT('Ctrl Pts',(-20.8077392211968,-18.5253123572864,
1.53528617643754));
#159399=CARTESIAN_POINT('Ctrl Pts',(-20.8211288647775,-18.5949948853297,
1.53073317031627));
#159400=CARTESIAN_POINT('Ctrl Pts',(-20.8279872923736,-18.6377113451497,
1.52800101026692));
#159401=CARTESIAN_POINT('Ctrl Pts',(-20.8344943172588,-18.6880513212877,
1.52487280887383));
#159402=CARTESIAN_POINT('Ctrl Pts',(-20.8354165122709,-18.6954967298112,
1.5244124814161));
#159403=CARTESIAN_POINT('Ctrl Pts',(-20.83684279883,-18.7075362599162,1.52367206636053));
#159404=CARTESIAN_POINT('Ctrl Pts',(-20.837371450688,-18.7121273292504,
1.52339064936815));
#159405=CARTESIAN_POINT('Ctrl Pts',(-20.8382824834223,-18.7202738327017,
1.52289298567027));
#159406=CARTESIAN_POINT('Ctrl Pts',(-20.8386708938216,-18.7238285380895,
1.52267640342196));
#159407=CARTESIAN_POINT('Ctrl Pts',(-20.8394063446568,-18.7307210257532,
1.52225757315985));
#159408=CARTESIAN_POINT('Ctrl Pts',(-20.8397544538287,-18.7340586292005,
1.52205526370317));
#159409=CARTESIAN_POINT('Ctrl Pts',(-20.8405037110542,-18.7414117750289,
1.52161063359276));
#159410=CARTESIAN_POINT('Ctrl Pts',(-20.8409013172897,-18.7454276761205,
1.5213685104107));
#159411=CARTESIAN_POINT('Ctrl Pts',(-20.8418560160587,-18.7553599020115,
1.52077138728864));
#159412=CARTESIAN_POINT('Ctrl Pts',(-20.842399689606,-18.7612775228126,
1.5204171133863));
#159413=CARTESIAN_POINT('Ctrl Pts',(-20.8445839011712,-18.786203172463,
1.51893086032492));
#159414=CARTESIAN_POINT('Ctrl Pts',(-20.8459924220239,-18.8052312825265,
1.51781091036615));
#159415=CARTESIAN_POINT('Ctrl Pts',(-20.8496863090444,-18.866345457104,
1.51425344004809));
#159416=CARTESIAN_POINT('Ctrl Pts',(-20.8509723412788,-18.9084830968548,
1.51186063670684));
#159417=CARTESIAN_POINT('Ctrl Pts',(-20.8509995586432,-18.950632994338,
1.50950279134391));
#159418=CARTESIAN_POINT('Ctrl Pts',(-20.7225805737622,-18.2258896078036,
0.755484073133953));
#159419=CARTESIAN_POINT('Ctrl Pts',(-20.7109390354868,-18.1940072148343,
0.757536143489459));
#159420=CARTESIAN_POINT('Ctrl Pts',(-20.6985367298582,-18.1624215432055,
0.759588213844964));
#159421=CARTESIAN_POINT('Ctrl Pts',(-20.6853897265628,-18.1311668043596,
0.761640284200469));
#159422=CARTESIAN_POINT('Ctrl Pts',(-20.6572744224869,-18.0643275051887,
0.766028704948043));
#159423=CARTESIAN_POINT('Ctrl Pts',(-20.6256662206413,-17.9988040174836,
0.770417125695617));
#159424=CARTESIAN_POINT('Ctrl Pts',(-20.5907099139161,-17.9349860888043,
0.774805546443191));
#159425=CARTESIAN_POINT('Ctrl Pts',(-20.555805473251,-17.8712628493194,
0.779187455916675));
#159426=CARTESIAN_POINT('Ctrl Pts',(-20.5175630191303,-17.8092405647745,
0.78356936539016));
#159427=CARTESIAN_POINT('Ctrl Pts',(-20.4761752495541,-17.7492887296441,
0.787951274863645));
#159428=CARTESIAN_POINT('Ctrl Pts',(-20.4348360994882,-17.6894073218137,
0.792328036770722));
#159429=CARTESIAN_POINT('Ctrl Pts',(-20.3903592465927,-17.631591926717,
0.796704798677799));
#159430=CARTESIAN_POINT('Ctrl Pts',(-20.3429822557086,-17.5761856590314,
0.801081560584876));
#159431=CARTESIAN_POINT('Ctrl Pts',(-20.2956353018765,-17.5208145189661,
0.805455547621227));
#159432=CARTESIAN_POINT('Ctrl Pts',(-20.2453921709553,-17.4678498414426,
0.809829534657577));
#159433=CARTESIAN_POINT('Ctrl Pts',(-20.192531655455,-17.4176029164406,
0.814203521693928));
#159434=CARTESIAN_POINT('Ctrl Pts',(-20.1396872205098,-17.3673712769204,
0.818576178131455));
#159435=CARTESIAN_POINT('Ctrl Pts',(-20.084227331126,-17.3198560806449,
0.822948834568982));
#159436=CARTESIAN_POINT('Ctrl Pts',(-20.0264675214797,-17.2753316649021,
0.827321491006509));
#159437=CARTESIAN_POINT('Ctrl Pts',(-19.9687062344823,-17.2308061103364,
0.831694259285623));
#159438=CARTESIAN_POINT('Ctrl Pts',(-19.9086452936504,-17.1892717810647,
0.836067027564738));
#159439=CARTESIAN_POINT('Ctrl Pts',(-19.8466318410332,-17.1509615811096,
0.840439795843852));
#159440=CARTESIAN_POINT('Ctrl Pts',(-19.7845540522246,-17.1126116360308,
0.844817100675033));
#159441=CARTESIAN_POINT('Ctrl Pts',(-19.720520118509,-17.0774927526079,
0.849194405506214));
#159442=CARTESIAN_POINT('Ctrl Pts',(-19.6549038734621,-17.0457930186251,
0.853571710337395));
#159443=CARTESIAN_POINT('Ctrl Pts',(-19.5892518018729,-17.0140759765525,
0.85795140518185));
#159444=CARTESIAN_POINT('Ctrl Pts',(-19.5220161437134,-16.9857819880477,
0.862331100026305));
#159445=CARTESIAN_POINT('Ctrl Pts',(-19.4535904002058,-16.9610508153316,
0.86671079487076));
#159446=CARTESIAN_POINT('Ctrl Pts',(-19.3850434278267,-16.9362758267649,
0.871098249155392));
#159447=CARTESIAN_POINT('Ctrl Pts',(-19.3153026214752,-16.915076399583,
0.875485703440023));
#159448=CARTESIAN_POINT('Ctrl Pts',(-19.2447757398887,-16.897542129042,
0.879873157724655));
#159449=CARTESIAN_POINT('Ctrl Pts',(-19.1968575055399,-16.8856287810247,
0.882854135443738));
#159450=CARTESIAN_POINT('Ctrl Pts',(-19.1485766460487,-16.8754063073494,
0.885835113162821));
#159451=CARTESIAN_POINT('Ctrl Pts',(-19.1000625448657,-16.866889160441,
0.888816090881904));
#159452=CARTESIAN_POINT('Ctrl Pts',(-19.028644802906,-16.8543510450208,
0.8932043963918));
#159453=CARTESIAN_POINT('Ctrl Pts',(-18.9564428168485,-16.8454619385439,
0.897592701901696));
#159454=CARTESIAN_POINT('Ctrl Pts',(-18.8838626572346,-16.8403110588994,
0.901981007411591));
#159455=CARTESIAN_POINT('Ctrl Pts',(-18.8113901761429,-16.8351678210004,
0.906362802516231));
#159456=CARTESIAN_POINT('Ctrl Pts',(-18.7385411124288,-16.8337518342884,
0.910744597620871));
#159457=CARTESIAN_POINT('Ctrl Pts',(-18.6657304379547,-16.8361010735628,
0.915126392725512));
#159458=CARTESIAN_POINT('Ctrl Pts',(-18.5930052675323,-16.8384475540456,
0.919503042139114));
#159459=CARTESIAN_POINT('Ctrl Pts',(-18.5203188765061,-16.8445504614284,
0.923879691552716));
#159460=CARTESIAN_POINT('Ctrl Pts',(-18.4480883417813,-16.854395765714,
0.928256340966318));
#159461=CARTESIAN_POINT('Ctrl Pts',(-18.3759035823937,-16.8642348306421,
0.932630216724654));
#159462=CARTESIAN_POINT('Ctrl Pts',(-18.3041745828625,-16.8778115217113,
0.937004092482989));
#159463=CARTESIAN_POINT('Ctrl Pts',(-18.2333139763946,-16.8950599168264,
0.941377968241324));
#159464=CARTESIAN_POINT('Ctrl Pts',(-18.1624749043755,-16.912303070176,
0.945750514784348));
#159465=CARTESIAN_POINT('Ctrl Pts',(-18.092504169876,-16.9332155982964,
0.950123061327371));
#159466=CARTESIAN_POINT('Ctrl Pts',(-18.0238032220047,-16.9576806834097,
0.954495607870394));
#159467=CARTESIAN_POINT('Ctrl Pts',(-17.9551004924925,-16.9821464029829,
0.958868267807887));
#159468=CARTESIAN_POINT('Ctrl Pts',(-17.8876680687169,-17.0101646987635,
0.96324092774538));
#159469=CARTESIAN_POINT('Ctrl Pts',(-17.8218896690581,-17.0415697489338,
0.967613587682873));
#159470=CARTESIAN_POINT('Ctrl Pts',(-17.7560429779044,-17.0730074039992,
0.971990787339865));
#159471=CARTESIAN_POINT('Ctrl Pts',(-17.6918541756222,-17.1078386254076,
0.976367986996856));
#159472=CARTESIAN_POINT('Ctrl Pts',(-17.6296837442221,-17.1458508900911,
0.980745186653848));
#159473=CARTESIAN_POINT('Ctrl Pts',(-17.5674793440156,-17.183883923993,
0.985124777934071));
#159474=CARTESIAN_POINT('Ctrl Pts',(-17.5072959086028,-17.2251011888991,
0.989504369214295));
#159475=CARTESIAN_POINT('Ctrl Pts',(-17.4494639302801,-17.2692474675138,
0.993883960494518));
#159476=CARTESIAN_POINT('Ctrl Pts',(-17.391529439673,-17.3134719993027,
0.99827131498672));
#159477=CARTESIAN_POINT('Ctrl Pts',(-17.3359550979025,-17.3606356005002,
1.00265866947892));
#159478=CARTESIAN_POINT('Ctrl Pts',(-17.2830369310415,-17.4104439119777,
1.00704602397112));
#159479=CARTESIAN_POINT('Ctrl Pts',(-17.2470699846496,-17.4442971796748,
1.01002798183519));
#159480=CARTESIAN_POINT('Ctrl Pts',(-17.2123293049363,-17.4793713923189,
1.01300993969927));
#159481=CARTESIAN_POINT('Ctrl Pts',(-17.1788971548152,-17.5155654762927,
1.01599189756334));
#159482=CARTESIAN_POINT('Ctrl Pts',(-17.1297001020368,-17.568826850541,
1.02037999518465));
#159483=CARTESIAN_POINT('Ctrl Pts',(-17.083146390969,-17.6247226231684,
1.02476809280597));
#159484=CARTESIAN_POINT('Ctrl Pts',(-17.0395308428605,-17.6829597029633,
1.02915619042728));
#159485=CARTESIAN_POINT('Ctrl Pts',(-16.9959800467907,-17.741110323461,
1.03353777343903));
#159486=CARTESIAN_POINT('Ctrl Pts',(-16.9553590412718,-17.8015949680233,
1.03791935645078));
#159487=CARTESIAN_POINT('Ctrl Pts',(-16.9179243827548,-17.8640853193162,
1.04230093946253));
#159488=CARTESIAN_POINT('Ctrl Pts',(-16.8805337321229,-17.926502207452,
1.04667737152035));
#159489=CARTESIAN_POINT('Ctrl Pts',(-16.8463222340327,-17.9909197065767,
1.05105380357816));
#159490=CARTESIAN_POINT('Ctrl Pts',(-16.8155038596719,-18.0569795759055,
1.05543023563597));
#159491=CARTESIAN_POINT('Ctrl Pts',(-16.7847050391281,-18.1229975311937,
1.05980389091035));
#159492=CARTESIAN_POINT('Ctrl Pts',(-16.7572952741608,-18.1906553530113,
1.06417754618474));
#159493=CARTESIAN_POINT('Ctrl Pts',(-16.7334425000676,-18.259570444403,
1.06855120145912));
#159494=CARTESIAN_POINT('Ctrl Pts',(-16.7095969904912,-18.3284645472576,
1.07292352470848));
#159495=CARTESIAN_POINT('Ctrl Pts',(-16.6893064787907,-18.3986147038968,
1.07729584795784));
#159496=CARTESIAN_POINT('Ctrl Pts',(-16.6726900528573,-18.4696201685282,
1.0816681712072));
#159497=CARTESIAN_POINT('Ctrl Pts',(-16.6560732054628,-18.5406274341515,
1.08604060535674));
#159498=CARTESIAN_POINT('Ctrl Pts',(-16.6431307368287,-18.6124895806671,
1.09041303950627));
#159499=CARTESIAN_POINT('Ctrl Pts',(-16.6339309337084,-18.6847942425672,
1.09478547365581));
#159500=CARTESIAN_POINT('Ctrl Pts',(-16.6247215836389,-18.7571739374787,
1.09916244522925));
#159501=CARTESIAN_POINT('Ctrl Pts',(-16.6192627145554,-18.8299965850532,
1.10353941680269));
#159502=CARTESIAN_POINT('Ctrl Pts',(-16.617570767733,-18.9028440765969,
1.10791638837613));
#159503=CARTESIAN_POINT('Ctrl Pts',(-16.6158778970465,-18.9757313455016,
1.1122957499341));
#159504=CARTESIAN_POINT('Ctrl Pts',(-16.6179560300807,-19.0486430028401,
1.11667511149208));
#159505=CARTESIAN_POINT('Ctrl Pts',(-16.6237694760295,-19.1211630447324,
1.12105447305006));
#159506=CARTESIAN_POINT('Ctrl Pts',(-16.6295932272271,-19.1938116398244,
1.12544159771636));
#159507=CARTESIAN_POINT('Ctrl Pts',(-16.6391654506535,-19.2660667545322,
1.12982872238266));
#159508=CARTESIAN_POINT('Ctrl Pts',(-16.6523988871432,-19.3375201771025,
1.13421584704896));
#159509=CARTESIAN_POINT('Ctrl Pts',(-16.6613997584561,-19.3861200295993,
1.13719979944756));
#159510=CARTESIAN_POINT('Ctrl Pts',(-16.6720933047965,-19.43434921752,1.14018375184616));
#159511=CARTESIAN_POINT('Ctrl Pts',(-16.6844389804884,-19.482083604065,
1.14316770424477));
#159512=CARTESIAN_POINT('Ctrl Pts',(-16.7025947176038,-19.552282513797,
1.14755594970543));
#159513=CARTESIAN_POINT('Ctrl Pts',(-16.7243966050156,-19.6216845828659,
1.1519441951661));
#159514=CARTESIAN_POINT('Ctrl Pts',(-16.7497577488962,-19.6898832488508,
1.15633244062676));
#159515=CARTESIAN_POINT('Ctrl Pts',(-16.7750812549564,-19.757980702952,
1.16071417360537));
#159516=CARTESIAN_POINT('Ctrl Pts',(-16.8039533648488,-19.8248778509223,
1.16509590658397));
#159517=CARTESIAN_POINT('Ctrl Pts',(-16.8362368540352,-19.8901812414549,
1.16947763956257));
#159518=CARTESIAN_POINT('Ctrl Pts',(-16.8684824103679,-19.9554079010014,
1.17385422403833));
#159519=CARTESIAN_POINT('Ctrl Pts',(-16.9041311706798,-20.0190440928805,
1.17823080851409));
#159520=CARTESIAN_POINT('Ctrl Pts',(-16.9429977000799,-20.080715979191,
1.18260739298985));
#159521=CARTESIAN_POINT('Ctrl Pts',(-16.9818395827806,-20.1423487570843,
1.186981202112));
#159522=CARTESIAN_POINT('Ctrl Pts',(-17.0238949293876,-20.2020192938346,
1.19135501123416));
#159523=CARTESIAN_POINT('Ctrl Pts',(-17.0689329083319,-20.2593792794151,
1.19572882035631));
#159524=CARTESIAN_POINT('Ctrl Pts',(-17.1139571835667,-20.316721812068,
1.2001012986592));
#159525=CARTESIAN_POINT('Ctrl Pts',(-17.1619619917057,-20.371754810121,
1.20447377696209));
#159526=CARTESIAN_POINT('Ctrl Pts',(-17.2126748020944,-20.4241612147512,
1.20884625526498));
#159527=CARTESIAN_POINT('Ctrl Pts',(-17.2633889101253,-20.4765689603592,
1.21321884545108));
#159528=CARTESIAN_POINT('Ctrl Pts',(-17.316810821104,-20.5263496338558,
1.21759143563718));
#159529=CARTESIAN_POINT('Ctrl Pts',(-17.3726307376193,-20.5732226039151,
1.22196402582327));
#159530=CARTESIAN_POINT('Ctrl Pts',(-17.4285085838715,-20.6201442185978,
1.22634115386995));
#159531=CARTESIAN_POINT('Ctrl Pts',(-17.4867890342101,-20.6641517941318,
1.23071828191663));
#159532=CARTESIAN_POINT('Ctrl Pts',(-17.5471294002341,-20.7050051852209,
1.23509540996331));
#159533=CARTESIAN_POINT('Ctrl Pts',(-17.607502719815,-20.7458808874863,
1.23947492848171));
#159534=CARTESIAN_POINT('Ctrl Pts',(-17.6699377817392,-20.7835987260512,
1.24385444700011));
#159535=CARTESIAN_POINT('Ctrl Pts',(-17.7340654500449,-20.8179635301383,
1.24823396551851));
#159536=CARTESIAN_POINT('Ctrl Pts',(-17.7983067766523,-20.8523892415588,
1.2526212461878));
#159537=CARTESIAN_POINT('Ctrl Pts',(-17.864246263625,-20.8834498451619,
1.25700852685708));
#159538=CARTESIAN_POINT('Ctrl Pts',(-17.9314934145806,-20.9109977489417,
1.26139580752637));
#159539=CARTESIAN_POINT('Ctrl Pts',(-17.9772094747549,-20.9297254066785,
1.26437837532632));
#159540=CARTESIAN_POINT('Ctrl Pts',(-18.0235294804888,-20.9468306624838,
1.26736094312626));
#159541=CARTESIAN_POINT('Ctrl Pts',(-18.070327288212,-20.9622804609377,
1.27034351092621));
#159542=CARTESIAN_POINT('Ctrl Pts',(-18.1391803753322,-20.9850115752931,
1.27473172931853));
#159543=CARTESIAN_POINT('Ctrl Pts',(-18.2093370332052,-21.0042455878006,
1.27911994771086));
#159544=CARTESIAN_POINT('Ctrl Pts',(-18.2804083784674,-21.0198354965701,
1.28350816610318));
#159545=CARTESIAN_POINT('Ctrl Pts',(-18.3513742469025,-21.0354022683904,
1.28788987195026));
#159546=CARTESIAN_POINT('Ctrl Pts',(-18.4232516406539,-21.0473355700023,
1.29227157779733));
#159547=CARTESIAN_POINT('Ctrl Pts',(-18.4956354572704,-21.0555378163393,
1.2966532836444));
#159548=CARTESIAN_POINT('Ctrl Pts',(-18.5679342235899,-21.0637304251147,
1.30102984102871));
#159549=CARTESIAN_POINT('Ctrl Pts',(-18.6407377537903,-21.068200633326,
1.30540639841303));
#159550=CARTESIAN_POINT('Ctrl Pts',(-18.7136313414975,-21.0689020094824,
1.30978295579735));
#159551=CARTESIAN_POINT('Ctrl Pts',(-18.7864787050571,-21.0696029408739,
1.31415673786712));
#159552=CARTESIAN_POINT('Ctrl Pts',(-18.8594155316466,-21.0665397775258,
1.31853051993688));
#159553=CARTESIAN_POINT('Ctrl Pts',(-18.9320240071873,-21.0597180771103,
1.32290430200665));
#159554=CARTESIAN_POINT('Ctrl Pts',(-19.0046103913194,-21.0528984522235,
1.32727675333636));
#159555=CARTESIAN_POINT('Ctrl Pts',(-19.0768681427674,-21.0423226056621,
1.33164920466608));
#159556=CARTESIAN_POINT('Ctrl Pts',(-19.1483831536915,-21.0280480731276,
1.33602165599579));
#159557=CARTESIAN_POINT('Ctrl Pts',(-19.2198999965103,-21.0137731749434,
1.34039421932815));
#159558=CARTESIAN_POINT('Ctrl Pts',(-19.290673588379,-20.9957994990627,
1.3447667826605));
#159559=CARTESIAN_POINT('Ctrl Pts',(-19.3603002793689,-20.974235634159,
1.34913934599286));
#159560=CARTESIAN_POINT('Ctrl Pts',(-19.4299992351055,-20.9526493883664,
1.35351644755872));
#159561=CARTESIAN_POINT('Ctrl Pts',(-19.4985484515708,-20.9274656569225,
1.35789354912458));
#159562=CARTESIAN_POINT('Ctrl Pts',(-19.5655605178868,-20.8988425989514,
1.36227065069045));
#159563=CARTESIAN_POINT('Ctrl Pts',(-19.6326091841496,-20.870203907939,
1.36665014289569));
#159564=CARTESIAN_POINT('Ctrl Pts',(-19.6981185952225,-20.8381223627168,
1.37102963510093));
#159565=CARTESIAN_POINT('Ctrl Pts',(-19.7617248412387,-20.8028027044234,
1.37540912730617));
#159566=CARTESIAN_POINT('Ctrl Pts',(-19.8254438302969,-20.7674204414965,
1.3797963822282));
#159567=CARTESIAN_POINT('Ctrl Pts',(-19.8872525083671,-20.7287888596301,
1.38418363715023));
#159568=CARTESIAN_POINT('Ctrl Pts',(-19.9468154099209,-20.6871564141191,
1.38857089207226));
#159569=CARTESIAN_POINT('Ctrl Pts',(-19.987311057632,-20.658851331546,1.39155370058405));
#159570=CARTESIAN_POINT('Ctrl Pts',(-20.0267692625344,-20.6291600259051,
1.39453650909585));
#159571=CARTESIAN_POINT('Ctrl Pts',(-20.0650939279425,-20.5981706943675,
1.39751931760764));
#159572=CARTESIAN_POINT('Ctrl Pts',(-20.1207402990933,-20.5531750283627,
1.40185027438838));
#159573=CARTESIAN_POINT('Ctrl Pts',(-20.1742249030448,-20.5052554319719,
1.40618123116912));
#159574=CARTESIAN_POINT('Ctrl Pts',(-20.225218155009,-20.4546501303269,
1.41051218794986));
#159575=CARTESIAN_POINT('Ctrl Pts',(-20.2761246583685,-20.4041309173141,
1.41483577700167));
#159576=CARTESIAN_POINT('Ctrl Pts',(-20.3245478764186,-20.3509354173609,
1.41915936605348));
#159577=CARTESIAN_POINT('Ctrl Pts',(-20.3701907266811,-20.295342438071,
1.42348295510528));
#159578=CARTESIAN_POINT('Ctrl Pts',(-20.4157901278605,-20.2398023797527,
1.427802428376));
#159579=CARTESIAN_POINT('Ctrl Pts',(-20.458614094256,-20.1818697469968,
1.43212190164671));
#159580=CARTESIAN_POINT('Ctrl Pts',(-20.4984028920068,-20.1218595790427,
1.43644137491742));
#159581=CARTESIAN_POINT('Ctrl Pts',(-20.5381677540013,-20.0618855114193,
1.44075824972159));
#159582=CARTESIAN_POINT('Ctrl Pts',(-20.5749007945914,-19.9998367995591,
1.44507512452575));
#159583=CARTESIAN_POINT('Ctrl Pts',(-20.6083841897886,-19.9360594032226,
1.44939199932992));
#159584=CARTESIAN_POINT('Ctrl Pts',(-20.6418591711516,-19.8722980331112,
1.45370778937347));
#159585=CARTESIAN_POINT('Ctrl Pts',(-20.6720858980915,-19.806809280176,
1.45802357941702));
#159586=CARTESIAN_POINT('Ctrl Pts',(-20.6988922427438,-19.7399641326896,
1.46233936946057));
#159587=CARTESIAN_POINT('Ctrl Pts',(-20.7257171905672,-19.6730725957484,
1.46665815459285));
#159588=CARTESIAN_POINT('Ctrl Pts',(-20.7491168267536,-19.6048232442395,
1.47097693972513));
#159589=CARTESIAN_POINT('Ctrl Pts',(-20.7689674510093,-19.5356064370212,
1.4752957248574));
#159590=CARTESIAN_POINT('Ctrl Pts',(-20.788824843842,-19.4663660285662,
1.47961598258968));
#159591=CARTESIAN_POINT('Ctrl Pts',(-20.8051307004056,-19.3961579909125,
1.48393624032195));
#159592=CARTESIAN_POINT('Ctrl Pts',(-20.8178121270028,-19.3253845462204,
1.48825649805423));
#159593=CARTESIAN_POINT('Ctrl Pts',(-20.8305133198985,-19.2545007883054,
1.49258348969011));
#159594=CARTESIAN_POINT('Ctrl Pts',(-20.8395787374245,-19.1830503562126,
1.49691048132598));
#159595=CARTESIAN_POINT('Ctrl Pts',(-20.8449873094553,-19.111441460476,
1.50123747296186));
#159596=CARTESIAN_POINT('Ctrl Pts',(-20.8490314541924,-19.0578974312625,
1.50447288895557));
#159597=CARTESIAN_POINT('Ctrl Pts',(-20.8510321497761,-19.0042649326901,
1.50770830494928));
#159598=CARTESIAN_POINT('Ctrl Pts',(-20.8509996091575,-18.9507135992268,
1.51094372094299));
#159599=CARTESIAN_POINT('Ctrl Pts',(-20.7225805737341,-18.2258896077265,
0.534177427254548));
#159600=CARTESIAN_POINT('Ctrl Pts',(-20.7114372979688,-18.1953717939748,
0.535943861241366));
#159601=CARTESIAN_POINT('Ctrl Pts',(-20.6995928300724,-18.1651141152618,
0.537705172282633));
#159602=CARTESIAN_POINT('Ctrl Pts',(-20.6589739959127,-18.0679971802694,
0.543420718962302));
#159603=CARTESIAN_POINT('Ctrl Pts',(-20.6274486114839,-18.0023487123035,
0.547383506222511));
#159604=CARTESIAN_POINT('Ctrl Pts',(-20.5661675725758,-17.8899733527578,
0.554496467580431));
#159605=CARTESIAN_POINT('Ctrl Pts',(-20.5378433424897,-17.8425464601804,
0.557608819686519));
#159606=CARTESIAN_POINT('Ctrl Pts',(-20.4889702401542,-17.7675400396367,
0.562757567744392));
#159607=CARTESIAN_POINT('Ctrl Pts',(-20.4695464598254,-17.7392575584176,
0.564754091830704));
#159608=CARTESIAN_POINT('Ctrl Pts',(-20.4431385100701,-17.7027400704759,
0.567411422912495));
#159609=CARTESIAN_POINT('Ctrl Pts',(-20.4367658473403,-17.694067855273,
0.568048536260424));
#159610=CARTESIAN_POINT('Ctrl Pts',(-20.4262255985486,-17.6799510508294,
0.569095773986359));
#159611=CARTESIAN_POINT('Ctrl Pts',(-20.4220971448156,-17.6744773843787,
0.569504357168897));
#159612=CARTESIAN_POINT('Ctrl Pts',(-20.41405836778,-17.6639262632964,0.570296901135609));
#159613=CARTESIAN_POINT('Ctrl Pts',(-20.4101514297622,-17.6588463148452,
0.570680724869242));
#159614=CARTESIAN_POINT('Ctrl Pts',(-20.4010835361084,-17.647166032395,
0.571568488047005));
#159615=CARTESIAN_POINT('Ctrl Pts',(-20.3959063681153,-17.640578473631,
0.572073073340858));
#159616=CARTESIAN_POINT('Ctrl Pts',(-20.3818931718824,-17.6229639730359,
0.573432898024445));
#159617=CARTESIAN_POINT('Ctrl Pts',(-20.372985736678,-17.6119946244254,
0.574291013654356));
#159618=CARTESIAN_POINT('Ctrl Pts',(-20.2682887424551,-17.4856678469225,
0.584307120689545));
#159619=CARTESIAN_POINT('Ctrl Pts',(-20.1606326762464,-17.3807345597759,
0.593981586658601));
#159620=CARTESIAN_POINT('Ctrl Pts',(-19.9681082338627,-17.2292981582217,
0.610137882418887));
#159621=CARTESIAN_POINT('Ctrl Pts',(-19.8895209050339,-17.175628199975,
0.616463024077607));
#159622=CARTESIAN_POINT('Ctrl Pts',(-19.7687968862645,-17.1045935663616,
0.625584773392738));
#159623=CARTESIAN_POINT('Ctrl Pts',(-19.7292811432573,-17.0830079998235,
0.628482572713435));
#159624=CARTESIAN_POINT('Ctrl Pts',(-19.6670830654527,-17.0515648159787,
0.63287774179694));
#159625=CARTESIAN_POINT('Ctrl Pts',(-19.6448671952155,-17.0408173890394,
0.63441587117762));
#159626=CARTESIAN_POINT('Ctrl Pts',(-19.6165114206779,-17.0277064543515,
0.636334549577888));
#159627=CARTESIAN_POINT('Ctrl Pts',(-19.6105425854013,-17.0249802398357,
0.636735959007892));
#159628=CARTESIAN_POINT('Ctrl Pts',(-19.6014989849698,-17.0209003661618,
0.637340315751712));
#159629=CARTESIAN_POINT('Ctrl Pts',(-19.5984335811499,-17.0195262307396,
0.637544504456244));
#159630=CARTESIAN_POINT('Ctrl Pts',(-19.5921219984971,-17.0167149464539,
0.637963541107619));
#159631=CARTESIAN_POINT('Ctrl Pts',(-19.5888755231369,-17.0152786873489,
0.638178326549259));
#159632=CARTESIAN_POINT('Ctrl Pts',(-19.581584573337,-17.0120750345173,
0.638659026358099));
#159633=CARTESIAN_POINT('Ctrl Pts',(-19.5775381800954,-17.0103121208095,
0.638924664550785));
#159634=CARTESIAN_POINT('Ctrl Pts',(-19.5672269241606,-17.0058580774846,
0.639598742979764));
#159635=CARTESIAN_POINT('Ctrl Pts',(-19.5609544653994,-17.0031845123946,
0.640006136707957));
#159636=CARTESIAN_POINT('Ctrl Pts',(-19.5252592061529,-16.9881731797153,
0.642310073973924));
#159637=CARTESIAN_POINT('Ctrl Pts',(-19.495571673944,-16.9764707688356,
0.644170640154768));
#159638=CARTESIAN_POINT('Ctrl Pts',(-19.2794561844563,-16.8968775715478,
0.657394736171677));
#159639=CARTESIAN_POINT('Ctrl Pts',(-19.0845520344043,-16.854815391008,
0.667705195132373));
#159640=CARTESIAN_POINT('Ctrl Pts',(-18.8308768713981,-16.8364793507316,
0.681839231662097));
#159641=CARTESIAN_POINT('Ctrl Pts',(-18.7749975640742,-16.8346593857397,
0.684989140635444));
#159642=CARTESIAN_POINT('Ctrl Pts',(-18.6844308353817,-16.8352962157188,
0.690198366812785));
#159643=CARTESIAN_POINT('Ctrl Pts',(-18.6497600394472,-16.8363924185085,
0.692217084492867));
#159644=CARTESIAN_POINT('Ctrl Pts',(-18.6042816533609,-16.838950005534,
0.694903368005656));
#159645=CARTESIAN_POINT('Ctrl Pts',(-18.5934351202104,-16.8396438187457,
0.69554689818027));
#159646=CARTESIAN_POINT('Ctrl Pts',(-18.5756897159066,-16.8409162082112,
0.696604598180517));
#159647=CARTESIAN_POINT('Ctrl Pts',(-18.5687874047928,-16.841445163318,
0.697017208626232));
#159648=CARTESIAN_POINT('Ctrl Pts',(-18.555439136671,-16.8425339820212,
0.697817528158793));
#159649=CARTESIAN_POINT('Ctrl Pts',(-18.5489929004935,-16.8430895622113,
0.69820509847197));
#159650=CARTESIAN_POINT('Ctrl Pts',(-18.5341253637447,-16.8444396381646,
0.699101510073222));
#159651=CARTESIAN_POINT('Ctrl Pts',(-18.5257061175842,-16.8452550689962,
0.699611003538169));
#159652=CARTESIAN_POINT('Ctrl Pts',(-18.5030997550544,-16.847581402876,
0.700984159917421));
#159653=CARTESIAN_POINT('Ctrl Pts',(-18.488922839185,-16.8491852852222,
0.701850727407893));
#159654=CARTESIAN_POINT('Ctrl Pts',(-18.3611876318254,-16.864945667576,
0.709708877508467));
#159655=CARTESIAN_POINT('Ctrl Pts',(-18.2489533345825,-16.8881426257189,
0.716988445908179));
#159656=CARTESIAN_POINT('Ctrl Pts',(-17.9820855705209,-16.9662759357056,
0.735128699931953));
#159657=CARTESIAN_POINT('Ctrl Pts',(-17.8308813018924,-17.0303206101844,
0.746145961979646));
#159658=CARTESIAN_POINT('Ctrl Pts',(-17.6600642190857,-17.1273287319056,
0.758628266601296));
#159659=CARTESIAN_POINT('Ctrl Pts',(-17.6319409962318,-17.1441754721256,
0.760682597349746));
#159660=CARTESIAN_POINT('Ctrl Pts',(-17.5980635973392,-17.1655536783302,
0.763145850395102));
#159661=CARTESIAN_POINT('Ctrl Pts',(-17.5919285120087,-17.1694695820435,
0.763591468481325));
#159662=CARTESIAN_POINT('Ctrl Pts',(-17.5823448931952,-17.175656406651,
0.764286678849229));
#159663=CARTESIAN_POINT('Ctrl Pts',(-17.5788826679878,-17.1779058659089,
0.764537650647354));
#159664=CARTESIAN_POINT('Ctrl Pts',(-17.5724300865637,-17.1821251010458,
0.76500501276939));
#159665=CARTESIAN_POINT('Ctrl Pts',(-17.5694381729535,-17.1840923177264,
0.765221562110266));
#159666=CARTESIAN_POINT('Ctrl Pts',(-17.5626250572158,-17.1885968181109,
0.765714339463772));
#159667=CARTESIAN_POINT('Ctrl Pts',(-17.5588071105342,-17.1911389288376,
0.765990239695704));
#159668=CARTESIAN_POINT('Ctrl Pts',(-17.5471004009189,-17.1989886641076,
0.766835563101407));
#159669=CARTESIAN_POINT('Ctrl Pts',(-17.5392389832897,-17.2043371255787,
0.767402312133544));
#159670=CARTESIAN_POINT('Ctrl Pts',(-17.4690615360394,-17.2527767172425,
0.772455924193651));
#159671=CARTESIAN_POINT('Ctrl Pts',(-17.4090573796301,-17.299136205502,
0.776737454769638));
#159672=CARTESIAN_POINT('Ctrl Pts',(-17.2444599364032,-17.4410420583912,
0.7887679435587));
#159673=CARTESIAN_POINT('Ctrl Pts',(-17.1467956137419,-17.5439843517251,
0.796291846501775));
#159674=CARTESIAN_POINT('Ctrl Pts',(-17.022284352449,-17.7047869375512,
0.807543773762307));
#159675=CARTESIAN_POINT('Ctrl Pts',(-16.9865971547358,-17.7552989850727,
0.811013087338098));
#159676=CARTESIAN_POINT('Ctrl Pts',(-16.9330236195699,-17.8386439593223,
0.81669927307816));
#159677=CARTESIAN_POINT('Ctrl Pts',(-16.913706476478,-17.8705154486512,
0.81886500089717));
#159678=CARTESIAN_POINT('Ctrl Pts',(-16.889721162182,-17.9125536836993,
0.821718118400923));
#159679=CARTESIAN_POINT('Ctrl Pts',(-16.8842775646661,-17.9222718896959,
0.822377440309922));
#159680=CARTESIAN_POINT('Ctrl Pts',(-16.8755513185413,-17.938142947066,
0.823453989790388));
#159681=CARTESIAN_POINT('Ctrl Pts',(-16.8722218878484,-17.9442699345928,
0.823869539519155));
#159682=CARTESIAN_POINT('Ctrl Pts',(-16.8658786503995,-17.9560818189598,
0.824670609821085));
#159683=CARTESIAN_POINT('Ctrl Pts',(-16.8628603670973,-17.9617642336677,
0.825055965522491));
#159684=CARTESIAN_POINT('Ctrl Pts',(-16.8560106148307,-17.9748031584827,
0.825940203282218));
#159685=CARTESIAN_POINT('Ctrl Pts',(-16.8521963996357,-17.9821685690393,
0.826439688171165));
#159686=CARTESIAN_POINT('Ctrl Pts',(-16.8421820600241,-18.0017881881941,
0.82777027896965));
#159687=CARTESIAN_POINT('Ctrl Pts',(-16.8360578054184,-18.014080484588,
0.828604027278096));
#159688=CARTESIAN_POINT('Ctrl Pts',(-16.7905171991408,-18.1077600425731,
0.834959681463982));
#159689=CARTESIAN_POINT('Ctrl Pts',(-16.7562374761297,-18.1915276729902,
0.840658450591947));
#159690=CARTESIAN_POINT('Ctrl Pts',(-16.6828138305152,-18.4098663849784,
0.855532659367458));
#159691=CARTESIAN_POINT('Ctrl Pts',(-16.6514720257712,-18.5466041109191,
0.864884455213787));
#159692=CARTESIAN_POINT('Ctrl Pts',(-16.6269167074976,-18.7400518439375,
0.877655292127132));
#159693=CARTESIAN_POINT('Ctrl Pts',(-16.6221157616113,-18.794940082407,
0.881224237294299));
#159694=CARTESIAN_POINT('Ctrl Pts',(-16.6180913442802,-18.8783338064409,
0.886508468406996));
#159695=CARTESIAN_POINT('Ctrl Pts',(-16.6172932101163,-18.9067374681944,
0.8882839514325));
#159696=CARTESIAN_POINT('Ctrl Pts',(-16.617011841802,-18.9420871916648,
0.890456402204427));
#159697=CARTESIAN_POINT('Ctrl Pts',(-16.6169907237583,-18.9490245832553,
0.890880961869076));
#159698=CARTESIAN_POINT('Ctrl Pts',(-16.6170112734271,-18.9600046128779,
0.891549968285345));
#159699=CARTESIAN_POINT('Ctrl Pts',(-16.6170304186052,-18.9640471716922,
0.891795644361729));
#159700=CARTESIAN_POINT('Ctrl Pts',(-16.6170883622668,-18.9716708854005,
0.892257727471336));
#159701=CARTESIAN_POINT('Ctrl Pts',(-16.6171246676817,-18.9752519529329,
0.892474265406916));
#159702=CARTESIAN_POINT('Ctrl Pts',(-16.6172284551278,-18.9834396489968,
0.892968196498979));
#159703=CARTESIAN_POINT('Ctrl Pts',(-16.617301887279,-18.9880461542013,
0.893245253677383));
#159704=CARTESIAN_POINT('Ctrl Pts',(-16.6175368194362,-19.0002781323422,
0.893978812221056));
#159705=CARTESIAN_POINT('Ctrl Pts',(-16.6177244937206,-19.0079031147136,
0.894433887282302));
#159706=CARTESIAN_POINT('Ctrl Pts',(-16.6193297206289,-19.0613722307344,
0.897610645242317));
#159707=CARTESIAN_POINT('Ctrl Pts',(-16.6221957053312,-19.1071643406512,
0.900257140898366));
#159708=CARTESIAN_POINT('Ctrl Pts',(-16.6301253428469,-19.1903754087313,
0.904988792027944));
#159709=CARTESIAN_POINT('Ctrl Pts',(-16.6347060009862,-19.2278194067312,
0.907089195880349));
#159710=CARTESIAN_POINT('Ctrl Pts',(-16.6596431292772,-19.3945632665945,
0.916389198441517));
#159711=CARTESIAN_POINT('Ctrl Pts',(-16.690963210163,-19.5219305423736,
0.923366387491949));
#159712=CARTESIAN_POINT('Ctrl Pts',(-16.7627867210685,-19.7290523575996,
0.935466793773518));
#159713=CARTESIAN_POINT('Ctrl Pts',(-16.7969202979498,-19.8106104005122,
0.940438829420389));
#159714=CARTESIAN_POINT('Ctrl Pts',(-16.8451368538583,-19.9081936353757,
0.946782341186288));
#159715=CARTESIAN_POINT('Ctrl Pts',(-16.8544956833137,-19.9264607395933,
0.947987351134396));
#159716=CARTESIAN_POINT('Ctrl Pts',(-16.8682707964664,-19.9524109019355,
0.949725690316531));
#159717=CARTESIAN_POINT('Ctrl Pts',(-16.872472196481,-19.9602071546664,
0.950251414748844));
#159718=CARTESIAN_POINT('Ctrl Pts',(-16.8798390522778,-19.9736742905901,
0.951165681465874));
#159719=CARTESIAN_POINT('Ctrl Pts',(-16.882981934529,-19.979357433399,0.951553413430187));
#159720=CARTESIAN_POINT('Ctrl Pts',(-16.8890741879418,-19.9902550926083,
0.952300626729609));
#159721=CARTESIAN_POINT('Ctrl Pts',(-16.8920196450403,-19.9954717342221,
0.952659964537832));
#159722=CARTESIAN_POINT('Ctrl Pts',(-16.8997915754416,-20.0091009990053,
0.953603162015657));
#159723=CARTESIAN_POINT('Ctrl Pts',(-16.904653747497,-20.0174930081285,
0.954188309087466));
#159724=CARTESIAN_POINT('Ctrl Pts',(-16.9217171354945,-20.0464829647469,
0.956225145887692));
#159725=CARTESIAN_POINT('Ctrl Pts',(-16.9342096073345,-20.0669065475066,
0.957687408843258));
#159726=CARTESIAN_POINT('Ctrl Pts',(-17.0303087553724,-20.2181908525007,
0.968729373948781));
#159727=CARTESIAN_POINT('Ctrl Pts',(-17.1277266748375,-20.3396860476931,
0.978845204940532));
#159728=CARTESIAN_POINT('Ctrl Pts',(-17.2901113290746,-20.5019680506941,
0.994012124241926));
#159729=CARTESIAN_POINT('Ctrl Pts',(-17.3454270809017,-20.5517128654059,
0.998935716793171));
#159730=CARTESIAN_POINT('Ctrl Pts',(-17.4390033241238,-20.6273466657035,
1.00677227019052));
#159731=CARTESIAN_POINT('Ctrl Pts',(-17.4756948790863,-20.6550771001664,
1.00973304637029));
#159732=CARTESIAN_POINT('Ctrl Pts',(-17.526918947316,-20.6912307867584,
1.01368767162696));
#159733=CARTESIAN_POINT('Ctrl Pts',(-17.540689410891,-20.7007076005282,
1.01473383051009));
#159734=CARTESIAN_POINT('Ctrl Pts',(-17.5644677100077,-20.7166600941096,
1.01650953185444));
#159735=CARTESIAN_POINT('Ctrl Pts',(-17.5744204528825,-20.7232160551428,
1.01724372037678));
#159736=CARTESIAN_POINT('Ctrl Pts',(-17.5886445411732,-20.732414301111,
1.01827959037356));
#159737=CARTESIAN_POINT('Ctrl Pts',(-17.5928705320101,-20.735125836598,
1.01858568352368));
#159738=CARTESIAN_POINT('Ctrl Pts',(-17.6001691636449,-20.7397723061836,
1.01911141362696));
#159739=CARTESIAN_POINT('Ctrl Pts',(-17.6032371940876,-20.7417144078817,
1.01933152364777));
#159740=CARTESIAN_POINT('Ctrl Pts',(-17.6091970815036,-20.7454656477817,
1.01975737351722));
#159741=CARTESIAN_POINT('Ctrl Pts',(-17.6120883110078,-20.7472756884987,
1.01996317633812));
#159742=CARTESIAN_POINT('Ctrl Pts',(-17.6198979819285,-20.7521386625336,
1.02051700875051));
#159743=CARTESIAN_POINT('Ctrl Pts',(-17.6248246334084,-20.7551784490053,
1.02086417721174));
#159744=CARTESIAN_POINT('Ctrl Pts',(-17.6431403978934,-20.766375964797,
1.02214690229825));
#159745=CARTESIAN_POINT('Ctrl Pts',(-17.6566079166495,-20.7744053183454,
1.02307442104436));
#159746=CARTESIAN_POINT('Ctrl Pts',(-17.7862426501802,-20.8497543212767,
1.03186589672374));
#159747=CARTESIAN_POINT('Ctrl Pts',(-17.9084935466971,-20.9060379904763,
1.03912854476416));
#159748=CARTESIAN_POINT('Ctrl Pts',(-18.186958345739,-21.0034038700418,
1.05514828884175));
#159749=CARTESIAN_POINT('Ctrl Pts',(-18.3441735056854,-21.0389929441575,
1.06389553130149));
#159750=CARTESIAN_POINT('Ctrl Pts',(-18.5224429415701,-21.0584854220862,
1.07436835997818));
#159751=CARTESIAN_POINT('Ctrl Pts',(-18.5410186473761,-21.0602683384654,
1.07546548286871));
#159752=CARTESIAN_POINT('Ctrl Pts',(-18.5681153630046,-21.0625080042181,
1.07707530749207));
#159753=CARTESIAN_POINT('Ctrl Pts',(-18.5766197305491,-21.0631592067393,
1.07758190379785));
#159754=CARTESIAN_POINT('Ctrl Pts',(-18.5915592531959,-21.0642123955715,
1.0784742923869));
#159755=CARTESIAN_POINT('Ctrl Pts',(-18.5979927810334,-21.0646364110575,
1.07885938800254));
#159756=CARTESIAN_POINT('Ctrl Pts',(-18.6105053522581,-21.0654036869368,
1.0796099520909));
#159757=CARTESIAN_POINT('Ctrl Pts',(-18.616584142826,-21.0657501241299,
1.07997531686228));
#159758=CARTESIAN_POINT('Ctrl Pts',(-18.6311459416443,-21.0665170088088,
1.08085233465806));
#159759=CARTESIAN_POINT('Ctrl Pts',(-18.6396301016567,-21.0669126357513,
1.08136476141346));
#159760=CARTESIAN_POINT('Ctrl Pts',(-18.6704145147752,-21.0681625446419,
1.08322946316574));
#159761=CARTESIAN_POINT('Ctrl Pts',(-18.6927249306074,-21.068715223672,
1.08459113297869));
#159762=CARTESIAN_POINT('Ctrl Pts',(-18.8983629553123,-21.0705570774406,
1.09724052907358));
#159763=CARTESIAN_POINT('Ctrl Pts',(-19.0810907955008,-21.0483779831166,
1.10930511710093));
#159764=CARTESIAN_POINT('Ctrl Pts',(-19.3376238586525,-20.9827572732755,
1.12678916331176));
#159765=CARTESIAN_POINT('Ctrl Pts',(-19.4153871112108,-20.9580035463373,
1.13214930867555));
#159766=CARTESIAN_POINT('Ctrl Pts',(-19.5255258326552,-20.9157976128368,
1.13967026937395));
#159767=CARTESIAN_POINT('Ctrl Pts',(-19.5591795901631,-20.9018956947146,
1.14195791219084));
#159768=CARTESIAN_POINT('Ctrl Pts',(-19.5993085682821,-20.8840937375448,
1.14465886514893));
#159769=CARTESIAN_POINT('Ctrl Pts',(-19.6061408200935,-20.8810193163322,
1.14511776581391));
#159770=CARTESIAN_POINT('Ctrl Pts',(-19.6167471219025,-20.8761787542721,
1.14582850047896));
#159771=CARTESIAN_POINT('Ctrl Pts',(-19.6205324434618,-20.87443766791,1.14608182704143));
#159772=CARTESIAN_POINT('Ctrl Pts',(-19.627548579015,-20.8711854152771,
1.14655072293382));
#159773=CARTESIAN_POINT('Ctrl Pts',(-19.6307806854641,-20.8696772730947,
1.14676646819574));
#159774=CARTESIAN_POINT('Ctrl Pts',(-19.63808683347,-20.8662456201758,1.14725358206064));
#159775=CARTESIAN_POINT('Ctrl Pts',(-19.6421585445008,-20.8643172738142,
1.14752464758625));
#159776=CARTESIAN_POINT('Ctrl Pts',(-19.6544481996741,-20.8584488373268,
1.14834167811367));
#159777=CARTESIAN_POINT('Ctrl Pts',(-19.6626470097959,-20.8544686056714,
1.14888521636138));
#159778=CARTESIAN_POINT('Ctrl Pts',(-19.72559356443,-20.8234064000575,1.15304837587856));
#159779=CARTESIAN_POINT('Ctrl Pts',(-19.77917724071,-20.794016751859,1.15653482463366));
#159780=CARTESIAN_POINT('Ctrl Pts',(-19.9708583559331,-20.6778210693829,
1.1690640806586));
#159781=CARTESIAN_POINT('Ctrl Pts',(-20.1000687156637,-20.5774657607867,
1.17766510613336));
#159782=CARTESIAN_POINT('Ctrl Pts',(-20.27310772629,-20.4077224818031,1.19111364917181));
#159783=CARTESIAN_POINT('Ctrl Pts',(-20.3265596928393,-20.349044093169,
1.19560095950127));
#159784=CARTESIAN_POINT('Ctrl Pts',(-20.3888155115893,-20.2724734603528,
1.2013596026769));
#159785=CARTESIAN_POINT('Ctrl Pts',(-20.4008332642335,-20.2572706115,1.20249833136437));
#159786=CARTESIAN_POINT('Ctrl Pts',(-20.417916064501,-20.2350396168923,
1.20415788796861));
#159787=CARTESIAN_POINT('Ctrl Pts',(-20.4231495686117,-20.2281417249908,
1.20467205338954));
#159788=CARTESIAN_POINT('Ctrl Pts',(-20.4322171031043,-20.216036977003,
1.20557309651751));
#159789=CARTESIAN_POINT('Ctrl Pts',(-20.4360698922146,-20.2108442672117,
1.20595923331387));
#159790=CARTESIAN_POINT('Ctrl Pts',(-20.4434805626342,-20.2007601011449,
1.2067083843911));
#159791=CARTESIAN_POINT('Ctrl Pts',(-20.4470413923956,-20.1958708819626,
1.20707127883666));
#159792=CARTESIAN_POINT('Ctrl Pts',(-20.4554655649932,-20.1841992377868,
1.20793685243778));
#159793=CARTESIAN_POINT('Ctrl Pts',(-20.4603098215203,-20.1774032193782,
1.20844026140814));
#159794=CARTESIAN_POINT('Ctrl Pts',(-20.4774343962811,-20.1530760392564,
1.21024031609457));
#159795=CARTESIAN_POINT('Ctrl Pts',(-20.4894885518545,-20.1353879489513,
1.21154553712713));
#159796=CARTESIAN_POINT('Ctrl Pts',(-20.6070116373583,-19.9571883818426,
1.22466380455483));
#159797=CARTESIAN_POINT('Ctrl Pts',(-20.6904215824267,-19.7832402127721,
1.23734172803333));
#159798=CARTESIAN_POINT('Ctrl Pts',(-20.7725200301161,-19.5281126179303,
1.25502394120177));
#159799=CARTESIAN_POINT('Ctrl Pts',(-20.7918958182709,-19.4545296440857,
1.26000957895954));
#159800=CARTESIAN_POINT('Ctrl Pts',(-20.814328049116,-19.3458809039321,
1.26707454839157));
#159801=CARTESIAN_POINT('Ctrl Pts',(-20.8205389602626,-19.3115308797393,
1.26926550463162));
#159802=CARTESIAN_POINT('Ctrl Pts',(-20.8270336493148,-19.2697323491855,
1.2718675311355));
#159803=CARTESIAN_POINT('Ctrl Pts',(-20.8281309522128,-19.2624178821867,
1.27232050370385));
#159804=CARTESIAN_POINT('Ctrl Pts',(-20.8297832007564,-19.2509965662707,
1.2730239599202));
#159805=CARTESIAN_POINT('Ctrl Pts',(-20.8303644475577,-19.246893667125,
1.27327589048324));
#159806=CARTESIAN_POINT('Ctrl Pts',(-20.8314236225284,-19.2392557603439,
1.27374340933906));
#159807=CARTESIAN_POINT('Ctrl Pts',(-20.8319046584578,-19.235721286609,
1.27395916587399));
#159808=CARTESIAN_POINT('Ctrl Pts',(-20.8329764090898,-19.2276946885975,
1.27444781320636));
#159809=CARTESIAN_POINT('Ctrl Pts',(-20.8335616366231,-19.2232018844577,
1.27472039173343));
#159810=CARTESIAN_POINT('Ctrl Pts',(-20.8352591869439,-19.2098348637777,
1.27552867654589));
#159811=CARTESIAN_POINT('Ctrl Pts',(-20.8363297189069,-19.2009553113893,
1.27606208409878));
#159812=CARTESIAN_POINT('Ctrl Pts',(-20.8440773310424,-19.1330752901942,
1.28011463463401));
#159813=CARTESIAN_POINT('Ctrl Pts',(-20.8483264232128,-19.0738184747974,
1.28350787833422));
#159814=CARTESIAN_POINT('Ctrl Pts',(-20.8506770343578,-18.9941772552031,
1.2879671464208));
#159815=CARTESIAN_POINT('Ctrl Pts',(-20.850984040619,-18.9738904697432,
1.28909422412876));
#159816=CARTESIAN_POINT('Ctrl Pts',(-20.8511051846576,-18.8138052346158,
1.29793914602207));
#159817=CARTESIAN_POINT('Ctrl Pts',(-20.8373639019979,-18.6743412751728,
1.30537420899821));
#159818=CARTESIAN_POINT('Ctrl Pts',(-20.7922497677195,-18.4485303721484,
1.31812045243393));
#159819=CARTESIAN_POINT('Ctrl Pts',(-20.7688587895497,-18.3610511026349,
1.32323614162662));
#159820=CARTESIAN_POINT('Ctrl Pts',(-20.7355595833628,-18.2623358416696,
1.32934390222889));
#159821=CARTESIAN_POINT('Ctrl Pts',(-20.7310458567807,-18.2493726096199,
1.33015267371104));
#159822=CARTESIAN_POINT('Ctrl Pts',(-20.7251405052162,-18.232929407642,
1.3311874287854));
#159823=CARTESIAN_POINT('Ctrl Pts',(-20.723865204357,-18.2294077938434,
1.3314095610146));
#159824=CARTESIAN_POINT('Ctrl Pts',(-20.7225805737606,-18.2258896077991,
1.33163200235201));
#159825=CARTESIAN_POINT('Origin',(-18.734,-18.952,0.));
#159826=CARTESIAN_POINT('',(-20.7225805738064,-18.2258896079248,2.35747639166834));
#159827=CARTESIAN_POINT('',(-20.7227693997001,-18.2258206865925,2.13351567424346));
#159828=CARTESIAN_POINT('',(-20.7225805737622,-18.2258896078036,0.));
#159829=CARTESIAN_POINT('Ctrl Pts',(-20.7225805738064,-18.2258896079247,
2.35747639166834));
#159830=CARTESIAN_POINT('Ctrl Pts',(-20.7258083163625,-18.2347293466398,
2.35692313238699));
#159831=CARTESIAN_POINT('Ctrl Pts',(-20.7289770784287,-18.2435905028254,
2.3563679571628));
#159832=CARTESIAN_POINT('Ctrl Pts',(-20.7349196707797,-18.2605645521431,
2.3553032437465));
#159833=CARTESIAN_POINT('Ctrl Pts',(-20.7377034742786,-18.268673656785,
2.35479405363621));
#159834=CARTESIAN_POINT('Ctrl Pts',(-20.742495817349,-18.2829146663808,
2.35389879366171));
#159835=CARTESIAN_POINT('Ctrl Pts',(-20.7445257367668,-18.2890392980362,
2.35351343617493));
#159836=CARTESIAN_POINT('Ctrl Pts',(-20.7484115458976,-18.3009454756058,
2.3527636241521));
#159837=CARTESIAN_POINT('Ctrl Pts',(-20.7502706244422,-18.3067259204055,
2.35239927919822));
#159838=CARTESIAN_POINT('Ctrl Pts',(-20.7546531720662,-18.3205564712627,
2.35152675227654));
#159839=CARTESIAN_POINT('Ctrl Pts',(-20.7571534251839,-18.3286137740462,
2.35101781318275));
#159840=CARTESIAN_POINT('Ctrl Pts',(-20.7659891981977,-18.3577010067049,
2.34917813211045));
#159841=CARTESIAN_POINT('Ctrl Pts',(-20.7720453439938,-18.3788137180527,
2.34783831423605));
#159842=CARTESIAN_POINT('Ctrl Pts',(-20.8265422864376,-18.5805937635665,
2.33498648880404));
#159843=CARTESIAN_POINT('Ctrl Pts',(-20.8511563473918,-18.7668066913728,
2.32266072461913));
#159844=CARTESIAN_POINT('Ctrl Pts',(-20.8509463099784,-19.0167905684345,
2.30615871560825));
#159845=CARTESIAN_POINT('Ctrl Pts',(-20.8480800907388,-19.0797716888197,
2.3020162197331));
#159846=CARTESIAN_POINT('Ctrl Pts',(-20.8379188594366,-19.1922138901616,
2.294736470999));
#159847=CARTESIAN_POINT('Ctrl Pts',(-20.8316744038733,-19.2417244246739,
2.2915721160161));
#159848=CARTESIAN_POINT('Ctrl Pts',(-20.8224344763622,-19.2986864810193,
2.28801336666911));
#159849=CARTESIAN_POINT('Ctrl Pts',(-20.8211403742118,-19.3063940473903,
2.28753358271605));
#159850=CARTESIAN_POINT('Ctrl Pts',(-20.8190058158421,-19.3186899278457,
2.28677117621273));
#159851=CARTESIAN_POINT('Ctrl Pts',(-20.818192841388,-19.3232828519414,
2.2864870599892));
#159852=CARTESIAN_POINT('Ctrl Pts',(-20.8167271896883,-19.3314065696945,
2.28598575937405));
#159853=CARTESIAN_POINT('Ctrl Pts',(-20.8160807013227,-19.3349384359324,
2.28576822723461));
#159854=CARTESIAN_POINT('Ctrl Pts',(-20.8146926433656,-19.3424141738573,
2.28530867660281));
#159855=CARTESIAN_POINT('Ctrl Pts',(-20.8139488464475,-19.346357578959,
2.28506678653678));
#159856=CARTESIAN_POINT('Ctrl Pts',(-20.8119140370227,-19.3569796604932,
2.28441656813197));
#159857=CARTESIAN_POINT('Ctrl Pts',(-20.8106020279226,-19.3636543345662,
2.28400941972416));
#159858=CARTESIAN_POINT('Ctrl Pts',(-20.8039707318822,-19.3965515454561,
2.28200928796493));
#159859=CARTESIAN_POINT('Ctrl Pts',(-20.7981865543776,-19.4226792186793,
2.28044134373731));
#159860=CARTESIAN_POINT('Ctrl Pts',(-20.7800922406585,-19.4976481565181,
2.27598372088627));
#159861=CARTESIAN_POINT('Ctrl Pts',(-20.766532160977,-19.5461709004844,
2.27314943457568));
#159862=CARTESIAN_POINT('Ctrl Pts',(-20.7111897755124,-19.7200192212083,
2.26303191982632));
#159863=CARTESIAN_POINT('Ctrl Pts',(-20.6594361095099,-19.8418489548003,
2.25599598032528));
#159864=CARTESIAN_POINT('Ctrl Pts',(-20.5472452680199,-20.0495631285174,
2.24300928277803));
#159865=CARTESIAN_POINT('Ctrl Pts',(-20.4911569502299,-20.1372841973632,
2.23716716396362));
#159866=CARTESIAN_POINT('Ctrl Pts',(-20.420431863255,-20.2317789747589,
2.2302504123524));
#159867=CARTESIAN_POINT('Ctrl Pts',(-20.4118958807706,-20.2429500581825,
2.22942232056066));
#159868=CARTESIAN_POINT('Ctrl Pts',(-20.3980907442966,-20.2606486717286,
2.22809320824314));
#159869=CARTESIAN_POINT('Ctrl Pts',(-20.3928928723692,-20.2672314572667,
2.22759500934397));
#159870=CARTESIAN_POINT('Ctrl Pts',(-20.3836314092623,-20.278818286173,
2.22671116545395));
#159871=CARTESIAN_POINT('Ctrl Pts',(-20.3795838022371,-20.2838350120582,
2.22632616449098));
#159872=CARTESIAN_POINT('Ctrl Pts',(-20.3711396584803,-20.2942036771062,
2.22552555578883));
#159873=CARTESIAN_POINT('Ctrl Pts',(-20.3667396475099,-20.2995526757355,
2.2251098099924));
#159874=CARTESIAN_POINT('Ctrl Pts',(-20.3553245597693,-20.3132917674634,
2.22403483497759));
#159875=CARTESIAN_POINT('Ctrl Pts',(-20.3482706399931,-20.3216491879681,
2.22337402350214));
#159876=CARTESIAN_POINT('Ctrl Pts',(-20.3180882802634,-20.3568519167258,
2.22056078797073));
#159877=CARTESIAN_POINT('Ctrl Pts',(-20.2943536084299,-20.383167693194,
2.21838335515681));
#159878=CARTESIAN_POINT('Ctrl Pts',(-20.2303135597651,-20.4506846003687,
2.21259364244598));
#159879=CARTESIAN_POINT('Ctrl Pts',(-20.1889687776947,-20.4908550048895,
2.20893880036528));
#159880=CARTESIAN_POINT('Ctrl Pts',(-20.046231988734,-20.618637775003,2.19660006888768));
#159881=CARTESIAN_POINT('Ctrl Pts',(-19.9381730510058,-20.6983093674286,
2.18767365898868));
#159882=CARTESIAN_POINT('Ctrl Pts',(-19.7463729528397,-20.8134091780896,
2.17297285950675));
#159883=CARTESIAN_POINT('Ctrl Pts',(-19.6665527493101,-20.8546540042086,
2.16715233064708));
#159884=CARTESIAN_POINT('Ctrl Pts',(-19.575507996101,-20.8945875652029,
2.16101032812413));
#159885=CARTESIAN_POINT('Ctrl Pts',(-19.5666425072347,-20.8984040226088,
2.160417326593));
#159886=CARTESIAN_POINT('Ctrl Pts',(-19.5535033396687,-20.9039540308319,
2.15954627821453));
#159887=CARTESIAN_POINT('Ctrl Pts',(-19.5492497453426,-20.9057344025882,
2.1592654936668));
#159888=CARTESIAN_POINT('Ctrl Pts',(-19.541688244613,-20.9088703274896,
2.15876852815635));
#159889=CARTESIAN_POINT('Ctrl Pts',(-19.5383826919449,-20.9102314124406,
2.15855201516348));
#159890=CARTESIAN_POINT('Ctrl Pts',(-19.5312874498149,-20.9131319316096,
2.1580888692551));
#159891=CARTESIAN_POINT('Ctrl Pts',(-19.52749675251,-20.9146687533098,2.15784239450916));
#159892=CARTESIAN_POINT('Ctrl Pts',(-19.5170660150691,-20.9188624161717,
2.15716676509725));
#159893=CARTESIAN_POINT('Ctrl Pts',(-19.5104168580256,-20.9214966397538,
2.15673895385215));
#159894=CARTESIAN_POINT('Ctrl Pts',(-19.4746420432678,-20.9354603635601,
2.15445192748817));
#159895=CARTESIAN_POINT('Ctrl Pts',(-19.4452799051509,-20.9461782218498,
2.15262718488174));
#159896=CARTESIAN_POINT('Ctrl Pts',(-19.2606291299342,-21.0089822427048,
2.141412702458));
#159897=CARTESIAN_POINT('Ctrl Pts',(-19.0999558538295,-21.0435551224519,
2.13275781703143));
#159898=CARTESIAN_POINT('Ctrl Pts',(-18.820250477949,-21.070485391847,2.11737630806303));
#159899=CARTESIAN_POINT('Ctrl Pts',(-18.7028972452879,-21.0720110436178,
2.11083594617432));
#159900=CARTESIAN_POINT('Ctrl Pts',(-18.5717696799672,-21.0628232171389,
2.1031352651694));
#159901=CARTESIAN_POINT('Ctrl Pts',(-18.5575209642284,-21.0616797069129,
2.10229349410253));
#159902=CARTESIAN_POINT('Ctrl Pts',(-18.534863540023,-21.0596302271924,
2.10094657192043));
#159903=CARTESIAN_POINT('Ctrl Pts',(-18.5264466385261,-21.0588180043002,
2.10044436437406));
#159904=CARTESIAN_POINT('Ctrl Pts',(-18.5116115644829,-21.0572966720063,
2.0995558624074));
#159905=CARTESIAN_POINT('Ctrl Pts',(-18.5051913109716,-21.0566085801907,
2.09917023444608));
#159906=CARTESIAN_POINT('Ctrl Pts',(-18.4919194259058,-21.0551247165029,
2.09837073803127));
#159907=CARTESIAN_POINT('Ctrl Pts',(-18.4850683423046,-21.05432480972,2.09795674344051));
#159908=CARTESIAN_POINT('Ctrl Pts',(-18.4674940039441,-21.052185785786,
2.09689140910206));
#159909=CARTESIAN_POINT('Ctrl Pts',(-18.4567769694191,-21.0507980287025,
2.09623854082589));
#159910=CARTESIAN_POINT('Ctrl Pts',(-18.4121029180219,-21.0446650132948,
2.09350332907598));
#159911=CARTESIAN_POINT('Ctrl Pts',(-18.3782546353486,-21.0391774262932,
2.0913976723594));
#159912=CARTESIAN_POINT('Ctrl Pts',(-18.2904311488428,-21.0227408786011,
2.08584406996937));
#159913=CARTESIAN_POINT('Ctrl Pts',(-18.2367261495752,-21.01050407104,2.08235775392238));
#159914=CARTESIAN_POINT('Ctrl Pts',(-18.0779620796321,-20.9677537702443,
2.07178969534737));
#159915=CARTESIAN_POINT('Ctrl Pts',(-17.9747308970806,-20.9311806329409,
2.06455955705839));
#159916=CARTESIAN_POINT('Ctrl Pts',(-17.8336087666274,-20.868511289613,
2.05435948503221));
#159917=CARTESIAN_POINT('Ctrl Pts',(-17.7930154194034,-20.8489101446456,
2.05138798456475));
#159918=CARTESIAN_POINT('Ctrl Pts',(-17.7315248675665,-20.8167584669132,
2.04685434478781));
#159919=CARTESIAN_POINT('Ctrl Pts',(-17.7101671044357,-20.8051181280426,
2.04527348681031));
#159920=CARTESIAN_POINT('Ctrl Pts',(-17.6764255488147,-20.785966958465,
2.04277097883368));
#159921=CARTESIAN_POINT('Ctrl Pts',(-17.6639103112282,-20.778692803976,
2.04184164016496));
#159922=CARTESIAN_POINT('Ctrl Pts',(-17.6195514150798,-20.752298002226,
2.03854613601304));
#159923=CARTESIAN_POINT('Ctrl Pts',(-17.5881354689064,-20.7324671883884,
2.03620921284529));
#159924=CARTESIAN_POINT('Ctrl Pts',(-17.5513005739013,-20.7078366624703,
2.0334803912852));
#159925=CARTESIAN_POINT('Ctrl Pts',(-17.5453657376142,-20.7038244522211,
2.0330410817079));
#159926=CARTESIAN_POINT('Ctrl Pts',(-17.5357204643577,-20.6972322411123,
2.03232785449199));
#159927=CARTESIAN_POINT('Ctrl Pts',(-17.5319977767078,-20.694670386801,
2.0320527579364));
#159928=CARTESIAN_POINT('Ctrl Pts',(-17.5253517737041,-20.6900653568766,
2.03156200186602));
#159929=CARTESIAN_POINT('Ctrl Pts',(-17.5224254021448,-20.6880267031779,
2.03134604189937));
#159930=CARTESIAN_POINT('Ctrl Pts',(-17.5161024911806,-20.6835980785477,
2.0308797122341));
#159931=CARTESIAN_POINT('Ctrl Pts',(-17.5127078390562,-20.681205512921,
2.03062952385904));
#159932=CARTESIAN_POINT('Ctrl Pts',(-17.5032535838909,-20.6745003847103,
2.02993316191436));
#159933=CARTESIAN_POINT('Ctrl Pts',(-17.497209565347,-20.6701658070654,
2.02948847196896));
#159934=CARTESIAN_POINT('Ctrl Pts',(-17.4624025899727,-20.6449245143009,
2.02692958108447));
#159935=CARTESIAN_POINT('Ctrl Pts',(-17.4341453339338,-20.6233262899623,
2.02486028058115));
#159936=CARTESIAN_POINT('Ctrl Pts',(-17.3453665331805,-20.5518544541814,
2.01833768880076));
#159937=CARTESIAN_POINT('Ctrl Pts',(-17.2870632426838,-20.4993245016502,
2.01401991869063));
#159938=CARTESIAN_POINT('Ctrl Pts',(-17.0991697150579,-20.3101061416014,
1.99947466152339));
#159939=CARTESIAN_POINT('Ctrl Pts',(-16.9849549549028,-20.1594593255126,
1.98942026280084));
#159940=CARTESIAN_POINT('Ctrl Pts',(-16.8813952245768,-19.9767054546765,
1.97719993950338));
#159941=CARTESIAN_POINT('Ctrl Pts',(-16.8709256924165,-19.9575445265391,
1.9759197804434));
#159942=CARTESIAN_POINT('Ctrl Pts',(-16.8568341383175,-19.9307789084316,
1.97413158216748));
#159943=CARTESIAN_POINT('Ctrl Pts',(-16.8529580873951,-19.923308984707,
1.97363252667585));
#159944=CARTESIAN_POINT('Ctrl Pts',(-16.8463647347101,-19.9104147898239,
1.97277100778911));
#159945=CARTESIAN_POINT('Ctrl Pts',(-16.8436260013233,-19.9050015467289,
1.97240930226415));
#159946=CARTESIAN_POINT('Ctrl Pts',(-16.8380212066333,-19.8938041650189,
1.97166102696565));
#159947=CARTESIAN_POINT('Ctrl Pts',(-16.8351582606411,-19.8880185455322,
1.97127435300053));
#159948=CARTESIAN_POINT('Ctrl Pts',(-16.828546258959,-19.8745014210438,
1.9703708072304));
#159949=CARTESIAN_POINT('Ctrl Pts',(-16.8248177442107,-19.8667600460524,
1.96985322680284));
#159950=CARTESIAN_POINT('Ctrl Pts',(-16.812989494903,-19.8418141593357,
1.96818488786011));
#159951=CARTESIAN_POINT('Ctrl Pts',(-16.8050745787497,-19.8245235131901,
1.96702777548759));
#159952=CARTESIAN_POINT('Ctrl Pts',(-16.7664578113606,-19.7370683256845,
1.96116988338359));
#159953=CARTESIAN_POINT('Ctrl Pts',(-16.7393497961598,-19.6653882738376,
1.95634866999069));
#159954=CARTESIAN_POINT('Ctrl Pts',(-16.6829208435642,-19.4875893693371,
1.94435183652842));
#159955=CARTESIAN_POINT('Ctrl Pts',(-16.6578749468097,-19.3803491484572,
1.93707796735621));
#159956=CARTESIAN_POINT('Ctrl Pts',(-16.6305262316083,-19.2013038494993,
1.92511515039769));
#159957=CARTESIAN_POINT('Ctrl Pts',(-16.6233338488449,-19.1304480869743,
1.92042997292323));
#159958=CARTESIAN_POINT('Ctrl Pts',(-16.61733433675,-19.0122994576882,1.91281694416701));
#159959=CARTESIAN_POINT('Ctrl Pts',(-16.616516366061,-18.9651665585077,
1.90983278489281));
#159960=CARTESIAN_POINT('Ctrl Pts',(-16.6173957729037,-18.9103499265088,
1.90645269333428));
#159961=CARTESIAN_POINT('Ctrl Pts',(-16.6175611038839,-18.9026584768015,
1.90598050484497));
#159962=CARTESIAN_POINT('Ctrl Pts',(-16.6178930520492,-18.890341202341,
1.90522784645326));
#159963=CARTESIAN_POINT('Ctrl Pts',(-16.6180329168794,-18.8857148087221,
1.90494594104846));
#159964=CARTESIAN_POINT('Ctrl Pts',(-16.6183080633057,-18.8775051236416,
1.90444714593629));
#159965=CARTESIAN_POINT('Ctrl Pts',(-16.6184372773653,-18.8739216744508,
1.90422992044497));
#159966=CARTESIAN_POINT('Ctrl Pts',(-16.6187311710324,-18.8663084199623,
1.90376947400334));
#159967=CARTESIAN_POINT('Ctrl Pts',(-16.6188982611728,-18.8622787610035,
1.90352638937618));
#159968=CARTESIAN_POINT('Ctrl Pts',(-16.6193821248796,-18.8513632430997,
1.9028695640882));
#159969=CARTESIAN_POINT('Ctrl Pts',(-16.6197210185941,-18.8444783445676,
1.90245704499849));
#159970=CARTESIAN_POINT('Ctrl Pts',(-16.6215987577909,-18.8097825790151,
1.90038656902143));
#159971=CARTESIAN_POINT('Ctrl Pts',(-16.623652803958,-18.782000929344,1.89875581630666));
#159972=CARTESIAN_POINT('Ctrl Pts',(-16.6312483625306,-18.7010359038296,
1.89406164285005));
#159973=CARTESIAN_POINT('Ctrl Pts',(-16.6382571225494,-18.6480098659028,
1.89106089326304));
#159974=CARTESIAN_POINT('Ctrl Pts',(-16.6709973699999,-18.4564744133057,
1.88031256066668));
#159975=CARTESIAN_POINT('Ctrl Pts',(-16.7085227065561,-18.3203597729883,
1.87282533207767));
#159976=CARTESIAN_POINT('Ctrl Pts',(-16.7922381469642,-18.1037033854721,
1.85997459704055));
#159977=CARTESIAN_POINT('Ctrl Pts',(-16.8306726552981,-18.0206631635639,
1.85480758304878));
#159978=CARTESIAN_POINT('Ctrl Pts',(-16.8809213157937,-17.9282922747449,
1.84864293319504));
#159979=CARTESIAN_POINT('Ctrl Pts',(-16.8876102508442,-17.9162765825241,
1.84783267844201));
#159980=CARTESIAN_POINT('Ctrl Pts',(-16.8985220833874,-17.8971167506601,
1.84652682022565));
#159981=CARTESIAN_POINT('Ctrl Pts',(-16.9026708156669,-17.8899306671746,
1.84603388301395));
#159982=CARTESIAN_POINT('Ctrl Pts',(-16.9101103046585,-17.8772178121379,
1.84515611594288));
#159983=CARTESIAN_POINT('Ctrl Pts',(-16.9133842217187,-17.8716812699107,
1.84477190080306));
#159984=CARTESIAN_POINT('Ctrl Pts',(-16.9202563122077,-17.8601797942408,
1.84396964703329));
#159985=CARTESIAN_POINT('Ctrl Pts',(-16.9238587932814,-17.8542175367383,
1.84355145407345));
#159986=CARTESIAN_POINT('Ctrl Pts',(-16.9332867957635,-17.8387863852644,
1.842463035049));
#159987=CARTESIAN_POINT('Ctrl Pts',(-16.9391575397187,-17.8293454977909,
1.84179115069594));
#159988=CARTESIAN_POINT('Ctrl Pts',(-16.9649382458894,-17.7886060388423,
1.83886542693539));
#159989=CARTESIAN_POINT('Ctrl Pts',(-16.9855935685652,-17.7577890989379,
1.83658402116728));
#159990=CARTESIAN_POINT('Ctrl Pts',(-17.0425763555219,-17.6774222651702,
1.83044611582504));
#159991=CARTESIAN_POINT('Ctrl Pts',(-17.0802671612465,-17.6288866510134,
1.82654041292096));
#159992=CARTESIAN_POINT('Ctrl Pts',(-17.2189499632095,-17.4654980048029,
1.81269808355463));
#159993=CARTESIAN_POINT('Ctrl Pts',(-17.3302137406399,-17.3600065199969,
1.80244490846915));
#159994=CARTESIAN_POINT('Ctrl Pts',(-17.5041023438883,-17.227659279133,
1.78822049381552));
#159995=CARTESIAN_POINT('Ctrl Pts',(-17.5581711048619,-17.1903452798502,
1.78401704030332));
#159996=CARTESIAN_POINT('Ctrl Pts',(-17.6217418817322,-17.1507070044708,
1.77939204599635));
#159997=CARTESIAN_POINT('Ctrl Pts',(-17.6296238945902,-17.1458637918616,
1.77882397340844));
#159998=CARTESIAN_POINT('Ctrl Pts',(-17.64141447723,-17.1387249475169,1.77798247006001));
#159999=CARTESIAN_POINT('Ctrl Pts',(-17.6452989596623,-17.1363900236628,
1.77770655796869));
#160000=CARTESIAN_POINT('Ctrl Pts',(-17.6522544746406,-17.1322394812958,
1.77721492108227));
#160001=CARTESIAN_POINT('Ctrl Pts',(-17.6553226166101,-17.1304191397979,
1.77699889129218));
#160002=CARTESIAN_POINT('Ctrl Pts',(-17.6619642374425,-17.1265013031458,
1.77653306083741));
#160003=CARTESIAN_POINT('Ctrl Pts',(-17.6655392658563,-17.1244065472081,
1.77628343801914));
#160004=CARTESIAN_POINT('Ctrl Pts',(-17.6755107948266,-17.1186030785951,
1.77559024100435));
#160005=CARTESIAN_POINT('Ctrl Pts',(-17.6819206808914,-17.1149173184498,
1.77514812864165));
#160006=CARTESIAN_POINT('Ctrl Pts',(-17.7186588369577,-17.0940477953854,
1.77263327134123));
#160007=CARTESIAN_POINT('Ctrl Pts',(-17.7493904500128,-17.0775805101372,
1.77060363897603));
#160008=CARTESIAN_POINT('Ctrl Pts',(-17.8482673766107,-17.0277014368395,
1.76426104601227));
#160009=CARTESIAN_POINT('Ctrl Pts',(-17.9178121788401,-16.9971888939484,
1.76007512693076));
#160010=CARTESIAN_POINT('Ctrl Pts',(-18.1687670878453,-16.9028176279223,
1.745436893082));
#160011=CARTESIAN_POINT('Ctrl Pts',(-18.3570388578499,-16.8599838383096,
1.73519054994283));
#160012=CARTESIAN_POINT('Ctrl Pts',(-18.5697961078931,-16.8412695656064,
1.72275938408976));
#160013=CARTESIAN_POINT('Ctrl Pts',(-18.5911153024642,-16.8397192897474,
1.72150573952255));
#160014=CARTESIAN_POINT('Ctrl Pts',(-18.6207808065394,-16.8380132490336,
1.71974884791671));
#160015=CARTESIAN_POINT('Ctrl Pts',(-18.6291105179942,-16.8375835881815,
1.71925417367039));
#160016=CARTESIAN_POINT('Ctrl Pts',(-18.6434832158891,-16.8369273585576,
1.718398196058));
#160017=CARTESIAN_POINT('Ctrl Pts',(-18.6495250753707,-16.8366774353009,
1.71803762802359));
#160018=CARTESIAN_POINT('Ctrl Pts',(-18.6620299053607,-16.8362138291616,
1.71728979448245));
#160019=CARTESIAN_POINT('Ctrl Pts',(-18.6684929431349,-16.8360038659546,
1.71690241628587));
#160020=CARTESIAN_POINT('Ctrl Pts',(-18.6836162569328,-16.8355819119939,
1.71599389482369));
#160021=CARTESIAN_POINT('Ctrl Pts',(-18.6922770263912,-16.8353934624515,
1.71547201926492));
#160022=CARTESIAN_POINT('Ctrl Pts',(-18.7203396814472,-16.8349551518393,
1.71377576959262));
#160023=CARTESIAN_POINT('Ctrl Pts',(-18.7397434734032,-16.8349188804873,
1.71259474004215));
#160024=CARTESIAN_POINT('Ctrl Pts',(-18.8386474360854,-16.8360936887253,
1.70653157378616));
#160025=CARTESIAN_POINT('Ctrl Pts',(-18.9180248987222,-16.8415159541797,
1.7015193141454));
#160026=CARTESIAN_POINT('Ctrl Pts',(-19.0942573378354,-16.8635723259758,
1.69007663410652));
#160027=CARTESIAN_POINT('Ctrl Pts',(-19.1906416201142,-16.882509372942,
1.68360009651738));
#160028=CARTESIAN_POINT('Ctrl Pts',(-19.4063500109858,-16.9406972572094,
1.66883648021722));
#160029=CARTESIAN_POINT('Ctrl Pts',(-19.5242191903774,-16.9840177772865,
1.66057003159706));
#160030=CARTESIAN_POINT('Ctrl Pts',(-19.6460713112528,-17.0415280107163,
1.65224947637826));
#160031=CARTESIAN_POINT('Ctrl Pts',(-19.6545425167093,-17.0455953259953,
1.65167233210071));
#160032=CARTESIAN_POINT('Ctrl Pts',(-19.6670850362769,-17.0517205155948,
1.65082006191709));
#160033=CARTESIAN_POINT('Ctrl Pts',(-19.671177101106,-17.0537352961618,
1.65054236272938));
#160034=CARTESIAN_POINT('Ctrl Pts',(-19.6784603842825,-17.05735060567,1.65004878161011));
#160035=CARTESIAN_POINT('Ctrl Pts',(-19.6816540885934,-17.0589459928654,
1.64983258476878));
#160036=CARTESIAN_POINT('Ctrl Pts',(-19.688453827781,-17.0623642636129,
1.64937279273653));
#160037=CARTESIAN_POINT('Ctrl Pts',(-19.692058671699,-17.064189387728,1.64912934088624));
#160038=CARTESIAN_POINT('Ctrl Pts',(-19.7019115533862,-17.0692133698439,
1.64846470424387));
#160039=CARTESIAN_POINT('Ctrl Pts',(-19.7081490069026,-17.0724330324869,
1.64804480499293));
#160040=CARTESIAN_POINT('Ctrl Pts',(-19.7220607645375,-17.0797018900318,
1.64710993832238));
#160041=CARTESIAN_POINT('Ctrl Pts',(-19.7297264643217,-17.0837673857878,
1.64659594184478));
#160042=CARTESIAN_POINT('Ctrl Pts',(-19.7533094442116,-17.0964609814777,
1.64501751795104));
#160043=CARTESIAN_POINT('Ctrl Pts',(-19.7691416062477,-17.1052464452622,
1.64396189282592));
#160044=CARTESIAN_POINT('Ctrl Pts',(-19.8297871908316,-17.1399244212828,
1.63992637847333));
#160045=CARTESIAN_POINT('Ctrl Pts',(-19.8737607067238,-17.1672552772322,
1.63701732715713));
#160046=CARTESIAN_POINT('Ctrl Pts',(-20.0313720688146,-17.273419179665,
1.62649131783225));
#160047=CARTESIAN_POINT('Ctrl Pts',(-20.1382110213948,-17.361716481028,
1.61913727159696));
#160048=CARTESIAN_POINT('Ctrl Pts',(-20.2625557831996,-17.4868515023126,
1.60939918489813));
#160049=CARTESIAN_POINT('Ctrl Pts',(-20.2886957421772,-17.5146190931428,
1.60727671698471));
#160050=CARTESIAN_POINT('Ctrl Pts',(-20.3545778677189,-17.5885041754545,
1.60169997695476));
#160051=CARTESIAN_POINT('Ctrl Pts',(-20.3931038409899,-17.6356539469045,
1.59820821953337));
#160052=CARTESIAN_POINT('Ctrl Pts',(-20.4369346911153,-17.6942818961194,
1.59390846431907));
#160053=CARTESIAN_POINT('Ctrl Pts',(-20.4442396234637,-17.7042332703202,
1.59318007342477));
#160054=CARTESIAN_POINT('Ctrl Pts',(-20.4561120697594,-17.7207070168619,
1.59197634644628));
#160055=CARTESIAN_POINT('Ctrl Pts',(-20.4607306240394,-17.7271923659234,
1.5915029862539));
#160056=CARTESIAN_POINT('Ctrl Pts',(-20.4689812727146,-17.7389173041586,
1.59064805307481));
#160057=CARTESIAN_POINT('Ctrl Pts',(-20.47262650721,-17.7441475625423,1.5902669898041));
#160058=CARTESIAN_POINT('Ctrl Pts',(-20.4803533574746,-17.7553416622544,
1.58945202523937));
#160059=CARTESIAN_POINT('Ctrl Pts',(-20.4844281627048,-17.7613100858529,
1.58901787138294));
#160060=CARTESIAN_POINT('Ctrl Pts',(-20.4953522979815,-17.7774880884497,
1.5878419722303));
#160061=CARTESIAN_POINT('Ctrl Pts',(-20.5021433032203,-17.7877365430192,
1.58709804124387));
#160062=CARTESIAN_POINT('Ctrl Pts',(-20.536092156357,-17.8399516236412,
1.58331219133672));
#160063=CARTESIAN_POINT('Ctrl Pts',(-20.5618449064526,-17.8828086852482,
1.58021863594657));
#160064=CARTESIAN_POINT('Ctrl Pts',(-20.6323246084185,-18.0100994383821,
1.57106281893894));
#160065=CARTESIAN_POINT('Ctrl Pts',(-20.6728801940735,-18.0966912835451,
1.56486873759636));
#160066=CARTESIAN_POINT('Ctrl Pts',(-20.7126288499503,-18.1990579622526,
1.55764706557724));
#160067=CARTESIAN_POINT('Ctrl Pts',(-20.7176731540642,-18.2124497783799,
1.55670439439033));
#160068=CARTESIAN_POINT('Ctrl Pts',(-20.7225805817976,-18.2258896298098,
1.55576077259462));
#160069=CARTESIAN_POINT('',(-20.8479201479212,-18.9528282578495,2.08900081515195));
#160070=CARTESIAN_POINT('Ctrl Pts',(-20.7225805737606,-18.2258896077991,
1.33163200235201));
#160071=CARTESIAN_POINT('Ctrl Pts',(-20.7210219544926,-18.2216210557561,
1.3319018864381));
#160072=CARTESIAN_POINT('Ctrl Pts',(-20.7194496013543,-18.217357549551,
1.33217222556062));
#160073=CARTESIAN_POINT('Ctrl Pts',(-20.7156191687899,-18.2070732799466,
1.33282621705284));
#160074=CARTESIAN_POINT('Ctrl Pts',(-20.7133473748435,-18.2010577141641,
1.33321032421728));
#160075=CARTESIAN_POINT('Ctrl Pts',(-20.7085566090551,-18.1885448558727,
1.33401261267353));
#160076=CARTESIAN_POINT('Ctrl Pts',(-20.7060328960234,-18.1820494725944,
1.33443094956896));
#160077=CARTESIAN_POINT('Ctrl Pts',(-20.6993949332336,-18.1652118167104,
1.33552031141627));
#160078=CARTESIAN_POINT('Ctrl Pts',(-20.695231145335,-18.1548894204065,
1.3361930006093));
#160079=CARTESIAN_POINT('Ctrl Pts',(-20.6767885701682,-18.1101880490247,
1.33912757212948));
#160080=CARTESIAN_POINT('Ctrl Pts',(-20.6616864855575,-18.0761579328253,
1.34141723280241));
#160081=CARTESIAN_POINT('Ctrl Pts',(-20.6191743280709,-17.9867963515471,
1.34758323029482));
#160082=CARTESIAN_POINT('Ctrl Pts',(-20.5902290777744,-17.9322388444417,
1.35150933954297));
#160083=CARTESIAN_POINT('Ctrl Pts',(-20.4847190248718,-17.7527841636449,
1.36495843115519));
#160084=CARTESIAN_POINT('Ctrl Pts',(-20.3975959098247,-17.6345861827553,
1.37476371722997));
#160085=CARTESIAN_POINT('Ctrl Pts',(-20.2858384039415,-17.5119070556623,
1.38559624898239));
#160086=CARTESIAN_POINT('Ctrl Pts',(-20.2724921199729,-17.4976574853576,
1.38686505685932));
#160087=CARTESIAN_POINT('Ctrl Pts',(-20.2223180981013,-17.4455513872136,
1.39153847476712));
#160088=CARTESIAN_POINT('Ctrl Pts',(-20.1842716027264,-17.4088890279648,
1.39489468586293));
#160089=CARTESIAN_POINT('Ctrl Pts',(-20.1384093900395,-17.3678917866915,
1.39868921784772));
#160090=CARTESIAN_POINT('Ctrl Pts',(-20.1318927168922,-17.3621382059105,
1.39922274062836));
#160091=CARTESIAN_POINT('Ctrl Pts',(-20.121966379467,-17.3534824452643,
1.40002664734232));
#160092=CARTESIAN_POINT('Ctrl Pts',(-20.1185827365551,-17.3505507532817,
1.40029915277575));
#160093=CARTESIAN_POINT('Ctrl Pts',(-20.1124893284901,-17.3453049858822,
1.40078711718506));
#160094=CARTESIAN_POINT('Ctrl Pts',(-20.1097830114673,-17.3429870096592,
1.40100286219499));
#160095=CARTESIAN_POINT('Ctrl Pts',(-20.1038860708835,-17.3379620016668,
1.40147083342266));
#160096=CARTESIAN_POINT('Ctrl Pts',(-20.1006932809769,-17.3352576013192,
1.40172286696978));
#160097=CARTESIAN_POINT('Ctrl Pts',(-20.0916937757519,-17.3276804279265,
1.40242958083411));
#160098=CARTESIAN_POINT('Ctrl Pts',(-20.0858688089899,-17.322829294348,
1.40288270525778));
#160099=CARTESIAN_POINT('Ctrl Pts',(-20.0507101727442,-17.2938669780083,
1.40559284898832));
#160100=CARTESIAN_POINT('Ctrl Pts',(-20.0207562176211,-17.2705156445126,
1.40779853364709));
#160101=CARTESIAN_POINT('Ctrl Pts',(-19.9196806853442,-17.1960036163395,
1.41496687867876));
#160102=CARTESIAN_POINT('Ctrl Pts',(-19.8460091755805,-17.1484479461188,
1.41976125592826));
#160103=CARTESIAN_POINT('Ctrl Pts',(-19.6172807610509,-17.020160746121,
1.43402853696588));
#160104=CARTESIAN_POINT('Ctrl Pts',(-19.454997698073,-16.9539150702231,
1.44342150466696));
#160105=CARTESIAN_POINT('Ctrl Pts',(-19.2641706547445,-16.9023318158306,
1.45490744633315));
#160106=CARTESIAN_POINT('Ctrl Pts',(-19.2418171655502,-16.8966795254018,
1.45625815047753));
#160107=CARTESIAN_POINT('Ctrl Pts',(-19.2100738278698,-16.8892023728475,
1.45818538481083));
#160108=CARTESIAN_POINT('Ctrl Pts',(-19.2007565986402,-16.8870741869883,
1.4587521657513));
#160109=CARTESIAN_POINT('Ctrl Pts',(-19.1855972773244,-16.8837194267867,
1.45967623934344));
#160110=CARTESIAN_POINT('Ctrl Pts',(-19.1797637795532,-16.8824543295368,
1.46003229214611));
#160111=CARTESIAN_POINT('Ctrl Pts',(-19.1675440460856,-16.8798583265037,
1.46077912510929));
#160112=CARTESIAN_POINT('Ctrl Pts',(-19.1611568617154,-16.8785322358552,
1.46117005519013));
#160113=CARTESIAN_POINT('Ctrl Pts',(-19.1459515160023,-16.8754485807152,
1.46210209142747));
#160114=CARTESIAN_POINT('Ctrl Pts',(-19.1371281390039,-16.8737176447569,
1.46264404196999));
#160115=CARTESIAN_POINT('Ctrl Pts',(-19.1073845945208,-16.868079208825,
1.46447482370204));
#160116=CARTESIAN_POINT('Ctrl Pts',(-19.0864171273515,-16.8644310704145,
1.46577186589623));
#160117=CARTESIAN_POINT('Ctrl Pts',(-18.9079913323057,-16.8361513397617,
1.47686732111653));
#160118=CARTESIAN_POINT('Ctrl Pts',(-18.7482991778209,-16.829061969009,
1.4872391166112));
#160119=CARTESIAN_POINT('Ctrl Pts',(-18.4580418721694,-16.8489402182039,
1.5064573147894));
#160120=CARTESIAN_POINT('Ctrl Pts',(-18.3278408708816,-16.8701608592363,
1.51519649684384));
#160121=CARTESIAN_POINT('Ctrl Pts',(-18.1852106042422,-16.9073075923962,
1.52439152159694));
#160122=CARTESIAN_POINT('Ctrl Pts',(-18.1700200043961,-16.9114453105206,
1.5253656186187));
#160123=CARTESIAN_POINT('Ctrl Pts',(-18.1492990465425,-16.9173385001607,
1.52668587666152));
#160124=CARTESIAN_POINT('Ctrl Pts',(-18.1437280856433,-16.9189476905789,
1.52703999355517));
#160125=CARTESIAN_POINT('Ctrl Pts',(-18.1348887763288,-16.9215403501383,
1.52760044325141));
#160126=CARTESIAN_POINT('Ctrl Pts',(-18.1316161212942,-16.9225088541452,
1.52780763364718));
#160127=CARTESIAN_POINT('Ctrl Pts',(-18.1248645275822,-16.9245246793535,
1.52823441316738));
#160128=CARTESIAN_POINT('Ctrl Pts',(-18.1213859413173,-16.9255730423128,
1.52845393405084));
#160129=CARTESIAN_POINT('Ctrl Pts',(-18.1131075133796,-16.9280912277091,
1.52897551502527));
#160130=CARTESIAN_POINT('Ctrl Pts',(-18.1083101307743,-16.929569188519,
1.52927710045831));
#160131=CARTESIAN_POINT('Ctrl Pts',(-18.0921660074794,-16.9346057558936,
1.53028986635736));
#160132=CARTESIAN_POINT('Ctrl Pts',(-18.0808437684171,-16.9382429734756,
1.5309965942119));
#160133=CARTESIAN_POINT('Ctrl Pts',(-17.9458033372821,-16.9828828663101,
1.53938988256371));
#160134=CARTESIAN_POINT('Ctrl Pts',(-17.8260773200397,-17.0351373174273,
1.5464801575605));
#160135=CARTESIAN_POINT('Ctrl Pts',(-17.5698310643447,-17.1764098954642,
1.56237647312155));
#160136=CARTESIAN_POINT('Ctrl Pts',(-17.4372483850795,-17.2707987052116,
1.57115794197504));
#160137=CARTESIAN_POINT('Ctrl Pts',(-17.2991238382424,-17.3952783531964,
1.58195474181514));
#160138=CARTESIAN_POINT('Ctrl Pts',(-17.2817684698181,-17.4114561346233,
1.58334401751069));
#160139=CARTESIAN_POINT('Ctrl Pts',(-17.2577289295277,-17.4346318190066,
1.5853169538283));
#160140=CARTESIAN_POINT('Ctrl Pts',(-17.2508148460581,-17.4413894397892,
1.58589021905392));
#160141=CARTESIAN_POINT('Ctrl Pts',(-17.2396930298643,-17.4524095397645,
1.58682197503756));
#160142=CARTESIAN_POINT('Ctrl Pts',(-17.2354566224797,-17.4566429810976,
1.58717918397107));
#160143=CARTESIAN_POINT('Ctrl Pts',(-17.2266556023215,-17.4655127992216,
1.58792611597125));
#160144=CARTESIAN_POINT('Ctrl Pts',(-17.2220942909596,-17.4701523503427,
1.58831597868886));
#160145=CARTESIAN_POINT('Ctrl Pts',(-17.2113461570787,-17.4811861310638,
1.5892412241861));
#160146=CARTESIAN_POINT('Ctrl Pts',(-17.2051781514898,-17.4875984450436,
1.58977741902104));
#160147=CARTESIAN_POINT('Ctrl Pts',(-17.1847724640048,-17.5090818153691,
1.59156897789293));
#160148=CARTESIAN_POINT('Ctrl Pts',(-17.1707161210026,-17.524322756537,
1.59283208234356));
#160149=CARTESIAN_POINT('Ctrl Pts',(-17.0968763169071,-17.6067835057797,
1.59962665289158));
#160150=CARTESIAN_POINT('Ctrl Pts',(-17.0412065289614,-17.6775479476279,
1.60532609872083));
#160151=CARTESIAN_POINT('Ctrl Pts',(-16.9134127850588,-17.8631952220271,
1.61993219425587));
#160152=CARTESIAN_POINT('Ctrl Pts',(-16.8475006227232,-17.9818711046256,
1.62898456836519));
#160153=CARTESIAN_POINT('Ctrl Pts',(-16.7632165096948,-18.1752121343744,
1.64277664843119));
#160154=CARTESIAN_POINT('Ctrl Pts',(-16.7367707097356,-18.2459797246284,
1.64763601727772));
#160155=CARTESIAN_POINT('Ctrl Pts',(-16.7113175913434,-18.3270720321725,
1.65288539227348));
#160156=CARTESIAN_POINT('Ctrl Pts',(-16.7085359778694,-18.3361472627092,
1.65346843799303));
#160157=CARTESIAN_POINT('Ctrl Pts',(-16.7045028214792,-18.3496287054191,
1.65432769977264));
#160158=CARTESIAN_POINT('Ctrl Pts',(-16.7032044327264,-18.3540206199109,
1.65460654983214));
#160159=CARTESIAN_POINT('Ctrl Pts',(-16.7009188439558,-18.3618451308687,
1.65510138478916));
#160160=CARTESIAN_POINT('Ctrl Pts',(-16.6999260703997,-18.3652760391831,
1.65531769101646));
#160161=CARTESIAN_POINT('Ctrl Pts',(-16.6978093832441,-18.3726610066657,
1.65578183770309));
#160162=CARTESIAN_POINT('Ctrl Pts',(-16.6966883049157,-18.3766158199115,
1.65602951240855));
#160163=CARTESIAN_POINT('Ctrl Pts',(-16.6936234206313,-18.387549036666,
1.65671183573583));
#160164=CARTESIAN_POINT('Ctrl Pts',(-16.6917038817193,-18.3945342662098,
1.65714509628754));
#160165=CARTESIAN_POINT('Ctrl Pts',(-16.6813503346419,-18.4329822939229,
1.65951585290567));
#160166=CARTESIAN_POINT('Ctrl Pts',(-16.6736069943411,-18.4646285266987,
1.66141581912851));
#160167=CARTESIAN_POINT('Ctrl Pts',(-16.6315967226036,-18.6552789435078,
1.67262441599101));
#160168=CARTESIAN_POINT('Ctrl Pts',(-16.6150141576487,-18.8176357407558,
1.68122134734676));
#160169=CARTESIAN_POINT('Ctrl Pts',(-16.6187512459146,-19.0971247355112,
1.69652331610837));
#160170=CARTESIAN_POINT('Ctrl Pts',(-16.6299803464647,-19.2135999186024,
1.70304546133171));
#160171=CARTESIAN_POINT('Ctrl Pts',(-16.6532984879152,-19.3426077519539,
1.71072563355701));
#160172=CARTESIAN_POINT('Ctrl Pts',(-16.6559824447445,-19.3566433286477,
1.71156713493904));
#160173=CARTESIAN_POINT('Ctrl Pts',(-16.6604801942807,-19.3789380466631,
1.71291370211074));
#160174=CARTESIAN_POINT('Ctrl Pts',(-16.662201760899,-19.3872155025885,
1.71341582668597));
#160175=CARTESIAN_POINT('Ctrl Pts',(-16.6653254417953,-19.4017957999027,
1.7143042270112));
#160176=CARTESIAN_POINT('Ctrl Pts',(-16.666706902714,-19.4081029904108,
1.7146898367329));
#160177=CARTESIAN_POINT('Ctrl Pts',(-16.6696238845199,-19.4211352011611,
1.715489339632));
#160178=CARTESIAN_POINT('Ctrl Pts',(-16.6711634629842,-19.4278592259625,
1.71590335916317));
#160179=CARTESIAN_POINT('Ctrl Pts',(-16.6751997329196,-19.44509967371,1.71696885089497));
#160180=CARTESIAN_POINT('Ctrl Pts',(-16.6777441292851,-19.4556046220085,
1.71762185256684));
#160181=CARTESIAN_POINT('Ctrl Pts',(-16.6886998391513,-19.4993693525557,
1.72035841401918));
#160182=CARTESIAN_POINT('Ctrl Pts',(-16.6978381780862,-19.5324401560304,
1.72246531639172));
#160183=CARTESIAN_POINT('Ctrl Pts',(-16.7237400580971,-19.618018735276,
1.72802300284975));
#160184=CARTESIAN_POINT('Ctrl Pts',(-16.741756817348,-19.67011717,1.73151222861715));
#160185=CARTESIAN_POINT('Ctrl Pts',(-16.8015463316852,-19.8233666406223,
1.74208586299712));
#160186=CARTESIAN_POINT('Ctrl Pts',(-16.8491460256669,-19.9220407373757,
1.74931865078059));
#160187=CARTESIAN_POINT('Ctrl Pts',(-16.9285119151277,-20.0584575806889,
1.75974409646991));
#160188=CARTESIAN_POINT('Ctrl Pts',(-16.9543026736481,-20.0994812704575,
1.7629376964586));
#160189=CARTESIAN_POINT('Ctrl Pts',(-16.9913860610773,-20.1542052948247,
1.76725022361704));
#160190=CARTESIAN_POINT('Ctrl Pts',(-17.0014762148944,-20.1687013888062,
1.76839776179512));
#160191=CARTESIAN_POINT('Ctrl Pts',(-17.0427697674996,-20.2264706188703,
1.77298712451094));
#160192=CARTESIAN_POINT('Ctrl Pts',(-17.0754251906874,-20.2686873950892,
1.77637848219373));
#160193=CARTESIAN_POINT('Ctrl Pts',(-17.1152358902283,-20.3163195363192,
1.78020794085174));
#160194=CARTESIAN_POINT('Ctrl Pts',(-17.1208694789783,-20.3229759182513,
1.78074315405901));
#160195=CARTESIAN_POINT('Ctrl Pts',(-17.1294614663248,-20.3330015179272,
1.7815491160224));
#160196=CARTESIAN_POINT('Ctrl Pts',(-17.1323896228271,-20.3363963663465,
1.78182200171947));
#160197=CARTESIAN_POINT('Ctrl Pts',(-17.1376648488982,-20.3424732239937,
1.78231038281676));
#160198=CARTESIAN_POINT('Ctrl Pts',(-17.1400079159528,-20.3451586190615,
1.78252616634789));
#160199=CARTESIAN_POINT('Ctrl Pts',(-17.1451137142276,-20.3509806436042,
1.78299391257254));
#160200=CARTESIAN_POINT('Ctrl Pts',(-17.1478789477303,-20.3541150018936,
1.78324568425772));
#160201=CARTESIAN_POINT('Ctrl Pts',(-17.1556718305835,-20.362895582882,
1.78395093748102));
#160202=CARTESIAN_POINT('Ctrl Pts',(-17.1607205268138,-20.3685231587688,
1.78440287335818));
#160203=CARTESIAN_POINT('Ctrl Pts',(-17.1910715248373,-20.4019917354561,
1.78709109148857));
#160204=CARTESIAN_POINT('Ctrl Pts',(-17.2170838484821,-20.4291831623205,
1.78927699878569));
#160205=CARTESIAN_POINT('Ctrl Pts',(-17.305044979401,-20.5163558918042,
1.7963489930711));
#160206=CARTESIAN_POINT('Ctrl Pts',(-17.3699362097486,-20.5732507928181,
1.80107191265039));
#160207=CARTESIAN_POINT('Ctrl Pts',(-17.5777787663376,-20.7341429368544,
1.81537586188073));
#160208=CARTESIAN_POINT('Ctrl Pts',(-17.7303977265982,-20.8243399315862,
1.82486537988993));
#160209=CARTESIAN_POINT('Ctrl Pts',(-17.9134587690612,-20.9036469625251,
1.83645910036613));
#160210=CARTESIAN_POINT('Ctrl Pts',(-17.9346247683343,-20.9124114253736,
1.83780125503696));
#160211=CARTESIAN_POINT('Ctrl Pts',(-17.9647936036023,-20.9243339953728,
1.83971835623945));
#160212=CARTESIAN_POINT('Ctrl Pts',(-17.9736824199401,-20.9277775792068,
1.84028369346282));
#160213=CARTESIAN_POINT('Ctrl Pts',(-17.9881701654244,-20.9332779795624,
1.84120604207386));
#160214=CARTESIAN_POINT('Ctrl Pts',(-17.9937551266535,-20.9353713975967,
1.84156182274692));
#160215=CARTESIAN_POINT('Ctrl Pts',(-18.0054700992802,-20.9397061613955,
1.84230859791443));
#160216=CARTESIAN_POINT('Ctrl Pts',(-18.0116017702445,-20.9419428123586,
1.84269974458839));
#160217=CARTESIAN_POINT('Ctrl Pts',(-18.0262242784434,-20.9472001770425,
1.84363324542762));
#160218=CARTESIAN_POINT('Ctrl Pts',(-18.0347242025274,-20.9501950789746,
1.84417645121177));
#160219=CARTESIAN_POINT('Ctrl Pts',(-18.0634764320616,-20.9601198472911,
1.84601599330436));
#160220=CARTESIAN_POINT('Ctrl Pts',(-18.083814126962,-20.9667966284326,
1.84732064871243));
#160221=CARTESIAN_POINT('Ctrl Pts',(-18.1954346345112,-21.0015751705085,
1.85450219302446));
#160222=CARTESIAN_POINT('Ctrl Pts',(-18.2884261445281,-21.0237795991593,
1.86056924158792));
#160223=CARTESIAN_POINT('Ctrl Pts',(-18.55057327573,-21.0679069297578,1.87784578984168));
#160224=CARTESIAN_POINT('Ctrl Pts',(-18.7213462302002,-21.0758042080899,
1.88933906399189));
#160225=CARTESIAN_POINT('Ctrl Pts',(-18.9278237861098,-21.0604280809679,
1.90255300589767));
#160226=CARTESIAN_POINT('Ctrl Pts',(-18.9643580577657,-21.0567499074251,
1.90486206446987));
#160227=CARTESIAN_POINT('Ctrl Pts',(-19.0078607894498,-21.0512237151479,
1.90756247423834));
#160228=CARTESIAN_POINT('Ctrl Pts',(-19.0149365169512,-21.0502884966069,
1.90800013635016));
#160229=CARTESIAN_POINT('Ctrl Pts',(-19.0264764509981,-21.0487038116536,
1.90871123005467));
#160230=CARTESIAN_POINT('Ctrl Pts',(-19.0309434835953,-21.0480758375145,
1.90898582907012));
#160231=CARTESIAN_POINT('Ctrl Pts',(-19.0389380785928,-21.0469258897975,
1.90947605035841));
#160232=CARTESIAN_POINT('Ctrl Pts',(-19.0424663476806,-21.0464092791225,
1.90969197030715));
#160233=CARTESIAN_POINT('Ctrl Pts',(-19.0501069340053,-21.0452708146114,
1.91015861429498));
#160234=CARTESIAN_POINT('Ctrl Pts',(-19.0542187161271,-21.044645758736,
1.91040915485919));
#160235=CARTESIAN_POINT('Ctrl Pts',(-19.0657052710019,-21.0428649729898,
1.91110749178292));
#160236=CARTESIAN_POINT('Ctrl Pts',(-19.0730758962609,-21.0416823352908,
1.91155379083758));
#160237=CARTESIAN_POINT('Ctrl Pts',(-19.1159589955889,-21.0345687559295,
1.91414068888689));
#160238=CARTESIAN_POINT('Ctrl Pts',(-19.1513240830883,-21.0277712434622,
1.91623523009846));
#160239=CARTESIAN_POINT('Ctrl Pts',(-19.264701771025,-21.0029638676532,
1.92287411602897));
#160240=CARTESIAN_POINT('Ctrl Pts',(-19.3418756446818,-20.9814300577038,
1.92727730868305));
#160241=CARTESIAN_POINT('Ctrl Pts',(-19.5934291658621,-20.8955962683125,
1.94176725306628));
#160242=CARTESIAN_POINT('Ctrl Pts',(-19.7605316247363,-20.8127556969666,
1.95170046577222));
#160243=CARTESIAN_POINT('Ctrl Pts',(-19.9330160070807,-20.6968603277342,
1.96378661426745));
#160244=CARTESIAN_POINT('Ctrl Pts',(-19.9511565896448,-20.6842548111247,
1.96508152927113));
#160245=CARTESIAN_POINT('Ctrl Pts',(-19.9759640131194,-20.6664345708322,
1.96688708733253));
#160246=CARTESIAN_POINT('Ctrl Pts',(-19.9828022141545,-20.6614600124947,
1.96738851347877));
#160247=CARTESIAN_POINT('Ctrl Pts',(-19.9945033272015,-20.6528401734789,
1.96825303460205));
#160248=CARTESIAN_POINT('Ctrl Pts',(-19.9993807174492,-20.6492146512237,
1.96861535943089));
#160249=CARTESIAN_POINT('Ctrl Pts',(-20.0092361051029,-20.6418227250401,
1.96935151421115));
#160250=CARTESIAN_POINT('Ctrl Pts',(-20.0142131874279,-20.6380552064691,
1.9697253856626));
#160251=CARTESIAN_POINT('Ctrl Pts',(-20.0257417283302,-20.6292479326595,
1.97059634111213));
#160252=CARTESIAN_POINT('Ctrl Pts',(-20.0322804456549,-20.6241917359335,
1.97109407196262));
#160253=CARTESIAN_POINT('Ctrl Pts',(-20.0459635004629,-20.6134824016452,
1.97214361526178));
#160254=CARTESIAN_POINT('Ctrl Pts',(-20.0531012773149,-20.6078211901165,
1.972695744184));
#160255=CARTESIAN_POINT('Ctrl Pts',(-20.0720063796626,-20.5926270967978,
1.9741706143622));
#160256=CARTESIAN_POINT('Ctrl Pts',(-20.0837081672744,-20.5830138525671,
1.97509656982422));
#160257=CARTESIAN_POINT('Ctrl Pts',(-20.1190797102583,-20.5533141121942,
1.97793603794961));
#160258=CARTESIAN_POINT('Ctrl Pts',(-20.1424108560363,-20.5328324999823,
1.97986538233887));
#160259=CARTESIAN_POINT('Ctrl Pts',(-20.2894008071012,-20.3979575807575,
1.99239225406707));
#160260=CARTESIAN_POINT('Ctrl Pts',(-20.3994672991205,-20.2696747844113,
2.00357954075189));
#160261=CARTESIAN_POINT('Ctrl Pts',(-20.5482428252334,-20.0474532103545,
2.02119626949266));
#160262=CARTESIAN_POINT('Ctrl Pts',(-20.5974979042015,-19.9613933731637,
2.02764856408787));
#160263=CARTESIAN_POINT('Ctrl Pts',(-20.6447646756313,-19.8634611024349,
2.03436716012927));
#160264=CARTESIAN_POINT('Ctrl Pts',(-20.6489187125123,-19.854701124164,
2.03496283317341));
#160265=CARTESIAN_POINT('Ctrl Pts',(-20.6549630922215,-19.8417253157629,
2.03583703971683));
#160266=CARTESIAN_POINT('Ctrl Pts',(-20.6568999800088,-19.8375314827846,
2.03611833908499));
#160267=CARTESIAN_POINT('Ctrl Pts',(-20.6603117271764,-19.8300802440368,
2.03661587282211));
#160268=CARTESIAN_POINT('Ctrl Pts',(-20.6617920753468,-19.8268254112306,
2.03683244207524));
#160269=CARTESIAN_POINT('Ctrl Pts',(-20.6649460105192,-19.8198439906,2.03729532896275));
#160270=CARTESIAN_POINT('Ctrl Pts',(-20.6666170552115,-19.8161163151537,
2.03754149041177));
#160271=CARTESIAN_POINT('Ctrl Pts',(-20.6711741826595,-19.805871179959,
2.03821537891727));
#160272=CARTESIAN_POINT('Ctrl Pts',(-20.6740381866446,-19.7993438756363,
2.03864177403876));
#160273=CARTESIAN_POINT('Ctrl Pts',(-20.6891489348888,-19.7644269710614,
2.04090765878748));
#160274=CARTESIAN_POINT('Ctrl Pts',(-20.7008062983066,-19.7357845066017,
2.0427134257502));
#160275=CARTESIAN_POINT('Ctrl Pts',(-20.7341848200402,-19.6483324694177,
2.04809763337037));
#160276=CARTESIAN_POINT('Ctrl Pts',(-20.7539265969983,-19.5888013137211,
2.05158937219301));
#160277=CARTESIAN_POINT('Ctrl Pts',(-20.8240164192346,-19.3411372216552,
2.06573528918478));
#160278=CARTESIAN_POINT('Ctrl Pts',(-20.8509329970117,-19.147403052089,
2.07601660755508));
#160279=CARTESIAN_POINT('Ctrl Pts',(-20.8509998750793,-18.9527272648688,
2.08722596880618));
#160280=CARTESIAN_POINT('Ctrl Pts',(-20.7227693997001,-18.2258206865925,
2.13351567424346));
#160281=CARTESIAN_POINT('Ctrl Pts',(-20.8048847893556,-18.4580153825123,
2.11869587583647));
#160282=CARTESIAN_POINT('Ctrl Pts',(-20.8469524796136,-18.7055595108412,
2.10387607742949));
#160283=CARTESIAN_POINT('Ctrl Pts',(-20.8478239065824,-18.9528314138757,
2.0890562790225));
#160284=CARTESIAN_POINT('Origin',(-18.734,-18.952,0.));
#160285=CARTESIAN_POINT('',(-20.7225805742799,-18.2258896092214,3.15472458816501));
#160286=CARTESIAN_POINT('',(-20.7225805736403,-18.2258896074698,2.9354567758078));
#160287=CARTESIAN_POINT('',(-20.7225805737622,-18.2258896078036,0.));
#160288=CARTESIAN_POINT('',(-20.8509999550624,-18.9524361948928,3.11292720174657));
#160289=CARTESIAN_POINT('Ctrl Pts',(-20.7225805742799,-18.2258896092214,
3.15472458816501));
#160290=CARTESIAN_POINT('Ctrl Pts',(-20.7854688877252,-18.398120278352,
3.14471652909388));
#160291=CARTESIAN_POINT('Ctrl Pts',(-20.8257155399036,-18.5777840081126,
3.13493381366904));
#160292=CARTESIAN_POINT('Ctrl Pts',(-20.8447697717378,-18.787446767605,
3.12275006577916));
#160293=CARTESIAN_POINT('Ctrl Pts',(-20.8467072353025,-18.8145415183661,
3.1211630550673));
#160294=CARTESIAN_POINT('Ctrl Pts',(-20.8486554031854,-18.8518703121812,
3.11895650893829));
#160295=CARTESIAN_POINT('Ctrl Pts',(-20.8491140971062,-18.8620790387422,
3.11835100055614));
#160296=CARTESIAN_POINT('Ctrl Pts',(-20.849728275663,-18.8783794155952,
3.11738074779484));
#160297=CARTESIAN_POINT('Ctrl Pts',(-20.8499314061552,-18.8844691911777,
3.11701750020532));
#160298=CARTESIAN_POINT('Ctrl Pts',(-20.8502862993201,-18.8966923163463,
3.11628683852707));
#160299=CARTESIAN_POINT('Ctrl Pts',(-20.8504376956001,-18.9028256166745,
3.11591941655117));
#160300=CARTESIAN_POINT('Ctrl Pts',(-20.8507174561215,-18.9165831187247,
3.11509344704485));
#160301=CARTESIAN_POINT('Ctrl Pts',(-20.8508312920901,-18.924207501338,
3.11463444858109));
#160302=CARTESIAN_POINT('Ctrl Pts',(-20.850969363229,-18.9387001154212,
3.11375954974115));
#160303=CARTESIAN_POINT('Ctrl Pts',(-20.8510013701757,-18.9455681758564,
3.11334390027904));
#160304=CARTESIAN_POINT('Ctrl Pts',(-20.8509999550624,-18.9524361948928,
3.11292720174657));
#160305=CARTESIAN_POINT('Ctrl Pts',(-20.8509999552293,-18.9524353839625,
3.11292725094757));
#160306=CARTESIAN_POINT('Ctrl Pts',(-20.8509977695416,-18.9630630163438,
3.11228244814287));
#160307=CARTESIAN_POINT('Ctrl Pts',(-20.8509155556714,-18.9736903655048,
3.11163514383949));
#160308=CARTESIAN_POINT('Ctrl Pts',(-20.8504244941627,-19.0058552024136,
3.10966822327283));
#160309=CARTESIAN_POINT('Ctrl Pts',(-20.8497669477593,-19.0273869463236,
3.10834094914419));
#160310=CARTESIAN_POINT('Ctrl Pts',(-20.8411521705333,-19.215390635193,
3.09665719184966));
#160311=CARTESIAN_POINT('Ctrl Pts',(-20.8138911677769,-19.3803675993858,
3.08568599821112));
#160312=CARTESIAN_POINT('Ctrl Pts',(-20.7441525987017,-19.6213898137481,
3.06911193324209));
#160313=CARTESIAN_POINT('Ctrl Pts',(-20.7159027153627,-19.7009056435757,
3.06356237554816));
#160314=CARTESIAN_POINT('Ctrl Pts',(-20.6684879343648,-19.812711331155,
3.05581333095038));
#160315=CARTESIAN_POINT('Ctrl Pts',(-20.6530940403106,-19.8465088136624,
3.05347889612171));
#160316=CARTESIAN_POINT('Ctrl Pts',(-20.6335168613556,-19.8866557758572,
3.0507305738603));
#160317=CARTESIAN_POINT('Ctrl Pts',(-20.6301795560165,-19.8934078930938,
3.05026920498877));
#160318=CARTESIAN_POINT('Ctrl Pts',(-20.624937023246,-19.9038737272136,
3.04955558390719));
#160319=CARTESIAN_POINT('Ctrl Pts',(-20.6230567674507,-19.9075997846823,
3.04930181776486));
#160320=CARTESIAN_POINT('Ctrl Pts',(-20.6195502374123,-19.914497796227,
3.04883261078509));
#160321=CARTESIAN_POINT('Ctrl Pts',(-20.6179269857595,-19.9176711749685,
3.04861699097109));
#160322=CARTESIAN_POINT('Ctrl Pts',(-20.6142402441416,-19.9248338996428,
3.04813082924854));
#160323=CARTESIAN_POINT('Ctrl Pts',(-20.6121720748999,-19.9288207767573,
3.04786058619553));
#160324=CARTESIAN_POINT('Ctrl Pts',(-20.6060336744734,-19.9405624023329,
3.04706568169849));
#160325=CARTESIAN_POINT('Ctrl Pts',(-20.6019279348417,-19.948298618839,
3.04654320709552));
#160326=CARTESIAN_POINT('Ctrl Pts',(-20.5720879301076,-20.0036915644863,
3.0428096905925));
#160327=CARTESIAN_POINT('Ctrl Pts',(-20.5445788662825,-20.0503749891729,
3.03970317627656));
#160328=CARTESIAN_POINT('Ctrl Pts',(-20.4249300121516,-20.2366858158767,
3.0272593482136));
#160329=CARTESIAN_POINT('Ctrl Pts',(-20.3181911824819,-20.3662163134544,
3.0184536253374));
#160330=CARTESIAN_POINT('Ctrl Pts',(-20.153980467728,-20.5232860707889,
3.0058658422293));
#160331=CARTESIAN_POINT('Ctrl Pts',(-20.1089106884917,-20.5628706484787,
3.0024966791266));
#160332=CARTESIAN_POINT('Ctrl Pts',(-20.0338325717932,-20.6233628136522,
2.99695987334473));
#160333=CARTESIAN_POINT('Ctrl Pts',(-20.004856256281,-20.6455000770281,
2.99483998983451));
#160334=CARTESIAN_POINT('Ctrl Pts',(-19.9686958267715,-20.6716750179054,
2.99220825633883));
#160335=CARTESIAN_POINT('Ctrl Pts',(-19.9620399704185,-20.6764343362604,
2.99172440933288));
#160336=CARTESIAN_POINT('Ctrl Pts',(-19.9491498834455,-20.6855390121142,
2.99078835132776));
#160337=CARTESIAN_POINT('Ctrl Pts',(-19.9429195097312,-20.6898896289598,
2.99033635047447));
#160338=CARTESIAN_POINT('Ctrl Pts',(-19.9366256366146,-20.694234364416,
2.98988014794073));
#160339=CARTESIAN_POINT('Ctrl Pts',(-19.9365853635496,-20.6942621633299,
2.98987722882094));
#160340=CARTESIAN_POINT('Ctrl Pts',(-19.9365031663644,-20.6943188966083,
2.98987127094159));
#160341=CARTESIAN_POINT('Ctrl Pts',(-19.9364612421273,-20.6943478308812,
2.98986823217493));
#160342=CARTESIAN_POINT('Ctrl Pts',(-19.9363756324267,-20.6944069103868,
2.9898620270206));
#160343=CARTESIAN_POINT('Ctrl Pts',(-19.936331946696,-20.6944370556124,
2.9898588606151));
#160344=CARTESIAN_POINT('Ctrl Pts',(-19.9362426927778,-20.6944986400934,
2.98985239140081));
#160345=CARTESIAN_POINT('Ctrl Pts',(-19.9361971245473,-20.6945300791651,
2.98984908859063));
#160346=CARTESIAN_POINT('Ctrl Pts',(-19.9361039725555,-20.6945943424986,
2.98984233692691));
#160347=CARTESIAN_POINT('Ctrl Pts',(-19.9360563888562,-20.6946271664792,
2.9898388880798));
#160348=CARTESIAN_POINT('Ctrl Pts',(-19.9359590602922,-20.6946942993632,
2.98983183379254));
#160349=CARTESIAN_POINT('Ctrl Pts',(-19.9359093151244,-20.6947286082087,
2.98982822833257));
#160350=CARTESIAN_POINT('Ctrl Pts',(-19.9358075019095,-20.694798821538,
2.98982084910535));
#160351=CARTESIAN_POINT('Ctrl Pts',(-19.9357554337759,-20.6948347257816,
2.98981707533423));
#160352=CARTESIAN_POINT('Ctrl Pts',(-19.9356487962604,-20.6949082519855,
2.98980934656431));
#160353=CARTESIAN_POINT('Ctrl Pts',(-19.9355942266161,-20.6949458737884,
2.9898053915492));
#160354=CARTESIAN_POINT('Ctrl Pts',(-19.9354823876159,-20.6950229709005,
2.98979728591565));
#160355=CARTESIAN_POINT('Ctrl Pts',(-19.9354251180778,-20.6950624459525,
2.98979313528709));
#160356=CARTESIAN_POINT('Ctrl Pts',(-19.9353076583195,-20.6951434007007,
2.98978462242109));
#160357=CARTESIAN_POINT('Ctrl Pts',(-19.9352474679084,-20.6951848800936,
2.98978026017332));
#160358=CARTESIAN_POINT('Ctrl Pts',(-19.9351239193287,-20.6952700124583,
2.98977130617299));
#160359=CARTESIAN_POINT('Ctrl Pts',(-19.9350605609644,-20.6953136650688,
2.98976671441022));
#160360=CARTESIAN_POINT('Ctrl Pts',(-19.9349303993287,-20.6954033332962,
2.98975728130622));
#160361=CARTESIAN_POINT('Ctrl Pts',(-19.9348635957845,-20.6954493485329,
2.98975243994976));
#160362=CARTESIAN_POINT('Ctrl Pts',(-19.9347262313793,-20.695543955459,
2.98974248503145));
#160363=CARTESIAN_POINT('Ctrl Pts',(-19.9346556702405,-20.6955925466861,
2.98973737145472));
#160364=CARTESIAN_POINT('Ctrl Pts',(-19.9345104371643,-20.6956925470043,
2.98972684649496));
#160365=CARTESIAN_POINT('Ctrl Pts',(-19.9344357648919,-20.6957439555701,
2.98972143509373));
#160366=CARTESIAN_POINT('Ctrl Pts',(-19.9342819076382,-20.6958498649359,
2.98971028537758));
#160367=CARTESIAN_POINT('Ctrl Pts',(-19.9342027222522,-20.6959043651356,
2.98970454704035));
#160368=CARTESIAN_POINT('Ctrl Pts',(-19.9340393794748,-20.6960167711766,
2.98969271018984));
#160369=CARTESIAN_POINT('Ctrl Pts',(-19.9339552215973,-20.6960746763246,
2.98968661164954));
#160370=CARTESIAN_POINT('Ctrl Pts',(-19.9337814059067,-20.6961942523361,
2.98967401616129));
#160371=CARTESIAN_POINT('Ctrl Pts',(-19.933691747565,-20.6962559223538,
2.98966751918468));
#160372=CARTESIAN_POINT('Ctrl Pts',(-19.9335063207716,-20.6963834440676,
2.98965408263791));
#160373=CARTESIAN_POINT('Ctrl Pts',(-19.9334105516113,-20.6964492948181,
2.98964714302782));
#160374=CARTESIAN_POINT('Ctrl Pts',(-19.9281812407947,-20.70004432796,2.98926822255984));
#160375=CARTESIAN_POINT('Ctrl Pts',(-19.9230321947558,-20.7035508119744,
2.98889538341952));
#160376=CARTESIAN_POINT('Ctrl Pts',(-19.9113144432798,-20.7114550831538,
2.98804746985103));
#160377=CARTESIAN_POINT('Ctrl Pts',(-19.9047364596769,-20.715838889278,
2.98757187442385));
#160378=CARTESIAN_POINT('Ctrl Pts',(-19.8858604891918,-20.7282664084734,
2.98620816343938));
#160379=CARTESIAN_POINT('Ctrl Pts',(-19.8735032785493,-20.7362189331811,
2.98531665819358));
#160380=CARTESIAN_POINT('Ctrl Pts',(-19.789592024767,-20.7889930289318,
2.97927023993084));
#160381=CARTESIAN_POINT('Ctrl Pts',(-19.7155032841278,-20.8296224716274,
2.97396256013928));
#160382=CARTESIAN_POINT('Ctrl Pts',(-19.5076321377924,-20.9279462165594,
2.95916188623186));
#160383=CARTESIAN_POINT('Ctrl Pts',(-19.3700083212911,-20.9764399912341,
2.94943500180701));
#160384=CARTESIAN_POINT('Ctrl Pts',(-19.1746042461389,-21.0233839295406,
2.93627202266629));
#160385=CARTESIAN_POINT('Ctrl Pts',(-19.1201982756254,-21.0342140189079,
2.93267809635083));
#160386=CARTESIAN_POINT('Ctrl Pts',(-19.0372416454391,-21.0473634162181,
2.92736165187186));
#160387=CARTESIAN_POINT('Ctrl Pts',(-19.0089677533935,-21.0512608847093,
2.92557816504653));
#160388=CARTESIAN_POINT('Ctrl Pts',(-18.9737216628097,-21.0553950642261,
2.92339730987514));
#160389=CARTESIAN_POINT('Ctrl Pts',(-18.9668171222875,-21.0561704927339,
2.92297210937185));
#160390=CARTESIAN_POINT('Ctrl Pts',(-18.9558866591985,-21.0573436000484,
2.92230230791951));
#160391=CARTESIAN_POINT('Ctrl Pts',(-18.9518632705746,-21.057763747376,
2.92205647330538));
#160392=CARTESIAN_POINT('Ctrl Pts',(-18.9442738178413,-21.0585343008492,
2.92159412182861));
#160393=CARTESIAN_POINT('Ctrl Pts',(-18.9407081124935,-21.0588871814911,
2.92137747381635));
#160394=CARTESIAN_POINT('Ctrl Pts',(-18.9325549793725,-21.0596731604716,
2.92088339372251));
#160395=CARTESIAN_POINT('Ctrl Pts',(-18.9279670277192,-21.0601003354403,
2.9206062970677));
#160396=CARTESIAN_POINT('Ctrl Pts',(-18.9157855622333,-21.0611944230948,
2.91987296836841));
#160397=CARTESIAN_POINT('Ctrl Pts',(-18.90818969931,-21.0618353152941,2.91941815837844));
#160398=CARTESIAN_POINT('Ctrl Pts',(-18.855046716413,-21.0660302375047,
2.91625236056243));
#160399=CARTESIAN_POINT('Ctrl Pts',(-18.809394859947,-21.0681503812393,
2.91361588352324));
#160400=CARTESIAN_POINT('Ctrl Pts',(-18.758205340195,-21.0688687659378,
2.91071732448469));
#160401=CARTESIAN_POINT('Ctrl Pts',(-18.7527036805514,-21.0689245248502,
2.91040654571446));
#160402=CARTESIAN_POINT('Ctrl Pts',(-18.7328742176782,-21.0690481857932,
2.90928891640793));
#160403=CARTESIAN_POINT('Ctrl Pts',(-18.7185458293019,-21.0689920809123,
2.90848604356407));
#160404=CARTESIAN_POINT('Ctrl Pts',(-18.6499567126346,-21.0680271008931,
2.90466078417337));
#160405=CARTESIAN_POINT('Ctrl Pts',(-18.5957418468549,-21.0651774867336,
2.90169086503889));
#160406=CARTESIAN_POINT('Ctrl Pts',(-18.4326910601129,-21.050304686801,
2.89277628524882));
#160407=CARTESIAN_POINT('Ctrl Pts',(-18.3246238016806,-21.0319230497364,
2.88688299139122));
#160408=CARTESIAN_POINT('Ctrl Pts',(-18.1648912508766,-20.9918175175315,
2.87772655565901));
#160409=CARTESIAN_POINT('Ctrl Pts',(-18.111866117343,-20.9762749457541,
2.87461210258433));
#160410=CARTESIAN_POINT('Ctrl Pts',(-18.0269372247122,-20.9477284956435,
2.86945763405028));
#160411=CARTESIAN_POINT('Ctrl Pts',(-17.9946353910591,-20.9359883502697,
2.86745721660099));
#160412=CARTESIAN_POINT('Ctrl Pts',(-17.9525628311587,-20.9195268556518,
2.864792789918));
#160413=CARTESIAN_POINT('Ctrl Pts',(-17.9425212660013,-20.9155089466603,
2.86415239441776));
#160414=CARTESIAN_POINT('Ctrl Pts',(-17.9261250296635,-20.9088021456633,
2.86309921054839));
#160415=CARTESIAN_POINT('Ctrl Pts',(-17.919751858174,-20.9061587875014,
2.86268796620739));
#160416=CARTESIAN_POINT('Ctrl Pts',(-17.9074403114557,-20.9009817249937,
2.86188984895989));
#160417=CARTESIAN_POINT('Ctrl Pts',(-17.9015003743258,-20.8984519143574,
2.86150311204705));
#160418=CARTESIAN_POINT('Ctrl Pts',(-17.8878120602564,-20.8925479618631,
2.86060798755312));
#160419=CARTESIAN_POINT('Ctrl Pts',(-17.8800721689093,-20.8891545311906,
2.86009894501476));
#160420=CARTESIAN_POINT('Ctrl Pts',(-17.8593114331308,-20.8799037217195,
2.85872560629793));
#160421=CARTESIAN_POINT('Ctrl Pts',(-17.8463293564329,-20.8739608898477,
2.85785838847722));
#160422=CARTESIAN_POINT('Ctrl Pts',(-17.7276347855214,-20.8181667386345,
2.8498502563495));
#160423=CARTESIAN_POINT('Ctrl Pts',(-17.6261774567779,-20.7597805843482,
2.8424073947021));
#160424=CARTESIAN_POINT('Ctrl Pts',(-17.3962082638498,-20.6007831880577,
2.82414522202982));
#160425=CARTESIAN_POINT('Ctrl Pts',(-17.2734695744201,-20.4931111841494,
2.81318589815666));
#160426=CARTESIAN_POINT('Ctrl Pts',(-17.1424765075164,-20.3483515449723,
2.80078078528216));
#160427=CARTESIAN_POINT('Ctrl Pts',(-17.1212321258497,-20.3237597153163,
2.79874441831563));
#160428=CARTESIAN_POINT('Ctrl Pts',(-17.0959564053863,-20.2931020011724,
2.79630109629527));
#160429=CARTESIAN_POINT('Ctrl Pts',(-17.0913803979649,-20.2874932579013,
2.79585789420545));
#160430=CARTESIAN_POINT('Ctrl Pts',(-17.0842517107691,-20.2786636610299,
2.79516625871425));
#160431=CARTESIAN_POINT('Ctrl Pts',(-17.0816795386985,-20.2754587190938,
2.79491645514562));
#160432=CARTESIAN_POINT('Ctrl Pts',(-17.076889096457,-20.2694540644666,
2.79445078641943));
#160433=CARTESIAN_POINT('Ctrl Pts',(-17.0746686041025,-20.2666562582818,
2.79423476589695));
#160434=CARTESIAN_POINT('Ctrl Pts',(-17.0696159747261,-20.2602567823454,
2.79374281215191));
#160435=CARTESIAN_POINT('Ctrl Pts',(-17.0667884477318,-20.2566515370123,
2.79346720823515));
#160436=CARTESIAN_POINT('Ctrl Pts',(-17.0581333679608,-20.24554176912,2.79262256074521));
#160437=CARTESIAN_POINT('Ctrl Pts',(-17.0523445221673,-20.2380070522076,
2.79205619267762));
#160438=CARTESIAN_POINT('Ctrl Pts',(-16.9739711988061,-20.1345627648873,
2.78436463603442));
#160439=CARTESIAN_POINT('Ctrl Pts',(-16.9096273046158,-20.0326612716488,
2.77776313640976));
#160440=CARTESIAN_POINT('Ctrl Pts',(-16.8042695649171,-19.8292968686495,
2.76529791680799));
#160441=CARTESIAN_POINT('Ctrl Pts',(-16.761768618844,-19.7290532622158,
2.75944056089084));
#160442=CARTESIAN_POINT('Ctrl Pts',(-16.7033687207892,-19.5551650524411,
2.74923475883848));
#160443=CARTESIAN_POINT('Ctrl Pts',(-16.683349675745,-19.4831337259984,
2.74499700951102));
#160444=CARTESIAN_POINT('Ctrl Pts',(-16.6631195411512,-19.391880895208,
2.73953920721983));
#160445=CARTESIAN_POINT('Ctrl Pts',(-16.6593021870224,-19.3735092265777,
2.73843612347462));
#160446=CARTESIAN_POINT('Ctrl Pts',(-16.6541023703782,-19.3466997454833,
2.73681926668054));
#160447=CARTESIAN_POINT('Ctrl Pts',(-16.6525259462666,-19.3383001412871,
2.73631167989067));
#160448=CARTESIAN_POINT('Ctrl Pts',(-16.6498494461607,-19.3235468291119,
2.7354182730538));
#160449=CARTESIAN_POINT('Ctrl Pts',(-16.6487274516848,-19.3171971729287,
2.73503315619491));
#160450=CARTESIAN_POINT('Ctrl Pts',(-16.6466038831833,-19.3048504204276,
2.73428309333823));
#160451=CARTESIAN_POINT('Ctrl Pts',(-16.6455991010574,-19.298853934378,
2.7339182535416));
#160452=CARTESIAN_POINT('Ctrl Pts',(-16.6432569502697,-19.284496897767,
2.73304337763043));
#160453=CARTESIAN_POINT('Ctrl Pts',(-16.641943886623,-19.2761325380828,
2.73253257514694));
#160454=CARTESIAN_POINT('Ctrl Pts',(-16.6373761642577,-19.2458510553143,
2.73067920422813));
#160455=CARTESIAN_POINT('Ctrl Pts',(-16.6344155582316,-19.2238916413541,
2.72932738285842));
#160456=CARTESIAN_POINT('Ctrl Pts',(-16.6099457114204,-19.0180394042224,
2.71657811543212));
#160457=CARTESIAN_POINT('Ctrl Pts',(-16.6123082225007,-18.8321483608013,
2.70438576278502));
#160458=CARTESIAN_POINT('Ctrl Pts',(-16.6503130376275,-18.5693655715215,
2.68685503401444));
#160459=CARTESIAN_POINT('Ctrl Pts',(-16.6663572077965,-18.4904640064932,
2.68156879537342));
#160460=CARTESIAN_POINT('Ctrl Pts',(-16.6960541679284,-18.3777442055429,
2.67413761749523));
#160461=CARTESIAN_POINT('Ctrl Pts',(-16.7061462954959,-18.3430643338559,
2.6718688044231));
#160462=CARTESIAN_POINT('Ctrl Pts',(-16.7193918330655,-18.3015395850717,
2.66918726181472));
#160463=CARTESIAN_POINT('Ctrl Pts',(-16.7216999612358,-18.2944337482181,
2.66872964477093));
#160464=CARTESIAN_POINT('Ctrl Pts',(-16.7253518975084,-18.2833901668765,
2.66802055976474));
#160465=CARTESIAN_POINT('Ctrl Pts',(-16.7266697508931,-18.2794439946736,
2.66776760805705));
#160466=CARTESIAN_POINT('Ctrl Pts',(-16.7291386924514,-18.2721229140524,
2.66729914455568));
#160467=CARTESIAN_POINT('Ctrl Pts',(-16.7302866632742,-18.2687470607406,
2.66708345859834));
#160468=CARTESIAN_POINT('Ctrl Pts',(-16.7329056093276,-18.2611088579796,
2.66659618029708));
#160469=CARTESIAN_POINT('Ctrl Pts',(-16.7343816719604,-18.2568483089747,
2.66632489275421));
#160470=CARTESIAN_POINT('Ctrl Pts',(-16.7388891765665,-18.243970875412,
2.6655063948906));
#160471=CARTESIAN_POINT('Ctrl Pts',(-16.7419628328504,-18.2353687346147,
2.66496162505084));
#160472=CARTESIAN_POINT('Ctrl Pts',(-16.7662514808348,-18.1687567801591,
2.66075661548381));
#160473=CARTESIAN_POINT('Ctrl Pts',(-16.7899425478092,-18.111674877791,
2.65723262273757));
#160474=CARTESIAN_POINT('Ctrl Pts',(-16.8367902575373,-18.0114295815509,
2.65105075814918));
#160475=CARTESIAN_POINT('Ctrl Pts',(-16.859009674805,-17.9678815348047,
2.64836766705726));
#160476=CARTESIAN_POINT('Ctrl Pts',(-16.8870843797334,-17.9172668203226,
2.64521014660781));
#160477=CARTESIAN_POINT('Ctrl Pts',(-16.8915017216318,-17.9094213906173,
2.64471959100856));
#160478=CARTESIAN_POINT('Ctrl Pts',(-16.9501145785086,-17.8068578955759,
2.63828892504994));
#160479=CARTESIAN_POINT('Ctrl Pts',(-17.0115045676925,-17.7164409311076,
2.63241175022768));
#160480=CARTESIAN_POINT('Ctrl Pts',(-17.1265997777106,-17.5722786641264,
2.62215224693034));
#160481=CARTESIAN_POINT('Ctrl Pts',(-17.1767171591789,-17.515951647562,
2.61788011849854));
#160482=CARTESIAN_POINT('Ctrl Pts',(-17.2429895847003,-17.4490255357458,
2.61238088307276));
#160483=CARTESIAN_POINT('Ctrl Pts',(-17.2564304908981,-17.4358098369583,
2.61127283436402));
#160484=CARTESIAN_POINT('Ctrl Pts',(-17.2762305823069,-17.4168548494912,
2.60965002467063));
#160485=CARTESIAN_POINT('Ctrl Pts',(-17.2824511916493,-17.4109716543871,
2.60914151530343));
#160486=CARTESIAN_POINT('Ctrl Pts',(-17.2934205574522,-17.4007226301013,
2.60824704262147));
#160487=CARTESIAN_POINT('Ctrl Pts',(-17.2981539270113,-17.3963404415128,
2.60786178778093));
#160488=CARTESIAN_POINT('Ctrl Pts',(-17.3073842221779,-17.3878729803363,
2.6071118711392));
#160489=CARTESIAN_POINT('Ctrl Pts',(-17.3118788560945,-17.3837852946636,
2.60674731748892));
#160490=CARTESIAN_POINT('Ctrl Pts',(-17.3226661612164,-17.3740591948397,
2.60587379902979));
#160491=CARTESIAN_POINT('Ctrl Pts',(-17.328975077989,-17.368439027263,2.60536407319583));
#160492=CARTESIAN_POINT('Ctrl Pts',(-17.3518656256528,-17.3482919369598,
2.6035186372327));
#160493=CARTESIAN_POINT('Ctrl Pts',(-17.3686398296293,-17.3339868579936,
2.60217377705548));
#160494=CARTESIAN_POINT('Ctrl Pts',(-17.5292275944535,-17.2013128164937,
2.58936426040597));
#160495=CARTESIAN_POINT('Ctrl Pts',(-17.6878248408545,-17.1021697917924,
2.57709367830812));
#160496=CARTESIAN_POINT('Ctrl Pts',(-17.9298504657469,-16.9920544581515,
2.55953971340276));
#160497=CARTESIAN_POINT('Ctrl Pts',(-18.0042174964672,-16.9631656175317,
2.55430347000594));
#160498=CARTESIAN_POINT('Ctrl Pts',(-18.1141968763846,-16.9274450428546,
2.54693294721454));
#160499=CARTESIAN_POINT('Ctrl Pts',(-18.1486318589578,-16.9172215892222,
2.54467686267104));
#160500=CARTESIAN_POINT('Ctrl Pts',(-18.1905148927086,-16.9059382763945,
2.54200829632643));
#160501=CARTESIAN_POINT('Ctrl Pts',(-18.1977275695632,-16.9040360054894,
2.54155142231712));
#160502=CARTESIAN_POINT('Ctrl Pts',(-18.2089760932919,-16.9011328214072,
2.54084323595441));
#160503=CARTESIAN_POINT('Ctrl Pts',(-18.2130050065336,-16.9001056303226,
2.54059044580314));
#160504=CARTESIAN_POINT('Ctrl Pts',(-18.2204950067648,-16.8982195009416,
2.54012212885059));
#160505=CARTESIAN_POINT('Ctrl Pts',(-18.223955204804,-16.8973574462796,
2.53990642884282));
#160506=CARTESIAN_POINT('Ctrl Pts',(-18.2317990320718,-16.8954243144646,
2.5394189248014));
#160507=CARTESIAN_POINT('Ctrl Pts',(-18.2361839063009,-16.8943585102735,
2.53914742676615));
#160508=CARTESIAN_POINT('Ctrl Pts',(-18.2475178980138,-16.8916419780715,
2.53844823370985));
#160509=CARTESIAN_POINT('Ctrl Pts',(-18.2544720864198,-16.8900123672903,
2.53802172425676));
#160510=CARTESIAN_POINT('Ctrl Pts',(-18.2973029754371,-16.8802039855284,
2.53540942859809));
#160511=CARTESIAN_POINT('Ctrl Pts',(-18.3333819803645,-16.8729260266833,
2.53327173696836));
#160512=CARTESIAN_POINT('Ctrl Pts',(-18.5372414799472,-16.8373074260169,
2.5214516820225));
#160513=CARTESIAN_POINT('Ctrl Pts',(-18.7077820129277,-16.8283326084829,
2.5124979413225));
#160514=CARTESIAN_POINT('Ctrl Pts',(-18.972930236559,-16.8463559883984,
2.49788030651757));
#160515=CARTESIAN_POINT('Ctrl Pts',(-19.0677304202319,-16.8592875780321,
2.4925218126008));
#160516=CARTESIAN_POINT('Ctrl Pts',(-19.1822990539436,-16.8828998331049,
2.48571043485678));
#160517=CARTESIAN_POINT('Ctrl Pts',(-19.2032044840941,-16.8875401081621,
2.48445396354954));
#160518=CARTESIAN_POINT('Ctrl Pts',(-19.2328041060998,-16.8945830010857,
2.48265418015873));
#160519=CARTESIAN_POINT('Ctrl Pts',(-19.2415593115042,-16.8967253747583,
2.48211922995132));
#160520=CARTESIAN_POINT('Ctrl Pts',(-19.2566304773285,-16.9005154187311,
2.48119378142771));
#160521=CARTESIAN_POINT('Ctrl Pts',(-19.262953036607,-16.9021365200069,
2.48080414563087));
#160522=CARTESIAN_POINT('Ctrl Pts',(-19.2750382247347,-16.9052947917458,
2.4800566633041));
#160523=CARTESIAN_POINT('Ctrl Pts',(-19.2808020609307,-16.9068271282971,
2.47969897674571));
#160524=CARTESIAN_POINT('Ctrl Pts',(-19.295759695732,-16.9108714200591,
2.47876762629992));
#160525=CARTESIAN_POINT('Ctrl Pts',(-19.3049430676765,-16.9134211213627,
2.47819274066827));
#160526=CARTESIAN_POINT('Ctrl Pts',(-19.336129882992,-16.9223071903796,
2.47622976998112));
#160527=CARTESIAN_POINT('Ctrl Pts',(-19.3580470117735,-16.9289383202925,
2.47483212517879));
#160528=CARTESIAN_POINT('Ctrl Pts',(-19.5481992773025,-16.989853739395,
2.46254314141727));
#160529=CARTESIAN_POINT('Ctrl Pts',(-19.709098980589,-17.0646482972645,
2.4509363949218));
#160530=CARTESIAN_POINT('Ctrl Pts',(-19.9317544890571,-17.2042903791135,
2.43357259671966));
#160531=CARTESIAN_POINT('Ctrl Pts',(-20.001853531418,-17.2544564655524,
2.4278993392237));
#160532=CARTESIAN_POINT('Ctrl Pts',(-20.0978870801496,-17.3324585809217,
2.42000187112837));
#160533=CARTESIAN_POINT('Ctrl Pts',(-20.1264343243009,-17.3569359162561,
2.41763741074223));
#160534=CARTESIAN_POINT('Ctrl Pts',(-20.1599214149946,-17.3872334833199,
2.41485859842912));
#160535=CARTESIAN_POINT('Ctrl Pts',(-20.165499358589,-17.3923347398302,
2.41439555569302));
#160536=CARTESIAN_POINT('Ctrl Pts',(-20.1741189386858,-17.400302893632,
2.41367991162881));
#160537=CARTESIAN_POINT('Ctrl Pts',(-20.1771795439561,-17.4031490478177,
2.41342578281701));
#160538=CARTESIAN_POINT('Ctrl Pts',(-20.1828344133771,-17.4084390052608,
2.41295624221562));
#160539=CARTESIAN_POINT('Ctrl Pts',(-20.1854309123638,-17.410880274347,
2.41274064931245));
#160540=CARTESIAN_POINT('Ctrl Pts',(-20.1912800749276,-17.4164076432322,
2.41225497327949));
#160541=CARTESIAN_POINT('Ctrl Pts',(-20.194529097568,-17.4194975174728,
2.41198518640582));
#160542=CARTESIAN_POINT('Ctrl Pts',(-20.2040695561237,-17.4286285493413,
2.41119286584023));
#160543=CARTESIAN_POINT('Ctrl Pts',(-20.210333590182,-17.4346983777288,
2.41067249781152));
#160544=CARTESIAN_POINT('Ctrl Pts',(-20.254664251811,-17.4781890914558,
2.40698720276468));
#160545=CARTESIAN_POINT('Ctrl Pts',(-20.2913444518108,-17.5170025642334,
2.40392378474618));
#160546=CARTESIAN_POINT('Ctrl Pts',(-20.3355342809387,-17.5674552793871,
2.40015208423915));
#160547=CARTESIAN_POINT('Ctrl Pts',(-20.3444477103439,-17.5778332269467,
2.39938689371169));
#160548=CARTESIAN_POINT('Ctrl Pts',(-20.3868894745888,-17.6282285501123,
2.39571801256821));
#160549=CARTESIAN_POINT('Ctrl Pts',(-20.4190315225978,-17.6693918689559,
2.3928615095606));
#160550=CARTESIAN_POINT('Ctrl Pts',(-20.5137302381864,-17.8003822313344,
2.38406095003522));
#160551=CARTESIAN_POINT('Ctrl Pts',(-20.5708677379246,-17.8938982825623,
2.37816909391497));
#160552=CARTESIAN_POINT('Ctrl Pts',(-20.6549212452758,-18.0589719937411,
2.36786978230487));
#160553=CARTESIAN_POINT('Ctrl Pts',(-20.6856664674143,-18.1283291310996,
2.36357214980944));
#160554=CARTESIAN_POINT('Ctrl Pts',(-20.7160027874429,-18.2080616742,2.35859161515212));
#160555=CARTESIAN_POINT('Ctrl Pts',(-20.7193217417052,-18.2169647250411,
2.35803497993091));
#160556=CARTESIAN_POINT('Ctrl Pts',(-20.7225805738064,-18.2258896079247,
2.35747639166834));
#160557=CARTESIAN_POINT('',(-20.849962012661,-18.9501158126703,2.8890562790225));
#160558=CARTESIAN_POINT('Ctrl Pts',(-20.849962012661,-18.9501158126703,
2.8890562790225));
#160559=CARTESIAN_POINT('Ctrl Pts',(-20.8456331599479,-19.4559949671801,
2.85866010167885));
#160560=CARTESIAN_POINT('Ctrl Pts',(-20.410193517051,-20.6740880447519,
2.78587198877475));
#160561=CARTESIAN_POINT('Ctrl Pts',(-18.3741968385222,-21.4292710094645,
2.67069194031011));
#160562=CARTESIAN_POINT('Ctrl Pts',(-16.4562524857842,-19.9903623098931,
2.54351613362868));
#160563=CARTESIAN_POINT('Ctrl Pts',(-16.6280001024638,-17.5988205946497,
2.41634032694725));
#160564=CARTESIAN_POINT('Ctrl Pts',(-18.7318719157381,-16.448737081536,
2.28916452026583));
#160565=CARTESIAN_POINT('Ctrl Pts',(-20.2929104264445,-17.2986361211697,
2.19488963603122));
#160566=CARTESIAN_POINT('Ctrl Pts',(-20.670180409037,-18.0771167134768,
2.1430066873571));
#160567=CARTESIAN_POINT('Ctrl Pts',(-20.7227693997001,-18.2258206865925,
2.13351567424346));
#160568=CARTESIAN_POINT('Ctrl Pts',(-20.8509991255275,-18.9500758077574,
2.88845974797779));
#160569=CARTESIAN_POINT('Ctrl Pts',(-20.850857410614,-18.7941608522463,
2.89867443023815));
#160570=CARTESIAN_POINT('Ctrl Pts',(-20.8334923215512,-18.6387336577071,
2.90915374483203));
#160571=CARTESIAN_POINT('Ctrl Pts',(-20.7924732127667,-18.456705003608,
2.92098938639697));
#160572=CARTESIAN_POINT('Ctrl Pts',(-20.7850834951854,-18.4269420749175,
2.9229085845561));
#160573=CARTESIAN_POINT('Ctrl Pts',(-20.7751867696799,-18.3904876570822,
2.92523075559935));
#160574=CARTESIAN_POINT('Ctrl Pts',(-20.7732896035714,-18.3836361587522,
2.92566594769897));
#160575=CARTESIAN_POINT('Ctrl Pts',(-20.7702491090473,-18.3728668375536,
2.92634787332317));
#160576=CARTESIAN_POINT('Ctrl Pts',(-20.7691289247223,-18.3689426148742,
2.92659591554719));
#160577=CARTESIAN_POINT('Ctrl Pts',(-20.7670057657387,-18.3615854447296,
2.92706008118862));
#160578=CARTESIAN_POINT('Ctrl Pts',(-20.7660054511583,-18.3581518398861,
2.92727634930289));
#160579=CARTESIAN_POINT('Ctrl Pts',(-20.7636912486175,-18.3502825948929,
2.92777119465781));
#160580=CARTESIAN_POINT('Ctrl Pts',(-20.7623715216973,-18.3458487224942,
2.92804942769785));
#160581=CARTESIAN_POINT('Ctrl Pts',(-20.7588689785161,-18.3342208018338,
2.92877765083969));
#160582=CARTESIAN_POINT('Ctrl Pts',(-20.7566623348027,-18.3270339201095,
2.92922628571805));
#160583=CARTESIAN_POINT('Ctrl Pts',(-20.7445408458542,-18.288291834689,
2.93163759997949));
#160584=CARTESIAN_POINT('Ctrl Pts',(-20.733925666785,-18.2569601334749,
2.93356211485035));
#160585=CARTESIAN_POINT('Ctrl Pts',(-20.7225805736403,-18.2258896074698,
2.9354567758078));
#160586=CARTESIAN_POINT('Origin',(-18.734,-18.952,0.));
#160587=CARTESIAN_POINT('',(-20.722580643286,-18.2258897982069,3.95421663535642));
#160588=CARTESIAN_POINT('',(-20.7225805737618,-18.2258896078024,3.73234499902338));
#160589=CARTESIAN_POINT('',(-20.7225805737622,-18.2258896078036,0.));
#160590=CARTESIAN_POINT('Ctrl Pts',(-20.722580643286,-18.2258897982069,
3.95421663535643));
#160591=CARTESIAN_POINT('Ctrl Pts',(-20.7432514728671,-18.2825005047965,
3.95029637644732));
#160592=CARTESIAN_POINT('Ctrl Pts',(-20.7615069693432,-18.339999464268,
3.94643464604714));
#160593=CARTESIAN_POINT('Ctrl Pts',(-20.7804090246118,-18.4097441966995,
3.94195346478622));
#160594=CARTESIAN_POINT('Ctrl Pts',(-20.7834316360229,-18.4212823382214,
3.9412186908867));
#160595=CARTESIAN_POINT('Ctrl Pts',(-20.7875891299676,-18.4377180308393,
3.94018194661357));
#160596=CARTESIAN_POINT('Ctrl Pts',(-20.7888042694118,-18.4425947839614,
3.93987556277719));
#160597=CARTESIAN_POINT('Ctrl Pts',(-20.7908681043649,-18.4510051823497,
3.93934935986463));
#160598=CARTESIAN_POINT('Ctrl Pts',(-20.7917250853805,-18.4545367552864,
3.93912906692465));
#160599=CARTESIAN_POINT('Ctrl Pts',(-20.793368805131,-18.4613873637551,
3.93870304221645));
#160600=CARTESIAN_POINT('Ctrl Pts',(-20.7941566162606,-18.4647060935657,
3.93849724659215));
#160601=CARTESIAN_POINT('Ctrl Pts',(-20.7962599600511,-18.4736629061791,
3.93794338394597));
#160602=CARTESIAN_POINT('Ctrl Pts',(-20.7975604024717,-18.4793045533346,
3.93759617847265));
#160603=CARTESIAN_POINT('Ctrl Pts',(-20.8022980768258,-18.5002499786051,
3.93631303011186));
#160604=CARTESIAN_POINT('Ctrl Pts',(-20.8055884395398,-18.5155869088825,
3.93538513345564));
#160605=CARTESIAN_POINT('Ctrl Pts',(-20.8354454606658,-18.6627095824125,
3.92658321823459));
#160606=CARTESIAN_POINT('Ctrl Pts',(-20.8495760231323,-18.7967260298796,
3.91931208592608));
#160607=CARTESIAN_POINT('Ctrl Pts',(-20.8509595378659,-18.9374794217699,
3.91166815891939));
#160608=CARTESIAN_POINT('Ctrl Pts',(-20.8509933270794,-18.9437668212733,
3.91132672589034));
#160609=CARTESIAN_POINT('Ctrl Pts',(-20.8511331452923,-19.0958927699035,
3.90306449741813));
#160610=CARTESIAN_POINT('Ctrl Pts',(-20.8361978944804,-19.2413359766959,
3.8951037815209));
#160611=CARTESIAN_POINT('Ctrl Pts',(-20.8015323044882,-19.4076057123349,
3.88524452288232));
#160612=CARTESIAN_POINT('Ctrl Pts',(-20.7962279547766,-19.4310429922329,
3.88383774041166));
#160613=CARTESIAN_POINT('Ctrl Pts',(-20.7882195556456,-19.4638256313104,
3.88184401110845));
#160614=CARTESIAN_POINT('Ctrl Pts',(-20.7858481757337,-19.4732509171373,
3.88126775903198));
#160615=CARTESIAN_POINT('Ctrl Pts',(-20.7819083814074,-19.4884664423229,
3.88033245111997));
#160616=CARTESIAN_POINT('Ctrl Pts',(-20.7803800925229,-19.4942669989618,
3.87997469653568));
#160617=CARTESIAN_POINT('Ctrl Pts',(-20.7771446747113,-19.5063384126534,
3.87922766363171));
#160618=CARTESIAN_POINT('Ctrl Pts',(-20.7754332825869,-19.5126080527688,
3.87883825025342));
#160619=CARTESIAN_POINT('Ctrl Pts',(-20.7713216387836,-19.5274024436891,
3.87791595248192));
#160620=CARTESIAN_POINT('Ctrl Pts',(-20.7688967234845,-19.5359201598563,
3.8773822701327));
#160621=CARTESIAN_POINT('Ctrl Pts',(-20.7606830657947,-19.564098689347,
3.87560769559069));
#160622=CARTESIAN_POINT('Ctrl Pts',(-20.7546623993838,-19.5836901740856,
3.87435926264209));
#160623=CARTESIAN_POINT('Ctrl Pts',(-20.7212770166753,-19.6869627376828,
3.86769856750041));
#160624=CARTESIAN_POINT('Ctrl Pts',(-20.6889997166902,-19.7689534180585,
3.86212565012843));
#160625=CARTESIAN_POINT('Ctrl Pts',(-20.596895197613,-19.9659340688863,
3.84804789280976));
#160626=CARTESIAN_POINT('Ctrl Pts',(-20.531438235175,-20.0779009529177,
3.83941397487547));
#160627=CARTESIAN_POINT('Ctrl Pts',(-20.4404280187582,-20.2052061074316,
3.82914932405589));
#160628=CARTESIAN_POINT('Ctrl Pts',(-20.4242597092025,-20.2269291436962,
3.82738151409786));
#160629=CARTESIAN_POINT('Ctrl Pts',(-20.3725012453261,-20.2937536422861,
3.82190467509247));
#160630=CARTESIAN_POINT('Ctrl Pts',(-20.3354861302741,-20.3377245765649,
3.81824387044658));
#160631=CARTESIAN_POINT('Ctrl Pts',(-20.2907366205742,-20.3866912153627,
3.81415065877349));
#160632=CARTESIAN_POINT('Ctrl Pts',(-20.2847073304121,-20.393205943303,
3.81360573899493));
#160633=CARTESIAN_POINT('Ctrl Pts',(-20.2755484457244,-20.4029782182891,
3.81278809120708));
#160634=CARTESIAN_POINT('Ctrl Pts',(-20.2724491963512,-20.4062638933788,
3.81251313465858));
#160635=CARTESIAN_POINT('Ctrl Pts',(-20.2668840549586,-20.4121260878752,
3.81202252978854));
#160636=CARTESIAN_POINT('Ctrl Pts',(-20.2644221547996,-20.41470630926,3.81180658179284));
#160637=CARTESIAN_POINT('Ctrl Pts',(-20.2590780366655,-20.4202790073261,
3.81134016612265));
#160638=CARTESIAN_POINT('Ctrl Pts',(-20.2561935353685,-20.4232692149426,
3.81108988037117));
#160639=CARTESIAN_POINT('Ctrl Pts',(-20.2481155994519,-20.4315939916044,
3.81039297116676));
#160640=CARTESIAN_POINT('Ctrl Pts',(-20.2429027405549,-20.4369097453308,
3.80994783512988));
#160641=CARTESIAN_POINT('Ctrl Pts',(-20.2125450870429,-20.4675416790893,
3.80738120982499));
#160642=CARTESIAN_POINT('Ctrl Pts',(-20.1867898930599,-20.4922480389433,
3.80530493917686));
#160643=CARTESIAN_POINT('Ctrl Pts',(-20.102148917991,-20.5694290007856,
3.79875037057054));
#160644=CARTESIAN_POINT('Ctrl Pts',(-20.0409487441668,-20.6192717091496,
3.79440913065695));
#160645=CARTESIAN_POINT('Ctrl Pts',(-19.9033750794258,-20.7190732835977,
3.78513986639871));
#160646=CARTESIAN_POINT('Ctrl Pts',(-19.8262702742676,-20.7677454640115,
3.78023284397057));
#160647=CARTESIAN_POINT('Ctrl Pts',(-19.652946817895,-20.8621090647309,
3.76938681059503));
#160648=CARTESIAN_POINT('Ctrl Pts',(-19.5559418736567,-20.9058135002402,
3.76342391385564));
#160649=CARTESIAN_POINT('Ctrl Pts',(-19.4428147572125,-20.9468607962405,
3.75637205774369));
#160650=CARTESIAN_POINT('Ctrl Pts',(-19.4295079082076,-20.9515391198206,
3.75554127869965));
#160651=CARTESIAN_POINT('Ctrl Pts',(-19.4082025843455,-20.9587910835033,
3.75420866601462));
#160652=CARTESIAN_POINT('Ctrl Pts',(-19.4002336772001,-20.9614507363524,
3.75370967776368));
#160653=CARTESIAN_POINT('Ctrl Pts',(-19.3861207167785,-20.966067811507,
3.75282491846104));
#160654=CARTESIAN_POINT('Ctrl Pts',(-19.3799831214154,-20.9680447376055,
3.75243979584654));
#160655=CARTESIAN_POINT('Ctrl Pts',(-19.3672398389072,-20.9720851960019,
3.75163941531339));
#160656=CARTESIAN_POINT('Ctrl Pts',(-19.3606328812423,-20.9741444367458,
3.75122402171573));
#160657=CARTESIAN_POINT('Ctrl Pts',(-19.3435841332429,-20.9793665723546,
3.75015098425139));
#160658=CARTESIAN_POINT('Ctrl Pts',(-19.3331278717998,-20.9824811795375,
3.74949176897933));
#160659=CARTESIAN_POINT('Ctrl Pts',(-19.2888354802327,-20.9953026425409,
3.74669438777854));
#160660=CARTESIAN_POINT('Ctrl Pts',(-19.2547856627965,-21.0042451508037,
3.74453156281268));
#160661=CARTESIAN_POINT('Ctrl Pts',(-19.1649577346654,-21.0254572458716,
3.73879018072131));
#160662=CARTESIAN_POINT('Ctrl Pts',(-19.1088812955984,-21.0363254608735,
3.73516993976684));
#160663=CARTESIAN_POINT('Ctrl Pts',(-18.9020664741558,-21.0677924445843,
3.72170210646169));
#160664=CARTESIAN_POINT('Ctrl Pts',(-18.7496716503156,-21.0743976122479,
3.71151603661502));
#160665=CARTESIAN_POINT('Ctrl Pts',(-18.5754032553887,-21.0631713745418,
3.70010994012028));
#160666=CARTESIAN_POINT('Ctrl Pts',(-18.5529239777217,-21.0613622317525,
3.69864423533809));
#160667=CARTESIAN_POINT('Ctrl Pts',(-18.4793791975006,-21.0542589343253,
3.69387531243316));
#160668=CARTESIAN_POINT('Ctrl Pts',(-18.428472714133,-21.0474661518653,
3.6906158705154));
#160669=CARTESIAN_POINT('Ctrl Pts',(-18.3700968251107,-21.0375036543208,
3.686963342813));
#160670=CARTESIAN_POINT('Ctrl Pts',(-18.3623415456984,-21.036135554764,
3.68647985595929));
#160671=CARTESIAN_POINT('Ctrl Pts',(-18.3499881034836,-21.0338851507914,
3.68571270205638));
#160672=CARTESIAN_POINT('Ctrl Pts',(-18.3453850076152,-21.0330308278389,
3.68542751260689));
#160673=CARTESIAN_POINT('Ctrl Pts',(-18.3372543307682,-21.031493876656,
3.68492499000434));
#160674=CARTESIAN_POINT('Ctrl Pts',(-18.3337256055918,-21.0308175290372,
3.68470730329842));
#160675=CARTESIAN_POINT('Ctrl Pts',(-18.3262686046166,-21.0293685606493,
3.68424816104702));
#160676=CARTESIAN_POINT('Ctrl Pts',(-18.3223408008086,-21.0285937811447,
3.68400683019085));
#160677=CARTESIAN_POINT('Ctrl Pts',(-18.3117869240203,-21.0264808539004,
3.68335970160561));
#160678=CARTESIAN_POINT('Ctrl Pts',(-18.305164958688,-21.025122091168,3.68295506454354));
#160679=CARTESIAN_POINT('Ctrl Pts',(-18.2728516921507,-21.0183302714414,
3.6809868957532));
#160680=CARTESIAN_POINT('Ctrl Pts',(-18.2472552510869,-21.0124509809377,
3.67944745098241));
#160681=CARTESIAN_POINT('Ctrl Pts',(-18.1742405819998,-20.9942434414176,
3.67509535991703));
#160682=CARTESIAN_POINT('Ctrl Pts',(-18.1271301565414,-20.9807430849332,
3.67233501553222));
#160683=CARTESIAN_POINT('Ctrl Pts',(-17.9886450523871,-20.9358010394224,
3.6642513840977));
#160684=CARTESIAN_POINT('Ctrl Pts',(-17.8989076960573,-20.8997276132652,
3.65904957781845));
#160685=CARTESIAN_POINT('Ctrl Pts',(-17.6849926586906,-20.7962241369201,
3.64611851301049));
#160686=CARTESIAN_POINT('Ctrl Pts',(-17.5645144196338,-20.7222754066084,
3.63833946390108));
#160687=CARTESIAN_POINT('Ctrl Pts',(-17.4409213804632,-20.628257942425,
3.62924206006671));
#160688=CARTESIAN_POINT('Ctrl Pts',(-17.4296416124583,-20.6194957834451,
3.62840094930856));
#160689=CARTESIAN_POINT('Ctrl Pts',(-17.411829060187,-20.6053676102057,
3.62705488629684));
#160690=CARTESIAN_POINT('Ctrl Pts',(-17.4052381398353,-20.6000753515461,
3.62655287166917));
#160691=CARTESIAN_POINT('Ctrl Pts',(-17.3936690618374,-20.5906713101343,
3.62566459434516));
#160692=CARTESIAN_POINT('Ctrl Pts',(-17.3886776615513,-20.5865759360453,
3.62527899702558));
#160693=CARTESIAN_POINT('Ctrl Pts',(-17.3783916972999,-20.5780574177055,
3.62447944953752));
#160694=CARTESIAN_POINT('Ctrl Pts',(-17.3730998703272,-20.5736311021093,
3.62406537266661));
#160695=CARTESIAN_POINT('Ctrl Pts',(-17.3595700481087,-20.562201298001,
3.6229995851441));
#160696=CARTESIAN_POINT('Ctrl Pts',(-17.3513639766922,-20.5551604826089,
3.62234634345402));
#160697=CARTESIAN_POINT('Ctrl Pts',(-17.3173225602285,-20.5254971458285,
3.6196075126603));
#160698=CARTESIAN_POINT('Ctrl Pts',(-17.2919868361175,-20.5023115991706,
3.61749853309025));
#160699=CARTESIAN_POINT('Ctrl Pts',(-17.2274367227848,-20.4402879953586,
3.61193407543417));
#160700=CARTESIAN_POINT('Ctrl Pts',(-17.1891592080074,-20.4005165406864,
3.60844003970799));
#160701=CARTESIAN_POINT('Ctrl Pts',(-17.0797169735442,-20.2775255702836,
3.59785715484333));
#160702=CARTESIAN_POINT('Ctrl Pts',(-17.0134092598667,-20.1902384301811,
3.59061995961833));
#160703=CARTESIAN_POINT('Ctrl Pts',(-16.9253148622675,-20.0534462249615,
3.57987230278306));
#160704=CARTESIAN_POINT('Ctrl Pts',(-16.8981766621931,-20.0075940145309,
3.57636186681366));
#160705=CARTESIAN_POINT('Ctrl Pts',(-16.8669437743949,-19.9499683788807,
3.57209596865354));
#160706=CARTESIAN_POINT('Ctrl Pts',(-16.8611855458393,-19.9391199844147,
3.57129908728673));
#160707=CARTESIAN_POINT('Ctrl Pts',(-16.8307532799089,-19.8805612281633,
3.56703290106919));
#160708=CARTESIAN_POINT('Ctrl Pts',(-16.807805072,-19.8319705603094,3.56361766533237));
#160709=CARTESIAN_POINT('Ctrl Pts',(-16.7833021256937,-19.774522383476,
3.55976484314492));
#160710=CARTESIAN_POINT('Ctrl Pts',(-16.779925545335,-19.7664681085246,
3.55922881886242));
#160711=CARTESIAN_POINT('Ctrl Pts',(-16.7748900638979,-19.7542452133867,
3.55842187739812));
#160712=CARTESIAN_POINT('Ctrl Pts',(-16.7731944603826,-19.75009195009,3.55814881572958));
#160713=CARTESIAN_POINT('Ctrl Pts',(-16.7701754192076,-19.7426293181134,
3.55766024530236));
#160714=CARTESIAN_POINT('Ctrl Pts',(-16.7688471312163,-19.7393219834874,
3.55744444743217));
#160715=CARTESIAN_POINT('Ctrl Pts',(-16.7659800356315,-19.7321306763522,
3.55697681494913));
#160716=CARTESIAN_POINT('Ctrl Pts',(-16.7644443751468,-19.7282455111885,
3.55672517056206));
#160717=CARTESIAN_POINT('Ctrl Pts',(-16.7601655837186,-19.7173258813387,
3.55602063045228));
#160718=CARTESIAN_POINT('Ctrl Pts',(-16.7574485384548,-19.7102811690266,
3.55556927538782));
#160719=CARTESIAN_POINT('Ctrl Pts',(-16.7414798344364,-19.6682087151315,
3.5528917129827));
#160720=CARTESIAN_POINT('Ctrl Pts',(-16.7291209747682,-19.6328465439972,
3.55071541726821));
#160721=CARTESIAN_POINT('Ctrl Pts',(-16.6916345280616,-19.5156938909797,
3.54368991079821));
#160722=CARTESIAN_POINT('Ctrl Pts',(-16.6705236685077,-19.4327028859298,
3.53900142683909));
#160723=CARTESIAN_POINT('Ctrl Pts',(-16.6212212041362,-19.1742301047384,
3.52467922389372));
#160724=CARTESIAN_POINT('Ctrl Pts',(-16.6100300165562,-18.9963325385406,
3.51514288356901));
#160725=CARTESIAN_POINT('Ctrl Pts',(-16.6226068843731,-18.7963418021158,
3.50349692494253));
#160726=CARTESIAN_POINT('Ctrl Pts',(-16.6244085276511,-18.7735788034323,
3.50215907793698));
#160727=CARTESIAN_POINT('Ctrl Pts',(-16.6274825309702,-18.7413728710314,
3.50024707615929));
#160728=CARTESIAN_POINT('Ctrl Pts',(-16.6284510170359,-18.7319020431186,
3.49968246037292));
#160729=CARTESIAN_POINT('Ctrl Pts',(-16.6301298608119,-18.7165111789643,
3.49876096907981));
#160730=CARTESIAN_POINT('Ctrl Pts',(-16.6308014124554,-18.7105869770904,
3.49840531969327));
#160731=CARTESIAN_POINT('Ctrl Pts',(-16.632260750175,-18.698181657758,3.49765855872333));
#160732=CARTESIAN_POINT('Ctrl Pts',(-16.6330535090957,-18.6917011986428,
3.49726729380674));
#160733=CARTESIAN_POINT('Ctrl Pts',(-16.6350132414274,-18.6762736894393,
3.49633302656511));
#160734=CARTESIAN_POINT('Ctrl Pts',(-16.6362074555004,-18.6673302838364,
3.49578916890026));
#160735=CARTESIAN_POINT('Ctrl Pts',(-16.6404362606815,-18.637133723556,
3.49394509935626));
#160736=CARTESIAN_POINT('Ctrl Pts',(-16.6437368836376,-18.6159197213011,
3.49263651248547));
#160737=CARTESIAN_POINT('Ctrl Pts',(-16.663566812613,-18.5000929542532,
3.48541771865636));
#160738=CARTESIAN_POINT('Ctrl Pts',(-16.6861953527151,-18.4066511612053,
3.47931513402387));
#160739=CARTESIAN_POINT('Ctrl Pts',(-16.7650870666264,-18.1565801944211,
3.46226905562621));
#160740=CARTESIAN_POINT('Ctrl Pts',(-16.8335759838245,-18.0045315827241,
3.45106738850449));
#160741=CARTESIAN_POINT('Ctrl Pts',(-16.9396684084912,-17.82787670827,3.43788089264322));
#160742=CARTESIAN_POINT('Ctrl Pts',(-16.9611615172917,-17.7942767079831,
3.43536743624608));
#160743=CARTESIAN_POINT('Ctrl Pts',(-16.9877110953604,-17.7552470253852,
3.43245945649443));
#160744=CARTESIAN_POINT('Ctrl Pts',(-16.9918611276591,-17.7492137456033,
3.4320102771075));
#160745=CARTESIAN_POINT('Ctrl Pts',(-16.9986503136441,-17.7394525470838,
3.43128427022541));
#160746=CARTESIAN_POINT('Ctrl Pts',(-17.0012703326298,-17.7357114815031,
3.43100619411151));
#160747=CARTESIAN_POINT('Ctrl Pts',(-17.0059601534859,-17.7290609019435,
3.43051220280399));
#160748=CARTESIAN_POINT('Ctrl Pts',(-17.0080252242335,-17.7261481236463,
3.43029597059652));
#160749=CARTESIAN_POINT('Ctrl Pts',(-17.012488550928,-17.7198862479496,
3.42983138873855));
#160750=CARTESIAN_POINT('Ctrl Pts',(-17.0148892078344,-17.7165389313289,
3.42958320798276));
#160751=CARTESIAN_POINT('Ctrl Pts',(-17.0215612462194,-17.7072929853906,
3.42889807392807));
#160752=CARTESIAN_POINT('Ctrl Pts',(-17.0258533656066,-17.7014092929413,
3.42846252755563));
#160753=CARTESIAN_POINT('Ctrl Pts',(-17.0498476960858,-17.6688715496211,
3.42605563313317));
#160754=CARTESIAN_POINT('Ctrl Pts',(-17.0701445885662,-17.6426593075903,
3.42412317563175));
#160755=CARTESIAN_POINT('Ctrl Pts',(-17.1933224983162,-17.4910750445309,
3.41291600934311));
#160756=CARTESIAN_POINT('Ctrl Pts',(-17.3097283755013,-17.3773727908762,
3.40434324969878));
#160757=CARTESIAN_POINT('Ctrl Pts',(-17.53019955142,-17.2066766759561,3.38907799497855));
#160758=CARTESIAN_POINT('Ctrl Pts',(-17.6281403069352,-17.1430339619579,
3.38256719283861));
#160759=CARTESIAN_POINT('Ctrl Pts',(-17.74341911688,-17.0809993606864,3.37489826862499));
#160760=CARTESIAN_POINT('Ctrl Pts',(-17.7560917917587,-17.074344706932,
3.37405538593873));
#160761=CARTESIAN_POINT('Ctrl Pts',(-17.7763617445352,-17.0639614490771,
3.37270701731893));
#160762=CARTESIAN_POINT('Ctrl Pts',(-17.7839157175794,-17.0601489352417,
3.37220448496859));
#160763=CARTESIAN_POINT('Ctrl Pts',(-17.7972748870594,-17.053506711104,
3.37131560448397));
#160764=CARTESIAN_POINT('Ctrl Pts',(-17.8030705883863,-17.0506580701087,
3.3709299246297));
#160765=CARTESIAN_POINT('Ctrl Pts',(-17.8150813455728,-17.0448227525706,
3.37013051304489));
#160766=CARTESIAN_POINT('Ctrl Pts',(-17.8212981340723,-17.0418398368857,
3.36971665612542));
#160767=CARTESIAN_POINT('Ctrl Pts',(-17.8372858275956,-17.0342645508872,
3.36865208090128));
#160768=CARTESIAN_POINT('Ctrl Pts',(-17.8470774026002,-17.0297164987353,
3.36799983827224));
#160769=CARTESIAN_POINT('Ctrl Pts',(-17.888027971071,-17.0110750073758,
3.36527068179004));
#160770=CARTESIAN_POINT('Ctrl Pts',(-17.9194899568447,-16.9976633667579,
3.36317058361158));
#160771=CARTESIAN_POINT('Ctrl Pts',(-18.0022416603367,-16.9647332183681,
3.35763512514042));
#160772=CARTESIAN_POINT('Ctrl Pts',(-18.0539873532097,-16.9464373562018,
3.35416170633538));
#160773=CARTESIAN_POINT('Ctrl Pts',(-18.2106712570855,-16.8977993402981,
3.34361843543464));
#160774=CARTESIAN_POINT('Ctrl Pts',(-18.3173020021354,-16.873545614891,
3.33640010712851));
#160775=CARTESIAN_POINT('Ctrl Pts',(-18.4467302746063,-16.8544696521033,
3.32775770745692));
#160776=CARTESIAN_POINT('Ctrl Pts',(-18.4681900765824,-16.8516422797544,
3.32632908382537));
#160777=CARTESIAN_POINT('Ctrl Pts',(-18.5860808693032,-16.8379456910899,
3.31851423229807));
#160778=CARTESIAN_POINT('Ctrl Pts',(-18.6831402305345,-16.8333864352845,
3.31219743472277));
#160779=CARTESIAN_POINT('Ctrl Pts',(-18.789869722037,-16.8357151623011,
3.30560165576851));
#160780=CARTESIAN_POINT('Ctrl Pts',(-18.7995583334116,-16.8359931348803,
3.30500613287629));
#160781=CARTESIAN_POINT('Ctrl Pts',(-18.8138609603363,-16.8365018170762,
3.30413210329348));
#160782=CARTESIAN_POINT('Ctrl Pts',(-18.8184765188449,-16.8366810988323,
3.30385083233343));
#160783=CARTESIAN_POINT('Ctrl Pts',(-18.8266639404182,-16.8370259625489,
3.30335332946701));
#160784=CARTESIAN_POINT('Ctrl Pts',(-18.8302360041293,-16.8371854887167,
3.30313676283711));
#160785=CARTESIAN_POINT('Ctrl Pts',(-18.8378885350119,-16.8375466752888,
3.30267386013529));
#160786=CARTESIAN_POINT('Ctrl Pts',(-18.841968816306,-16.83775109662,3.30242768036104));
#160787=CARTESIAN_POINT('Ctrl Pts',(-18.8531677295385,-16.8383446643873,
3.30175369164198));
#160788=CARTESIAN_POINT('Ctrl Pts',(-18.8602851030168,-16.8387579642702,
3.30132721528465));
#160789=CARTESIAN_POINT('Ctrl Pts',(-18.8982760273659,-16.8411566866239,
3.29906013320382));
#160790=CARTESIAN_POINT('Ctrl Pts',(-18.9291070962337,-16.8437828491535,
3.29725329225451));
#160791=CARTESIAN_POINT('Ctrl Pts',(-19.0222559743602,-16.8537783352635,
3.29186470316022));
#160792=CARTESIAN_POINT('Ctrl Pts',(-19.0843169673968,-16.8632432324067,
3.28836982246393));
#160793=CARTESIAN_POINT('Ctrl Pts',(-19.1792931399587,-16.8820811414239,
3.28304854736592));
#160794=CARTESIAN_POINT('Ctrl Pts',(-19.2125520155061,-16.8895165204692,
3.28119047272072));
#160795=CARTESIAN_POINT('Ctrl Pts',(-19.4135711000635,-16.9395809904895,
3.26992286268552));
#160796=CARTESIAN_POINT('Ctrl Pts',(-19.5757407703526,-17.0018428716841,
3.26060614985132));
#160797=CARTESIAN_POINT('Ctrl Pts',(-19.7489514508732,-17.0940176975786,
3.24920663689869));
#160798=CARTESIAN_POINT('Ctrl Pts',(-19.7692030571273,-17.1052246340875,
3.2478508445953));
#160799=CARTESIAN_POINT('Ctrl Pts',(-19.7975724039737,-17.1215370684914,
3.24591702942949));
#160800=CARTESIAN_POINT('Ctrl Pts',(-19.8058458968547,-17.126369377193,
3.24534883649737));
#160801=CARTESIAN_POINT('Ctrl Pts',(-19.8192235376731,-17.1343051540565,
3.24442310390202));
#160802=CARTESIAN_POINT('Ctrl Pts',(-19.8243479137603,-17.1373743897096,
3.24406681329985));
#160803=CARTESIAN_POINT('Ctrl Pts',(-19.8349259928411,-17.143771095013,
3.24332780767733));
#160804=CARTESIAN_POINT('Ctrl Pts',(-19.8403777544357,-17.1471016434035,
3.24294498232711));
#160805=CARTESIAN_POINT('Ctrl Pts',(-19.8532206524236,-17.1550275802876,
3.24203847591952));
#160806=CARTESIAN_POINT('Ctrl Pts',(-19.860598648776,-17.1596439452331,
3.24151402463974));
#160807=CARTESIAN_POINT('Ctrl Pts',(-19.8761590769948,-17.1695140409634,
3.24040003327959));
#160808=CARTESIAN_POINT('Ctrl Pts',(-19.8843341771871,-17.1747789031278,
3.23981008691391));
#160809=CARTESIAN_POINT('Ctrl Pts',(-19.9510641806848,-17.2184071406053,
3.23495567788343));
#160810=CARTESIAN_POINT('Ctrl Pts',(-20.0077135852105,-17.2595930329532,
3.23058526770339));
#160811=CARTESIAN_POINT('Ctrl Pts',(-20.204160162884,-17.41787270299,3.21449467864826));
#160812=CARTESIAN_POINT('Ctrl Pts',(-20.3307340145016,-17.550092909698,
3.2022186384488));
#160813=CARTESIAN_POINT('Ctrl Pts',(-20.4746945688649,-17.7456254667022,
3.18645674799399));
#160814=CARTESIAN_POINT('Ctrl Pts',(-20.5084970030197,-17.7959208813146,
3.18259024483368));
#160815=CARTESIAN_POINT('Ctrl Pts',(-20.5447854385542,-17.8552658458411,
3.17829709609899));
#160816=CARTESIAN_POINT('Ctrl Pts',(-20.5494233970414,-17.862960236993,
3.17774549514192));
#160817=CARTESIAN_POINT('Ctrl Pts',(-20.556331044366,-17.8745868143683,
3.17691981671473));
#160818=CARTESIAN_POINT('Ctrl Pts',(-20.5586372279976,-17.8784970447523,
3.17664344662023));
#160819=CARTESIAN_POINT('Ctrl Pts',(-20.5627335848153,-17.8854939253556,
3.17615131277197));
#160820=CARTESIAN_POINT('Ctrl Pts',(-20.5645285437771,-17.8885777026366,
3.17593524148028));
#160821=CARTESIAN_POINT('Ctrl Pts',(-20.568388443538,-17.8952478231693,
3.175469681873));
#160822=CARTESIAN_POINT('Ctrl Pts',(-20.5704506616512,-17.8988356761564,
3.17522036948238));
#160823=CARTESIAN_POINT('Ctrl Pts',(-20.576156204574,-17.908829911938,3.1745289120667));
#160824=CARTESIAN_POINT('Ctrl Pts',(-20.5797766571047,-17.91524937888,3.17408821694127));
#160825=CARTESIAN_POINT('Ctrl Pts',(-20.600144166551,-17.9518081301121,
3.17159718489627));
#160826=CARTESIAN_POINT('Ctrl Pts',(-20.6161875052244,-17.9823359703258,
3.1695890088521));
#160827=CARTESIAN_POINT('Ctrl Pts',(-20.6645332732958,-18.0800558020181,
3.16334241150832));
#160828=CARTESIAN_POINT('Ctrl Pts',(-20.6940384747307,-18.148572161805,
3.15922662494613));
#160829=CARTESIAN_POINT('Ctrl Pts',(-20.7207777061902,-18.220966334771,
3.15501082377172));
#160830=CARTESIAN_POINT('Ctrl Pts',(-20.7216814543783,-18.2234272117775,
3.15486767429015));
#160831=CARTESIAN_POINT('Ctrl Pts',(-20.7225805742799,-18.2258896092214,
3.15472458816501));
#160832=CARTESIAN_POINT('Ctrl Pts',(-20.7225805736403,-18.2258896074698,
2.9354567758078));
#160833=CARTESIAN_POINT('Ctrl Pts',(-20.7189843536169,-18.2160407286345,
2.93605735418876));
#160834=CARTESIAN_POINT('Ctrl Pts',(-20.7153147924264,-18.2062180923754,
2.93665493133054));
#160835=CARTESIAN_POINT('Ctrl Pts',(-20.6612838647028,-18.0648029998778,
2.94524329629832));
#160836=CARTESIAN_POINT('Ctrl Pts',(-20.5979773450729,-17.9385224517111,
2.95274653475215));
#160837=CARTESIAN_POINT('Ctrl Pts',(-20.4767571152221,-17.7470827157633,
2.965118514207));
#160838=CARTESIAN_POINT('Ctrl Pts',(-20.4265788956208,-17.6775577911004,
2.96985046744715));
#160839=CARTESIAN_POINT('Ctrl Pts',(-20.3428766244402,-17.5752763841308,
2.97737858817665));
#160840=CARTESIAN_POINT('Ctrl Pts',(-20.3122467006406,-17.5402674519987,
2.98006796802977));
#160841=CARTESIAN_POINT('Ctrl Pts',(-20.2724475184664,-17.4976936556449,
2.98349877117431));
#160842=CARTESIAN_POINT('Ctrl Pts',(-20.2643330904796,-17.4891574472824,
2.98419508992308));
#160843=CARTESIAN_POINT('Ctrl Pts',(-20.2511078907146,-17.4754752834189,
2.98532513730128));
#160844=CARTESIAN_POINT('Ctrl Pts',(-20.2460410921869,-17.4702870304024,
2.98575695145402));
#160845=CARTESIAN_POINT('Ctrl Pts',(-20.2364723931874,-17.4605891543958,
2.98657038829752));
#160846=CARTESIAN_POINT('Ctrl Pts',(-20.2319765851902,-17.4560736142701,
2.98695174024383));
#160847=CARTESIAN_POINT('Ctrl Pts',(-20.2218439581215,-17.4459879963035,
2.9878093996426));
#160848=CARTESIAN_POINT('Ctrl Pts',(-20.2161961337275,-17.4404291556478,
2.9882861949552));
#160849=CARTESIAN_POINT('Ctrl Pts',(-20.2017573966941,-17.4263766370199,
2.98950203354851));
#160850=CARTESIAN_POINT('Ctrl Pts',(-20.1929239736271,-17.417927234267,
2.99024298776385));
#160851=CARTESIAN_POINT('Ctrl Pts',(-20.1410560003854,-17.3691673156042,
2.99457763020889));
#160852=CARTESIAN_POINT('Ctrl Pts',(-20.0964291091927,-17.3305957500309,
2.99824448473656));
#160853=CARTESIAN_POINT('Ctrl Pts',(-20.0322504144338,-17.2796473889378,
3.00343722176584));
#160854=CARTESIAN_POINT('Ctrl Pts',(-20.0140157604129,-17.2656498016767,
3.00490392852665));
#160855=CARTESIAN_POINT('Ctrl Pts',(-19.8762572259285,-17.1634230950747,
3.01591749261086));
#160856=CARTESIAN_POINT('Ctrl Pts',(-19.747975118475,-17.0877022525259,
3.02584367188202));
#160857=CARTESIAN_POINT('Ctrl Pts',(-19.561180903465,-17.0024652853895,
3.03930122532286));
#160858=CARTESIAN_POINT('Ctrl Pts',(-19.5085863124353,-16.9809772237723,
3.04298513856761));
#160859=CARTESIAN_POINT('Ctrl Pts',(-19.4279314484675,-16.9517528654554,
3.04841761159787));
#160860=CARTESIAN_POINT('Ctrl Pts',(-19.4004733291517,-16.9424371245519,
3.05023006749216));
#160861=CARTESIAN_POINT('Ctrl Pts',(-19.3661731828607,-16.9315805301787,
3.05244118199199));
#160862=CARTESIAN_POINT('Ctrl Pts',(-19.3595048816588,-16.9295061401032,
3.05286858399254));
#160863=CARTESIAN_POINT('Ctrl Pts',(-19.3489502596895,-16.9262799784452,
3.05354105790895));
#160864=CARTESIAN_POINT('Ctrl Pts',(-19.345070755755,-16.9251063274758,
3.05378737986643));
#160865=CARTESIAN_POINT('Ctrl Pts',(-19.3377567865251,-16.922916568922,
3.05425012471986));
#160866=CARTESIAN_POINT('Ctrl Pts',(-19.3343231553902,-16.9218980476742,
3.05446668177415));
#160867=CARTESIAN_POINT('Ctrl Pts',(-19.3264786844876,-16.9195927773217,
3.05495988787756));
#160868=CARTESIAN_POINT('Ctrl Pts',(-19.3220662356164,-16.9183116724023,
3.05523620581616));
#160869=CARTESIAN_POINT('Ctrl Pts',(-19.3103651369411,-16.914955656489,
3.05596611322994));
#160870=CARTESIAN_POINT('Ctrl Pts',(-19.3030693813276,-16.9129054775131,
3.05641830172112));
#160871=CARTESIAN_POINT('Ctrl Pts',(-19.2525952298821,-16.8990137443759,
3.05952755652775));
#160872=CARTESIAN_POINT('Ctrl Pts',(-19.2090582999983,-16.8885044652083,
3.06211308673206));
#160873=CARTESIAN_POINT('Ctrl Pts',(-19.1583506230665,-16.8779544980118,
3.06504805793413));
#160874=CARTESIAN_POINT('Ctrl Pts',(-19.1514765912673,-16.8765599278267,
3.06544431710876));
#160875=CARTESIAN_POINT('Ctrl Pts',(-19.1224766395757,-16.8708264664554,
3.0671097274662));
#160876=CARTESIAN_POINT('Ctrl Pts',(-19.1002885778672,-16.8668069384044,
3.06836848375035));
#160877=CARTESIAN_POINT('Ctrl Pts',(-18.9305672089543,-16.8388534072115,
3.07790703647508));
#160878=CARTESIAN_POINT('Ctrl Pts',(-18.7809355827223,-16.8302490165657,
3.08583099852675));
#160879=CARTESIAN_POINT('Ctrl Pts',(-18.5728501230387,-16.8403219584417,
3.09738096150395));
#160880=CARTESIAN_POINT('Ctrl Pts',(-18.5142075431053,-16.8456182804935,
3.10069079874861));
#160881=CARTESIAN_POINT('Ctrl Pts',(-18.4201980566194,-16.8580774143171,
3.10613883521242));
#160882=CARTESIAN_POINT('Ctrl Pts',(-18.3846593851271,-16.8637125763828,
3.10823125268132));
#160883=CARTESIAN_POINT('Ctrl Pts',(-18.3384695212449,-16.872248676956,
3.11100070417082));
#160884=CARTESIAN_POINT('Ctrl Pts',(-18.3276719142188,-16.8743312571223,
3.1116516829094));
#160885=CARTESIAN_POINT('Ctrl Pts',(-18.3100877337299,-16.8778651088371,
3.11271784752408));
#160886=CARTESIAN_POINT('Ctrl Pts',(-18.3032911204841,-16.8792658116447,
3.1131314140681));
#160887=CARTESIAN_POINT('Ctrl Pts',(-18.2901994267912,-16.8820310291557,
3.11393092398268));
#160888=CARTESIAN_POINT('Ctrl Pts',(-18.2839034378841,-16.8833909087535,
3.11431671480448));
#160889=CARTESIAN_POINT('Ctrl Pts',(-18.2694533322152,-16.8865810999715,
3.11520517431173));
#160890=CARTESIAN_POINT('Ctrl Pts',(-18.2613036904933,-16.8884309958241,
3.11570846720079));
#160891=CARTESIAN_POINT('Ctrl Pts',(-18.2395758359834,-16.8934984904283,
3.11705631887774));
#160892=CARTESIAN_POINT('Ctrl Pts',(-18.226018298626,-16.8968021274566,
3.11790363290874));
#160893=CARTESIAN_POINT('Ctrl Pts',(-18.1162945233602,-16.9246911205168,
3.12481336577925));
#160894=CARTESIAN_POINT('Ctrl Pts',(-18.0219469884596,-16.9558745120497,
3.13109045023209));
#160895=CARTESIAN_POINT('Ctrl Pts',(-17.8032023036515,-17.0456595430858,
3.14642330491281));
#160896=CARTESIAN_POINT('Ctrl Pts',(-17.6816281939147,-17.1099825485712,
3.15560040410879));
#160897=CARTESIAN_POINT('Ctrl Pts',(-17.5252449601914,-17.2132872656533,
3.16784040676498));
#160898=CARTESIAN_POINT('Ctrl Pts',(-17.4843401028195,-17.2424499035351,
3.17108389014052));
#160899=CARTESIAN_POINT('Ctrl Pts',(-17.4233301878936,-17.2893073797455,
3.17594397430546));
#160900=CARTESIAN_POINT('Ctrl Pts',(-17.4024601395307,-17.3059733113391,
3.17761066245976));
#160901=CARTESIAN_POINT('Ctrl Pts',(-17.376679220801,-17.3273721925587,
3.17966896859267));
#160902=CARTESIAN_POINT('Ctrl Pts',(-17.3714693573658,-17.3317390762166,
3.18008488467663));
#160903=CARTESIAN_POINT('Ctrl Pts',(-17.3632183201068,-17.338722999153,
3.18074340955068));
#160904=CARTESIAN_POINT('Ctrl Pts',(-17.3601634470322,-17.3413236756751,
3.18098718390694));
#160905=CARTESIAN_POINT('Ctrl Pts',(-17.3543883840835,-17.3462684896978,
3.18144792088457));
#160906=CARTESIAN_POINT('Ctrl Pts',(-17.3516667996478,-17.3486108341045,
3.18166500181216));
#160907=CARTESIAN_POINT('Ctrl Pts',(-17.3454222998186,-17.3540129091287,
3.18216299237442));
#160908=CARTESIAN_POINT('Ctrl Pts',(-17.3419035333888,-17.3570773684487,
3.18244354741235));
#160909=CARTESIAN_POINT('Ctrl Pts',(-17.3325137043957,-17.3653096277068,
3.18319213288148));
#160910=CARTESIAN_POINT('Ctrl Pts',(-17.3266610369521,-17.3704984281846,
3.18365864546064));
#160911=CARTESIAN_POINT('Ctrl Pts',(-17.2835876265928,-17.4091144918838,
3.18709258576527));
#160912=CARTESIAN_POINT('Ctrl Pts',(-17.2475302829614,-17.4438221653688,
3.18997053400485));
#160913=CARTESIAN_POINT('Ctrl Pts',(-17.1954854466555,-17.4976007652329,
3.19419123180259));
#160914=CARTESIAN_POINT('Ctrl Pts',(-17.1785511370833,-17.515725977811,
3.19557589495216));
#160915=CARTESIAN_POINT('Ctrl Pts',(-17.1318547353183,-17.5675010916156,
3.19944012691856));
#160916=CARTESIAN_POINT('Ctrl Pts',(-17.1028390432233,-17.6018071130015,
3.20189612836868));
#160917=CARTESIAN_POINT('Ctrl Pts',(-17.0070173732553,-17.72270112243,3.21029482615913));
#160918=CARTESIAN_POINT('Ctrl Pts',(-16.9458402864307,-17.8135235278335,
3.2161825470462));
#160919=CARTESIAN_POINT('Ctrl Pts',(-16.8647983488402,-17.9566054534937,
3.22532602475029));
#160920=CARTESIAN_POINT('Ctrl Pts',(-16.839526304835,-18.0055889428265,
3.22843304907867));
#160921=CARTESIAN_POINT('Ctrl Pts',(-16.8016680748937,-18.0865757902056,
3.23357631824372));
#160922=CARTESIAN_POINT('Ctrl Pts',(-16.7878994557455,-18.1179986769741,
3.23557319031905));
#160923=CARTESIAN_POINT('Ctrl Pts',(-16.7708048958734,-18.1597432199516,
3.23823356323112));
#160924=CARTESIAN_POINT('Ctrl Pts',(-16.7667856448499,-18.1697765685351,
3.23887354193017));
#160925=CARTESIAN_POINT('Ctrl Pts',(-16.76032743814,-18.1862629681567,3.23992621484952));
#160926=CARTESIAN_POINT('Ctrl Pts',(-16.757842849447,-18.1926980192562,
3.24033736798002));
#160927=CARTESIAN_POINT('Ctrl Pts',(-16.75309356181,-18.2051798246134,3.24113543293024));
#160928=CARTESIAN_POINT('Ctrl Pts',(-16.7508249867812,-18.2112250296219,
3.24152220941669));
#160929=CARTESIAN_POINT('Ctrl Pts',(-16.7456497624845,-18.2252099204902,
3.24241760717204));
#160930=CARTESIAN_POINT('Ctrl Pts',(-16.7427629665166,-18.2331567904292,
3.24292688465869));
#160931=CARTESIAN_POINT('Ctrl Pts',(-16.7351250803477,-18.2545817008641,
3.24430126836301));
#160932=CARTESIAN_POINT('Ctrl Pts',(-16.7304627973821,-18.2680907294162,
3.24516930314691));
#160933=CARTESIAN_POINT('Ctrl Pts',(-16.6889155219294,-18.3925465770094,
3.25318084185257));
#160934=CARTESIAN_POINT('Ctrl Pts',(-16.6611499802037,-18.5063054517084,
3.26062649665945));
#160935=CARTESIAN_POINT('Ctrl Pts',(-16.6175000989483,-18.7826956361877,
3.27890436611869));
#160936=CARTESIAN_POINT('Ctrl Pts',(-16.6107477305492,-18.9460246569622,
3.28987716959584));
#160937=CARTESIAN_POINT('Ctrl Pts',(-16.6251785692284,-19.1406850008487,
3.30227739287311));
#160938=CARTESIAN_POINT('Ctrl Pts',(-16.6282990647217,-19.1728023788463,
3.30429910398492));
#160939=CARTESIAN_POINT('Ctrl Pts',(-16.6330153371594,-19.2120088745054,
3.3067273133095));
#160940=CARTESIAN_POINT('Ctrl Pts',(-16.6339146751838,-19.2191755981908,
3.30716954264857));
#160941=CARTESIAN_POINT('Ctrl Pts',(-16.6353827729412,-19.2304090394308,
3.30785999945032));
#160942=CARTESIAN_POINT('Ctrl Pts',(-16.6359267052709,-19.2344788656722,
3.30810958955294));
#160943=CARTESIAN_POINT('Ctrl Pts',(-16.6369660263569,-19.242086669096,
3.30857507365987));
#160944=CARTESIAN_POINT('Ctrl Pts',(-16.6374585242223,-19.2456249355406,
3.30879112174236));
#160945=CARTESIAN_POINT('Ctrl Pts',(-16.6386038540456,-19.2537035491606,
3.30928341475434));
#160946=CARTESIAN_POINT('Ctrl Pts',(-16.6392624862227,-19.2582430233319,
3.30955932862126));
#160947=CARTESIAN_POINT('Ctrl Pts',(-16.6413346149369,-19.2722051999186,
3.31040587146329));
#160948=CARTESIAN_POINT('Ctrl Pts',(-16.6427969970258,-19.2816206788458,
3.31097380747373));
#160949=CARTESIAN_POINT('Ctrl Pts',(-16.6634632591337,-19.4090026304001,
3.31862150857607));
#160950=CARTESIAN_POINT('Ctrl Pts',(-16.6925631239484,-19.5251645372952,
3.32518438122037));
#160951=CARTESIAN_POINT('Ctrl Pts',(-16.7897756523401,-19.8088544672473,
3.3415077460384));
#160952=CARTESIAN_POINT('Ctrl Pts',(-16.8697804148336,-19.9712577305101,
3.35119077557762));
#160953=CARTESIAN_POINT('Ctrl Pts',(-16.98128353714,-20.1394919427283,3.36294181459621));
#160954=CARTESIAN_POINT('Ctrl Pts',(-16.9934449610202,-20.1572469536441,
3.36420443967313));
#160955=CARTESIAN_POINT('Ctrl Pts',(-17.0110913380963,-20.1821854779148,
3.36601152113869));
#160956=CARTESIAN_POINT('Ctrl Pts',(-17.0163551176466,-20.1895243923299,
3.36654752159014));
#160957=CARTESIAN_POINT('Ctrl Pts',(-17.0255055982009,-20.2021114049617,
3.36747421490887));
#160958=CARTESIAN_POINT('Ctrl Pts',(-17.0293699478217,-20.2073756527556,
3.36786403902431));
#160959=CARTESIAN_POINT('Ctrl Pts',(-17.0368078309837,-20.2174103159717,
3.36861148471517));
#160960=CARTESIAN_POINT('Ctrl Pts',(-17.0403772806056,-20.2221836912667,
3.36896894439813));
#160961=CARTESIAN_POINT('Ctrl Pts',(-17.0496943817044,-20.2345342228267,
3.36989883371197));
#160962=CARTESIAN_POINT('Ctrl Pts',(-17.0554729727319,-20.2420877732378,
3.37047247748487));
#160963=CARTESIAN_POINT('Ctrl Pts',(-17.0752613334934,-20.2675963242239,
3.37242666728757));
#160964=CARTESIAN_POINT('Ctrl Pts',(-17.08950948013,-20.2853636107827,3.37381665733718));
#160965=CARTESIAN_POINT('Ctrl Pts',(-17.2178354197352,-20.4401985122437,
3.38619210787419));
#160966=CARTESIAN_POINT('Ctrl Pts',(-17.3485021423432,-20.5625467944461,
3.39790730800877));
#160967=CARTESIAN_POINT('Ctrl Pts',(-17.5618104034091,-20.7169058298442,
3.41530114228959));
#160968=CARTESIAN_POINT('Ctrl Pts',(-17.6336513022824,-20.7625677690027,
3.42090105858941));
#160969=CARTESIAN_POINT('Ctrl Pts',(-17.7406927695132,-20.8218723223083,
3.42871059508615));
#160970=CARTESIAN_POINT('Ctrl Pts',(-17.773812010481,-20.839093313998,3.43105731415141));
#160971=CARTESIAN_POINT('Ctrl Pts',(-17.8141533229791,-20.8587322790657,
3.43381811558067));
#160972=CARTESIAN_POINT('Ctrl Pts',(-17.8209528628771,-20.8619975975332,
3.43428017246368));
#160973=CARTESIAN_POINT('Ctrl Pts',(-17.8315438207849,-20.8670141731043,
3.43499462511591));
#160974=CARTESIAN_POINT('Ctrl Pts',(-17.8353231341563,-20.8687906328252,
3.43524854038106));
#160975=CARTESIAN_POINT('Ctrl Pts',(-17.8423378767047,-20.8720625932222,
3.43571788434527));
#160976=CARTESIAN_POINT('Ctrl Pts',(-17.8455717973452,-20.8735610927136,
3.4359334929003));
#160977=CARTESIAN_POINT('Ctrl Pts',(-17.8528865314438,-20.8769281022962,
3.43641945404905));
#160978=CARTESIAN_POINT('Ctrl Pts',(-17.8569695001643,-20.8787918015944,
3.43668950885962));
#160979=CARTESIAN_POINT('Ctrl Pts',(-17.8690236782532,-20.8842477600165,
3.43748334668969));
#160980=CARTESIAN_POINT('Ctrl Pts',(-17.8770113618401,-20.8878036892465,
3.43800495162242));
#160981=CARTESIAN_POINT('Ctrl Pts',(-17.9341712078765,-20.9128267677483,
3.44170760911095));
#160982=CARTESIAN_POINT('Ctrl Pts',(-17.9841261743647,-20.9324691340475,
3.44478611407843));
#160983=CARTESIAN_POINT('Ctrl Pts',(-18.0363416526327,-20.9507407473983,
3.44789636329138));
#160984=CARTESIAN_POINT('Ctrl Pts',(-18.037906110668,-20.9512861331552,
3.44798945300118));
#160985=CARTESIAN_POINT('Ctrl Pts',(-18.178835146446,-21.0002299373614,
3.45636641883946));
#160986=CARTESIAN_POINT('Ctrl Pts',(-18.322883395962,-21.0339324152017,
3.46418901548635));
#160987=CARTESIAN_POINT('Ctrl Pts',(-18.5662393653546,-21.0646043497105,
3.47766689188908));
#160988=CARTESIAN_POINT('Ctrl Pts',(-18.6639245256478,-21.0700951227057,
3.48313960275757));
#160989=CARTESIAN_POINT('Ctrl Pts',(-18.783299321396,-21.0685368170402,
3.49008940250181));
#160990=CARTESIAN_POINT('Ctrl Pts',(-18.8049596666604,-21.0679213585148,
3.49136060243591));
#160991=CARTESIAN_POINT('Ctrl Pts',(-18.8356538619996,-21.066577383287,
3.49317784822377));
#160992=CARTESIAN_POINT('Ctrl Pts',(-18.844698803562,-21.066123172518,3.49371530619552));
#160993=CARTESIAN_POINT('Ctrl Pts',(-18.8602649303925,-21.0652413191265,
3.49464372852697));
#160994=CARTESIAN_POINT('Ctrl Pts',(-18.8667876103792,-21.0648414882721,
3.49503381546947));
#160995=CARTESIAN_POINT('Ctrl Pts',(-18.879250753923,-21.0640195749745,
3.49578121673235));
#160996=CARTESIAN_POINT('Ctrl Pts',(-18.8851915012086,-21.063602613047,
3.49613836650912));
#160997=CARTESIAN_POINT('Ctrl Pts',(-18.9005867993991,-21.0624567652107,
3.49706625479941));
#160998=CARTESIAN_POINT('Ctrl Pts',(-18.9100382768923,-21.0616894179121,
3.49763819706302));
#160999=CARTESIAN_POINT('Ctrl Pts',(-18.9420026723806,-21.0588779970453,
3.49958040923052));
#161000=CARTESIAN_POINT('Ctrl Pts',(-18.9644872949331,-21.0565368970037,
3.50095996651489));
#161001=CARTESIAN_POINT('Ctrl Pts',(-19.1659644661462,-21.0322916634332,
3.51344598014439));
#161002=CARTESIAN_POINT('Ctrl Pts',(-19.3414810967892,-20.9879636674441,
3.52530090045895));
#161003=CARTESIAN_POINT('Ctrl Pts',(-19.5870795254064,-20.8913157871317,
3.54273401533952));
#161004=CARTESIAN_POINT('Ctrl Pts',(-19.66306218108,-20.8560839497504,3.54824056464897));
#161005=CARTESIAN_POINT('Ctrl Pts',(-19.7693191502955,-20.7989352124162,
3.55593787172297));
#161006=CARTESIAN_POINT('Ctrl Pts',(-19.8014125794361,-20.780574907359,
3.55826174865167));
#161007=CARTESIAN_POINT('Ctrl Pts',(-19.8394398714855,-20.7574772975466,
3.56099934003732));
#161008=CARTESIAN_POINT('Ctrl Pts',(-19.8458481690119,-20.7535380191362,
3.56146011403399));
#161009=CARTESIAN_POINT('Ctrl Pts',(-19.855777463325,-20.7473611680652,
3.56217301605454));
#161010=CARTESIAN_POINT('Ctrl Pts',(-19.8593129982942,-20.7451472492753,
3.56242665320708));
#161011=CARTESIAN_POINT('Ctrl Pts',(-19.8658576162719,-20.7410220913646,
3.56289574191379));
#161012=CARTESIAN_POINT('Ctrl Pts',(-19.8688683886892,-20.7391137198135,
3.5631113716836));
#161013=CARTESIAN_POINT('Ctrl Pts',(-19.8756641113796,-20.734782166603,
3.5635977078792));
#161014=CARTESIAN_POINT('Ctrl Pts',(-19.8794461640324,-20.7323545385483,
3.56386811451777));
#161015=CARTESIAN_POINT('Ctrl Pts',(-19.8905864468391,-20.7251536080428,
3.56466394647772));
#161016=CARTESIAN_POINT('Ctrl Pts',(-19.8979228802584,-20.7203465332218,
3.56518717733244));
#161017=CARTESIAN_POINT('Ctrl Pts',(-19.950759722872,-20.6852547976941,
3.56895082240495));
#161018=CARTESIAN_POINT('Ctrl Pts',(-19.9951061769294,-20.6532609195377,
3.57208474954758));
#161019=CARTESIAN_POINT('Ctrl Pts',(-20.1707488300931,-20.5158959470292,
3.58461108215611));
#161020=CARTESIAN_POINT('Ctrl Pts',(-20.2904968955431,-20.3967638835054,
3.59346953487657));
#161021=CARTESIAN_POINT('Ctrl Pts',(-20.4314207942789,-20.2184616133704,
3.60606882687358));
#161022=CARTESIAN_POINT('Ctrl Pts',(-20.466016053466,-20.1707214601449,
3.60938274878419));
#161023=CARTESIAN_POINT('Ctrl Pts',(-20.5184689858925,-20.0915860170233,
3.61483690256046));
#161024=CARTESIAN_POINT('Ctrl Pts',(-20.5375947524117,-20.0610678944997,
3.61693121802819));
#161025=CARTESIAN_POINT('Ctrl Pts',(-20.5615339674283,-20.0206110628523,
3.61970283292729));
#161026=CARTESIAN_POINT('Ctrl Pts',(-20.567061873677,-20.0111006402215,
3.62035402539116));
#161027=CARTESIAN_POINT('Ctrl Pts',(-20.5759561201111,-19.995520397025,
3.62142045227264));
#161028=CARTESIAN_POINT('Ctrl Pts',(-20.5793672167413,-19.9894762652877,
3.62183406582366));
#161029=CARTESIAN_POINT('Ctrl Pts',(-20.585886552817,-19.9777907588083,
3.62263360509031));
#161030=CARTESIAN_POINT('Ctrl Pts',(-20.588998892178,-19.9721517504557,
3.62301937792684));
#161031=CARTESIAN_POINT('Ctrl Pts',(-20.5960893372995,-19.9591653828508,
3.62390770805839));
#161032=CARTESIAN_POINT('Ctrl Pts',(-20.6000497574506,-19.9518085357159,
3.62441088895957));
#161033=CARTESIAN_POINT('Ctrl Pts',(-20.6105051153137,-19.932108206293,
3.62575824584063));
#161034=CARTESIAN_POINT('Ctrl Pts',(-20.6169217054464,-19.9197238141047,
3.62660517388026));
#161035=CARTESIAN_POINT('Ctrl Pts',(-20.667862316851,-19.8189805017949,
3.63349516038651));
#161036=CARTESIAN_POINT('Ctrl Pts',(-20.7062580256466,-19.7276752427533,
3.63975146334344));
#161037=CARTESIAN_POINT('Ctrl Pts',(-20.7819943072982,-19.5051266499831,
3.65499316859155));
#161038=CARTESIAN_POINT('Ctrl Pts',(-20.8133221629822,-19.3722922033889,
3.66409683868163));
#161039=CARTESIAN_POINT('Ctrl Pts',(-20.8417531160729,-19.1633140867206,
3.67787832339337));
#161040=CARTESIAN_POINT('Ctrl Pts',(-20.8479010495714,-19.0887540779393,
3.68268512141501));
#161041=CARTESIAN_POINT('Ctrl Pts',(-20.8503509139228,-19.0051628183103,
3.68784417170587));
#161042=CARTESIAN_POINT('Ctrl Pts',(-20.8505548518314,-18.9963062253306,
3.68838787831956));
#161043=CARTESIAN_POINT('Ctrl Pts',(-20.8507777608891,-18.9829958412862,
3.68920038145952));
#161044=CARTESIAN_POINT('Ctrl Pts',(-20.8508382797348,-18.9785429738362,
3.68947141983799));
#161045=CARTESIAN_POINT('Ctrl Pts',(-20.8509183444026,-18.9708703424099,
3.68993706203665));
#161046=CARTESIAN_POINT('Ctrl Pts',(-20.8509445960242,-18.9676507038288,
3.69013203820979));
#161047=CARTESIAN_POINT('Ctrl Pts',(-20.8509874023548,-18.9603608802205,
3.69057254223413));
#161048=CARTESIAN_POINT('Ctrl Pts',(-20.850999564596,-18.9562907096263,
3.69081782134309));
#161049=CARTESIAN_POINT('Ctrl Pts',(-20.8510007238669,-18.9451601480982,
3.69148680677765));
#161050=CARTESIAN_POINT('Ctrl Pts',(-20.8509661391287,-18.9380997334676,
3.69190921330968));
#161051=CARTESIAN_POINT('Ctrl Pts',(-20.8505991936736,-18.9010402233319,
3.69411677269202));
#161052=CARTESIAN_POINT('Ctrl Pts',(-20.8496644750514,-18.8710488854179,
3.69587022658714));
#161053=CARTESIAN_POINT('Ctrl Pts',(-20.8449576296193,-18.7813334830055,
3.70104316947266));
#161054=CARTESIAN_POINT('Ctrl Pts',(-20.8392906868578,-18.7217363983877,
3.70438375873542));
#161055=CARTESIAN_POINT('Ctrl Pts',(-20.8105320875148,-18.5134442303815,
3.71596092773406));
#161056=CARTESIAN_POINT('Ctrl Pts',(-20.7741426799691,-18.3671014728962,
3.723948917646));
#161057=CARTESIAN_POINT('Ctrl Pts',(-20.7225805737618,-18.2258896078024,
3.73234499902338));
#161058=CARTESIAN_POINT('Origin',(-18.734,-18.952,0.));
#161059=CARTESIAN_POINT('',(-20.7225805756119,-18.2258896128692,4.75730100916854));
#161060=CARTESIAN_POINT('',(-20.7225805465488,-18.2258895332749,4.53222344315201));
#161061=CARTESIAN_POINT('',(-20.7225805737622,-18.2258896078036,0.));
#161062=CARTESIAN_POINT('',(-20.8510004573069,-18.9525763811924,4.70909255089851));
#161063=CARTESIAN_POINT('Ctrl Pts',(-20.7225805756119,-18.2258896128692,
4.75730100916854));
#161064=CARTESIAN_POINT('Ctrl Pts',(-20.7394204630776,-18.2720085965712,
4.75422026792543));
#161065=CARTESIAN_POINT('Ctrl Pts',(-20.7546509859817,-18.3186997180878,
4.75109074222835));
#161066=CARTESIAN_POINT('Ctrl Pts',(-20.8232026681109,-18.556621319464,
4.73511031612701));
#161067=CARTESIAN_POINT('Ctrl Pts',(-20.8510537300821,-18.7541142038182,
4.72162174956493));
#161068=CARTESIAN_POINT('Ctrl Pts',(-20.8509999221896,-18.9525739767941,
4.70909177449283));
#161069=CARTESIAN_POINT('Ctrl Pts',(-20.8509999215522,-18.9525763226662,
4.70909162638368));
#161070=CARTESIAN_POINT('Ctrl Pts',(-20.8509956361641,-18.9683177933136,
4.70809777210637));
#161071=CARTESIAN_POINT('Ctrl Pts',(-20.8508157763218,-18.9840592918394,
4.70711104263526));
#161072=CARTESIAN_POINT('Ctrl Pts',(-20.8502148550793,-19.0106677173036,
4.70545679613841));
#161073=CARTESIAN_POINT('Ctrl Pts',(-20.8498856304571,-19.021535774254,
4.70478498365393));
#161074=CARTESIAN_POINT('Ctrl Pts',(-20.8492914998136,-19.0371682430673,
4.70382466716472));
#161075=CARTESIAN_POINT('Ctrl Pts',(-20.8490942019335,-19.041934847292,
4.70353265478901));
#161076=CARTESIAN_POINT('Ctrl Pts',(-20.8487208814591,-19.0502719292856,
4.70302336263931));
#161077=CARTESIAN_POINT('Ctrl Pts',(-20.8485519258392,-19.0538426822487,
4.70280570115822));
#161078=CARTESIAN_POINT('Ctrl Pts',(-20.8482044718395,-19.0608119131399,
4.70238181422817));
#161079=CARTESIAN_POINT('Ctrl Pts',(-20.8480268213021,-19.064210430191,
4.70217554205354));
#161080=CARTESIAN_POINT('Ctrl Pts',(-20.8476550554517,-19.0710079708271,
4.70176385304503));
#161081=CARTESIAN_POINT('Ctrl Pts',(-20.8474609360373,-19.0744069556023,
4.70155843620369));
#161082=CARTESIAN_POINT('Ctrl Pts',(-20.8469736816507,-19.0825917698856,
4.70106481870128));
#161083=CARTESIAN_POINT('Ctrl Pts',(-20.8466724839536,-19.0873771261272,
4.70077706715283));
#161084=CARTESIAN_POINT('Ctrl Pts',(-20.8455076200067,-19.1049326369219,
4.69972440335841));
#161085=CARTESIAN_POINT('Ctrl Pts',(-20.8445443860772,-19.1176962076478,
4.69896485939855));
#161086=CARTESIAN_POINT('Ctrl Pts',(-20.8412948277738,-19.1561092511592,
4.69669428548022));
#161087=CARTESIAN_POINT('Ctrl Pts',(-20.8386561572594,-19.1817273610097,
4.6952006328698));
#161088=CARTESIAN_POINT('Ctrl Pts',(-20.8126752036858,-19.395601144094,
4.68285649487282));
#161089=CARTESIAN_POINT('Ctrl Pts',(-20.7645928184162,-19.5799984010765,
4.67295994885061));
#161090=CARTESIAN_POINT('Ctrl Pts',(-20.6698522696631,-19.8109231607585,
4.65913210644751));
#161091=CARTESIAN_POINT('Ctrl Pts',(-20.6447914006982,-19.8653172694487,
4.65576807668629));
#161092=CARTESIAN_POINT('Ctrl Pts',(-20.6008326662732,-19.9509750429593,
4.6502389452701));
#161093=CARTESIAN_POINT('Ctrl Pts',(-20.5833720719599,-19.9829403697677,
4.64812142982974));
#161094=CARTESIAN_POINT('Ctrl Pts',(-20.5595535596603,-20.0239912249072,
4.64532338115277));
#161095=CARTESIAN_POINT('Ctrl Pts',(-20.5539360688136,-20.0335006629245,
4.64466959096941));
#161096=CARTESIAN_POINT('Ctrl Pts',(-20.5446628799948,-20.0489217103262,
4.64359997605349));
#161097=CARTESIAN_POINT('Ctrl Pts',(-20.5410519815476,-20.054860117055,
4.64318579088357));
#161098=CARTESIAN_POINT('Ctrl Pts',(-20.5340402940104,-20.0662645024054,
4.64238589126276));
#161099=CARTESIAN_POINT('Ctrl Pts',(-20.5306436819236,-20.0717329682412,
4.64200033369208));
#161100=CARTESIAN_POINT('Ctrl Pts',(-20.5227931860363,-20.0842443983085,
4.64111356041141));
#161101=CARTESIAN_POINT('Ctrl Pts',(-20.5183225750907,-20.0912766937104,
4.64061172828545));
#161102=CARTESIAN_POINT('Ctrl Pts',(-20.5062991728745,-20.1099451999045,
4.63927032576621));
#161103=CARTESIAN_POINT('Ctrl Pts',(-20.4986734230881,-20.1215337274407,
4.63842804148149));
#161104=CARTESIAN_POINT('Ctrl Pts',(-20.4373813341076,-20.2127123608421,
4.63172336173501));
#161105=CARTESIAN_POINT('Ctrl Pts',(-20.3784792952977,-20.2886327202349,
4.62566071632389));
#161106=CARTESIAN_POINT('Ctrl Pts',(-20.2144279288533,-20.4727611334893,
4.60969389042609));
#161107=CARTESIAN_POINT('Ctrl Pts',(-20.1025089562092,-20.5742083254242,
4.599590028446));
#161108=CARTESIAN_POINT('Ctrl Pts',(-19.9458032578401,-20.6884027855696,
4.58698689948742));
#161109=CARTESIAN_POINT('Ctrl Pts',(-19.9100533195716,-20.7128125479089,
4.5842058921462));
#161110=CARTESIAN_POINT('Ctrl Pts',(-19.8600571198533,-20.7447469892644,
4.58046833843027));
#161111=CARTESIAN_POINT('Ctrl Pts',(-19.8464379320344,-20.7532296591141,
4.57946513797292));
#161112=CARTESIAN_POINT('Ctrl Pts',(-19.8259213924213,-20.7656868510066,
4.57797755733392));
#161113=CARTESIAN_POINT('Ctrl Pts',(-19.8190962333495,-20.7697784489669,
4.57748655713292));
#161114=CARTESIAN_POINT('Ctrl Pts',(-19.8066052418891,-20.7771712220598,
4.57659521931768));
#161115=CARTESIAN_POINT('Ctrl Pts',(-19.8009468640458,-20.7804847242108,
4.5761941399543));
#161116=CARTESIAN_POINT('Ctrl Pts',(-19.7918811798887,-20.7857371066348,
4.57555594911289));
#161117=CARTESIAN_POINT('Ctrl Pts',(-19.7884837786593,-20.7876928741311,
4.57531776753106));
#161118=CARTESIAN_POINT('Ctrl Pts',(-19.7850704059233,-20.7896452328837,
4.57507946610141));
#161119=CARTESIAN_POINT('Ctrl Pts',(-19.7850598806106,-20.7896512529636,
4.57507873129605));
#161120=CARTESIAN_POINT('Ctrl Pts',(-19.7850387628336,-20.7896633312908,
4.57507725701638));
#161121=CARTESIAN_POINT('Ctrl Pts',(-19.7850281709602,-20.7896693891987,
4.57507651758343));
#161122=CARTESIAN_POINT('Ctrl Pts',(-19.785006899568,-20.7896815548981,
4.57507503261827));
#161123=CARTESIAN_POINT('Ctrl Pts',(-19.784996251202,-20.7896876448706,
4.57507428926086));
#161124=CARTESIAN_POINT('Ctrl Pts',(-19.7819654538141,-20.7914209720074,
4.57486271352688));
#161125=CARTESIAN_POINT('Ctrl Pts',(-19.7789410960357,-20.7931407362307,
4.57465237488139));
#161126=CARTESIAN_POINT('Ctrl Pts',(-19.7718898819355,-20.797127352347,
4.5741637849482));
#161127=CARTESIAN_POINT('Ctrl Pts',(-19.7678598345856,-20.7993884801959,
4.57388590307482));
#161128=CARTESIAN_POINT('Ctrl Pts',(-19.7571231115253,-20.8053663672551,
4.57314911936777));
#161129=CARTESIAN_POINT('Ctrl Pts',(-19.7504035211481,-20.8090599556381,
4.57269166101939));
#161130=CARTESIAN_POINT('Ctrl Pts',(-19.702691852327,-20.8349493031433,
4.56946829392327));
#161131=CARTESIAN_POINT('Ctrl Pts',(-19.6609932679525,-20.855824091235,
4.56677998671634));
#161132=CARTESIAN_POINT('Ctrl Pts',(-19.6064242874687,-20.8809234153024,
4.56338213954585));
#161133=CARTESIAN_POINT('Ctrl Pts',(-19.5941589960978,-20.8864239951325,
4.56262605861538));
#161134=CARTESIAN_POINT('Ctrl Pts',(-19.4323495090433,-20.9571469264488,
4.55274123491598));
#161135=CARTESIAN_POINT('Ctrl Pts',(-19.275800652933,-21.0049891365391,
4.54413717891616));
#161136=CARTESIAN_POINT('Ctrl Pts',(-19.0356857083949,-21.0489563911361,
4.53060672122021));
#161137=CARTESIAN_POINT('Ctrl Pts',(-18.9553060775102,-21.0589556061523,
4.52603185771475));
#161138=CARTESIAN_POINT('Ctrl Pts',(-18.855009070423,-21.0656294881102,
4.52016760183698));
#161139=CARTESIAN_POINT('Ctrl Pts',(-18.835444670874,-21.0666587783344,
4.51901658439269));
#161140=CARTESIAN_POINT('Ctrl Pts',(-18.8071792166809,-21.0677526869848,
4.51734234690472));
#161141=CARTESIAN_POINT('Ctrl Pts',(-18.7984872684684,-21.0680354484276,
4.51682595821711));
#161142=CARTESIAN_POINT('Ctrl Pts',(-18.7833241851723,-21.0684352131238,
4.51592233671));
#161143=CARTESIAN_POINT('Ctrl Pts',(-18.7768537560792,-21.0685761126754,
4.5155358577334));
#161144=CARTESIAN_POINT('Ctrl Pts',(-18.7643456771615,-21.0687911087188,
4.51478700380021));
#161145=CARTESIAN_POINT('Ctrl Pts',(-18.7583081497677,-21.068869049033,
4.51442475321397));
#161146=CARTESIAN_POINT('Ctrl Pts',(-18.7439645783304,-21.0689928434738,
4.51356223911529));
#161147=CARTESIAN_POINT('Ctrl Pts',(-18.7356584812932,-21.0690156443694,
4.51306125760957));
#161148=CARTESIAN_POINT('Ctrl Pts',(-18.7061860513453,-21.0689230996007,
4.51127813375996));
#161149=CARTESIAN_POINT('Ctrl Pts',(-18.6850223655456,-21.0685391953912,
4.50998762432205));
#161150=CARTESIAN_POINT('Ctrl Pts',(-18.4700720242088,-21.0614144662779,
4.49677402209619));
#161151=CARTESIAN_POINT('Ctrl Pts',(-18.2781107854518,-21.0283961381152,
4.48396670417523));
#161152=CARTESIAN_POINT('Ctrl Pts',(-18.0220320605073,-20.9470924163692,
4.46624541318947));
#161153=CARTESIAN_POINT('Ctrl Pts',(-17.9519342183132,-20.9206713155592,
4.46133988176395));
#161154=CARTESIAN_POINT('Ctrl Pts',(-17.8517247269387,-20.8767010855841,
4.45437312319282));
#161155=CARTESIAN_POINT('Ctrl Pts',(-17.8204129689883,-20.8620374295146,
4.45220348673806));
#161156=CARTESIAN_POINT('Ctrl Pts',(-17.7828717150715,-20.8433218613853,
4.44962325556869));
#161157=CARTESIAN_POINT('Ctrl Pts',(-17.7762881444837,-20.8399966639886,
4.44917156489774));
#161158=CARTESIAN_POINT('Ctrl Pts',(-17.7660368544956,-20.834751572612,
4.44846964984388));
#161159=CARTESIAN_POINT('Ctrl Pts',(-17.7623572346028,-20.8328552502403,
4.44821798887171));
#161160=CARTESIAN_POINT('Ctrl Pts',(-17.7555163688688,-20.8293043211756,
4.447750686974));
#161161=CARTESIAN_POINT('Ctrl Pts',(-17.7523537758621,-20.827652532211,
4.44753487955362));
#161162=CARTESIAN_POINT('Ctrl Pts',(-17.7451783526409,-20.8238817648832,
4.44704575592972));
#161163=CARTESIAN_POINT('Ctrl Pts',(-17.741168159685,-20.8217578799741,
4.44677275426929));
#161164=CARTESIAN_POINT('Ctrl Pts',(-17.7307902425689,-20.8162187086294,
4.44606710972104));
#161165=CARTESIAN_POINT('Ctrl Pts',(-17.7244330589556,-20.8127836537179,
4.44563568918966));
#161166=CARTESIAN_POINT('Ctrl Pts',(-17.6845977067841,-20.7909946891815,
4.44293679688666));
#161167=CARTESIAN_POINT('Ctrl Pts',(-17.651601309818,-20.7717692497599,
4.44072115258957));
#161168=CARTESIAN_POINT('Ctrl Pts',(-17.6086601237746,-20.7451679121406,
4.43784016549691));
#161169=CARTESIAN_POINT('Ctrl Pts',(-17.5982361918938,-20.7385837738038,
4.43714100626698));
#161170=CARTESIAN_POINT('Ctrl Pts',(-17.5823406566037,-20.7283482233389,
4.4360742271592));
#161171=CARTESIAN_POINT('Ctrl Pts',(-17.576827693612,-20.7247618307421,
4.43570412526519));
#161172=CARTESIAN_POINT('Ctrl Pts',(-17.4333767608454,-20.6304872335884,
4.42606839797569));
#161173=CARTESIAN_POINT('Ctrl Pts',(-17.3064941032793,-20.5239968610187,
4.41736987188445));
#161174=CARTESIAN_POINT('Ctrl Pts',(-17.1366846938526,-20.3437903046219,
4.40365776898426));
#161175=CARTESIAN_POINT('Ctrl Pts',(-17.0836655695203,-20.2804918285709,
4.39899842308611));
#161176=CARTESIAN_POINT('Ctrl Pts',(-17.0226760480942,-20.1983751990404,
4.39303223611609));
#161177=CARTESIAN_POINT('Ctrl Pts',(-17.0110975491467,-20.18232024722,4.39186946064101));
#161178=CARTESIAN_POINT('Ctrl Pts',(-16.9947378607424,-20.1589517277808,
4.39018117846389));
#161179=CARTESIAN_POINT('Ctrl Pts',(-16.9897739320065,-20.1517669284059,
4.38966266617503));
#161180=CARTESIAN_POINT('Ctrl Pts',(-16.9812054617203,-20.1391993391955,
4.3887565658211));
#161181=CARTESIAN_POINT('Ctrl Pts',(-16.9775808862501,-20.1338303007725,
4.38836974389897));
#161182=CARTESIAN_POINT('Ctrl Pts',(-16.9706308489813,-20.12343270472,4.38762112295267));
#161183=CARTESIAN_POINT('Ctrl Pts',(-16.9673021086385,-20.1184064059932,
4.38725945254638));
#161184=CARTESIAN_POINT('Ctrl Pts',(-16.9594582251438,-20.1064517648688,
4.38639973500791));
#161185=CARTESIAN_POINT('Ctrl Pts',(-16.9549621448496,-20.0995110871035,
4.38590098073955));
#161186=CARTESIAN_POINT('Ctrl Pts',(-16.9392200408535,-20.0748948285133,
4.38413330124108));
#161187=CARTESIAN_POINT('Ctrl Pts',(-16.9281961306753,-20.057079288413,
4.38285619663186));
#161188=CARTESIAN_POINT('Ctrl Pts',(-16.8170198525766,-19.8713025817194,
4.36955749566356));
#161189=CARTESIAN_POINT('Ctrl Pts',(-16.7403537964452,-19.6904257909128,
4.35663410099709));
#161190=CARTESIAN_POINT('Ctrl Pts',(-16.6623492899738,-19.4002960903783,
4.33682265673636));
#161191=CARTESIAN_POINT('Ctrl Pts',(-16.6426696297756,-19.2970342340231,
4.32996620057552));
#161192=CARTESIAN_POINT('Ctrl Pts',(-16.629677361173,-19.1835192046731,
4.32291230438946));
#161193=CARTESIAN_POINT('Ctrl Pts',(-16.6286838568976,-19.1743035204364,
4.32234311412888));
#161194=CARTESIAN_POINT('Ctrl Pts',(-16.6272943560971,-19.1605687008737,
4.32150028303963));
#161195=CARTESIAN_POINT('Ctrl Pts',(-16.6268523205152,-19.15605447989,4.32122414963919));
#161196=CARTESIAN_POINT('Ctrl Pts',(-16.6260915671063,-19.1480192264726,
4.3207342430941));
#161197=CARTESIAN_POINT('Ctrl Pts',(-16.6257671585498,-19.144498793391,
4.32052015434745));
#161198=CARTESIAN_POINT('Ctrl Pts',(-16.6250830412315,-19.1368656379594,
4.32005715840702));
#161199=CARTESIAN_POINT('Ctrl Pts',(-16.6247265442202,-19.1327526832205,
4.31980843322359));
#161200=CARTESIAN_POINT('Ctrl Pts',(-16.6237868683195,-19.1215300154826,
4.31913173921145));
#161201=CARTESIAN_POINT('Ctrl Pts',(-16.623227583917,-19.1144182811866,
4.31870509021443));
#161202=CARTESIAN_POINT('Ctrl Pts',(-16.6206619198955,-19.0795390470501,
4.31662263802556));
#161203=CARTESIAN_POINT('Ctrl Pts',(-16.6191673596634,-19.0517352520293,
4.31499376850785));
#161204=CARTESIAN_POINT('Ctrl Pts',(-16.6174480459763,-19.0011476052357,
4.3120736842937));
#161205=CARTESIAN_POINT('Ctrl Pts',(-16.6170417809572,-18.9783748204424,
4.31077518281084));
#161206=CARTESIAN_POINT('Ctrl Pts',(-16.6169556454356,-18.9277105634466,
4.30791337245531));
#161207=CARTESIAN_POINT('Ctrl Pts',(-16.6174593272411,-18.8998228752555,
4.30635633985962));
#161208=CARTESIAN_POINT('Ctrl Pts',(-16.6201690247286,-18.8282113321721,
4.30238731691615));
#161209=CARTESIAN_POINT('Ctrl Pts',(-16.6231804165231,-18.7845308530063,
4.29999424763356));
#161210=CARTESIAN_POINT('Ctrl Pts',(-16.6384422448624,-18.6321875904551,
4.29165862003666));
#161211=CARTESIAN_POINT('Ctrl Pts',(-16.6577514473825,-18.5244098407094,
4.28577144546639));
#161212=CARTESIAN_POINT('Ctrl Pts',(-16.7043621617311,-18.3453823325774,
4.27548482915905));
#161213=CARTESIAN_POINT('Ctrl Pts',(-16.7273378551811,-18.2732363856319,
4.27119533143887));
#161214=CARTESIAN_POINT('Ctrl Pts',(-16.7608130177595,-18.1848109353364,
4.26567516157173));
#161215=CARTESIAN_POINT('Ctrl Pts',(-16.7677379395606,-18.1672328987087,
4.2645646111783));
#161216=CARTESIAN_POINT('Ctrl Pts',(-16.7781446660458,-18.141819553038,
4.26293880282761));
#161217=CARTESIAN_POINT('Ctrl Pts',(-16.7814403886477,-18.1339086818589,
4.26242982954687));
#161218=CARTESIAN_POINT('Ctrl Pts',(-16.7873012555541,-18.120077754298,
4.26153482044794));
#161219=CARTESIAN_POINT('Ctrl Pts',(-16.7898456141496,-18.1141489708324,
4.26114949576392));
#161220=CARTESIAN_POINT('Ctrl Pts',(-16.7948375713383,-18.1026620470568,
4.26039965080252));
#161221=CARTESIAN_POINT('Ctrl Pts',(-16.7972820667713,-18.097102620803,
4.26003523965215));
#161222=CARTESIAN_POINT('Ctrl Pts',(-16.8031810063599,-18.0838420336578,
4.2591623979966));
#161223=CARTESIAN_POINT('Ctrl Pts',(-16.8066576318921,-18.0761509070661,
4.25865320912794));
#161224=CARTESIAN_POINT('Ctrl Pts',(-16.8193572420039,-18.048498124709,
4.25681170432923));
#161225=CARTESIAN_POINT('Ctrl Pts',(-16.8288448633642,-18.028660204738,
4.25547028904417));
#161226=CARTESIAN_POINT('Ctrl Pts',(-16.9218504330035,-17.8417309709721,
4.24263174756426));
#161227=CARTESIAN_POINT('Ctrl Pts',(-17.026816802389,-17.686266711004,4.23032333190481));
#161228=CARTESIAN_POINT('Ctrl Pts',(-17.2034579078826,-17.4872720984696,
4.21275803813741));
#161229=CARTESIAN_POINT('Ctrl Pts',(-17.2594402441859,-17.4309273063874,
4.20754582033244));
#161230=CARTESIAN_POINT('Ctrl Pts',(-17.3450899978938,-17.3539071244404,
4.20020448090626));
#161231=CARTESIAN_POINT('Ctrl Pts',(-17.3723276669348,-17.3306361782222,
4.19795454430411));
#161232=CARTESIAN_POINT('Ctrl Pts',(-17.40593232047,-17.3033700262208,4.19529224826232));
#161233=CARTESIAN_POINT('Ctrl Pts',(-17.4117449699798,-17.298704445285,
4.19483573493524));
#161234=CARTESIAN_POINT('Ctrl Pts',(-17.4208373847754,-17.2914849527131,
4.19412798481151));
#161235=CARTESIAN_POINT('Ctrl Pts',(-17.4241001696066,-17.2889098908023,
4.19387527310076));
#161236=CARTESIAN_POINT('Ctrl Pts',(-17.4301763850375,-17.284143381945,
4.19340702716097));
#161237=CARTESIAN_POINT('Ctrl Pts',(-17.4329877418883,-17.2819494553036,
4.1931913201905));
#161238=CARTESIAN_POINT('Ctrl Pts',(-17.4393705153862,-17.2769943654663,
4.19270370593182));
#161239=CARTESIAN_POINT('Ctrl Pts',(-17.4429452188959,-17.2742375224107,
4.1924321052258));
#161240=CARTESIAN_POINT('Ctrl Pts',(-17.4535657445287,-17.2661009218965,
4.19162948798825));
#161241=CARTESIAN_POINT('Ctrl Pts',(-17.4606366702142,-17.260753885237,
4.19110072211353));
#161242=CARTESIAN_POINT('Ctrl Pts',(-17.5135253556929,-17.2212791748119,
4.18718545958272));
#161243=CARTESIAN_POINT('Ctrl Pts',(-17.5606785595797,-17.1889710846047,
4.18391541245938));
#161244=CARTESIAN_POINT('Ctrl Pts',(-17.7373360986381,-17.078161730896,
4.17222377550504));
#161245=CARTESIAN_POINT('Ctrl Pts',(-17.8738514152183,-17.0117013736056,
4.16420804402765));
#161246=CARTESIAN_POINT('Ctrl Pts',(-18.1035139377817,-16.9289401534201,
4.15076219570785));
#161247=CARTESIAN_POINT('Ctrl Pts',(-18.1926929172031,-16.903276596604,
4.14555636384181));
#161248=CARTESIAN_POINT('Ctrl Pts',(-18.3038460490648,-16.879055120033,
4.13892983092316));
#161249=CARTESIAN_POINT('Ctrl Pts',(-18.3244970633135,-16.8748769428532,
4.13769329115882));
#161250=CARTESIAN_POINT('Ctrl Pts',(-18.354009170546,-16.8693631709015,
4.13591716638905));
#161251=CARTESIAN_POINT('Ctrl Pts',(-18.3628221173852,-16.8677744440461,
4.13538564220391));
#161252=CARTESIAN_POINT('Ctrl Pts',(-18.37806512875,-16.8651263017487,4.13446424764891));
#161253=CARTESIAN_POINT('Ctrl Pts',(-18.3844905400722,-16.8640405652931,
4.13407521953175));
#161254=CARTESIAN_POINT('Ctrl Pts',(-18.3968182073372,-16.86201599143,4.13332758941227));
#161255=CARTESIAN_POINT('Ctrl Pts',(-18.4027196348812,-16.8610724460349,
4.13296914105122));
#161256=CARTESIAN_POINT('Ctrl Pts',(-18.4181095289915,-16.8586786332849,
4.13203290742792));
#161257=CARTESIAN_POINT('Ctrl Pts',(-18.4276039248941,-16.8572678991258,
4.13145387492879));
#161258=CARTESIAN_POINT('Ctrl Pts',(-18.4601864003512,-16.8526528548455,
4.12946164038942));
#161259=CARTESIAN_POINT('Ctrl Pts',(-18.4833169877505,-16.8497654073732,
4.12803848849328));
#161260=CARTESIAN_POINT('Ctrl Pts',(-18.676284952268,-16.8289066859607,
4.11608805901549));
#161261=CARTESIAN_POINT('Ctrl Pts',(-18.8476467851267,-16.8311702138189,
4.10489891875928));
#161262=CARTESIAN_POINT('Ctrl Pts',(-19.1063780758457,-16.8660501245892,
4.08764679579089));
#161263=CARTESIAN_POINT('Ctrl Pts',(-19.1950601337237,-16.8838419152233,
4.08168373699695));
#161264=CARTESIAN_POINT('Ctrl Pts',(-19.3196747113404,-16.9172596287982,
4.07344070960928));
#161265=CARTESIAN_POINT('Ctrl Pts',(-19.3567325587045,-16.9282935386706,
4.07100783619525));
#161266=CARTESIAN_POINT('Ctrl Pts',(-19.4007095398341,-16.9427102167108,
4.06815970144026));
#161267=CARTESIAN_POINT('Ctrl Pts',(-19.4079363608653,-16.9451226172756,
4.0676929411998));
#161268=CARTESIAN_POINT('Ctrl Pts',(-19.419119611067,-16.9489229433357,
4.06697280601723));
#161269=CARTESIAN_POINT('Ctrl Pts',(-19.4230851201527,-16.9502836678763,
4.06671787331074));
#161270=CARTESIAN_POINT('Ctrl Pts',(-19.4304131787936,-16.9528225744732,
4.0662475879667));
#161271=CARTESIAN_POINT('Ctrl Pts',(-19.4337767684433,-16.9539974552095,
4.06603204949048));
#161272=CARTESIAN_POINT('Ctrl Pts',(-19.441350765548,-16.9566644774353,
4.06554742614101));
#161273=CARTESIAN_POINT('Ctrl Pts',(-19.4455594134304,-16.9581614520906,
4.06527863186256));
#161274=CARTESIAN_POINT('Ctrl Pts',(-19.4578988539727,-16.9625945163389,
4.06449191973399));
#161275=CARTESIAN_POINT('Ctrl Pts',(-19.466016550509,-16.9655671406344,
4.0639761219348));
#161276=CARTESIAN_POINT('Ctrl Pts',(-19.5224627289239,-16.986630212118,
4.0604002852531));
#161277=CARTESIAN_POINT('Ctrl Pts',(-19.5701380319181,-17.0064342721398,
4.0574350446848));
#161278=CARTESIAN_POINT('Ctrl Pts',(-19.6369264924716,-17.0370871436343,
4.05329621495599));
#161279=CARTESIAN_POINT('Ctrl Pts',(-19.6566651142311,-17.0465193175835,
4.05207499299354));
#161280=CARTESIAN_POINT('Ctrl Pts',(-19.7995539146676,-17.1175403016805,
4.04322481883443));
#161281=CARTESIAN_POINT('Ctrl Pts',(-19.9165826885246,-17.1907083248481,
4.03590143513793));
#161282=CARTESIAN_POINT('Ctrl Pts',(-20.0975672381432,-17.3300857386213,
4.02330718542647));
#161283=CARTESIAN_POINT('Ctrl Pts',(-20.1658130826768,-17.3900044663649,
4.01820667831549));
#161284=CARTESIAN_POINT('Ctrl Pts',(-20.2447378582517,-17.4688297678791,
4.0117075684252));
#161285=CARTESIAN_POINT('Ctrl Pts',(-20.2592564804963,-17.4837645158633,
4.01048494693836));
#161286=CARTESIAN_POINT('Ctrl Pts',(-20.2796703504513,-17.5053930653889,
4.0087253621927));
#161287=CARTESIAN_POINT('Ctrl Pts',(-20.2857476135237,-17.5119139623791,
4.00819625278742));
#161288=CARTESIAN_POINT('Ctrl Pts',(-20.2961911255587,-17.5232627055851,
4.00727770927457));
#161289=CARTESIAN_POINT('Ctrl Pts',(-20.3005766554149,-17.5280727018293,
4.006889103194));
#161290=CARTESIAN_POINT('Ctrl Pts',(-20.3089521336291,-17.5373443520888,
4.00614134217163));
#161291=CARTESIAN_POINT('Ctrl Pts',(-20.3129454851778,-17.5418028580787,
4.00578233634828));
#161292=CARTESIAN_POINT('Ctrl Pts',(-20.3233262532745,-17.5534921723223,
4.0048425500341));
#161293=CARTESIAN_POINT('Ctrl Pts',(-20.3296831879249,-17.5607497556598,
4.00426050367409));
#161294=CARTESIAN_POINT('Ctrl Pts',(-20.3514218806424,-17.5859133700444,
4.00224718124831));
#161295=CARTESIAN_POINT('Ctrl Pts',(-20.3665531867615,-17.6040325515282,
4.00080567044052));
#161296=CARTESIAN_POINT('Ctrl Pts',(-20.4850680651712,-17.7508728413211,
3.98918383764586));
#161297=CARTESIAN_POINT('Ctrl Pts',(-20.5733553141143,-17.8910107571822,
3.97838998571285));
#161298=CARTESIAN_POINT('Ctrl Pts',(-20.6734508076956,-18.1006783079954,
3.9630363360022));
#161299=CARTESIAN_POINT('Ctrl Pts',(-20.6995189376785,-18.1627312566259,
3.95859032807702));
#161300=CARTESIAN_POINT('Ctrl Pts',(-20.722580643286,-18.2258897982069,
3.95421663535643));
#161301=CARTESIAN_POINT('',(-20.8509992439666,-18.9537891464354,4.48828857340046));
#161302=CARTESIAN_POINT('Ctrl Pts',(-20.7225805737618,-18.2258896078024,
3.73234499902339));
#161303=CARTESIAN_POINT('Ctrl Pts',(-20.7168697221505,-18.2102494397289,
3.73327492175908));
#161304=CARTESIAN_POINT('Ctrl Pts',(-20.7109727301829,-18.1946721917005,
3.73420940116923));
#161305=CARTESIAN_POINT('Ctrl Pts',(-20.6832637474869,-18.1240088539995,
3.73849011524215));
#161306=CARTESIAN_POINT('Ctrl Pts',(-20.6593332283651,-18.0697928105943,
3.74189148108078));
#161307=CARTESIAN_POINT('Ctrl Pts',(-20.6277538838877,-18.0056728464178,
3.74609045171824));
#161308=CARTESIAN_POINT('Ctrl Pts',(-20.6222502083618,-17.9947382826347,
3.74681283467328));
#161309=CARTESIAN_POINT('Ctrl Pts',(-20.6130255220663,-17.9768000343595,
3.74800864578225));
#161310=CARTESIAN_POINT('Ctrl Pts',(-20.6093593923728,-17.969768340775,
3.74848014291643));
#161311=CARTESIAN_POINT('Ctrl Pts',(-20.6026761185634,-17.9571235391769,
3.7493330553719));
#161312=CARTESIAN_POINT('Ctrl Pts',(-20.5996729600961,-17.9515031169549,
3.74971397141702));
#161313=CARTESIAN_POINT('Ctrl Pts',(-20.5931997963148,-17.9395190601124,
3.75053009033484));
#161314=CARTESIAN_POINT('Ctrl Pts',(-20.5897224009617,-17.9331595292752,
3.75096555342475));
#161315=CARTESIAN_POINT('Ctrl Pts',(-20.5802117912778,-17.9159765604133,
3.75214866567443));
#161316=CARTESIAN_POINT('Ctrl Pts',(-20.5741161655625,-17.9051881579636,
3.7528985466986));
#161317=CARTESIAN_POINT('Ctrl Pts',(-20.5423240187755,-17.8500563176615,
3.75676760963817));
#161318=CARTESIAN_POINT('Ctrl Pts',(-20.5151198986635,-17.8066062554593,
3.75994119002768));
#161319=CARTESIAN_POINT('Ctrl Pts',(-20.3905653456497,-17.622851978179,
3.77392306328615));
#161320=CARTESIAN_POINT('Ctrl Pts',(-20.2780247687421,-17.4936399234176,
3.78529485027403));
#161321=CARTESIAN_POINT('Ctrl Pts',(-20.0828494593477,-17.3177524352721,
3.80257317049292));
#161322=CARTESIAN_POINT('Ctrl Pts',(-20.0105243814876,-17.2606545437336,
3.80854937783097));
#161323=CARTESIAN_POINT('Ctrl Pts',(-19.9267413771648,-17.2029572659246,
3.81483430344893));
#161324=CARTESIAN_POINT('Ctrl Pts',(-19.9187408255114,-17.1975280957139,
3.8154283430354));
#161325=CARTESIAN_POINT('Ctrl Pts',(-19.9068673184446,-17.1895889964345,
3.81630061898091));
#161326=CARTESIAN_POINT('Ctrl Pts',(-19.903023032076,-17.1870367019195,
3.81658160396411));
#161327=CARTESIAN_POINT('Ctrl Pts',(-19.8961854867887,-17.1825292667591,
3.81707879084146));
#161328=CARTESIAN_POINT('Ctrl Pts',(-19.8931955929792,-17.1805691209102,
3.81729532587539));
#161329=CARTESIAN_POINT('Ctrl Pts',(-19.8867759856138,-17.176383701083,
3.81775837123296));
#161330=CARTESIAN_POINT('Ctrl Pts',(-19.8833447970638,-17.1741607912693,
3.81800472415984));
#161331=CARTESIAN_POINT('Ctrl Pts',(-19.8739015151528,-17.1680816861667,
3.81867967564129));
#161332=CARTESIAN_POINT('Ctrl Pts',(-19.86787624839,-17.1642459141915,3.81910693525725));
#161333=CARTESIAN_POINT('Ctrl Pts',(-19.8354946652376,-17.1438608947054,
3.82138569286831));
#161334=CARTESIAN_POINT('Ctrl Pts',(-19.8087937604208,-17.1278629093827,
3.82320301273716));
#161335=CARTESIAN_POINT('Ctrl Pts',(-19.6393307700231,-17.0313418143417,
3.83441822222573));
#161336=CARTESIAN_POINT('Ctrl Pts',(-19.4879600044594,-16.9670293801568,
3.84307893037099));
#161337=CARTESIAN_POINT('Ctrl Pts',(-19.2182121849648,-16.8877893440932,
3.85846831213238));
#161338=CARTESIAN_POINT('Ctrl Pts',(-19.1032203073109,-16.864154665791,
3.86501037276029));
#161339=CARTESIAN_POINT('Ctrl Pts',(-18.9726798996914,-16.8484493711898,
3.87271296574712));
#161340=CARTESIAN_POINT('Ctrl Pts',(-18.9584707412171,-16.8468857005147,
3.87355476065347));
#161341=CARTESIAN_POINT('Ctrl Pts',(-18.9358327568135,-16.8446262684153,
3.87490171391459));
#161342=CARTESIAN_POINT('Ctrl Pts',(-18.9274135616089,-16.8438368902485,
3.87540392848714));
#161343=CARTESIAN_POINT('Ctrl Pts',(-18.9125575901256,-16.8425337450693,
3.87629243871259));
#161344=CARTESIAN_POINT('Ctrl Pts',(-18.9061227332175,-16.8419989438469,
3.87667806786772));
#161345=CARTESIAN_POINT('Ctrl Pts',(-18.8928091424546,-16.8409537586411,
3.87747756266242));
#161346=CARTESIAN_POINT('Ctrl Pts',(-18.8859301671272,-16.8404475380783,
3.87789155441923));
#161347=CARTESIAN_POINT('Ctrl Pts',(-18.8682679991568,-16.8392345420039,
3.87895687284404));
#161348=CARTESIAN_POINT('Ctrl Pts',(-18.8574817442179,-16.8385767039793,
3.87960972795125));
#161349=CARTESIAN_POINT('Ctrl Pts',(-18.8124547088774,-16.8361764443806,
3.88234481127979));
#161350=CARTESIAN_POINT('Ctrl Pts',(-18.7781807484749,-16.8351834502245,
3.88445034999934));
#161351=CARTESIAN_POINT('Ctrl Pts',(-18.6888394547021,-16.8347656773168,
3.89000356659341));
#161352=CARTESIAN_POINT('Ctrl Pts',(-18.6337946447766,-16.8366563589487,
3.89348960818688));
#161353=CARTESIAN_POINT('Ctrl Pts',(-18.4698251781524,-16.8487026087623,
3.90405713853167));
#161354=CARTESIAN_POINT('Ctrl Pts',(-18.3615529764208,-16.8651535753061,
3.91128702477762));
#161355=CARTESIAN_POINT('Ctrl Pts',(-18.211490921814,-16.9000076486786,
3.92146366081904));
#161356=CARTESIAN_POINT('Ctrl Pts',(-18.1682667023315,-16.911501443557,
3.92441203990845));
#161357=CARTESIAN_POINT('Ctrl Pts',(-18.101277103865,-16.9316071981858,
3.92898249715486));
#161358=CARTESIAN_POINT('Ctrl Pts',(-18.0772469763796,-16.9392901665316,
3.93062212700737));
#161359=CARTESIAN_POINT('Ctrl Pts',(-18.0061325540957,-16.9634363283126,
3.93546462661598));
#161360=CARTESIAN_POINT('Ctrl Pts',(-17.9594829648241,-16.9811370611288,
3.93862846713814));
#161361=CARTESIAN_POINT('Ctrl Pts',(-17.9062944398526,-17.0034996590645,
3.94218670786626));
#161362=CARTESIAN_POINT('Ctrl Pts',(-17.8991070586414,-17.0065684659426,
3.9426664709249));
#161363=CARTESIAN_POINT('Ctrl Pts',(-17.8876574002023,-17.0115322836678,
3.94342885061462));
#161364=CARTESIAN_POINT('Ctrl Pts',(-17.8833841857784,-17.0134016682366,
3.9437129607577));
#161365=CARTESIAN_POINT('Ctrl Pts',(-17.8758324061171,-17.0167350898375,
3.94421425445942));
#161366=CARTESIAN_POINT('Ctrl Pts',(-17.8725513443565,-17.0181933638216,
3.94443178573277));
#161367=CARTESIAN_POINT('Ctrl Pts',(-17.865611029865,-17.02129916862,3.9448913387585));
#161368=CARTESIAN_POINT('Ctrl Pts',(-17.8619527541751,-17.0229487551107,
3.94513323206303));
#161369=CARTESIAN_POINT('Ctrl Pts',(-17.8521059224498,-17.0274226152305,
3.94578346822859));
#161370=CARTESIAN_POINT('Ctrl Pts',(-17.8459261911831,-17.0302663590007,
3.94619063104797));
#161371=CARTESIAN_POINT('Ctrl Pts',(-17.8155053916162,-17.044443260245,
3.94819094726377));
#161372=CARTESIAN_POINT('Ctrl Pts',(-17.7914658130374,-17.0562060981686,
3.9497590559918));
#161373=CARTESIAN_POINT('Ctrl Pts',(-17.7228380190854,-17.0914147101625,
3.95421729099424));
#161374=CARTESIAN_POINT('Ctrl Pts',(-17.6788533313467,-17.1160009921855,
3.95705200676497));
#161375=CARTESIAN_POINT('Ctrl Pts',(-17.5228334666803,-17.2106728722606,
3.96717233163782));
#161376=CARTESIAN_POINT('Ctrl Pts',(-17.416543620544,-17.2896355191146,
3.97421052526027));
#161377=CARTESIAN_POINT('Ctrl Pts',(-17.2410259751958,-17.4474998421393,
3.98719700211521));
#161378=CARTESIAN_POINT('Ctrl Pts',(-17.1689801213214,-17.5225942139705,
3.99303628406593));
#161379=CARTESIAN_POINT('Ctrl Pts',(-17.0937843035524,-17.6135011799298,
3.99994986438718));
#161380=CARTESIAN_POINT('Ctrl Pts',(-17.0849324333799,-17.6244222174506,
4.00077789123713));
#161381=CARTESIAN_POINT('Ctrl Pts',(-17.070974088759,-17.6419984105496,
4.00210691902117));
#161382=CARTESIAN_POINT('Ctrl Pts',(-17.0657971709286,-17.6485972748951,
4.00260509890296));
#161383=CARTESIAN_POINT('Ctrl Pts',(-17.0567111757926,-17.660321731045,
4.00348892083461));
#161384=CARTESIAN_POINT('Ctrl Pts',(-17.0527860178988,-17.6654347683578,
4.00387391896328));
#161385=CARTESIAN_POINT('Ctrl Pts',(-17.0446917462228,-17.6760789217614,
4.00467453348143));
#161386=CARTESIAN_POINT('Ctrl Pts',(-17.0405263084735,-17.68161272499,4.00509028798615));
#161387=CARTESIAN_POINT('Ctrl Pts',(-17.0298536589532,-17.6959371566041,
4.00616531056579));
#161388=CARTESIAN_POINT('Ctrl Pts',(-17.0233873389283,-17.7047578683298,
4.00682616116333));
#161389=CARTESIAN_POINT('Ctrl Pts',(-16.9962585801112,-17.7423720610006,
4.0096397853944));
#161390=CARTESIAN_POINT('Ctrl Pts',(-16.9762535228617,-17.7716305336951,
4.01181757638246));
#161391=CARTESIAN_POINT('Ctrl Pts',(-16.9256652404467,-17.8497583361539,
4.01760847568817));
#161392=CARTESIAN_POINT('Ctrl Pts',(-16.8963287769265,-17.8993961651912,
4.02126416786822));
#161393=CARTESIAN_POINT('Ctrl Pts',(-16.7931670747894,-18.0914347198208,
4.03530432881969));
#161394=CARTESIAN_POINT('Ctrl Pts',(-16.7335834175254,-18.2408522016946,
4.04607042921717));
#161395=CARTESIAN_POINT('Ctrl Pts',(-16.6876803118108,-18.4093498401971,
4.05742882719627));
#161396=CARTESIAN_POINT('Ctrl Pts',(-16.6840616688482,-18.4231840446689,
4.05835545116412));
#161397=CARTESIAN_POINT('Ctrl Pts',(-16.6781716169031,-18.4466714243848,
4.05991754687039));
#161398=CARTESIAN_POINT('Ctrl Pts',(-16.6758273864821,-18.4563057307955,
4.06055515887759));
#161399=CARTESIAN_POINT('Ctrl Pts',(-16.6640323666881,-18.5063074839135,
4.06384693626785));
#161400=CARTESIAN_POINT('Ctrl Pts',(-16.6557004798112,-18.5469327822474,
4.06646291261482));
#161401=CARTESIAN_POINT('Ctrl Pts',(-16.6472919455488,-18.5950778980493,
4.0694743436486));
#161402=CARTESIAN_POINT('Ctrl Pts',(-16.6460555825447,-18.6023830600729,
4.06992887936833));
#161403=CARTESIAN_POINT('Ctrl Pts',(-16.6441148723517,-18.614227515328,
4.0706618123081));
#161404=CARTESIAN_POINT('Ctrl Pts',(-16.6433869156504,-18.6187628012485,
4.07094149668904));
#161405=CARTESIAN_POINT('Ctrl Pts',(-16.6421189503297,-18.6268301361703,
4.07143725050983));
#161406=CARTESIAN_POINT('Ctrl Pts',(-16.6415731177856,-18.6303612125954,
4.07165364588344));
#161407=CARTESIAN_POINT('Ctrl Pts',(-16.6404198651223,-18.6379489790814,
4.0721173586375));
#161408=CARTESIAN_POINT('Ctrl Pts',(-16.6398152961342,-18.6420060457917,
4.07236451355341));
#161409=CARTESIAN_POINT('Ctrl Pts',(-16.6381814540095,-18.6531931750551,
4.07304392833033));
#161410=CARTESIAN_POINT('Ctrl Pts',(-16.6371767662285,-18.6603268506334,
4.07347481963509));
#161411=CARTESIAN_POINT('Ctrl Pts',(-16.6319088623105,-18.6991656178361,
4.07580867617781));
#161412=CARTESIAN_POINT('Ctrl Pts',(-16.628328049734,-18.7309609454628,
4.07767547651267));
#161413=CARTESIAN_POINT('Ctrl Pts',(-16.6108906364366,-18.9253192593608,
4.08888643334251));
#161414=CARTESIAN_POINT('Ctrl Pts',(-16.6151425729429,-19.088968908908,
4.09750876911649));
#161415=CARTESIAN_POINT('Ctrl Pts',(-16.6546491864938,-19.3663365232059,
4.1128457270043));
#161416=CARTESIAN_POINT('Ctrl Pts',(-16.6807143096475,-19.4805708641486,
4.11937599655691));
#161417=CARTESIAN_POINT('Ctrl Pts',(-16.7203982244778,-19.6056827593115,
4.12706531716991));
#161418=CARTESIAN_POINT('Ctrl Pts',(-16.7248570590233,-19.6192614839888,
4.1279069449177));
#161419=CARTESIAN_POINT('Ctrl Pts',(-16.7321720536246,-19.6407999457756,
4.12925368066921));
#161420=CARTESIAN_POINT('Ctrl Pts',(-16.7349390562625,-19.6487896614111,
4.12975584639551));
#161421=CARTESIAN_POINT('Ctrl Pts',(-16.7399033693759,-19.6628511234073,
4.13064429971968));
#161422=CARTESIAN_POINT('Ctrl Pts',(-16.7420807467644,-19.6689298285605,
4.13102992109362));
#161423=CARTESIAN_POINT('Ctrl Pts',(-16.7466416666493,-19.6814816217122,
4.13182942873961));
#161424=CARTESIAN_POINT('Ctrl Pts',(-16.7490291032123,-19.6879532041565,
4.13224344127172));
#161425=CARTESIAN_POINT('Ctrl Pts',(-16.7552383172479,-19.7045343927794,
4.13330887419664));
#161426=CARTESIAN_POINT('Ctrl Pts',(-16.7591059275504,-19.7146265175454,
4.13396182366307));
#161427=CARTESIAN_POINT('Ctrl Pts',(-16.7755692399774,-19.7566206178897,
4.13669782121422));
#161428=CARTESIAN_POINT('Ctrl Pts',(-16.7888614373468,-19.7882422713803,
4.13880419929231));
#161429=CARTESIAN_POINT('Ctrl Pts',(-16.8254906767519,-19.8697777962227,
4.14436015730516));
#161430=CARTESIAN_POINT('Ctrl Pts',(-16.8500172953326,-19.9191257769245,
4.1478481481997));
#161431=CARTESIAN_POINT('Ctrl Pts',(-16.9289062920239,-20.0634361660146,
4.15841942326031));
#161432=CARTESIAN_POINT('Ctrl Pts',(-16.9887300524645,-20.1551969870905,
4.16565109249587));
#161433=CARTESIAN_POINT('Ctrl Pts',(-17.0840670701738,-20.2792635926364,
4.17598684778336));
#161434=CARTESIAN_POINT('Ctrl Pts',(-17.1140041876896,-20.3156425847411,
4.17909212856166));
#161435=CARTESIAN_POINT('Ctrl Pts',(-17.1581979842347,-20.3658345106149,
4.18345759856539));
#161436=CARTESIAN_POINT('Ctrl Pts',(-17.1714730647769,-20.3804920815762,
4.18474276004411));
#161437=CARTESIAN_POINT('Ctrl Pts',(-17.220851665177,-20.4335009897875,
4.18942272787567));
#161438=CARTESIAN_POINT('Ctrl Pts',(-17.2581806269553,-20.4706906354358,
4.19276953974709));
#161439=CARTESIAN_POINT('Ctrl Pts',(-17.3032424571743,-20.5123516845133,
4.19655506074864));
#161440=CARTESIAN_POINT('Ctrl Pts',(-17.3096600739558,-20.5182120886848,
4.19708843796626));
#161441=CARTESIAN_POINT('Ctrl Pts',(-17.3194380961194,-20.5270313209435,
4.1978921904044));
#161442=CARTESIAN_POINT('Ctrl Pts',(-17.3227720078672,-20.5300192004333,
4.19816468538043));
#161443=CARTESIAN_POINT('Ctrl Pts',(-17.3287766645609,-20.5353663745537,
4.198652650921));
#161444=CARTESIAN_POINT('Ctrl Pts',(-17.3314438983081,-20.5377295105773,
4.19886840743268));
#161445=CARTESIAN_POINT('Ctrl Pts',(-17.3372563150521,-20.5428531013295,
4.19933641996592));
#161446=CARTESIAN_POINT('Ctrl Pts',(-17.340403709584,-20.5456109598914,
4.19958848321721));
#161447=CARTESIAN_POINT('Ctrl Pts',(-17.3492772959581,-20.5533399180345,
4.20029538112856));
#161448=CARTESIAN_POINT('Ctrl Pts',(-17.3550221156571,-20.5582896683398,
4.2007486585063));
#161449=CARTESIAN_POINT('Ctrl Pts',(-17.3897289212988,-20.587869707223,
4.20346178695947));
#161450=CARTESIAN_POINT('Ctrl Pts',(-17.4193254743493,-20.6117486944671,
4.20567016992761));
#161451=CARTESIAN_POINT('Ctrl Pts',(-17.5193335035214,-20.6880820297534,
4.21285180062573));
#161452=CARTESIAN_POINT('Ctrl Pts',(-17.5923671122747,-20.7369572272965,
4.21765604623029));
#161453=CARTESIAN_POINT('Ctrl Pts',(-17.8188876546578,-20.8689407396943,
4.2319182372502));
#161454=CARTESIAN_POINT('Ctrl Pts',(-17.9797938389152,-20.9377640143448,
4.24129778576002));
#161455=CARTESIAN_POINT('Ctrl Pts',(-18.1694807681475,-20.9924752892524,
4.25276860950246));
#161456=CARTESIAN_POINT('Ctrl Pts',(-18.191752541717,-20.9985065359321,
4.25412028802448));
#161457=CARTESIAN_POINT('Ctrl Pts',(-18.2233847235402,-21.0065199989763,
4.25604865524583));
#161458=CARTESIAN_POINT('Ctrl Pts',(-18.2326673031133,-21.0088047815055,
4.2566155779612));
#161459=CARTESIAN_POINT('Ctrl Pts',(-18.247770759272,-21.0124139773417,
4.25753980385405));
#161460=CARTESIAN_POINT('Ctrl Pts',(-18.2535823891813,-21.0137767945768,
4.2578958661323));
#161461=CARTESIAN_POINT('Ctrl Pts',(-18.2657561712153,-21.0165772594493,
4.25864265464775));
#161462=CARTESIAN_POINT('Ctrl Pts',(-18.2721193505151,-21.0180101179771,
4.25903353051147));
#161463=CARTESIAN_POINT('Ctrl Pts',(-18.2872668470791,-21.0213475496345,
4.2599653186582));
#161464=CARTESIAN_POINT('Ctrl Pts',(-18.2960568191622,-21.0232256172517,
4.260507074363));
#161465=CARTESIAN_POINT('Ctrl Pts',(-18.3256818941194,-21.0293583044502,
4.26233663142532));
#161466=CARTESIAN_POINT('Ctrl Pts',(-18.3465685511101,-21.0333548523242,
4.26363262975263));
#161467=CARTESIAN_POINT('Ctrl Pts',(-18.5180610329841,-21.0634982453379,
4.27432675358716));
#161468=CARTESIAN_POINT('Ctrl Pts',(-18.671006367347,-21.0735725529928,
4.28424846201762));
#161469=CARTESIAN_POINT('Ctrl Pts',(-18.8986403735704,-21.0639215443319,
4.29928955277329));
#161470=CARTESIAN_POINT('Ctrl Pts',(-18.9733859392728,-21.0567598033286,
4.30426333563097));
#161471=CARTESIAN_POINT('Ctrl Pts',(-19.0689464494272,-21.042446366361,
4.31057340736452));
#161472=CARTESIAN_POINT('Ctrl Pts',(-19.0902487570828,-21.038921656892,
4.31197670313412));
#161473=CARTESIAN_POINT('Ctrl Pts',(-19.1624906348318,-21.0258299955245,
4.31671694991476));
#161474=CARTESIAN_POINT('Ctrl Pts',(-19.2131355584661,-21.0147179039281,
4.32000857355429));
#161475=CARTESIAN_POINT('Ctrl Pts',(-19.2717049571741,-20.9995930439963,
4.3237396361131));
#161476=CARTESIAN_POINT('Ctrl Pts',(-19.2800710662406,-20.9973777869312,
4.32427075368187));
#161477=CARTESIAN_POINT('Ctrl Pts',(-19.2927365011485,-20.9939408644478,
4.32507178270113));
#161478=CARTESIAN_POINT('Ctrl Pts',(-19.2970458135304,-20.9927568165587,
4.32534379289797));
#161479=CARTESIAN_POINT('Ctrl Pts',(-19.3047840644833,-20.9906042398618,
4.32583124232455));
#161480=CARTESIAN_POINT('Ctrl Pts',(-19.3082143191658,-20.9896406972988,
4.32604696479259));
#161481=CARTESIAN_POINT('Ctrl Pts',(-19.3156739781137,-20.9875249804295,
4.32651530853815));
#161482=CARTESIAN_POINT('Ctrl Pts',(-19.3197023857499,-20.9863695039969,
4.32676773484543));
#161483=CARTESIAN_POINT('Ctrl Pts',(-19.3310372398869,-20.9830818456228,
4.3274766784815));
#161484=CARTESIAN_POINT('Ctrl Pts',(-19.3383357426789,-20.9809221876494,
4.32793162403818));
#161485=CARTESIAN_POINT('Ctrl Pts',(-19.3825006867438,-20.9675941334572,
4.33067612958164));
#161486=CARTESIAN_POINT('Ctrl Pts',(-19.4190708346027,-20.9554598132532,
4.3329128273252));
#161487=CARTESIAN_POINT('Ctrl Pts',(-19.5397207533015,-20.9117365783304,
4.34023440044692));
#161488=CARTESIAN_POINT('Ctrl Pts',(-19.6221241974076,-20.8757960807179,
4.34514267545348));
#161489=CARTESIAN_POINT('Ctrl Pts',(-19.8194143922129,-20.7743596654897,
4.35720611269695));
#161490=CARTESIAN_POINT('Ctrl Pts',(-19.9309150909577,-20.7031455672504,
4.36432152674259));
#161491=CARTESIAN_POINT('Ctrl Pts',(-20.0786549033234,-20.5880461256331,
4.37491345477961));
#161492=CARTESIAN_POINT('Ctrl Pts',(-20.1209047998701,-20.5523868420532,
4.37809311767221));
#161493=CARTESIAN_POINT('Ctrl Pts',(-20.1705533815596,-20.5070391854187,
4.38204488634361));
#161494=CARTESIAN_POINT('Ctrl Pts',(-20.1793290715956,-20.4988860178472,
4.3827519558898));
#161495=CARTESIAN_POINT('Ctrl Pts',(-20.1937395371283,-20.4852681066787,
4.38392758240623));
#161496=CARTESIAN_POINT('Ctrl Pts',(-20.1994140270802,-20.4798456498979,
4.38439432077853));
#161497=CARTESIAN_POINT('Ctrl Pts',(-20.2096363750362,-20.4699679900609,
4.38524212799756));
#161498=CARTESIAN_POINT('Ctrl Pts',(-20.2141945581368,-20.4655235706366,
4.38562272430894));
#161499=CARTESIAN_POINT('Ctrl Pts',(-20.2230070130457,-20.4568531729851,
4.38636356221871));
#161500=CARTESIAN_POINT('Ctrl Pts',(-20.2272635173306,-20.4526295424922,
4.38672369852369));
#161501=CARTESIAN_POINT('Ctrl Pts',(-20.2390028832041,-20.4408814366082,
4.38772339568961));
#161502=CARTESIAN_POINT('Ctrl Pts',(-20.2464471236839,-20.4333187713544,
4.3883646522824));
#161503=CARTESIAN_POINT('Ctrl Pts',(-20.277859433537,-20.4009231134952,
4.39110220598966));
#161504=CARTESIAN_POINT('Ctrl Pts',(-20.3012740847431,-20.3755630869155,
4.39322224941792));
#161505=CARTESIAN_POINT('Ctrl Pts',(-20.3609390066158,-20.3076840678458,
4.3988413133372));
#161506=CARTESIAN_POINT('Ctrl Pts',(-20.3961425504659,-20.2642846916682,
4.40238019096822));
#161507=CARTESIAN_POINT('Ctrl Pts',(-20.4700011956537,-20.1654846202707,
4.41031397141715));
#161508=CARTESIAN_POINT('Ctrl Pts',(-20.5078047722082,-20.1095235261941,
4.41472963716753));
#161509=CARTESIAN_POINT('Ctrl Pts',(-20.6208277875352,-19.9236411078564,
4.42906585649656));
#161510=CARTESIAN_POINT('Ctrl Pts',(-20.6849387302686,-19.7874937439154,
4.43910103211185));
#161511=CARTESIAN_POINT('Ctrl Pts',(-20.7392626760684,-19.6308647095153,
4.44944310789046));
#161512=CARTESIAN_POINT('Ctrl Pts',(-20.7442442921562,-19.6159680813706,
4.45041491264633));
#161513=CARTESIAN_POINT('Ctrl Pts',(-20.7508357270801,-19.5955030738574,
4.45173255597078));
#161514=CARTESIAN_POINT('Ctrl Pts',(-20.7525890218951,-19.5899819108629,
4.45208631193859));
#161515=CARTESIAN_POINT('Ctrl Pts',(-20.7553388603962,-19.5811977830754,
4.45264631902943));
#161516=CARTESIAN_POINT('Ctrl Pts',(-20.7563502019316,-19.5779395337446,
4.45285342558835));
#161517=CARTESIAN_POINT('Ctrl Pts',(-20.7584224470292,-19.5712059103387,
4.4532801523043));
#161518=CARTESIAN_POINT('Ctrl Pts',(-20.7594822797561,-19.5677302477369,
4.45349970374035));
#161519=CARTESIAN_POINT('Ctrl Pts',(-20.7619859826601,-19.5594430748376,
4.45402153234239));
#161520=CARTESIAN_POINT('Ctrl Pts',(-20.763421696862,-19.5546290837025,
4.45432333355589));
#161521=CARTESIAN_POINT('Ctrl Pts',(-20.7682044078215,-19.5383815760942,
4.45533760250583));
#161522=CARTESIAN_POINT('Ctrl Pts',(-20.7714720955077,-19.5269246909914,
4.45604559944944));
#161523=CARTESIAN_POINT('Ctrl Pts',(-20.8080701392433,-19.3943755823844,
4.46416013233734));
#161524=CARTESIAN_POINT('Ctrl Pts',(-20.8306623676895,-19.2705577245453,
4.47101316477815));
#161525=CARTESIAN_POINT('Ctrl Pts',(-20.8479900579051,-19.0817297789905,
4.48131925557765));
#161526=CARTESIAN_POINT('Ctrl Pts',(-20.8509451663437,-19.0177762435095,
4.48478351540402));
#161527=CARTESIAN_POINT('Ctrl Pts',(-20.8509992439666,-18.9537891464354,
4.48828857340046));
#161528=CARTESIAN_POINT('Ctrl Pts',(-20.850999245597,-18.9537872161824,
4.48828867913505));
#161529=CARTESIAN_POINT('Ctrl Pts',(-20.8510695256919,-18.8705388048596,
4.49284882620142));
#161530=CARTESIAN_POINT('Ctrl Pts',(-20.8462293926872,-18.7873633754263,
4.49747288514878));
#161531=CARTESIAN_POINT('Ctrl Pts',(-20.8325134503724,-18.6707567027903,
4.50419748944219));
#161532=CARTESIAN_POINT('Ctrl Pts',(-20.8277010638379,-18.636925153178,
4.50617704217313));
#161533=CARTESIAN_POINT('Ctrl Pts',(-20.8203844097302,-18.5931211120813,
4.50878341840881));
#161534=CARTESIAN_POINT('Ctrl Pts',(-20.8186232354125,-18.5830285617623,
4.50938693124433));
#161535=CARTESIAN_POINT('Ctrl Pts',(-20.8155220318927,-18.5659882221832,
4.51041115234559));
#161536=CARTESIAN_POINT('Ctrl Pts',(-20.8142202897792,-18.5590335815711,
4.51083064729524));
#161537=CARTESIAN_POINT('Ctrl Pts',(-20.8115755323949,-18.5452852796706,
4.51166292069851));
#161538=CARTESIAN_POINT('Ctrl Pts',(-20.8102339970038,-18.5384914215251,
4.51207564743034));
#161539=CARTESIAN_POINT('Ctrl Pts',(-20.8075793318785,-18.5253862276186,
4.51287464056693));
#161540=CARTESIAN_POINT('Ctrl Pts',(-20.8062706592279,-18.5190740596167,
4.51326076035452));
#161541=CARTESIAN_POINT('Ctrl Pts',(-20.8031923985453,-18.5045603800297,
4.51415156749671));
#161542=CARTESIAN_POINT('Ctrl Pts',(-20.8014028510898,-18.4963632544922,
4.51465688989135));
#161543=CARTESIAN_POINT('Ctrl Pts',(-20.7964824170247,-18.4744508519889,
4.51601371912014));
#161544=CARTESIAN_POINT('Ctrl Pts',(-20.7932635065878,-18.4607559621306,
4.51686803926679));
#161545=CARTESIAN_POINT('Ctrl Pts',(-20.7715055583977,-18.3721604885119,
4.52243681453723));
#161546=CARTESIAN_POINT('Ctrl Pts',(-20.7490266170535,-18.2983167241065,
4.52727678947559));
#161547=CARTESIAN_POINT('Ctrl Pts',(-20.7225805465488,-18.2258895332749,
4.53222344315201));
#161548=CARTESIAN_POINT('Origin',(-18.734,-18.952,0.));
#161549=CARTESIAN_POINT('',(-20.7225805962997,-18.2258896695266,5.55626859415409));
#161550=CARTESIAN_POINT('',(-20.7225805585332,-18.2258895660964,5.33540095489714));
#161551=CARTESIAN_POINT('',(-20.7225805737622,-18.2258896078036,0.));
#161552=CARTESIAN_POINT('Ctrl Pts',(-20.7225805962997,-18.2258896695266,
5.55626859415409));
#161553=CARTESIAN_POINT('Ctrl Pts',(-20.7320990939749,-18.2519577462201,
5.55474542935323));
#161554=CARTESIAN_POINT('Ctrl Pts',(-20.7411068523736,-18.2782180382529,
5.55321409559504));
#161555=CARTESIAN_POINT('Ctrl Pts',(-20.7754133681831,-18.385036223238,
5.54697995143813));
#161556=CARTESIAN_POINT('Ctrl Pts',(-20.7963949754118,-18.4668804316982,
5.54218754382626));
#161557=CARTESIAN_POINT('Ctrl Pts',(-20.8151326641375,-18.5636990555802,
5.53639859959952));
#161558=CARTESIAN_POINT('Ctrl Pts',(-20.817691286621,-18.5776720735792,
5.53556038790442));
#161559=CARTESIAN_POINT('Ctrl Pts',(-20.8214097414357,-18.599199818088,
5.5342643715788));
#161560=CARTESIAN_POINT('Ctrl Pts',(-20.8226696399543,-18.6067370135883,
5.53380975054751));
#161561=CARTESIAN_POINT('Ctrl Pts',(-20.8248931361726,-18.6204965495217,
5.53297817438786));
#161562=CARTESIAN_POINT('Ctrl Pts',(-20.8258698386648,-18.6267167060361,
5.53260164016139));
#161563=CARTESIAN_POINT('Ctrl Pts',(-20.8279419770428,-18.6403085844017,
5.53177749068674));
#161564=CARTESIAN_POINT('Ctrl Pts',(-20.8290262605791,-18.6476818982542,
5.53132952710003));
#161565=CARTESIAN_POINT('Ctrl Pts',(-20.8318905539539,-18.6679007246484,
5.53009865754964));
#161566=CARTESIAN_POINT('Ctrl Pts',(-20.8335914771489,-18.680756950372,
5.52931326311956));
#161567=CARTESIAN_POINT('Ctrl Pts',(-20.8416314800243,-18.7461410913131,
5.52530442004773));
#161568=CARTESIAN_POINT('Ctrl Pts',(-20.8461174153946,-18.7988739479112,
5.52202314179027));
#161569=CARTESIAN_POINT('Ctrl Pts',(-20.8502336388908,-18.8856700870332,
5.51653987840504));
#161570=CARTESIAN_POINT('Ctrl Pts',(-20.8510257893312,-18.9196565836178,
5.51437232070036));
#161571=CARTESIAN_POINT('Ctrl Pts',(-20.8508977918913,-19.0842687682467,
5.50378110567431));
#161572=CARTESIAN_POINT('Ctrl Pts',(-20.8387067138667,-19.2145945166531,
5.49508956453502));
#161573=CARTESIAN_POINT('Ctrl Pts',(-20.7970384706232,-19.4363469421699,
5.48023965567002));
#161574=CARTESIAN_POINT('Ctrl Pts',(-20.7732180764462,-19.5284664748066,
5.4740598682392));
#161575=CARTESIAN_POINT('Ctrl Pts',(-20.7402342465002,-19.627874953247,
5.46758880239061));
#161576=CARTESIAN_POINT('Ctrl Pts',(-20.7371210646396,-19.6370465771283,
5.46699371560475));
#161577=CARTESIAN_POINT('Ctrl Pts',(-20.7324307946542,-19.65055900348,5.46612020156299));
#161578=CARTESIAN_POINT('Ctrl Pts',(-20.73090232296,-19.6549163789916,5.46583901464156));
#161579=CARTESIAN_POINT('Ctrl Pts',(-20.7281650633119,-19.6626387860193,
5.46534160466696));
#161580=CARTESIAN_POINT('Ctrl Pts',(-20.7269619965802,-19.6660057876478,
5.4651250473556));
#161581=CARTESIAN_POINT('Ctrl Pts',(-20.7243657194792,-19.6732142537527,
5.46466210288583));
#161582=CARTESIAN_POINT('Ctrl Pts',(-20.7229699196435,-19.6770547265529,
5.46441587234752));
#161583=CARTESIAN_POINT('Ctrl Pts',(-20.7191070461289,-19.6875881295587,
5.46374160139872));
#161584=CARTESIAN_POINT('Ctrl Pts',(-20.7166172253563,-19.6942727409491,
5.46331489543619));
#161585=CARTESIAN_POINT('Ctrl Pts',(-20.7031297619653,-19.7299314999597,
5.46104439826444));
#161586=CARTESIAN_POINT('Ctrl Pts',(-20.6915300523097,-19.7586757470262,
5.45923449245834));
#161587=CARTESIAN_POINT('Ctrl Pts',(-20.6147736122224,-19.9374619914397,
5.44804390875201));
#161588=CARTESIAN_POINT('Ctrl Pts',(-20.5330352574374,-20.0797983909561,
5.43939877325784));
#161589=CARTESIAN_POINT('Ctrl Pts',(-20.3657124170988,-20.3059019476789,
5.42400426268554));
#161590=CARTESIAN_POINT('Ctrl Pts',(-20.2879589804636,-20.3944777437368,
5.4174378463749));
#161591=CARTESIAN_POINT('Ctrl Pts',(-20.1929613257168,-20.4860551997828,
5.40970784017757));
#161592=CARTESIAN_POINT('Ctrl Pts',(-20.1825655589441,-20.4958754199795,
5.40886571333382));
#161593=CARTESIAN_POINT('Ctrl Pts',(-20.1658644144752,-20.5113347404798,
5.40751832816367));
#161594=CARTESIAN_POINT('Ctrl Pts',(-20.1596232407252,-20.517042781091,
5.40701601660862));
#161595=CARTESIAN_POINT('Ctrl Pts',(-20.1485570617929,-20.5270425442269,
5.40612739340277));
#161596=CARTESIAN_POINT('Ctrl Pts',(-20.1437462841084,-20.5313499011332,
5.40574174879371));
#161597=CARTESIAN_POINT('Ctrl Pts',(-20.1337566254966,-20.5402121889069,
5.40494227948084));
#161598=CARTESIAN_POINT('Ctrl Pts',(-20.1285750471709,-20.5447639510207,
5.40452832894341));
#161599=CARTESIAN_POINT('Ctrl Pts',(-20.1152202524201,-20.5563803552348,
5.40346323768274));
#161600=CARTESIAN_POINT('Ctrl Pts',(-20.1070151075129,-20.5634078371799,
5.40281056977836));
#161601=CARTESIAN_POINT('Ctrl Pts',(-20.072567336689,-20.5924572900762,
5.40007729926763));
#161602=CARTESIAN_POINT('Ctrl Pts',(-20.045847087181,-20.6139024158623,
5.39797342479381));
#161603=CARTESIAN_POINT('Ctrl Pts',(-19.9749016419944,-20.6680644784892,
5.3924256423955));
#161604=CARTESIAN_POINT('Ctrl Pts',(-19.9299030056876,-20.6997211916748,
5.38894346429663));
#161605=CARTESIAN_POINT('Ctrl Pts',(-19.8068133684807,-20.7793343126961,
5.37952170024796));
#161606=CARTESIAN_POINT('Ctrl Pts',(-19.7267586041929,-20.8240329402428,
5.37349494489065));
#161607=CARTESIAN_POINT('Ctrl Pts',(-19.5956096943228,-20.8864762017771,
5.36389726998934));
#161608=CARTESIAN_POINT('Ctrl Pts',(-19.5462916510206,-20.9076972876215,
5.3603473547928));
#161609=CARTESIAN_POINT('Ctrl Pts',(-19.46184805834,-20.9402865963154,5.3544124441374));
#161610=CARTESIAN_POINT('Ctrl Pts',(-19.4271344415691,-20.9526527033317,
5.35201230835054));
#161611=CARTESIAN_POINT('Ctrl Pts',(-19.3471261965966,-20.9788215852332,
5.34659427775521));
#161612=CARTESIAN_POINT('Ctrl Pts',(-19.3016530781386,-20.9920245603641,
5.3435963624006));
#161613=CARTESIAN_POINT('Ctrl Pts',(-19.2483054253403,-21.0055915572527,
5.3402024991186));
#161614=CARTESIAN_POINT('Ctrl Pts',(-19.2408284606263,-21.0074496515824,
5.33972961739137));
#161615=CARTESIAN_POINT('Ctrl Pts',(-19.2288403586848,-21.0103594127946,
5.33897606882577));
#161616=CARTESIAN_POINT('Ctrl Pts',(-19.2243357048836,-21.0114371440469,
5.3386939612166));
#161617=CARTESIAN_POINT('Ctrl Pts',(-19.2163370376984,-21.0133230806223,
5.33819493760871));
#161618=CARTESIAN_POINT('Ctrl Pts',(-19.2128444657841,-21.014137201778,
5.33797768473212));
#161619=CARTESIAN_POINT('Ctrl Pts',(-19.2054215107038,-21.015847622707,
5.33751732307798));
#161620=CARTESIAN_POINT('Ctrl Pts',(-19.2014906401088,-21.0167415704012,
5.33727434989112));
#161621=CARTESIAN_POINT('Ctrl Pts',(-19.1908396926436,-21.0191318034293,
5.33661814244093));
#161622=CARTESIAN_POINT('Ctrl Pts',(-19.1841147638346,-21.0206065599516,
5.33620612582413));
#161623=CARTESIAN_POINT('Ctrl Pts',(-19.1502495377332,-21.0278601358075,
5.33414235463855));
#161624=CARTESIAN_POINT('Ctrl Pts',(-19.1230032941099,-21.0331380505443,
5.33251759368829));
#161625=CARTESIAN_POINT('Ctrl Pts',(-19.0432774335999,-21.0469613027593,
5.32784622894791));
#161626=CARTESIAN_POINT('Ctrl Pts',(-18.9905679072737,-21.0540678087979,
5.32486157307193));
#161627=CARTESIAN_POINT('Ctrl Pts',(-18.7975190746788,-21.0727245317466,
5.31413089258638));
#161628=CARTESIAN_POINT('Ctrl Pts',(-18.6563924159986,-21.0722562367394,
5.30664728833413));
#161629=CARTESIAN_POINT('Ctrl Pts',(-18.4249583140915,-21.0483359736485,
5.29377739315979));
#161630=CARTESIAN_POINT('Ctrl Pts',(-18.3342855036138,-21.0329508897311,
5.28858530666603));
#161631=CARTESIAN_POINT('Ctrl Pts',(-18.231513554845,-21.0085470628715,
5.28239285691151));
#161632=CARTESIAN_POINT('Ctrl Pts',(-18.218153439244,-21.005236655084,5.28158189924194));
#161633=CARTESIAN_POINT('Ctrl Pts',(-18.1967890293315,-20.9997212418233,
5.28027512348966));
#161634=CARTESIAN_POINT('Ctrl Pts',(-18.1887636370328,-20.9975989872708,
5.27978197769535));
#161635=CARTESIAN_POINT('Ctrl Pts',(-18.1745419070837,-20.9937485206113,
5.27890396997101));
#161636=CARTESIAN_POINT('Ctrl Pts',(-18.168340541722,-20.9920391552611,
5.2785197239155));
#161637=CARTESIAN_POINT('Ctrl Pts',(-18.1554415226266,-20.9884202887534,
5.27771753767462));
#161638=CARTESIAN_POINT('Ctrl Pts',(-18.1487453172299,-20.9865059495316,
5.27729944381542));
#161639=CARTESIAN_POINT('Ctrl Pts',(-18.1313918791334,-20.9814521144882,
5.2762115710938));
#161640=CARTESIAN_POINT('Ctrl Pts',(-18.1207497996914,-20.9782617345215,
5.27554013706721));
#161641=CARTESIAN_POINT('Ctrl Pts',(-18.0747523316687,-20.9640766363893,
5.27261908344881));
#161642=CARTESIAN_POINT('Ctrl Pts',(-18.0396654119785,-20.952239757448,
5.27034200643461));
#161643=CARTESIAN_POINT('Ctrl Pts',(-17.9473895480668,-20.9183892430523,
5.26421874866686));
#161644=CARTESIAN_POINT('Ctrl Pts',(-17.8908183251948,-20.8948037004754,
5.26032365529616));
#161645=CARTESIAN_POINT('Ctrl Pts',(-17.6944466185338,-20.8027394395837,
5.2463168607768));
#161646=CARTESIAN_POINT('Ctrl Pts',(-17.5612676906098,-20.7213503680756,
5.23587293866638));
#161647=CARTESIAN_POINT('Ctrl Pts',(-17.4256023732808,-20.6163434452836,
5.22471978443441));
#161648=CARTESIAN_POINT('Ctrl Pts',(-17.4130984808814,-20.6064372608426,
5.22368701034349));
#161649=CARTESIAN_POINT('Ctrl Pts',(-17.3725517901845,-20.5735614945797,
5.22032500008119));
#161650=CARTESIAN_POINT('Ctrl Pts',(-17.3449852768872,-20.5500116787952,
5.21801848939177));
#161651=CARTESIAN_POINT('Ctrl Pts',(-17.305541829119,-20.5145231864353,
5.21470356088933));
#161652=CARTESIAN_POINT('Ctrl Pts',(-17.2931819286684,-20.5031333856305,
5.21366261490008));
#161653=CARTESIAN_POINT('Ctrl Pts',(-17.2766273317193,-20.4875094837152,
5.21226699678137));
#161654=CARTESIAN_POINT('Ctrl Pts',(-17.2723133256403,-20.4834034533058,
5.21190317838199));
#161655=CARTESIAN_POINT('Ctrl Pts',(-17.2655322335265,-20.476894513707,
5.21133117764928));
#161656=CARTESIAN_POINT('Ctrl Pts',(-17.2630536237669,-20.474503733245,
5.21112207515763));
#161657=CARTESIAN_POINT('Ctrl Pts',(-17.2579847596926,-20.4695905514969,
5.21069441932304));
#161658=CARTESIAN_POINT('Ctrl Pts',(-17.2553951358538,-20.4670675653159,
5.2104759211946));
#161659=CARTESIAN_POINT('Ctrl Pts',(-17.2493007956321,-20.4610995406159,
5.20996165229366));
#161660=CARTESIAN_POINT('Ctrl Pts',(-17.2458015641383,-20.4576488858785,
5.20966632019869));
#161661=CARTESIAN_POINT('Ctrl Pts',(-17.2343063843572,-20.4462340581502,
5.20869583950129));
#161662=CARTESIAN_POINT('Ctrl Pts',(-17.2263619453711,-20.4382179753091,
5.20802465250578));
#161663=CARTESIAN_POINT('Ctrl Pts',(-17.2076029501314,-20.4189845964016,
5.20643751193313));
#161664=CARTESIAN_POINT('Ctrl Pts',(-17.1968472436489,-20.4077105457049,
5.20552566059723));
#161665=CARTESIAN_POINT('Ctrl Pts',(-17.1579279519793,-20.3660032398131,
5.2022147269221));
#161666=CARTESIAN_POINT('Ctrl Pts',(-17.1305342343258,-20.3348616038547,
5.19986187949899));
#161667=CARTESIAN_POINT('Ctrl Pts',(-17.0382569739199,-20.2235272329372,
5.1917747795191));
#161668=CARTESIAN_POINT('Ctrl Pts',(-16.9783299183852,-20.1394134549622,
5.18622093521156));
#161669=CARTESIAN_POINT('Ctrl Pts',(-16.8492616557765,-19.9269855375339,
5.17270455541167));
#161670=CARTESIAN_POINT('Ctrl Pts',(-16.7867686653616,-19.7952779304493,
5.16470175202433));
#161671=CARTESIAN_POINT('Ctrl Pts',(-16.7335073509736,-19.6447638562186,
5.15534808615831));
#161672=CARTESIAN_POINT('Ctrl Pts',(-16.7288835867194,-19.6312648626565,
5.15450780240407));
#161673=CARTESIAN_POINT('Ctrl Pts',(-16.7217399386323,-19.6097004061198,
5.15316281559621));
#161674=CARTESIAN_POINT('Ctrl Pts',(-16.7191312221228,-19.6016646700917,
5.15266104273462));
#161675=CARTESIAN_POINT('Ctrl Pts',(-16.7146140928229,-19.5874614351978,
5.15177304694336));
#161676=CARTESIAN_POINT('Ctrl Pts',(-16.7126856497075,-19.5813003842409,
5.15138748803535));
#161677=CARTESIAN_POINT('Ctrl Pts',(-16.7087542489773,-19.5685356982459,
5.15058787643289));
#161678=CARTESIAN_POINT('Ctrl Pts',(-16.706755340773,-19.5619309052087,
5.15017369632704));
#161679=CARTESIAN_POINT('Ctrl Pts',(-16.7017051435544,-19.5449449342119,
5.14910733993762));
#161680=CARTESIAN_POINT('Ctrl Pts',(-16.6987011153821,-19.5345500167439,
5.14845362946145));
#161681=CARTESIAN_POINT('Ctrl Pts',(-16.6864782806407,-19.4910061595938,
5.14571024768578));
#161682=CARTESIAN_POINT('Ctrl Pts',(-16.6779890411347,-19.4576595199721,
5.1435970886076));
#161683=CARTESIAN_POINT('Ctrl Pts',(-16.6579770921975,-19.3701857256668,
5.138018966348));
#161684=CARTESIAN_POINT('Ctrl Pts',(-16.6477578552025,-19.3157901837531,
5.13451520904312));
#161685=CARTESIAN_POINT('Ctrl Pts',(-16.6236834456273,-19.1526521921083,
5.12391366090748));
#161686=CARTESIAN_POINT('Ctrl Pts',(-16.6161281154048,-19.0431728121681,
5.11666758811027));
#161687=CARTESIAN_POINT('Ctrl Pts',(-16.6176040924039,-18.8732644851859,
5.10544395485926));
#161688=CARTESIAN_POINT('Ctrl Pts',(-16.6207084800713,-18.8129661559535,
5.10146795922218));
#161689=CARTESIAN_POINT('Ctrl Pts',(-16.631866298205,-18.6948640367435,
5.09377757539713));
#161690=CARTESIAN_POINT('Ctrl Pts',(-16.639741305982,-18.6370923399227,
5.09006219147965));
#161691=CARTESIAN_POINT('Ctrl Pts',(-16.6515574770134,-18.5709469105798,
5.08591579450477));
#161692=CARTESIAN_POINT('Ctrl Pts',(-16.6531790026899,-18.5621894023436,
5.08536902531434));
#161693=CARTESIAN_POINT('Ctrl Pts',(-16.6557073108253,-18.5490000545843,
5.08454915366039));
#161694=CARTESIAN_POINT('Ctrl Pts',(-16.656573085641,-18.544560588238,5.08427380500038));
#161695=CARTESIAN_POINT('Ctrl Pts',(-16.6581470321114,-18.5366252563615,
5.08378277694119));
#161696=CARTESIAN_POINT('Ctrl Pts',(-16.6588498142237,-18.5331283859793,
5.08356679568525));
#161697=CARTESIAN_POINT('Ctrl Pts',(-16.6603894328382,-18.5255666069461,
5.0831006217891));
#161698=CARTESIAN_POINT('Ctrl Pts',(-16.6612293827033,-18.5215023905906,
5.0828506093918));
#161699=CARTESIAN_POINT('Ctrl Pts',(-16.6636051997308,-18.5101748250063,
5.08215523248421));
#161700=CARTESIAN_POINT('Ctrl Pts',(-16.6651673473983,-18.5029169637195,
5.08171134480171));
#161701=CARTESIAN_POINT('Ctrl Pts',(-16.6743850952166,-18.4611596486151,
5.07916626318092));
#161702=CARTESIAN_POINT('Ctrl Pts',(-16.6828658790819,-18.4268457799038,
5.07710940487219));
#161703=CARTESIAN_POINT('Ctrl Pts',(-16.7127046556053,-18.3179041069915,
5.07064362912736));
#161704=CARTESIAN_POINT('Ctrl Pts',(-16.7373094376311,-18.2442280455371,
5.06636752551238));
#161705=CARTESIAN_POINT('Ctrl Pts',(-16.8357150806297,-17.9959106470385,
5.05179380847907));
#161706=CARTESIAN_POINT('Ctrl Pts',(-16.9288462779434,-17.8299452343977,
5.04167931543869));
#161707=CARTESIAN_POINT('Ctrl Pts',(-17.055864877666,-17.6612551605165,
5.02939282215334));
#161708=CARTESIAN_POINT('Ctrl Pts',(-17.0691808837866,-17.6441250104138,
5.02812061338992));
#161709=CARTESIAN_POINT('Ctrl Pts',(-17.0880100217009,-17.6206561519008,
5.02634178905651));
#161710=CARTESIAN_POINT('Ctrl Pts',(-17.09330140717,-17.6141406744599,5.02584403293302));
#161711=CARTESIAN_POINT('Ctrl Pts',(-17.1024800924234,-17.6029749725938,
5.02498415881919));
#161712=CARTESIAN_POINT('Ctrl Pts',(-17.106348899909,-17.5983096260279,
5.02462279199697));
#161713=CARTESIAN_POINT('Ctrl Pts',(-17.1143816338957,-17.5887072727857,
5.02387465494208));
#161714=CARTESIAN_POINT('Ctrl Pts',(-17.1185482215765,-17.5837725839421,
5.02348777801813));
#161715=CARTESIAN_POINT('Ctrl Pts',(-17.1283239173964,-17.5723016628018,
5.02258278396236));
#161716=CARTESIAN_POINT('Ctrl Pts',(-17.1339504336124,-17.5657804771283,
5.02206395131675));
#161717=CARTESIAN_POINT('Ctrl Pts',(-17.1522004083113,-17.5448877290204,
5.02038750539962));
#161718=CARTESIAN_POINT('Ctrl Pts',(-17.1649786280055,-17.5306531781655,
5.0192234514144));
#161719=CARTESIAN_POINT('Ctrl Pts',(-17.230447603557,-17.4596815094645,
5.01330633636717));
#161720=CARTESIAN_POINT('Ctrl Pts',(-17.2860244426002,-17.405698372404,
5.00843008756804));
#161721=CARTESIAN_POINT('Ctrl Pts',(-17.4460897109082,-17.2664333449365,
4.99477785312247));
#161722=CARTESIAN_POINT('Ctrl Pts',(-17.5559601144885,-17.1878955537262,
4.98580051803567));
#161723=CARTESIAN_POINT('Ctrl Pts',(-17.7149109337702,-17.0957819939485,
4.97372323715053));
#161724=CARTESIAN_POINT('Ctrl Pts',(-17.7581287537793,-17.0727013045635,
4.97052590718076));
#161725=CARTESIAN_POINT('Ctrl Pts',(-17.8414844967424,-17.0318364595991,
4.96456640732377));
#161726=CARTESIAN_POINT('Ctrl Pts',(-17.8814523113951,-17.0137598198785,
4.96179517689643));
#161727=CARTESIAN_POINT('Ctrl Pts',(-17.9289120917072,-16.9940471921087,
4.95862781609513));
#161728=CARTESIAN_POINT('Ctrl Pts',(-17.9358838622746,-16.9911949682367,
4.95816560378432));
#161729=CARTESIAN_POINT('Ctrl Pts',(-17.947165780133,-16.9866495601573,
4.95742275633351));
#161730=CARTESIAN_POINT('Ctrl Pts',(-17.9514664473751,-16.9849332291708,
4.95714077791609));
#161731=CARTESIAN_POINT('Ctrl Pts',(-17.9590991312861,-16.9819161344486,
4.95664249199223));
#161732=CARTESIAN_POINT('Ctrl Pts',(-17.9624288455908,-16.9806096916112,
4.95642584584564));
#161733=CARTESIAN_POINT('Ctrl Pts',(-17.9695621264708,-16.9778317272273,
4.9559632898184));
#161734=CARTESIAN_POINT('Ctrl Pts',(-17.9733666282959,-16.9763627594611,
4.95571753353962));
#161735=CARTESIAN_POINT('Ctrl Pts',(-17.9838031937001,-16.9723676814884,
4.95504589833326));
#161736=CARTESIAN_POINT('Ctrl Pts',(-17.9904438219302,-16.9698638851024,
4.9546213365227));
#161737=CARTESIAN_POINT('Ctrl Pts',(-18.0256827101666,-16.9567793559822,
4.95238249163214));
#161738=CARTESIAN_POINT('Ctrl Pts',(-18.0544960802675,-16.9467834424431,
4.95060098467386));
#161739=CARTESIAN_POINT('Ctrl Pts',(-18.2377752046706,-16.8876050835041,
4.93951745963536));
#161740=CARTESIAN_POINT('Ctrl Pts',(-18.3972603588826,-16.8556736823997,
4.93094268497014));
#161741=CARTESIAN_POINT('Ctrl Pts',(-18.6781020273253,-16.8323572495901,
4.91552930121469));
#161742=CARTESIAN_POINT('Ctrl Pts',(-18.7979705985112,-16.8325868265202,
4.90885800939638));
#161743=CARTESIAN_POINT('Ctrl Pts',(-18.932821038579,-16.8442984017036,
4.90092860974278));
#161744=CARTESIAN_POINT('Ctrl Pts',(-18.948457091729,-16.8458319229441,
4.90000298475811));
#161745=CARTESIAN_POINT('Ctrl Pts',(-18.9720878358004,-16.848415400701,
4.89859414442555));
#161746=CARTESIAN_POINT('Ctrl Pts',(-18.9800961951671,-16.8493372491194,
4.89811496295466));
#161747=CARTESIAN_POINT('Ctrl Pts',(-18.9944375160585,-16.8510711425286,
4.89725366733439));
#161748=CARTESIAN_POINT('Ctrl Pts',(-19.0007724680078,-16.8518661440613,
4.89687209560441));
#161749=CARTESIAN_POINT('Ctrl Pts',(-19.0142071226201,-16.8536138864864,
4.89606048385466));
#161750=CARTESIAN_POINT('Ctrl Pts',(-19.0213057664531,-16.8545740281115,
4.8956302141999));
#161751=CARTESIAN_POINT('Ctrl Pts',(-19.0402901067684,-16.8572399781245,
4.89447563006658));
#161752=CARTESIAN_POINT('Ctrl Pts',(-19.0521662611979,-16.8590108935598,
4.89374926375494));
#161753=CARTESIAN_POINT('Ctrl Pts',(-19.1099184349702,-16.8681255180905,
4.89019666408887));
#161754=CARTESIAN_POINT('Ctrl Pts',(-19.1555563695704,-16.8768765770421,
4.88732612215798));
#161755=CARTESIAN_POINT('Ctrl Pts',(-19.3657128989447,-16.9243927411314,
4.87380333280703));
#161756=CARTESIAN_POINT('Ctrl Pts',(-19.5254827714283,-16.9812665585503,
4.86258058250836));
#161757=CARTESIAN_POINT('Ctrl Pts',(-19.7656361258193,-17.1007116078515,
4.84491085389191));
#161758=CARTESIAN_POINT('Ctrl Pts',(-19.8513036570371,-17.1511171540428,
4.83844240407972));
#161759=CARTESIAN_POINT('Ctrl Pts',(-19.9411074612132,-17.2128408968588,
4.83170982320692));
#161760=CARTESIAN_POINT('Ctrl Pts',(-19.9490518323792,-17.2183818581448,
4.8311147213328));
#161761=CARTESIAN_POINT('Ctrl Pts',(-19.9607272799889,-17.2266448182095,
4.83024118945379));
#161762=CARTESIAN_POINT('Ctrl Pts',(-19.964487796717,-17.2293247241968,
4.82995999962427));
#161763=CARTESIAN_POINT('Ctrl Pts',(-19.971058383223,-17.2340396995757,
4.82946902054066));
#161764=CARTESIAN_POINT('Ctrl Pts',(-19.9738722480909,-17.2360693934808,
4.82925886674482));
#161765=CARTESIAN_POINT('Ctrl Pts',(-19.976694523198,-17.2381157208593,
4.82904819919936));
#161766=CARTESIAN_POINT('Ctrl Pts',(-19.9767078753003,-17.2381254022133,
4.82904720253976));
#161767=CARTESIAN_POINT('Ctrl Pts',(-19.9767343421635,-17.2381445933015,
4.8290452269417));
#161768=CARTESIAN_POINT('Ctrl Pts',(-19.9767474569972,-17.23815410308,4.82904424799773));
#161769=CARTESIAN_POINT('Ctrl Pts',(-19.9767734550326,-17.2381729551324,
4.82904230740449));
#161770=CARTESIAN_POINT('Ctrl Pts',(-19.9767863381139,-17.2381822973108,
4.82904134576413));
#161771=CARTESIAN_POINT('Ctrl Pts',(-19.9768118775577,-17.2382008177018,
4.82903943941112));
#161772=CARTESIAN_POINT('Ctrl Pts',(-19.9768245340366,-17.238209995991,
4.82903849468971));
#161773=CARTESIAN_POINT('Ctrl Pts',(-19.9768496251652,-17.2382281921263,
4.82903662180938));
#161774=CARTESIAN_POINT('Ctrl Pts',(-19.9768620599652,-17.238237210074,
4.82903569363918));
#161775=CARTESIAN_POINT('Ctrl Pts',(-19.9768867133356,-17.2382550895651,
4.82903385344305));
#161776=CARTESIAN_POINT('Ctrl Pts',(-19.9768989316573,-17.238263950921,
4.82903294143562));
#161777=CARTESIAN_POINT('Ctrl Pts',(-19.9769231561415,-17.2382815201594,
4.82903113326101));
#161778=CARTESIAN_POINT('Ctrl Pts',(-19.9769351624872,-17.2382902281679,
4.82903023708009));
#161779=CARTESIAN_POINT('Ctrl Pts',(-19.9769589684708,-17.2383074946448,
4.82902846015136));
#161780=CARTESIAN_POINT('Ctrl Pts',(-19.9769707678798,-17.2383160529407,
4.82902757942057));
#161781=CARTESIAN_POINT('Ctrl Pts',(-19.9769941631387,-17.2383330222566,
4.82902583315689));
#161782=CARTESIAN_POINT('Ctrl Pts',(-19.977005759516,-17.2383414336527,
4.82902496758456));
#161783=CARTESIAN_POINT('Ctrl Pts',(-19.9770287548157,-17.2383581135781,
4.82902325118198));
#161784=CARTESIAN_POINT('Ctrl Pts',(-19.977040153179,-17.2383663816956,
4.82902240039339));
#161785=CARTESIAN_POINT('Ctrl Pts',(-19.9770627555768,-17.238382777313,
4.82902071332475));
#161786=CARTESIAN_POINT('Ctrl Pts',(-19.9770739598371,-17.2383909049709,
4.82901987702778));
#161787=CARTESIAN_POINT('Ctrl Pts',(-19.9770961785962,-17.2384070229647,
4.8290182186013));
#161788=CARTESIAN_POINT('Ctrl Pts',(-19.9771071930207,-17.2384150132412,
4.82901739647727));
#161789=CARTESIAN_POINT('Ctrl Pts',(-19.9771290361249,-17.2384308593692,
4.82901576609667));
#161790=CARTESIAN_POINT('Ctrl Pts',(-19.9771398647644,-17.2384387151863,
4.82901495784305));
#161791=CARTESIAN_POINT('Ctrl Pts',(-19.9771613400607,-17.2384542951087,
4.82901335492229));
#161792=CARTESIAN_POINT('Ctrl Pts',(-19.9771719867371,-17.238462019223,
4.82901256025364));
#161793=CARTESIAN_POINT('Ctrl Pts',(-19.9771931024015,-17.23847733884,4.82901098418214));
#161794=CARTESIAN_POINT('Ctrl Pts',(-19.9772035711358,-17.2384849341536,
4.82901020279816));
#161795=CARTESIAN_POINT('Ctrl Pts',(-19.9772237352472,-17.2384995639739,
4.82900869775636));
#161796=CARTESIAN_POINT('Ctrl Pts',(-19.9772334306857,-17.2385065985044,
4.82900797409373));
#161797=CARTESIAN_POINT('Ctrl Pts',(-19.9772527849239,-17.2385206412328,
4.82900652950578));
#161798=CARTESIAN_POINT('Ctrl Pts',(-19.9772624437172,-17.2385276494251,
4.82900580858092));
#161799=CARTESIAN_POINT('Ctrl Pts',(-19.9772817254746,-17.2385416400617,
4.82900436940807));
#161800=CARTESIAN_POINT('Ctrl Pts',(-19.9772913482979,-17.2385486224031,
4.82900365117055));
#161801=CARTESIAN_POINT('Ctrl Pts',(-19.9773105568827,-17.2385625604404,
4.82900221746436));
#161802=CARTESIAN_POINT('Ctrl Pts',(-19.9773201434178,-17.2385695166971,
4.82900150193792));
#161803=CARTESIAN_POINT('Ctrl Pts',(-19.9773392810324,-17.2385834037278,
4.82900007353395));
#161804=CARTESIAN_POINT('Ctrl Pts',(-19.9773488318792,-17.2385903343322,
4.82899936067377));
#161805=CARTESIAN_POINT('Ctrl Pts',(-19.9806516390466,-17.2409870697267,
4.82875284478144));
#161806=CARTESIAN_POINT('Ctrl Pts',(-19.9839380300116,-17.2433863870169,
4.82850770451671));
#161807=CARTESIAN_POINT('Ctrl Pts',(-19.9907317717478,-17.2483764304588,
4.82800120773937));
#161808=CARTESIAN_POINT('Ctrl Pts',(-19.994238080825,-17.2509685501977,
4.82773994794951));
#161809=CARTESIAN_POINT('Ctrl Pts',(-20.0031347309729,-17.257588211032,
4.82707735269185));
#161810=CARTESIAN_POINT('Ctrl Pts',(-20.0085139694754,-17.2616306852538,
4.82667701072026));
#161811=CARTESIAN_POINT('Ctrl Pts',(-20.0239756832433,-17.2733658629342,
4.8255268345415));
#161812=CARTESIAN_POINT('Ctrl Pts',(-20.0340086051042,-17.2811237411081,
4.82478116518051));
#161813=CARTESIAN_POINT('Ctrl Pts',(-20.068204360882,-17.308059818423,4.82223963905115));
#161814=CARTESIAN_POINT('Ctrl Pts',(-20.0920183841967,-17.327676492657,
4.82046966123372));
#161815=CARTESIAN_POINT('Ctrl Pts',(-20.2108685129124,-17.4300202812137,
4.81158694628816));
#161816=CARTESIAN_POINT('Ctrl Pts',(-20.298818187395,-17.5205979337703,
4.80483692030293));
#161817=CARTESIAN_POINT('Ctrl Pts',(-20.4064864810014,-17.6533487062865,
4.79553206515607));
#161818=CARTESIAN_POINT('Ctrl Pts',(-20.4336602988542,-17.6891219737193,
4.79307711846138));
#161819=CARTESIAN_POINT('Ctrl Pts',(-20.5143634568165,-17.8026920858774,
4.78537988888213));
#161820=CARTESIAN_POINT('Ctrl Pts',(-20.5638360196076,-17.883215804101,
4.78005127147159));
#161821=CARTESIAN_POINT('Ctrl Pts',(-20.6142037020075,-17.9790075371923,
4.77370715362279));
#161822=CARTESIAN_POINT('Ctrl Pts',(-20.6205202468542,-17.9913118932795,
4.77289231173098));
#161823=CARTESIAN_POINT('Ctrl Pts',(-20.6304430559604,-18.0111163872429,
4.77158046959409));
#161824=CARTESIAN_POINT('Ctrl Pts',(-20.6341265157695,-18.0185775563508,
4.7710861751603));
#161825=CARTESIAN_POINT('Ctrl Pts',(-20.640580691291,-18.031847575125,4.77020684443803));
#161826=CARTESIAN_POINT('Ctrl Pts',(-20.6433690996284,-18.0376477388998,
4.76982243041251));
#161827=CARTESIAN_POINT('Ctrl Pts',(-20.649116064526,-18.0497429196095,
4.76902062071427));
#161828=CARTESIAN_POINT('Ctrl Pts',(-20.6520701269773,-18.0560399752663,
4.76860307497836));
#161829=CARTESIAN_POINT('Ctrl Pts',(-20.6596449323438,-18.0723960386983,
4.76751821072469));
#161830=CARTESIAN_POINT('Ctrl Pts',(-20.6642178631581,-18.08247683892,4.7668492541554));
#161831=CARTESIAN_POINT('Ctrl Pts',(-20.6835890262932,-18.1260855208706,
4.76395371378824));
#161832=CARTESIAN_POINT('Ctrl Pts',(-20.697593594552,-18.1599570527064,
4.76170026312353));
#161833=CARTESIAN_POINT('Ctrl Pts',(-20.7147526103457,-18.2047145499013,
4.7587149690439));
#161834=CARTESIAN_POINT('Ctrl Pts',(-20.7187091228593,-18.2152869608762,
4.75800926474269));
#161835=CARTESIAN_POINT('Ctrl Pts',(-20.7225805756119,-18.2258896128692,
4.75730100916854));
#161836=CARTESIAN_POINT('Ctrl Pts',(-20.7225805465488,-18.2258895332749,
4.53222344315201));
#161837=CARTESIAN_POINT('Ctrl Pts',(-20.7132341698751,-18.2002928456002,
4.53397165328878));
#161838=CARTESIAN_POINT('Ctrl Pts',(-20.7033922852884,-18.1748730681182,
4.53573282534905));
#161839=CARTESIAN_POINT('Ctrl Pts',(-20.6611690694518,-18.0717793604969,
4.54297361842479));
#161840=CARTESIAN_POINT('Ctrl Pts',(-20.6246658403405,-17.9958878264983,
4.54853816195081));
#161841=CARTESIAN_POINT('Ctrl Pts',(-20.5387822929292,-17.8415962180799,
4.56020410800601));
#161842=CARTESIAN_POINT('Ctrl Pts',(-20.4885726480977,-17.7638447041638,
4.56629230712149));
#161843=CARTESIAN_POINT('Ctrl Pts',(-20.4146871476279,-17.6643787788858,
4.57415758382117));
#161844=CARTESIAN_POINT('Ctrl Pts',(-20.3953759382021,-17.6395565026307,
4.57612685398926));
#161845=CARTESIAN_POINT('Ctrl Pts',(-20.3709929261639,-17.6096161115965,
4.57850089209391));
#161846=CARTESIAN_POINT('Ctrl Pts',(-20.3664398639034,-17.6040829260377,
4.57893957344197));
#161847=CARTESIAN_POINT('Ctrl Pts',(-20.3592417851384,-17.5954253078551,
4.57962572993124));
#161848=CARTESIAN_POINT('Ctrl Pts',(-20.3566157000718,-17.5922853071087,
4.57987454040405));
#161849=CARTESIAN_POINT('Ctrl Pts',(-20.3516794645867,-17.5864177337804,
4.58033935590371));
#161850=CARTESIAN_POINT('Ctrl Pts',(-20.3493715402575,-17.5836884261612,
4.58055551029482));
#161851=CARTESIAN_POINT('Ctrl Pts',(-20.3440734337965,-17.5774550729701,
4.58104906821316));
#161852=CARTESIAN_POINT('Ctrl Pts',(-20.3410787255451,-17.5739549392488,
4.58132613415012));
#161853=CARTESIAN_POINT('Ctrl Pts',(-20.3332092480032,-17.5648178495249,
4.58204930169394));
#161854=CARTESIAN_POINT('Ctrl Pts',(-20.3283160476508,-17.5591967542389,
4.58249407838711));
#161855=CARTESIAN_POINT('Ctrl Pts',(-20.2954625318247,-17.5218560713192,
4.58544887372895));
#161856=CARTESIAN_POINT('Ctrl Pts',(-20.2665849052554,-17.4909521077891,
4.58789516401588));
#161857=CARTESIAN_POINT('Ctrl Pts',(-20.18430508153,-17.4080249723628,4.59453070354902));
#161858=CARTESIAN_POINT('Ctrl Pts',(-20.1290503460957,-17.3579235472439,
4.59862316268444));
#161859=CARTESIAN_POINT('Ctrl Pts',(-20.0017406212783,-17.2541880063822,
4.60757114625466));
#161860=CARTESIAN_POINT('Ctrl Pts',(-19.928688100799,-17.2020137225569,
4.61240567856214));
#161861=CARTESIAN_POINT('Ctrl Pts',(-19.7927399723901,-17.1174098734573,
4.62121398285934));
#161862=CARTESIAN_POINT('Ctrl Pts',(-19.7311161795932,-17.0832010766469,
4.62514337858843));
#161863=CARTESIAN_POINT('Ctrl Pts',(-19.6436970962353,-17.0402291360845,
4.63071709143391));
#161864=CARTESIAN_POINT('Ctrl Pts',(-19.6192644837784,-17.0287934731523,
4.6322745660965));
#161865=CARTESIAN_POINT('Ctrl Pts',(-19.5765470545152,-17.009786110035,
4.63500129709143));
#161866=CARTESIAN_POINT('Ctrl Pts',(-19.5583619685493,-17.0019980412646,
4.63616320377414));
#161867=CARTESIAN_POINT('Ctrl Pts',(-19.5320226890888,-16.9911520855306,
4.63784880855595));
#161868=CARTESIAN_POINT('Ctrl Pts',(-19.5239542558002,-16.9878877256442,
4.63836551344969));
#161869=CARTESIAN_POINT('Ctrl Pts',(-19.5098224391324,-16.9822713799362,
4.63927123937356));
#161870=CARTESIAN_POINT('Ctrl Pts',(-19.5037678830984,-16.9798973914996,
4.63965951291637));
#161871=CARTESIAN_POINT('Ctrl Pts',(-19.4921132355662,-16.9753894576432,
4.64040739481024));
#161872=CARTESIAN_POINT('Ctrl Pts',(-19.4865148256578,-16.973251317091,
4.64076685768586));
#161873=CARTESIAN_POINT('Ctrl Pts',(-19.4718422547873,-16.9677188534331,
4.64170954464167));
#161874=CARTESIAN_POINT('Ctrl Pts',(-19.46275381587,-16.9643630279792,4.64229404985813));
#161875=CARTESIAN_POINT('Ctrl Pts',(-19.431217001625,-16.9529637132039,
4.64432449566297));
#161876=CARTESIAN_POINT('Ctrl Pts',(-19.4086566245709,-16.945237435757,
4.64578090473388));
#161877=CARTESIAN_POINT('Ctrl Pts',(-19.2347577410227,-16.8889459198539,
4.65704092704006));
#161878=CARTESIAN_POINT('Ctrl Pts',(-19.0785398342249,-16.8571909180743,
4.66740835014237));
#161879=CARTESIAN_POINT('Ctrl Pts',(-18.7874110144881,-16.8314749848445,
4.68671882997158));
#161880=CARTESIAN_POINT('Ctrl Pts',(-18.6537237659806,-16.8323203358347,
4.69556321698931));
#161881=CARTESIAN_POINT('Ctrl Pts',(-18.5090891374847,-16.8469471982232,
4.70457890295002));
#161882=CARTESIAN_POINT('Ctrl Pts',(-18.4971935837579,-16.8482521703523,
4.70531613825132));
#161883=CARTESIAN_POINT('Ctrl Pts',(-18.4803117678559,-16.850249156788,
4.70635572617602));
#161884=CARTESIAN_POINT('Ctrl Pts',(-18.4753161756283,-16.8508581660727,
4.70666252461021));
#161885=CARTESIAN_POINT('Ctrl Pts',(-18.4667158674537,-16.8519377611493,
4.7071892133745));
#161886=CARTESIAN_POINT('Ctrl Pts',(-18.4631101202749,-16.8523998265388,
4.70740957988198));
#161887=CARTESIAN_POINT('Ctrl Pts',(-18.456125210662,-16.8533132145747,
4.70783556917243));
#161888=CARTESIAN_POINT('Ctrl Pts',(-18.452745948205,-16.8537634116723,
4.70804125665595));
#161889=CARTESIAN_POINT('Ctrl Pts',(-18.4436401179133,-16.8549989154241,
4.70859445284494));
#161890=CARTESIAN_POINT('Ctrl Pts',(-18.4379156058049,-16.8557995221983,
4.70894110371066));
#161891=CARTESIAN_POINT('Ctrl Pts',(-18.4167307325724,-16.858850866087,
4.71022003850795));
#161892=CARTESIAN_POINT('Ctrl Pts',(-18.4012917160183,-16.8612493418011,
4.71114434419333));
#161893=CARTESIAN_POINT('Ctrl Pts',(-18.2518420397532,-16.886164033899,
4.72002861835446));
#161894=CARTESIAN_POINT('Ctrl Pts',(-18.1202473313518,-16.9213664980603,
4.72737209707388));
#161895=CARTESIAN_POINT('Ctrl Pts',(-17.8474697539941,-17.0233050659381,
4.74318579733434));
#161896=CARTESIAN_POINT('Ctrl Pts',(-17.7084584309003,-17.0934906421178,
4.75164275711871));
#161897=CARTESIAN_POINT('Ctrl Pts',(-17.5605541346376,-17.1898517935364,
4.76192306858276));
#161898=CARTESIAN_POINT('Ctrl Pts',(-17.5429075551342,-17.2017313806992,
4.76317135723129));
#161899=CARTESIAN_POINT('Ctrl Pts',(-17.5180627038245,-17.2190065480735,
4.76496143173987));
#161900=CARTESIAN_POINT('Ctrl Pts',(-17.5107148152778,-17.2241854365431,
4.76549497998513));
#161901=CARTESIAN_POINT('Ctrl Pts',(-17.4980927009536,-17.2332025440944,
4.76641876835455));
#161902=CARTESIAN_POINT('Ctrl Pts',(-17.4928027806735,-17.2370186567979,
4.76680815426463));
#161903=CARTESIAN_POINT('Ctrl Pts',(-17.4827059284014,-17.2443736427606,
4.76755569184351));
#161904=CARTESIAN_POINT('Ctrl Pts',(-17.4778961553104,-17.2479085236472,
4.76791368611938));
#161905=CARTESIAN_POINT('Ctrl Pts',(-17.4654235125766,-17.2571566279455,
4.76884701308591));
#161906=CARTESIAN_POINT('Ctrl Pts',(-17.4577843351987,-17.2629014438258,
4.76942357782286));
#161907=CARTESIAN_POINT('Ctrl Pts',(-17.4318448287081,-17.2826849034036,
4.77139842544028));
#161908=CARTESIAN_POINT('Ctrl Pts',(-17.4137356461174,-17.2969704076124,
4.77280642563418));
#161909=CARTESIAN_POINT('Ctrl Pts',(-17.2606433229297,-17.4218496533437,
4.78496779960191));
#161910=CARTESIAN_POINT('Ctrl Pts',(-17.1396036025273,-17.5484270415927,
4.79641594462189));
#161911=CARTESIAN_POINT('Ctrl Pts',(-16.9831336496416,-17.7587488697623,
4.81373668220938));
#161912=CARTESIAN_POINT('Ctrl Pts',(-16.9352031781223,-17.832306664799,
4.81951870117531));
#161913=CARTESIAN_POINT('Ctrl Pts',(-16.873244462909,-17.9416922878681,
4.82754620714642));
#161914=CARTESIAN_POINT('Ctrl Pts',(-16.8554092272129,-17.9752554245049,
4.82993665574684));
#161915=CARTESIAN_POINT('Ctrl Pts',(-16.8351098187183,-18.0160712838823,
4.83274182588761));
#161916=CARTESIAN_POINT('Ctrl Pts',(-16.8317700583309,-18.022877976134,
4.8332062963631));
#161917=CARTESIAN_POINT('Ctrl Pts',(-16.826643889089,-18.0334690122416,
4.83392366556618));
#161918=CARTESIAN_POINT('Ctrl Pts',(-16.8248320506798,-18.0372408779958,
4.83417810337687));
#161919=CARTESIAN_POINT('Ctrl Pts',(-16.8214979335923,-18.0442348625049,
4.83464792936058));
#161920=CARTESIAN_POINT('Ctrl Pts',(-16.8199726200361,-18.0474554251367,
4.83486350046578));
#161921=CARTESIAN_POINT('Ctrl Pts',(-16.816549249544,-18.0547309966319,
4.83534876790478));
#161922=CARTESIAN_POINT('Ctrl Pts',(-16.8146559253095,-18.0587881725892,
4.83561817017496));
#161923=CARTESIAN_POINT('Ctrl Pts',(-16.809124752865,-18.0707396324551,
4.83640831557005));
#161924=CARTESIAN_POINT('Ctrl Pts',(-16.8055225852273,-18.0786504600029,
4.83692691077849));
#161925=CARTESIAN_POINT('Ctrl Pts',(-16.7804077321024,-18.1347190292277,
4.84057293604675));
#161926=CARTESIAN_POINT('Ctrl Pts',(-16.7606507745182,-18.1836480249946,
4.84360127844008));
#161927=CARTESIAN_POINT('Ctrl Pts',(-16.73735532374,-18.2481884793583,4.84746205677662));
#161928=CARTESIAN_POINT('Ctrl Pts',(-16.7321376863721,-18.2631691681107,
4.84834901037666));
#161929=CARTESIAN_POINT('Ctrl Pts',(-16.7109324729106,-18.3263295177812,
4.85205540294843));
#161930=CARTESIAN_POINT('Ctrl Pts',(-16.6965116118114,-18.3750189036801,
4.85483249117402));
#161931=CARTESIAN_POINT('Ctrl Pts',(-16.6565766058816,-18.5301337781672,
4.86355328254866));
#161932=CARTESIAN_POINT('Ctrl Pts',(-16.6375535424663,-18.6380407012192,
4.86944421280929));
#161933=CARTESIAN_POINT('Ctrl Pts',(-16.6216105990453,-18.8018505503604,
4.87859515234573));
#161934=CARTESIAN_POINT('Ctrl Pts',(-16.618415026896,-18.8569557334196,
4.88170645412652));
#161935=CARTESIAN_POINT('Ctrl Pts',(-16.6167287794547,-18.9464533285306,
4.8868561722034));
#161936=CARTESIAN_POINT('Ctrl Pts',(-16.6169173843099,-18.9807956270069,
4.88885508612901));
#161937=CARTESIAN_POINT('Ctrl Pts',(-16.6182634673156,-19.0259245254794,
4.8915177937537));
#161938=CARTESIAN_POINT('Ctrl Pts',(-16.618668626598,-19.0367294832906,
4.89215801258617));
#161939=CARTESIAN_POINT('Ctrl Pts',(-16.6194678543697,-19.0544226581958,
4.89321097988307));
#161940=CARTESIAN_POINT('Ctrl Pts',(-16.6198128589424,-19.0613129757628,
4.8936221855651));
#161941=CARTESIAN_POINT('Ctrl Pts',(-16.620545930046,-19.0746481990425,
4.89442028063306));
#161942=CARTESIAN_POINT('Ctrl Pts',(-16.6209298132785,-19.0810932650825,
4.89480703430517));
#161943=CARTESIAN_POINT('Ctrl Pts',(-16.6218843407219,-19.0959718411295,
4.89570227454407));
#161944=CARTESIAN_POINT('Ctrl Pts',(-16.6224760212405,-19.104403848681,
4.89621141660208));
#161945=CARTESIAN_POINT('Ctrl Pts',(-16.6242032953423,-19.1270739123451,
4.89758519790726));
#161946=CARTESIAN_POINT('Ctrl Pts',(-16.6254324974504,-19.1413042029773,
4.89845276172805));
#161947=CARTESIAN_POINT('Ctrl Pts',(-16.6403655321411,-19.2959165237637,
4.90793723006079));
#161948=CARTESIAN_POINT('Ctrl Pts',(-16.6679197445768,-19.4345794148788,
4.91700377262712));
#161949=CARTESIAN_POINT('Ctrl Pts',(-16.7372255039126,-19.6618705569734,
4.93263656447653));
#161950=CARTESIAN_POINT('Ctrl Pts',(-16.7717001889072,-19.7522526135086,
4.93906371547369));
#161951=CARTESIAN_POINT('Ctrl Pts',(-16.832768076071,-19.8844185044703,
4.94856446621622));
#161952=CARTESIAN_POINT('Ctrl Pts',(-16.8548461434578,-19.9281498414661,
4.95172468780281));
#161953=CARTESIAN_POINT('Ctrl Pts',(-16.8910600140968,-19.9940894445889,
4.95647524086287));
#161954=CARTESIAN_POINT('Ctrl Pts',(-16.9041251107082,-20.0168644225433,
4.95811320058636));
#161955=CARTESIAN_POINT('Ctrl Pts',(-16.9210830106382,-20.0451910522236,
4.96014122342321));
#161956=CARTESIAN_POINT('Ctrl Pts',(-16.9245826731284,-20.0509738973456,
4.9605547499238));
#161957=CARTESIAN_POINT('Ctrl Pts',(-16.930199125645,-20.0601549675977,
4.96121037107058));
#161958=CARTESIAN_POINT('Ctrl Pts',(-16.9322979273812,-20.0635640641327,
4.96145361400821));
#161959=CARTESIAN_POINT('Ctrl Pts',(-16.9362987504488,-20.0700215235412,
4.96191394807351));
#161960=CARTESIAN_POINT('Ctrl Pts',(-16.9381988377285,-20.0730709591624,
4.96213115415988));
#161961=CARTESIAN_POINT('Ctrl Pts',(-16.9425927711319,-20.080082913768,
4.96263021362789));
#161962=CARTESIAN_POINT('Ctrl Pts',(-16.9450920042347,-20.0840420061228,
4.962911707208));
#161963=CARTESIAN_POINT('Ctrl Pts',(-16.9518304867256,-20.0946385481305,
4.96366445104067));
#161964=CARTESIAN_POINT('Ctrl Pts',(-16.9560937213901,-20.1012607600365,
4.96413415680802));
#161965=CARTESIAN_POINT('Ctrl Pts',(-16.9884341288233,-20.150885443716,
4.9676498060224));
#161966=CARTESIAN_POINT('Ctrl Pts',(-17.0180332723692,-20.1928809883391,
4.97060141188804));
#161967=CARTESIAN_POINT('Ctrl Pts',(-17.0626669549787,-20.2515516526043,
4.97475416758939));
#161968=CARTESIAN_POINT('Ctrl Pts',(-17.076481924843,-20.2691266167594,
4.97600207142634));
#161969=CARTESIAN_POINT('Ctrl Pts',(-17.119514681734,-20.3221219415788,
4.97978792889078));
#161970=CARTESIAN_POINT('Ctrl Pts',(-17.149609077374,-20.3568140883186,
4.98229853088526));
#161971=CARTESIAN_POINT('Ctrl Pts',(-17.2551134179209,-20.4707301954672,
4.99075196207313));
#161972=CARTESIAN_POINT('Ctrl Pts',(-17.3355222207308,-20.5450806466628,
4.99664017659348));
#161973=CARTESIAN_POINT('Ctrl Pts',(-17.4645497862562,-20.6470582914016,
5.00578480191334));
#161974=CARTESIAN_POINT('Ctrl Pts',(-17.5091039392043,-20.6795287121224,
5.00889248403912));
#161975=CARTESIAN_POINT('Ctrl Pts',(-17.5833664464427,-20.7293318583208,
5.01403674499457));
#161976=CARTESIAN_POINT('Ctrl Pts',(-17.6123200062058,-20.7477449440492,
5.01603393114697));
#161977=CARTESIAN_POINT('Ctrl Pts',(-17.6509662137625,-20.7710227194652,
5.01869466319579));
#161978=CARTESIAN_POINT('Ctrl Pts',(-17.6602678299966,-20.7765287217809,
5.01933467884781));
#161979=CARTESIAN_POINT('Ctrl Pts',(-17.6755739798853,-20.7854314672858,
5.02038739706774));
#161980=CARTESIAN_POINT('Ctrl Pts',(-17.6815537456503,-20.7888705630128,
5.02079855828543));
#161981=CARTESIAN_POINT('Ctrl Pts',(-17.6931629868897,-20.7954719967072,
5.02159662786776));
#161982=CARTESIAN_POINT('Ctrl Pts',(-17.6987903379179,-20.798637930024,
5.02198340084067));
#161983=CARTESIAN_POINT('Ctrl Pts',(-17.7118194744673,-20.8058898171546,
5.02287877434169));
#161984=CARTESIAN_POINT('Ctrl Pts',(-17.7192313926116,-20.809957252239,
5.02338803097568));
#161985=CARTESIAN_POINT('Ctrl Pts',(-17.7392356903843,-20.8207795918798,
5.0247623219171));
#161986=CARTESIAN_POINT('Ctrl Pts',(-17.7518722593776,-20.8274514870012,
5.02563028417575));
#161987=CARTESIAN_POINT('Ctrl Pts',(-17.8684343403599,-20.8874931911693,
5.03363629200761));
#161988=CARTESIAN_POINT('Ctrl Pts',(-17.9765265204829,-20.9322938996647,
5.04107600485072));
#161989=CARTESIAN_POINT('Ctrl Pts',(-18.2426389377099,-21.0176017536676,
5.05932949857795));
#161990=CARTESIAN_POINT('Ctrl Pts',(-18.402733842658,-21.0492384447102,
5.07028316856227));
#161991=CARTESIAN_POINT('Ctrl Pts',(-18.5973543192778,-21.0648366936974,
5.08269036370956));
#161992=CARTESIAN_POINT('Ctrl Pts',(-18.6298954305007,-21.0666899170629,
5.0847329084645));
#161993=CARTESIAN_POINT('Ctrl Pts',(-18.669709243479,-21.068035961258,5.08718259740535));
#161994=CARTESIAN_POINT('Ctrl Pts',(-18.6769514839577,-21.0682435968064,
5.08762620712772));
#161995=CARTESIAN_POINT('Ctrl Pts',(-18.6883044942779,-21.0685107653795,
5.08831833651239));
#161996=CARTESIAN_POINT('Ctrl Pts',(-18.692414534851,-21.0685955090576,
5.08856822950109));
#161997=CARTESIAN_POINT('Ctrl Pts',(-18.7000959912316,-21.0687315076159,
5.08903397575754));
#161998=CARTESIAN_POINT('Ctrl Pts',(-18.7036672506855,-21.0687856957413,
5.08924998492894));
#161999=CARTESIAN_POINT('Ctrl Pts',(-18.7118178866375,-21.0688887372833,
5.08974179744461));
#162000=CARTESIAN_POINT('Ctrl Pts',(-18.7163972862393,-21.0689317696994,
5.09001727221514));
#162001=CARTESIAN_POINT('Ctrl Pts',(-18.7304669815236,-21.0690183239641,
5.09086113069955));
#162002=CARTESIAN_POINT('Ctrl Pts',(-18.739957609618,-21.0690128910078,
5.09142684615873));
#162003=CARTESIAN_POINT('Ctrl Pts',(-18.8248630376806,-21.0683933063672,
5.09645906364571));
#162004=CARTESIAN_POINT('Ctrl Pts',(-18.9002035832334,-21.0638133558985,
5.10072176045197));
#162005=CARTESIAN_POINT('Ctrl Pts',(-19.0179674183209,-21.0503110439731,
5.10728418536582));
#162006=CARTESIAN_POINT('Ctrl Pts',(-19.06062951064,-21.044094664851,5.10964041612543));
#162007=CARTESIAN_POINT('Ctrl Pts',(-19.2107236004419,-21.0175206389198,
5.11793913118044));
#162008=CARTESIAN_POINT('Ctrl Pts',(-19.3167349574163,-20.9901511189904,
5.12382599657494));
#162009=CARTESIAN_POINT('Ctrl Pts',(-19.4722607396144,-20.9368662105857,
5.13296748542311));
#162010=CARTESIAN_POINT('Ctrl Pts',(-19.5236475170903,-20.9169882818635,
5.13607336980315));
#162011=CARTESIAN_POINT('Ctrl Pts',(-19.6056757259783,-20.8815197605387,
5.14121492016582));
#162012=CARTESIAN_POINT('Ctrl Pts',(-19.6368163463106,-20.8671468680067,
5.14321124788829));
#162013=CARTESIAN_POINT('Ctrl Pts',(-19.6772925860797,-20.8472585300596,
5.14587099834465));
#162014=CARTESIAN_POINT('Ctrl Pts',(-19.686955487947,-20.8424183743692,
5.14651091298803));
#162015=CARTESIAN_POINT('Ctrl Pts',(-19.702724319387,-20.8343681290028,
5.14756350738441));
#162016=CARTESIAN_POINT('Ctrl Pts',(-19.7088524441597,-20.8312017694866,
5.14797464649899));
#162017=CARTESIAN_POINT('Ctrl Pts',(-19.7206868542345,-20.825013546177,
5.14877270342908));
#162018=CARTESIAN_POINT('Ctrl Pts',(-19.7263950103721,-20.8219954102718,
5.14915948601311));
#162019=CARTESIAN_POINT('Ctrl Pts',(-19.7395460668224,-20.8149647350969,
5.15005492583848));
#162020=CARTESIAN_POINT('Ctrl Pts',(-19.7469788757128,-20.810933643473,
5.15056423949151));
#162021=CARTESIAN_POINT('Ctrl Pts',(-19.7669102989717,-20.7999690476493,
5.15193878407969));
#162022=CARTESIAN_POINT('Ctrl Pts',(-19.7793630077215,-20.7929534087402,
5.15280694464777));
#162023=CARTESIAN_POINT('Ctrl Pts',(-19.8931567518873,-20.7273171444248,
5.16082820197506));
#162024=CARTESIAN_POINT('Ctrl Pts',(-19.9895263038909,-20.6605201751907,
5.16828430063986));
#162025=CARTESIAN_POINT('Ctrl Pts',(-20.2060270758592,-20.4822081569832,
5.18660646187756));
#162026=CARTESIAN_POINT('Ctrl Pts',(-20.3197247266999,-20.3640474464165,
5.19761444217112));
#162027=CARTESIAN_POINT('Ctrl Pts',(-20.4378770607849,-20.2087796611593,
5.21000238967397));
#162028=CARTESIAN_POINT('Ctrl Pts',(-20.4564901138432,-20.1831458939925,
5.21198632647171));
#162029=CARTESIAN_POINT('Ctrl Pts',(-20.4786101724612,-20.1511980331212,
5.21437553034573));
#162030=CARTESIAN_POINT('Ctrl Pts',(-20.4826683393949,-20.1452726506132,
5.21481521474922));
#162031=CARTESIAN_POINT('Ctrl Pts',(-20.4889941122921,-20.1359347323959,
5.2155025871682));
#162032=CARTESIAN_POINT('Ctrl Pts',(-20.4912820552425,-20.132536134023,
5.21575161821234));
#162033=CARTESIAN_POINT('Ctrl Pts',(-20.4955472989714,-20.1261605024198,
5.21621662195751));
#162034=CARTESIAN_POINT('Ctrl Pts',(-20.4975269050341,-20.1231851379675,
5.21643274535901));
#162035=CARTESIAN_POINT('Ctrl Pts',(-20.502037840125,-20.1163677955967,
5.21692594123951));
#162036=CARTESIAN_POINT('Ctrl Pts',(-20.5045641807298,-20.1125225764154,
5.21720267799311));
#162037=CARTESIAN_POINT('Ctrl Pts',(-20.5111396724453,-20.1024428919576,
5.21792442154061));
#162038=CARTESIAN_POINT('Ctrl Pts',(-20.5151685959468,-20.0961952191495,
5.21836811189974));
#162039=CARTESIAN_POINT('Ctrl Pts',(-20.541703546346,-20.0545675216058,
5.22130102276341));
#162040=CARTESIAN_POINT('Ctrl Pts',(-20.5631887144981,-20.0185441508521,
5.2237275831468));
#162041=CARTESIAN_POINT('Ctrl Pts',(-20.5941629419433,-19.9629179261417,
5.22734528599898));
#162042=CARTESIAN_POINT('Ctrl Pts',(-20.6044420996057,-19.9437699469114,
5.22856809922211));
#162043=CARTESIAN_POINT('Ctrl Pts',(-20.6222695281991,-19.909297667153,
5.23073557943077));
#162044=CARTESIAN_POINT('Ctrl Pts',(-20.629930472772,-19.8940341268798,
5.2316836403405));
#162045=CARTESIAN_POINT('Ctrl Pts',(-20.6957491953938,-19.7588419955118,
5.23999253111414));
#162046=CARTESIAN_POINT('Ctrl Pts',(-20.7426454644707,-19.6337617913964,
5.24709268312486));
#162047=CARTESIAN_POINT('Ctrl Pts',(-20.8031161820857,-19.410347912284,
5.25986486011464));
#162048=CARTESIAN_POINT('Ctrl Pts',(-20.822138260334,-19.3139387120578,
5.26540006226036));
#162049=CARTESIAN_POINT('Ctrl Pts',(-20.836236815956,-19.2020092178444,
5.27201867132379));
#162050=CARTESIAN_POINT('Ctrl Pts',(-20.8379188842745,-19.1874348137934,
5.27288400798651));
#162051=CARTESIAN_POINT('Ctrl Pts',(-20.840256748618,-19.1651464720422,
5.27421317025278));
#162052=CARTESIAN_POINT('Ctrl Pts',(-20.8410219635071,-19.1574442807824,
5.27467354796835));
#162053=CARTESIAN_POINT('Ctrl Pts',(-20.8422815028458,-19.1440185067431,
5.27547794502019));
#162054=CARTESIAN_POINT('Ctrl Pts',(-20.8427948029168,-19.1382967534845,
5.2758213631654));
#162055=CARTESIAN_POINT('Ctrl Pts',(-20.8438966146506,-19.1254264216854,
5.27659522283431));
#162056=CARTESIAN_POINT('Ctrl Pts',(-20.8444720950169,-19.1182768247099,
5.27702607003716));
#162057=CARTESIAN_POINT('Ctrl Pts',(-20.8459169689305,-19.0991085327299,
5.27818382203152));
#162058=CARTESIAN_POINT('Ctrl Pts',(-20.8467200884103,-19.0870852422579,
5.2789127983333));
#162059=CARTESIAN_POINT('Ctrl Pts',(-20.8498276623848,-19.0337143082532,
5.28216143303529));
#162060=CARTESIAN_POINT('Ctrl Pts',(-20.8510211084385,-18.9923134313835,
5.28471560481465));
#162061=CARTESIAN_POINT('Ctrl Pts',(-20.8509121655105,-18.7814276655538,
5.29790822725658));
#162062=CARTESIAN_POINT('Ctrl Pts',(-20.8304727786253,-18.6125948125901,
5.30913940085526));
#162063=CARTESIAN_POINT('Ctrl Pts',(-20.7716984107369,-18.3727973124188,
5.32541882928644));
#162064=CARTESIAN_POINT('Ctrl Pts',(-20.7491431140367,-18.298635775203,
5.33048901901233));
#162065=CARTESIAN_POINT('Ctrl Pts',(-20.7225805585332,-18.2258895660964,
5.33540095489714));
#162066=CARTESIAN_POINT('Origin',(-18.734,-18.952,0.));
#162067=CARTESIAN_POINT('',(-20.7225805737622,-18.2258896078036,6.35350377396604));
#162068=CARTESIAN_POINT('',(-20.7225805737622,-18.2258896078036,6.13370788795281));
#162069=CARTESIAN_POINT('',(-20.7225805737622,-18.2258896078036,0.));
#162070=CARTESIAN_POINT('',(-20.8509995791066,-18.9506650608985,6.31236863518829));
#162071=CARTESIAN_POINT('Ctrl Pts',(-20.7225805737622,-18.2258896078036,
6.35350377396603));
#162072=CARTESIAN_POINT('Ctrl Pts',(-20.7233987857641,-18.228130424778,
6.35336132124997));
#162073=CARTESIAN_POINT('Ctrl Pts',(-20.7242132152326,-18.2303726385444,
6.35321908228664));
#162074=CARTESIAN_POINT('Ctrl Pts',(-20.7362148871419,-18.2635894227243,
6.3511163241643));
#162075=CARTESIAN_POINT('Ctrl Pts',(-20.7466823514128,-18.2948214849994,
6.34919592571695));
#162076=CARTESIAN_POINT('Ctrl Pts',(-20.804402162798,-18.4813823304818,
6.33798821755311));
#162077=CARTESIAN_POINT('Ctrl Pts',(-20.8343919994919,-18.6414983883584,
6.3294064643659));
#162078=CARTESIAN_POINT('Ctrl Pts',(-20.8492292021156,-18.852470693199,
6.31782784890908));
#162079=CARTESIAN_POINT('Ctrl Pts',(-20.850968615029,-18.9015609936698,
6.31511813187666));
#162080=CARTESIAN_POINT('Ctrl Pts',(-20.8509995791066,-18.9506650608985,
6.31236863518829));
#162081=CARTESIAN_POINT('Ctrl Pts',(-20.850999580792,-18.950667736265,6.31236848538577));
#162082=CARTESIAN_POINT('Ctrl Pts',(-20.851043483142,-19.0204296415699,
6.30846228705901));
#162083=CARTESIAN_POINT('Ctrl Pts',(-20.8476391052175,-19.0901465311592,
6.3044787447757));
#162084=CARTESIAN_POINT('Ctrl Pts',(-20.8397874280136,-19.1698415376233,
6.29977974061186));
#162085=CARTESIAN_POINT('Ctrl Pts',(-20.838699830613,-19.1801101595302,
6.29917153797656));
#162086=CARTESIAN_POINT('Ctrl Pts',(-20.8367367427085,-19.1974337468722,
6.29814066915109));
#162087=CARTESIAN_POINT('Ctrl Pts',(-20.8359007542262,-19.2044930707003,
6.29771924246229));
#162088=CARTESIAN_POINT('Ctrl Pts',(-20.8342952243256,-19.2174897628251,
6.29694082323744));
#162089=CARTESIAN_POINT('Ctrl Pts',(-20.8335360182493,-19.2234283523007,
6.29658415929102));
#162090=CARTESIAN_POINT('Ctrl Pts',(-20.8319167098582,-19.2356813162761,
6.29584620337817));
#162091=CARTESIAN_POINT('Ctrl Pts',(-20.8310532669144,-19.2419951810888,
6.29546480933832));
#162092=CARTESIAN_POINT('Ctrl Pts',(-20.8290511037879,-19.256159157267,
6.29460664266265));
#162093=CARTESIAN_POINT('Ctrl Pts',(-20.827896748574,-19.2640069295245,
6.29412937965364));
#162094=CARTESIAN_POINT('Ctrl Pts',(-20.8248477368161,-19.2839559768024,
6.29291155896707));
#162095=CARTESIAN_POINT('Ctrl Pts',(-20.8228921293394,-19.2960475129605,
6.29216907962002));
#162096=CARTESIAN_POINT('Ctrl Pts',(-20.8108473634669,-19.3666285385382,
6.28780914956202));
#162097=CARTESIAN_POINT('Ctrl Pts',(-20.798407807303,-19.4246849952108,
6.28411753440282));
#162098=CARTESIAN_POINT('Ctrl Pts',(-20.7682289796244,-19.5413582338922,
6.27647858351458));
#162099=CARTESIAN_POINT('Ctrl Pts',(-20.750352624344,-19.5998825593458,
6.27253040362192));
#162100=CARTESIAN_POINT('Ctrl Pts',(-20.6757998924098,-19.8107896640081,
6.25791902873149));
#162101=CARTESIAN_POINT('Ctrl Pts',(-20.6041653868007,-19.9572800498515,
6.24697387471078));
#162102=CARTESIAN_POINT('Ctrl Pts',(-20.498817485321,-20.1216921367102,
6.2345635089915));
#162103=CARTESIAN_POINT('Ctrl Pts',(-20.4805198616982,-20.1488413001332,
6.23251162573885));
#162104=CARTESIAN_POINT('Ctrl Pts',(-20.4574056988078,-20.1814773001668,
6.23005231627239));
#162105=CARTESIAN_POINT('Ctrl Pts',(-20.4531820976744,-20.1873762798653,
6.22960809306921));
#162106=CARTESIAN_POINT('Ctrl Pts',(-20.446516599077,-20.1965853988361,
6.22891522043675));
#162107=CARTESIAN_POINT('Ctrl Pts',(-20.444095284521,-20.199910267461,6.22866519291995));
#162108=CARTESIAN_POINT('Ctrl Pts',(-20.439553433237,-20.2061089431634,
6.2281993298121));
#162109=CARTESIAN_POINT('Ctrl Pts',(-20.4374353375712,-20.2089844095676,
6.22798333750798));
#162110=CARTESIAN_POINT('Ctrl Pts',(-20.4325865241339,-20.2155322561536,
6.2274917365059));
#162111=CARTESIAN_POINT('Ctrl Pts',(-20.4298511743862,-20.219201143286,
6.22721645528447));
#162112=CARTESIAN_POINT('Ctrl Pts',(-20.4214167320953,-20.2304379232171,
6.22637377849424));
#162113=CARTESIAN_POINT('Ctrl Pts',(-20.4156786290726,-20.2379765734037,
6.22580904033915));
#162114=CARTESIAN_POINT('Ctrl Pts',(-20.3357810536373,-20.3414956833256,
6.21805867897201));
#162115=CARTESIAN_POINT('Ctrl Pts',(-20.2535455451829,-20.4309830144674,
6.21140581709675));
#162116=CARTESIAN_POINT('Ctrl Pts',(-20.0841705050021,-20.5861590206874,
6.19890604494905));
#162117=CARTESIAN_POINT('Ctrl Pts',(-19.9987512761304,-20.6531288356912,
6.1930651781268));
#162118=CARTESIAN_POINT('Ctrl Pts',(-19.8636984675659,-20.7431954412522,
6.18403046750809));
#162119=CARTESIAN_POINT('Ctrl Pts',(-19.8176879652415,-20.7714008681651,
6.18098566704922));
#162120=CARTESIAN_POINT('Ctrl Pts',(-19.7510779233441,-20.8088105799518,
6.1765884665442));
#162121=CARTESIAN_POINT('Ctrl Pts',(-19.7313300613595,-20.8194918276574,
6.17528622691319));
#162122=CARTESIAN_POINT('Ctrl Pts',(-19.6962437822886,-20.837754089413,
6.17297262699503));
#162123=CARTESIAN_POINT('Ctrl Pts',(-19.680976173762,-20.8454671064222,
6.17196591636279));
#162124=CARTESIAN_POINT('Ctrl Pts',(-19.6582589621574,-20.8566000935249,
6.17046734883786));
#162125=CARTESIAN_POINT('Ctrl Pts',(-19.6508800291644,-20.8601632934894,
6.16998049039768));
#162126=CARTESIAN_POINT('Ctrl Pts',(-19.6379488512007,-20.8663152827094,
6.16912704763187));
#162127=CARTESIAN_POINT('Ctrl Pts',(-19.6324056771298,-20.8689229940936,
6.16876112497135));
#162128=CARTESIAN_POINT('Ctrl Pts',(-19.621338875214,-20.8740706755956,
6.16803037806014));
#162129=CARTESIAN_POINT('Ctrl Pts',(-19.6158154687229,-20.8766109839063,
6.16766556987319));
#162130=CARTESIAN_POINT('Ctrl Pts',(-19.6025755757097,-20.8826312758761,
6.16679084379954));
#162131=CARTESIAN_POINT('Ctrl Pts',(-19.5948490539073,-20.8860888183434,
6.16628016013403));
#162132=CARTESIAN_POINT('Ctrl Pts',(-19.5668348071423,-20.8984237932242,
6.16442766854472));
#162133=CARTESIAN_POINT('Ctrl Pts',(-19.5464293832845,-20.9070288584913,
6.16307661912572));
#162134=CARTESIAN_POINT('Ctrl Pts',(-19.3541095852768,-20.984600208948,
6.15032301682864));
#162135=CARTESIAN_POINT('Ctrl Pts',(-19.1740053997905,-21.031030376741,
6.13812470538277));
#162136=CARTESIAN_POINT('Ctrl Pts',(-18.9104071992707,-21.0631685341847,
6.12059190829744));
#162137=CARTESIAN_POINT('Ctrl Pts',(-18.8301098525211,-21.0683451279764,
6.11530922327973));
#162138=CARTESIAN_POINT('Ctrl Pts',(-18.7136130670479,-21.0692095534174,
6.1078823534815));
#162139=CARTESIAN_POINT('Ctrl Pts',(-18.6775145577286,-21.0685541984524,
6.10561444227034));
#162140=CARTESIAN_POINT('Ctrl Pts',(-18.633984969242,-21.0666493323093,
6.10293381883117));
#162141=CARTESIAN_POINT('Ctrl Pts',(-18.6265234886838,-21.0662832374951,
6.10247625427274));
#162142=CARTESIAN_POINT('Ctrl Pts',(-18.614909936501,-21.0656517839587,
6.1017672327431));
#162143=CARTESIAN_POINT('Ctrl Pts',(-18.6107565307587,-21.0654136734281,
6.1015142924468));
#162144=CARTESIAN_POINT('Ctrl Pts',(-18.6030445165533,-21.0649487395556,
6.1010458393058));
#162145=CARTESIAN_POINT('Ctrl Pts',(-18.5994858128871,-21.0647251710473,
6.10083015236547));
#162146=CARTESIAN_POINT('Ctrl Pts',(-18.5914280222152,-21.0641985143231,
6.10034285816504));
#162147=CARTESIAN_POINT('Ctrl Pts',(-18.5869293402096,-21.06389004322,6.10007155579034));
#162148=CARTESIAN_POINT('Ctrl Pts',(-18.575318338226,-21.0630566050789,
6.09937320108826));
#162149=CARTESIAN_POINT('Ctrl Pts',(-18.5682075575847,-21.0625100636874,
6.09894732958605));
#162150=CARTESIAN_POINT('Ctrl Pts',(-18.5245995980859,-21.0589365593799,
6.09634599517287));
#162151=CARTESIAN_POINT('Ctrl Pts',(-18.4881808926155,-21.0549986976973,
6.09421816496268));
#162152=CARTESIAN_POINT('Ctrl Pts',(-18.2828037996395,-21.0273830302017,
6.08238008614659));
#162153=CARTESIAN_POINT('Ctrl Pts',(-18.1170802547153,-20.9842930045862,
6.0734041916488));
#162154=CARTESIAN_POINT('Ctrl Pts',(-17.8695853032667,-20.8868306854097,
6.05877220236035));
#162155=CARTESIAN_POINT('Ctrl Pts',(-17.7833289432465,-20.8459387582868,
6.05342533555794));
#162156=CARTESIAN_POINT('Ctrl Pts',(-17.6814645164485,-20.7889309953434,
6.04662804272619));
#162157=CARTESIAN_POINT('Ctrl Pts',(-17.6629608295743,-20.7782041156094,
6.04537307950603));
#162158=CARTESIAN_POINT('Ctrl Pts',(-17.6368985461135,-20.7625630517011,
6.04357508507643));
#162159=CARTESIAN_POINT('Ctrl Pts',(-17.6292035343362,-20.757877883452,
6.04304039277113));
#162160=CARTESIAN_POINT('Ctrl Pts',(-17.6159861778431,-20.7497142948798,
6.04211524976306));
#162161=CARTESIAN_POINT('Ctrl Pts',(-17.6104495410475,-20.7462591666941,
6.04172566005054));
#162162=CARTESIAN_POINT('Ctrl Pts',(-17.5998832179371,-20.7395971877396,
6.04097816807181));
#162163=CARTESIAN_POINT('Ctrl Pts',(-17.5948509283285,-20.7363945674513,
6.04062042530392));
#162164=CARTESIAN_POINT('Ctrl Pts',(-17.5818091895734,-20.7280169672079,
6.03968871343354));
#162165=CARTESIAN_POINT('Ctrl Pts',(-17.5738211167267,-20.7228091047865,
6.03911352070479));
#162166=CARTESIAN_POINT('Ctrl Pts',(-17.5467468687812,-20.7048960898247,
6.03714837701873));
#162167=CARTESIAN_POINT('Ctrl Pts',(-17.5278325493053,-20.6919352618201,
6.03574883757156));
#162168=CARTESIAN_POINT('Ctrl Pts',(-17.3652842988574,-20.5766266259218,
6.02348271163937));
#162169=CARTESIAN_POINT('Ctrl Pts',(-17.2347769488205,-20.4570251849565,
6.01190444970991));
#162170=CARTESIAN_POINT('Ctrl Pts',(-17.0646907389936,-20.2568219800019,
5.99454841312577));
#162171=CARTESIAN_POINT('Ctrl Pts',(-17.0128306891587,-20.1876099355561,
5.98885571168467));
#162172=CARTESIAN_POINT('Ctrl Pts',(-16.9446426697063,-20.0839488401,5.98093496450927));
#162173=CARTESIAN_POINT('Ctrl Pts',(-16.9247842413231,-20.0519302596216,
5.97856583002893));
#162174=CARTESIAN_POINT('Ctrl Pts',(-16.9019763393875,-20.0128654501939,
5.97578227494572));
#162175=CARTESIAN_POINT('Ctrl Pts',(-16.8981980989368,-20.0063137960191,
5.97531897400177));
#162176=CARTESIAN_POINT('Ctrl Pts',(-16.8923860703478,-19.996109481399,
5.97460301792126));
#162177=CARTESIAN_POINT('Ctrl Pts',(-16.8903278990199,-19.9924708836874,
5.97434883320603));
#162178=CARTESIAN_POINT('Ctrl Pts',(-16.8865350407324,-19.9857189780537,
5.97387924108417));
#162179=CARTESIAN_POINT('Ctrl Pts',(-16.8847974526987,-19.9826074134515,
5.97366365223436));
#162180=CARTESIAN_POINT('Ctrl Pts',(-16.8808921200445,-19.9755723118657,
5.97317805058498));
#162181=CARTESIAN_POINT('Ctrl Pts',(-16.8787289803507,-19.971646280271,
5.97290833364313));
#162182=CARTESIAN_POINT('Ctrl Pts',(-16.8723961207589,-19.96006546309,5.9721164086354));
#162183=CARTESIAN_POINT('Ctrl Pts',(-16.8682611313399,-19.9523916537852,
5.97159636300104));
#162184=CARTESIAN_POINT('Ctrl Pts',(-16.8391843743181,-19.8976229359669,
5.96791656424516));
#162185=CARTESIAN_POINT('Ctrl Pts',(-16.8159791199815,-19.8496223666053,
5.9648579862251));
#162186=CARTESIAN_POINT('Ctrl Pts',(-16.7878680592657,-19.7853919224357,
5.96091481108591));
#162187=CARTESIAN_POINT('Ctrl Pts',(-16.7813111923146,-19.7699107949034,
5.959975541821));
#162188=CARTESIAN_POINT('Ctrl Pts',(-16.7185516531651,-19.6166743055174,
5.95077269045208));
#162189=CARTESIAN_POINT('Ctrl Pts',(-16.6768332173567,-19.4734329147004,
5.94288593558575));
#162190=CARTESIAN_POINT('Ctrl Pts',(-16.6395602777455,-19.266339899341,
5.93124378932298));
#162191=CARTESIAN_POINT('Ctrl Pts',(-16.6312979563321,-19.2052401723438,
5.9277849957254));
#162192=CARTESIAN_POINT('Ctrl Pts',(-16.6223429019767,-19.1068412132478,
5.92211439282943));
#162193=CARTESIAN_POINT('Ctrl Pts',(-16.6199492677345,-19.0697317040826,
5.91995341939017));
#162194=CARTESIAN_POINT('Ctrl Pts',(-16.6181106058018,-19.0214613240935,
5.91710590560176));
#162195=CARTESIAN_POINT('Ctrl Pts',(-16.6177747565675,-19.0103396600716,
5.91644732130659));
#162196=CARTESIAN_POINT('Ctrl Pts',(-16.6173711879845,-18.9922495687759,
5.9153718212583));
#162197=CARTESIAN_POINT('Ctrl Pts',(-16.6172501725339,-18.9852824545151,
5.91495657978525));
#162198=CARTESIAN_POINT('Ctrl Pts',(-16.6170836125737,-18.9718839711603,
5.91415599775826));
#162199=CARTESIAN_POINT('Ctrl Pts',(-16.6170329747036,-18.9654527341202,
5.91377082141));
#162200=CARTESIAN_POINT('Ctrl Pts',(-16.6169841377968,-18.9507281979257,
5.9128868464682));
#162201=CARTESIAN_POINT('Ctrl Pts',(-16.617005364764,-18.9424349790369,
5.91238744439236));
#162202=CARTESIAN_POINT('Ctrl Pts',(-16.6171911963953,-18.9204058743269,
5.91105674736304));
#162203=CARTESIAN_POINT('Ctrl Pts',(-16.6174407656691,-18.9066712739723,
5.91022280649256));
#162204=CARTESIAN_POINT('Ctrl Pts',(-16.6203575480668,-18.8021596104344,
5.90384346646464));
#162205=CARTESIAN_POINT('Ctrl Pts',(-16.6287295390135,-18.7116480599021,
5.89811957756085));
#162206=CARTESIAN_POINT('Ctrl Pts',(-16.6647945271128,-18.483140163643,
5.88317960886447));
#162207=CARTESIAN_POINT('Ctrl Pts',(-16.7004741667683,-18.3468482943189,
5.87378633691796));
#162208=CARTESIAN_POINT('Ctrl Pts',(-16.7682319149218,-18.1643607000658,
5.86104500790171));
#162209=CARTESIAN_POINT('Ctrl Pts',(-16.7890172317557,-18.1143469324901,
5.85753903952122));
#162210=CARTESIAN_POINT('Ctrl Pts',(-16.8234640977505,-18.039678553686,
5.85233645326813));
#162211=CARTESIAN_POINT('Ctrl Pts',(-16.8357367009845,-18.0144102813451,
5.85058167652124));
#162212=CARTESIAN_POINT('Ctrl Pts',(-16.8516520833486,-17.9832363056716,
5.84843086234387));
#162213=CARTESIAN_POINT('Ctrl Pts',(-16.8548251434399,-17.9770955758191,
5.84800788227506));
#162214=CARTESIAN_POINT('Ctrl Pts',(-16.8598991621421,-17.9673927945477,
5.84734077684181));
#162215=CARTESIAN_POINT('Ctrl Pts',(-16.8617803004878,-17.9638205138352,
5.84709543424074));
#162216=CARTESIAN_POINT('Ctrl Pts',(-16.8653510635632,-17.9570864340622,
5.84663347558478));
#162217=CARTESIAN_POINT('Ctrl Pts',(-16.8670384790357,-17.9539235847165,
5.84641673142875));
#162218=CARTESIAN_POINT('Ctrl Pts',(-16.8709195724475,-17.9466932426711,
5.8459217497663));
#162219=CARTESIAN_POINT('Ctrl Pts',(-16.8731185379313,-17.9426286407291,
5.84564385212606));
#162220=CARTESIAN_POINT('Ctrl Pts',(-16.8790018237925,-17.9318384575283,
5.84490699899004));
#162221=CARTESIAN_POINT('Ctrl Pts',(-16.8827094469492,-17.9251255682,5.84444948741176));
#162222=CARTESIAN_POINT('Ctrl Pts',(-16.909220316352,-17.8777362295717,
5.84122508016357));
#162223=CARTESIAN_POINT('Ctrl Pts',(-16.9333274430777,-17.8377995728001,
5.83853584201645));
#162224=CARTESIAN_POINT('Ctrl Pts',(-16.9612096157079,-17.7948812206126,
5.83564063338084));
#162225=CARTESIAN_POINT('Ctrl Pts',(-16.9636954794544,-17.7910816043858,
5.83538427195669));
#162226=CARTESIAN_POINT('Ctrl Pts',(-16.9790311182565,-17.7678050455661,
5.83381333308899));
#162227=CARTESIAN_POINT('Ctrl Pts',(-16.9921902791466,-17.7485331670506,
5.83251067145313));
#162228=CARTESIAN_POINT('Ctrl Pts',(-17.0319419082789,-17.6923343035576,
5.82869415952251));
#162229=CARTESIAN_POINT('Ctrl Pts',(-17.0594097316307,-17.6560420220676,
5.82620612657616));
#162230=CARTESIAN_POINT('Ctrl Pts',(-17.1567932640125,-17.5356437880277,
5.81777532092394));
#162231=CARTESIAN_POINT('Ctrl Pts',(-17.2320431804647,-17.4560819422162,
5.81188731274403));
#162232=CARTESIAN_POINT('Ctrl Pts',(-17.3539496719778,-17.3457039537544,
5.80274316712434));
#162233=CARTESIAN_POINT('Ctrl Pts',(-17.3962268068528,-17.3103276409578,
5.79963575995488));
#162234=CARTESIAN_POINT('Ctrl Pts',(-17.4669834836391,-17.2556701091351,
5.79449191356694));
#162235=CARTESIAN_POINT('Ctrl Pts',(-17.4946377919628,-17.2353616944497,
5.79249485870071));
#162236=CARTESIAN_POINT('Ctrl Pts',(-17.5316371066315,-17.2095507746281,
5.78983427677929));
#162237=CARTESIAN_POINT('Ctrl Pts',(-17.5405490939458,-17.203434657032,
5.78919427657986));
#162238=CARTESIAN_POINT('Ctrl Pts',(-17.5552247326988,-17.1935275226246,
5.78814157730774));
#162239=CARTESIAN_POINT('Ctrl Pts',(-17.5609608388292,-17.1896959090112,
5.78773041947644));
#162240=CARTESIAN_POINT('Ctrl Pts',(-17.5721021388198,-17.182332220164,
5.78693235184349));
#162241=CARTESIAN_POINT('Ctrl Pts',(-17.5775049727688,-17.1787967004989,
5.78654557740911));
#162242=CARTESIAN_POINT('Ctrl Pts',(-17.5900196131293,-17.1706888655283,
5.78565019378876));
#162243=CARTESIAN_POINT('Ctrl Pts',(-17.5971427698195,-17.1661343504382,
5.78514092845027));
#162244=CARTESIAN_POINT('Ctrl Pts',(-17.6163783350559,-17.1539969347018,
5.78376659877236));
#162245=CARTESIAN_POINT('Ctrl Pts',(-17.6285403945448,-17.1464939064731,
5.78289860622476));
#162246=CARTESIAN_POINT('Ctrl Pts',(-17.7408543942565,-17.0787652857835,
5.77489029412853));
#162247=CARTESIAN_POINT('Ctrl Pts',(-17.8457402330073,-17.0268160438482,
5.76744810588576));
#162248=CARTESIAN_POINT('Ctrl Pts',(-18.1056911581054,-16.9238453656543,
5.74918452634749));
#162249=CARTESIAN_POINT('Ctrl Pts',(-18.2634257144639,-16.8815548440293,
5.73822295915745));
#162250=CARTESIAN_POINT('Ctrl Pts',(-18.4565509253096,-16.8530087668865,
5.72581866731969));
#162251=CARTESIAN_POINT('Ctrl Pts',(-18.4887619029087,-16.8490019665329,
5.72378474652386));
#162252=CARTESIAN_POINT('Ctrl Pts',(-18.5282533819443,-16.8450093292195,
5.72134394612462));
#162253=CARTESIAN_POINT('Ctrl Pts',(-18.5354563422,-16.844318388127,5.72090090583395));
#162254=CARTESIAN_POINT('Ctrl Pts',(-18.5467548495372,-16.8432930179311,
5.72020946638671));
#162255=CARTESIAN_POINT('Ctrl Pts',(-18.5508479896444,-16.8429335656827,
5.7199596983162));
#162256=CARTESIAN_POINT('Ctrl Pts',(-18.5585013941033,-16.8422839057024,
5.71949406034148));
#162257=CARTESIAN_POINT('Ctrl Pts',(-18.5620613071291,-16.8419907949648,
5.71927803528614));
#162258=CARTESIAN_POINT('Ctrl Pts',(-18.5701900930888,-16.8413422081078,
5.7187860253456));
#162259=CARTESIAN_POINT('Ctrl Pts',(-18.5747593802421,-16.8409925566207,
5.71851037005742));
#162260=CARTESIAN_POINT('Ctrl Pts',(-18.5888102378123,-16.8399632357146,
5.71766540856972));
#162261=CARTESIAN_POINT('Ctrl Pts',(-18.5982954299812,-16.8393325775135,
5.71709878076436));
#162262=CARTESIAN_POINT('Ctrl Pts',(-18.683689920298,-16.8342322969739,
5.71202884219081));
#162263=CARTESIAN_POINT('Ctrl Pts',(-18.7597932037826,-16.8337912103267,
5.70773273720709));
#162264=CARTESIAN_POINT('Ctrl Pts',(-18.8781845333406,-16.8394887975101,
5.70117313781305));
#162265=CARTESIAN_POINT('Ctrl Pts',(-18.9205362033227,-16.8428065078548,
5.69885152820335));
#162266=CARTESIAN_POINT('Ctrl Pts',(-19.0714391837038,-16.8592089376823,
5.69058749971214));
#162267=CARTESIAN_POINT('Ctrl Pts',(-19.179038682833,-16.8794220601524,
5.68470091809202));
#162268=CARTESIAN_POINT('Ctrl Pts',(-19.3377693555559,-16.9221762172933,
5.67556008892389));
#162269=CARTESIAN_POINT('Ctrl Pts',(-19.3903645927526,-16.9385683769579,
5.67245458262747));
#162270=CARTESIAN_POINT('Ctrl Pts',(-19.4745732409515,-16.9684637297445,
5.66731360235643));
#162271=CARTESIAN_POINT('Ctrl Pts',(-19.5066030971589,-16.9807189143662,
5.66531745520338));
#162272=CARTESIAN_POINT('Ctrl Pts',(-19.5483165361838,-16.9978520092493,
5.66265791123408));
#162273=CARTESIAN_POINT('Ctrl Pts',(-19.5582814113878,-17.0020343748818,
5.66201801784993));
#162274=CARTESIAN_POINT('Ctrl Pts',(-19.5745533217416,-17.0090108872502,
5.66096544951941));
#162275=CARTESIAN_POINT('Ctrl Pts',(-19.5808795733104,-17.0117599206456,
5.66055431506169));
#162276=CARTESIAN_POINT('Ctrl Pts',(-19.5931016142093,-17.0171420958222,
5.65975626080593));
#162277=CARTESIAN_POINT('Ctrl Pts',(-19.5989990202117,-17.0197713938314,
5.65936947620586));
#162278=CARTESIAN_POINT('Ctrl Pts',(-19.6125913967767,-17.0259061140363,
5.65847402243893));
#162279=CARTESIAN_POINT('Ctrl Pts',(-19.6202775395163,-17.0294307243313,
5.65796469679604));
#162280=CARTESIAN_POINT('Ctrl Pts',(-19.6408989791659,-17.0390369716712,
5.65659009885363));
#162281=CARTESIAN_POINT('Ctrl Pts',(-19.6537939662945,-17.0452036422302,
5.65572189656714));
#162282=CARTESIAN_POINT('Ctrl Pts',(-19.7717737099056,-17.1030994109468,
5.64769737814423));
#162283=CARTESIAN_POINT('Ctrl Pts',(-19.8724413164911,-17.1633269806716,
5.64023777418421));
#162284=CARTESIAN_POINT('Ctrl Pts',(-20.1005659073467,-17.3268981327463,
5.62190029248212));
#162285=CARTESIAN_POINT('Ctrl Pts',(-20.2220276625825,-17.4373276444542,
5.61088001980022));
#162286=CARTESIAN_POINT('Ctrl Pts',(-20.3502424711645,-17.584359854051,
5.59849619923141));
#162287=CARTESIAN_POINT('Ctrl Pts',(-20.3703947342259,-17.6085373792621,
5.59652530378752));
#162288=CARTESIAN_POINT('Ctrl Pts',(-20.3944666603229,-17.6387632201585,
5.59414958451253));
#162289=CARTESIAN_POINT('Ctrl Pts',(-20.3989032904284,-17.644392487449,
5.59371079159916));
#162290=CARTESIAN_POINT('Ctrl Pts',(-20.4058289752123,-17.6532723008965,
5.5930244998631));
#162291=CARTESIAN_POINT('Ctrl Pts',(-20.4083372881398,-17.6565076592358,
5.59277566485376));
#162292=CARTESIAN_POINT('Ctrl Pts',(-20.4130180235565,-17.6625814286736,
5.59231082845444));
#162293=CARTESIAN_POINT('Ctrl Pts',(-20.415192617805,-17.6654180330958,
5.59209467755134));
#162294=CARTESIAN_POINT('Ctrl Pts',(-20.4201529741126,-17.6719225176489,
5.59160116008826));
#162295=CARTESIAN_POINT('Ctrl Pts',(-20.4229339523977,-17.6755939837619,
5.59132413091035));
#162296=CARTESIAN_POINT('Ctrl Pts',(-20.4301820178,-17.6852280910533,5.5906011224146));
#162297=CARTESIAN_POINT('Ctrl Pts',(-20.4346296941597,-17.6912053482633,
5.59015646706207));
#162298=CARTESIAN_POINT('Ctrl Pts',(-20.4640847896414,-17.7312296782737,
5.58720412581317));
#162299=CARTESIAN_POINT('Ctrl Pts',(-20.4881017004804,-17.7659977568095,
5.58476004801791));
#162300=CARTESIAN_POINT('Ctrl Pts',(-20.5515194671736,-17.8639498378017,
5.57813166305266));
#162301=CARTESIAN_POINT('Ctrl Pts',(-20.5886541327809,-17.9285305558673,
5.5740439278453));
#162302=CARTESIAN_POINT('Ctrl Pts',(-20.6602986497802,-18.0698871727679,
5.56540875113171));
#162303=CARTESIAN_POINT('Ctrl Pts',(-20.6937779253687,-18.1470084993638,
5.5608776423495));
#162304=CARTESIAN_POINT('Ctrl Pts',(-20.7225805962997,-18.2258896695266,
5.55626859415409));
#162305=CARTESIAN_POINT('',(-20.8509995343428,-18.9505958660381,6.0890562790225));
#162306=CARTESIAN_POINT('Ctrl Pts',(-20.7225805585332,-18.2258895660964,
5.33540095489714));
#162307=CARTESIAN_POINT('Ctrl Pts',(-20.7135660112331,-18.2012016499504,
5.33706792095253));
#162308=CARTESIAN_POINT('Ctrl Pts',(-20.7040899377832,-18.1766767254248,
5.33871643378043));
#162309=CARTESIAN_POINT('Ctrl Pts',(-20.6904971171894,-18.143358003269,
5.34093970850242));
#162310=CARTESIAN_POINT('Ctrl Pts',(-20.6867761540128,-18.1344132162557,
5.34153493717554));
#162311=CARTESIAN_POINT('Ctrl Pts',(-20.6811908866969,-18.1212425280375,
5.34240861895589));
#162312=CARTESIAN_POINT('Ctrl Pts',(-20.6793740068711,-18.1169968258862,
5.34268983322622));
#162313=CARTESIAN_POINT('Ctrl Pts',(-20.676125788991,-18.1094745083999,
5.34318727343144));
#162314=CARTESIAN_POINT('Ctrl Pts',(-20.6747000298907,-18.1061955433311,
5.34340383377577));
#162315=CARTESIAN_POINT('Ctrl Pts',(-20.6716271661213,-18.0991772400302,
5.34386676465063));
#162316=CARTESIAN_POINT('Ctrl Pts',(-20.6699775458628,-18.0954390638267,
5.34411297866601));
#162317=CARTESIAN_POINT('Ctrl Pts',(-20.6654189078965,-18.0851892564606,
5.34478715773716));
#162318=CARTESIAN_POINT('Ctrl Pts',(-20.6624877611379,-18.0786874435046,
5.34521378895089));
#162319=CARTESIAN_POINT('Ctrl Pts',(-20.6466515921782,-18.0440285031547,
5.34748317357265));
#162320=CARTESIAN_POINT('Ctrl Pts',(-20.6331619274932,-18.0161407406079,
5.34929208090094));
#162321=CARTESIAN_POINT('Ctrl Pts',(-20.5446480403026,-17.842955145594,
5.36047872978793));
#162322=CARTESIAN_POINT('Ctrl Pts',(-20.4536052723327,-17.7064491710487,
5.36912124662805));
#162323=CARTESIAN_POINT('Ctrl Pts',(-20.2715338980583,-17.4920196635696,
5.38451638569335));
#162324=CARTESIAN_POINT('Ctrl Pts',(-20.18797841007,-17.4087908422596,5.39108663600945));
#162325=CARTESIAN_POINT('Ctrl Pts',(-20.0870076680023,-17.3237298193577,
5.39882095723859));
#162326=CARTESIAN_POINT('Ctrl Pts',(-20.0759772265521,-17.3146269089445,
5.39966313469165));
#162327=CARTESIAN_POINT('Ctrl Pts',(-20.058277884116,-17.300319454549,5.40101058571771));
#162328=CARTESIAN_POINT('Ctrl Pts',(-20.0516684377585,-17.2950418159929,
5.40151291206349));
#162329=CARTESIAN_POINT('Ctrl Pts',(-20.0399575021166,-17.2858050232956,
5.40240155250734));
#162330=CARTESIAN_POINT('Ctrl Pts',(-20.034869163559,-17.2818293154277,
5.40278719948083));
#162331=CARTESIAN_POINT('Ctrl Pts',(-20.024308750341,-17.2736556089414,
5.40358666493282));
#162332=CARTESIAN_POINT('Ctrl Pts',(-20.0188341972768,-17.2694609514304,
5.40400060920177));
#162333=CARTESIAN_POINT('Ctrl Pts',(-20.0047322515299,-17.2587648583807,
5.40506566588964));
#162334=CARTESIAN_POINT('Ctrl Pts',(-19.9960754930004,-17.2523026319117,
5.4057183052982));
#162335=CARTESIAN_POINT('Ctrl Pts',(-19.9597641850371,-17.2256267725265,
5.40845129989368));
#162336=CARTESIAN_POINT('Ctrl Pts',(-19.9316718048834,-17.2060205069075,
5.41055492107091));
#162337=CARTESIAN_POINT('Ctrl Pts',(-19.8572712356199,-17.156735416053,
5.41610187652821));
#162338=CARTESIAN_POINT('Ctrl Pts',(-19.8102625662508,-17.1281657785285,
5.41958346675837));
#162339=CARTESIAN_POINT('Ctrl Pts',(-19.666653594967,-17.0483736690716,
5.43014244420328));
#162340=CARTESIAN_POINT('Ctrl Pts',(-19.5671477062197,-17.0027700578779,
5.43736825701715));
#162341=CARTESIAN_POINT('Ctrl Pts',(-19.4286084545432,-16.951830855491,
5.44711898869856));
#162342=CARTESIAN_POINT('Ctrl Pts',(-19.3922884268291,-16.9395850430519,
5.44964658586146));
#162343=CARTESIAN_POINT('Ctrl Pts',(-19.3246467361848,-16.918806031766,
5.45428250504768));
#162344=CARTESIAN_POINT('Ctrl Pts',(-19.2934220655813,-16.909994031609,
5.45639500985962));
#162345=CARTESIAN_POINT('Ctrl Pts',(-19.256085492626,-16.9003779298283,
5.45887994061256));
#162346=CARTESIAN_POINT('Ctrl Pts',(-19.2501581272849,-16.8988786764193,
5.45927321318656));
#162347=CARTESIAN_POINT('Ctrl Pts',(-19.2018755185495,-16.886888497545,
5.46246634254817));
#162348=CARTESIAN_POINT('Ctrl Pts',(-19.1592082255338,-16.8776828625035,
5.46522351884134));
#162349=CARTESIAN_POINT('Ctrl Pts',(-19.1088857525218,-16.8684438459875,
5.46837679874758));
#162350=CARTESIAN_POINT('Ctrl Pts',(-19.1014804961831,-16.8671250245751,
5.4688383358078));
#162351=CARTESIAN_POINT('Ctrl Pts',(-19.0895084869368,-16.8650586672177,
5.46958031171733));
#162352=CARTESIAN_POINT('Ctrl Pts',(-19.0849461127333,-16.8642866006908,
5.46986208886646));
#162353=CARTESIAN_POINT('Ctrl Pts',(-19.0768529212297,-16.862944312483,
5.47036015182437));
#162354=CARTESIAN_POINT('Ctrl Pts',(-19.0733231563496,-16.8623680737048,
5.47057677515913));
#162355=CARTESIAN_POINT('Ctrl Pts',(-19.0657633011453,-16.8611535780393,
5.47103942893412));
#162356=CARTESIAN_POINT('Ctrl Pts',(-19.0617328320122,-16.8605180278854,
5.47128530500882));
#162357=CARTESIAN_POINT('Ctrl Pts',(-19.0506781036699,-16.8588075880518,
5.47195760577381));
#162358=CARTESIAN_POINT('Ctrl Pts',(-19.0436501562667,-16.8577563945981,
5.47238270898023));
#162359=CARTESIAN_POINT('Ctrl Pts',(-19.0063137545842,-16.8523639226998,
5.47462949566018));
#162360=CARTESIAN_POINT('Ctrl Pts',(-18.9759173890594,-16.8486449097502,
5.47641812652884));
#162361=CARTESIAN_POINT('Ctrl Pts',(-18.8840169356094,-16.8394196148042,
5.48173263747361));
#162362=CARTESIAN_POINT('Ctrl Pts',(-18.8223395391613,-16.8359427705003,
5.48517443335155));
#162363=CARTESIAN_POINT('Ctrl Pts',(-18.6140799929785,-16.8333263510387,
5.49662776081094));
#162364=CARTESIAN_POINT('Ctrl Pts',(-18.4677734657393,-16.8467011993875,
5.504421425657));
#162365=CARTESIAN_POINT('Ctrl Pts',(-18.2500273164865,-16.8896839391248,
5.51680892369875));
#162366=CARTESIAN_POINT('Ctrl Pts',(-18.1768760839219,-16.9082318526576,
5.52110478521814));
#162367=CARTESIAN_POINT('Ctrl Pts',(-18.0923220510918,-16.9345483256142,
5.52630057373922));
#162368=CARTESIAN_POINT('Ctrl Pts',(-18.0798057078927,-16.9385721604367,
5.52707566604996));
#162369=CARTESIAN_POINT('Ctrl Pts',(-18.0595388562537,-16.9452966056,5.52834078923163));
#162370=CARTESIAN_POINT('Ctrl Pts',(-18.0517650280505,-16.9479262020394,
5.52882847957221));
#162371=CARTESIAN_POINT('Ctrl Pts',(-18.0379553303796,-16.952687170475,
5.52969922967628));
#162372=CARTESIAN_POINT('Ctrl Pts',(-18.0319134375454,-16.9548008537353,
5.53008169916945));
#162373=CARTESIAN_POINT('Ctrl Pts',(-18.0192089621152,-16.9593101343908,
5.53088914843016));
#162374=CARTESIAN_POINT('Ctrl Pts',(-18.0125486365597,-16.9617118156818,
5.53131432693003));
#162375=CARTESIAN_POINT('Ctrl Pts',(-17.9949779392209,-16.968147509922,
5.53244101641201));
#162376=CARTESIAN_POINT('Ctrl Pts',(-17.9840886665018,-16.9722380718542,
5.53314440929393));
#162377=CARTESIAN_POINT('Ctrl Pts',(-17.9338102135396,-16.9915995300672,
5.53641641630369));
#162378=CARTESIAN_POINT('Ctrl Pts',(-17.8948522858883,-17.007956685442,
5.53902131813492));
#162379=CARTESIAN_POINT('Ctrl Pts',(-17.7890749204608,-17.0561411626773,
5.54629293078017));
#162380=CARTESIAN_POINT('Ctrl Pts',(-17.7233988435647,-17.0903212964203,
5.55103442014254));
#162381=CARTESIAN_POINT('Ctrl Pts',(-17.528073950343,-17.2053605156642,
5.5657968061218));
#162382=CARTESIAN_POINT('Ctrl Pts',(-17.405273586751,-17.2968591907233,
5.57605686761176));
#162383=CARTESIAN_POINT('Ctrl Pts',(-17.2580948998451,-17.4335426444481,
5.58899242826385));
#162384=CARTESIAN_POINT('Ctrl Pts',(-17.2239295827149,-17.46751465858,5.59204440728228));
#162385=CARTESIAN_POINT('Ctrl Pts',(-17.1856498353416,-17.508268478083,
5.59549198810629));
#162386=CARTESIAN_POINT('Ctrl Pts',(-17.1803802319196,-17.5139406965637,
5.59596722427078));
#162387=CARTESIAN_POINT('Ctrl Pts',(-17.1720004384982,-17.5230605590853,
5.59672379565999));
#162388=CARTESIAN_POINT('Ctrl Pts',(-17.1688703244286,-17.5264896859279,
5.59700658960716));
#162389=CARTESIAN_POINT('Ctrl Pts',(-17.1633415316753,-17.5325867948411,
5.59750638975362));
#162390=CARTESIAN_POINT('Ctrl Pts',(-17.1609383238777,-17.535250609689,
5.59772373654553));
#162391=CARTESIAN_POINT('Ctrl Pts',(-17.1558533954762,-17.5409158444572,
5.59818381408242));
#162392=CARTESIAN_POINT('Ctrl Pts',(-17.1531734648347,-17.5439188000216,
5.59842641171024));
#162393=CARTESIAN_POINT('Ctrl Pts',(-17.1459516885744,-17.5520576563149,
5.599080541687));
#162394=CARTESIAN_POINT('Ctrl Pts',(-17.1414261561243,-17.5572080585964,
5.59949086952868));
#162395=CARTESIAN_POINT('Ctrl Pts',(-17.1189400086327,-17.5830511383967,
5.60153230711408));
#162396=CARTESIAN_POINT('Ctrl Pts',(-17.1013563914851,-17.604070190905,
5.60313711806937));
#162397=CARTESIAN_POINT('Ctrl Pts',(-17.0514933329909,-17.6660831771208,
5.60773291477103));
#162398=CARTESIAN_POINT('Ctrl Pts',(-17.0203135728354,-17.7079379729551,
5.6106643157784));
#162399=CARTESIAN_POINT('Ctrl Pts',(-16.9116076690405,-17.865715536876,
5.62127357467201));
#162400=CARTESIAN_POINT('Ctrl Pts',(-16.8440392596118,-17.9880609395962,
5.62868690682174));
#162401=CARTESIAN_POINT('Ctrl Pts',(-16.751676510829,-18.2029915233819,
5.64161059620066));
#162402=CARTESIAN_POINT('Ctrl Pts',(-16.7202241469305,-18.2922093393727,
5.6469441738315));
#162403=CARTESIAN_POINT('Ctrl Pts',(-16.6911214235892,-18.3965474969471,
5.65329380954537));
#162404=CARTESIAN_POINT('Ctrl Pts',(-16.6875355641712,-18.4099080701129,
5.65410879298426));
#162405=CARTESIAN_POINT('Ctrl Pts',(-16.6820027344617,-18.4313605168971,
5.65542081972188));
#162406=CARTESIAN_POINT('Ctrl Pts',(-16.6799720577307,-18.4394305329991,
5.65591515598409));
#162407=CARTESIAN_POINT('Ctrl Pts',(-16.6764553774996,-18.4537625613928,
5.65679453493138));
#162408=CARTESIAN_POINT('Ctrl Pts',(-16.6749502422923,-18.4600198045835,
5.65717895512081));
#162409=CARTESIAN_POINT('Ctrl Pts',(-16.6718778942383,-18.4730534516674,
5.65798075132927));
#162410=CARTESIAN_POINT('Ctrl Pts',(-16.6703154998704,-18.4798309017319,
5.65839827728063));
#162411=CARTESIAN_POINT('Ctrl Pts',(-16.6663534353189,-18.4974131706843,
5.6594830328968));
#162412=CARTESIAN_POINT('Ctrl Pts',(-16.6640050737539,-18.5082292260038,
5.66015189999645));
#162413=CARTESIAN_POINT('Ctrl Pts',(-16.6542496807475,-18.5549235402367,
5.66304652316464));
#162414=CARTESIAN_POINT('Ctrl Pts',(-16.6476901973596,-18.590970569524,
5.6652991249978));
#162415=CARTESIAN_POINT('Ctrl Pts',(-16.6328073443966,-18.6868166955601,
5.67133982202806));
#162416=CARTESIAN_POINT('Ctrl Pts',(-16.6261013401342,-18.7468294803527,
5.67517521063258));
#162417=CARTESIAN_POINT('Ctrl Pts',(-16.6106548534774,-18.9718850524776,
5.68973439322023));
#162418=CARTESIAN_POINT('Ctrl Pts',(-16.6186785147509,-19.1374675704465,
5.70085095367274));
#162419=CARTESIAN_POINT('Ctrl Pts',(-16.6466295126158,-19.3049798581185,
5.71184199648554));
#162420=CARTESIAN_POINT('Ctrl Pts',(-16.6474045776612,-19.3095330415694,
5.71214050335372));
#162421=CARTESIAN_POINT('Ctrl Pts',(-16.6483125256036,-19.3147633319331,
5.7124830972345));
#162422=CARTESIAN_POINT('Ctrl Pts',(-16.6484308417836,-19.3154429283221,
5.7125276061728));
#162423=CARTESIAN_POINT('Ctrl Pts',(-16.6504318302204,-19.3269032548044,
5.71327807870787));
#162424=CARTESIAN_POINT('Ctrl Pts',(-16.6523977688055,-19.3376694531432,
5.71398159220466));
#162425=CARTESIAN_POINT('Ctrl Pts',(-16.6620277805191,-19.3881868693206,
5.71727416243951));
#162426=CARTESIAN_POINT('Ctrl Pts',(-16.6707481340064,-19.4277311132873,
5.71982693886713));
#162427=CARTESIAN_POINT('Ctrl Pts',(-16.6823874262688,-19.4741388318139,
5.72277464005917));
#162428=CARTESIAN_POINT('Ctrl Pts',(-16.6842141588694,-19.4812646988971,
5.72322589934859));
#162429=CARTESIAN_POINT('Ctrl Pts',(-16.6872377838357,-19.4928090075172,
5.72395459646749));
#162430=CARTESIAN_POINT('Ctrl Pts',(-16.6884119106158,-19.4972332726534,
5.72423329782207));
#162431=CARTESIAN_POINT('Ctrl Pts',(-16.6905276796529,-19.5051027312929,
5.72472797305055));
#162432=CARTESIAN_POINT('Ctrl Pts',(-16.6914636975086,-19.5085493770067,
5.72494426740744));
#162433=CARTESIAN_POINT('Ctrl Pts',(-16.693496256492,-19.5159595587861,
5.72540850548611));
#162434=CARTESIAN_POINT('Ctrl Pts',(-16.694595622108,-19.519922261681,5.72565628283512));
#162435=CARTESIAN_POINT('Ctrl Pts',(-16.6976654942767,-19.5308638594846,
5.72633916638811));
#162436=CARTESIAN_POINT('Ctrl Pts',(-16.6996603447386,-19.5378359476061,
5.72677288082037));
#162437=CARTESIAN_POINT('Ctrl Pts',(-16.7108434076673,-19.5761752274405,
5.72915069929992));
#162438=CARTESIAN_POINT('Ctrl Pts',(-16.7207218191578,-19.6073384954114,
5.73105701045006));
#162439=CARTESIAN_POINT('Ctrl Pts',(-16.784013906238,-19.7920402849525,
5.74226543886967));
#162440=CARTESIAN_POINT('Ctrl Pts',(-16.8542508862671,-19.9392530083768,
5.75085776160672));
#162441=CARTESIAN_POINT('Ctrl Pts',(-17.0027194984562,-20.1759273173352,
5.76615304170199));
#162442=CARTESIAN_POINT('Ctrl Pts',(-17.0728581933659,-20.2695480614537,
5.77267334289562));
#162443=CARTESIAN_POINT('Ctrl Pts',(-17.1598351761568,-20.3675911473464,
5.78035144233042));
#162444=CARTESIAN_POINT('Ctrl Pts',(-17.1694258859234,-20.3781840749792,
5.78119292552645));
#162445=CARTESIAN_POINT('Ctrl Pts',(-17.1848605383916,-20.3948885641239,
5.78253947318229));
#162446=CARTESIAN_POINT('Ctrl Pts',(-17.1906352321315,-20.4010637219014,
5.78304159666562));
#162447=CARTESIAN_POINT('Ctrl Pts',(-17.2008850422826,-20.4118935635214,
5.78393000078321));
#162448=CARTESIAN_POINT('Ctrl Pts',(-17.2053447793969,-20.416562701111,
5.78431561543046));
#162449=CARTESIAN_POINT('Ctrl Pts',(-17.2146131852289,-20.4261778361843,
5.78511513420377));
#162450=CARTESIAN_POINT('Ctrl Pts',(-17.2194248029293,-20.4311208727698,
5.78552916471337));
#162451=CARTESIAN_POINT('Ctrl Pts',(-17.2318378015758,-20.4437488286995,
5.78659469671665));
#162452=CARTESIAN_POINT('Ctrl Pts',(-17.2394739679688,-20.4513991366863,
5.78724772783286));
#162453=CARTESIAN_POINT('Ctrl Pts',(-17.2715919344855,-20.4830874657198,
5.78998451671004));
#162454=CARTESIAN_POINT('Ctrl Pts',(-17.2965965758149,-20.5065859119125,
5.79209162134595));
#162455=CARTESIAN_POINT('Ctrl Pts',(-17.3632291513305,-20.566222423206,
5.79764995273216));
#162456=CARTESIAN_POINT('Ctrl Pts',(-17.4057149383756,-20.6013588829749,
5.80113963136773));
#162457=CARTESIAN_POINT('Ctrl Pts',(-17.5364854946473,-20.7011761845427,
5.81171414833407));
#162458=CARTESIAN_POINT('Ctrl Pts',(-17.6284596213665,-20.7607109555451,
5.81894736091875));
#162459=CARTESIAN_POINT('Ctrl Pts',(-17.8286596664689,-20.8693050643782,
5.83399225978492));
#162460=CARTESIAN_POINT('Ctrl Pts',(-17.9372687529282,-20.9169238339103,
5.84177589648977));
#162461=CARTESIAN_POINT('Ctrl Pts',(-18.0583209110286,-20.9582994912081,
5.84967761096853));
#162462=CARTESIAN_POINT('Ctrl Pts',(-18.0673625331739,-20.9613218695196,
5.85026323333849));
#162463=CARTESIAN_POINT('Ctrl Pts',(-18.0807854438123,-20.9657082193506,
5.85112554954407));
#162464=CARTESIAN_POINT('Ctrl Pts',(-18.0851511010813,-20.9671191419822,
5.85140490399214));
#162465=CARTESIAN_POINT('Ctrl Pts',(-18.0929242660442,-20.9696034461522,
5.8519002953606));
#162466=CARTESIAN_POINT('Ctrl Pts',(-18.0963299317984,-20.9706824037902,
5.85211665638576));
#162467=CARTESIAN_POINT('Ctrl Pts',(-18.1036551236241,-20.9729827288844,
5.85258054341281));
#162468=CARTESIAN_POINT('Ctrl Pts',(-18.1075754644813,-20.974201314306,
5.85282790564607));
#162469=CARTESIAN_POINT('Ctrl Pts',(-18.1183999969435,-20.9775314764298,
5.85350847531314));
#162470=CARTESIAN_POINT('Ctrl Pts',(-18.1253115585935,-20.9796191729427,
5.85394030648065));
#162471=CARTESIAN_POINT('Ctrl Pts',(-18.1631243408226,-20.9908300782805,
5.85628868661778));
#162472=CARTESIAN_POINT('Ctrl Pts',(-18.1942218783975,-20.9992828189253,
5.85816853705458));
#162473=CARTESIAN_POINT('Ctrl Pts',(-18.383680714159,-21.0461627927648,
5.8693785749537));
#162474=CARTESIAN_POINT('Ctrl Pts',(-18.5458657190907,-21.0669134396363,
5.87799093693147));
#162475=CARTESIAN_POINT('Ctrl Pts',(-18.8257554460276,-21.0702400933843,
5.89331411136127));
#162476=CARTESIAN_POINT('Ctrl Pts',(-18.9425694519663,-21.0619416269869,
5.8998411419959));
#162477=CARTESIAN_POINT('Ctrl Pts',(-19.0722153176857,-21.0418573243487,
5.90752681667408));
#162478=CARTESIAN_POINT('Ctrl Pts',(-19.0863152331751,-21.0395265743963,
5.90836839777694));
#162479=CARTESIAN_POINT('Ctrl Pts',(-19.1087176984666,-21.0355899631908,
5.90971507283278));
#162480=CARTESIAN_POINT('Ctrl Pts',(-19.1170362441381,-21.0340767807088,
5.91021722492811));
#162481=CARTESIAN_POINT('Ctrl Pts',(-19.1316910170746,-21.0313202125601,
5.91110566237399));
#162482=CARTESIAN_POINT('Ctrl Pts',(-19.1380310740476,-21.0300975870255,
5.91149128157707));
#162483=CARTESIAN_POINT('Ctrl Pts',(-19.1511325799385,-21.0275088517307,
5.91229079281219));
#162484=CARTESIAN_POINT('Ctrl Pts',(-19.1578931359694,-21.0261386622848,
5.91270481114415));
#162485=CARTESIAN_POINT('Ctrl Pts',(-19.1752290944058,-21.0225368156599,
5.91377027603383));
#162486=CARTESIAN_POINT('Ctrl Pts',(-19.1857942253928,-21.0202571865874,
5.91442325184223));
#162487=CARTESIAN_POINT('Ctrl Pts',(-19.2298154035022,-21.0104053836241,
5.91715950466795));
#162488=CARTESIAN_POINT('Ctrl Pts',(-19.2631008442643,-21.002101879917,
5.91926611712376));
#162489=CARTESIAN_POINT('Ctrl Pts',(-19.3492886245532,-20.9783624408507,
5.92482284071704));
#162490=CARTESIAN_POINT('Ctrl Pts',(-19.4018134129606,-20.9616639664461,
5.92831137601296));
#162491=CARTESIAN_POINT('Ctrl Pts',(-19.6495371044364,-20.8721242887725,
5.94524250178755));
#162492=CARTESIAN_POINT('Ctrl Pts',(-19.8338993122075,-20.7727948994148,
5.95943299137011));
#162493=CARTESIAN_POINT('Ctrl Pts',(-20.0044076837944,-20.6454502673376,
5.97284947527249));
#162494=CARTESIAN_POINT('Ctrl Pts',(-20.0080258472485,-20.6427299110824,
5.97313425506109));
#162495=CARTESIAN_POINT('Ctrl Pts',(-20.0280037889704,-20.6276087295909,
5.97470702797371));
#162496=CARTESIAN_POINT('Ctrl Pts',(-20.0441919305309,-20.6149815386789,
5.97598272523516));
#162497=CARTESIAN_POINT('Ctrl Pts',(-20.0652189160412,-20.5980822423302,
5.9776386286751));
#162498=CARTESIAN_POINT('Ctrl Pts',(-20.0702249333119,-20.594021157299,
5.97803277399033));
#162499=CARTESIAN_POINT('Ctrl Pts',(-20.078255760117,-20.5874451759944,
5.9786648286444));
#162500=CARTESIAN_POINT('Ctrl Pts',(-20.0812922001731,-20.5849446408951,
5.97890374995387));
#162501=CARTESIAN_POINT('Ctrl Pts',(-20.0869640603339,-20.5802472240868,
5.97934990184067));
#162502=CARTESIAN_POINT('Ctrl Pts',(-20.0896011096847,-20.5780523985531,
5.97955727488255));
#162503=CARTESIAN_POINT('Ctrl Pts',(-20.0958374887617,-20.5728361231763,
5.98004757816586));
#162504=CARTESIAN_POINT('Ctrl Pts',(-20.0994321377805,-20.5698090623061,
5.98033009954665));
#162505=CARTESIAN_POINT('Ctrl Pts',(-20.1106650327052,-20.5602857117942,
5.98121277586101));
#162506=CARTESIAN_POINT('Ctrl Pts',(-20.1182673520699,-20.5537469993475,
5.98180991118469));
#162507=CARTESIAN_POINT('Ctrl Pts',(-20.1360931391857,-20.5381934312686,
5.9832102571503));
#162508=CARTESIAN_POINT('Ctrl Pts',(-20.1462766852041,-20.5291332717567,
5.98401040178967));
#162509=CARTESIAN_POINT('Ctrl Pts',(-20.1816923608735,-20.4970063112347,
5.9867965794332));
#162510=CARTESIAN_POINT('Ctrl Pts',(-20.2064537415239,-20.4734262727678,
5.98875090838179));
#162511=CARTESIAN_POINT('Ctrl Pts',(-20.2843263290296,-20.3955859953749,
5.99496002150858));
#162512=CARTESIAN_POINT('Ctrl Pts',(-20.3350957616044,-20.3390637948339,
5.99910803332371));
#162513=CARTESIAN_POINT('Ctrl Pts',(-20.4906342492996,-20.1459519721364,
6.01259284077695));
#162514=CARTESIAN_POINT('Ctrl Pts',(-20.5818013463658,-19.9993340180964,
6.02185806072684));
#162515=CARTESIAN_POINT('Ctrl Pts',(-20.6640048104395,-19.8222356646158,
6.03320084879666));
#162516=CARTESIAN_POINT('Ctrl Pts',(-20.6734378130662,-19.8010050569571,
6.03456163412833));
#162517=CARTESIAN_POINT('Ctrl Pts',(-20.6862667133323,-19.7708012979155,
6.03650078366958));
#162518=CARTESIAN_POINT('Ctrl Pts',(-20.6899541465969,-19.7619532438794,
6.03706923108221));
#162519=CARTESIAN_POINT('Ctrl Pts',(-20.6958419147377,-19.7475507467972,
6.03799526562721));
#162520=CARTESIAN_POINT('Ctrl Pts',(-20.6980790779002,-19.742011432689,
6.03835160206131));
#162521=CARTESIAN_POINT('Ctrl Pts',(-20.7027082021864,-19.7304083153777,
6.0390984161855));
#162522=CARTESIAN_POINT('Ctrl Pts',(-20.7050956594865,-19.7243427933783,
6.03948904107576));
#162523=CARTESIAN_POINT('Ctrl Pts',(-20.7107003759924,-19.7099083145188,
6.04041922051662));
#162524=CARTESIAN_POINT('Ctrl Pts',(-20.7138925368234,-19.701529804898,
6.04095961076518));
#162525=CARTESIAN_POINT('Ctrl Pts',(-20.724429857036,-19.6733352943484,
6.04277978457929));
#162526=CARTESIAN_POINT('Ctrl Pts',(-20.73153131129,-19.6534301335466,6.04406765108529));
#162527=CARTESIAN_POINT('Ctrl Pts',(-20.7683471023197,-19.5451403217933,
6.05109146810279));
#162528=CARTESIAN_POINT('Ctrl Pts',(-20.7924915414983,-19.4549832624818,
6.05700835583422));
#162529=CARTESIAN_POINT('Ctrl Pts',(-20.8375614576733,-19.2275614183288,
6.07205891368725));
#162530=CARTESIAN_POINT('Ctrl Pts',(-20.8510859073101,-19.0892811223752,
6.0813351986236));
#162531=CARTESIAN_POINT('Ctrl Pts',(-20.8509995894478,-18.9506815623441,
6.09037079128207));
#162532=CARTESIAN_POINT('Ctrl Pts',(-20.7225805737622,-18.2258896078036,
6.13370788795281));
#162533=CARTESIAN_POINT('Ctrl Pts',(-20.7475745958775,-18.2943401180468,
6.1293268890434));
#162534=CARTESIAN_POINT('Ctrl Pts',(-20.7690040532235,-18.3640107463775,
6.124945890134));
#162535=CARTESIAN_POINT('Ctrl Pts',(-20.7867732913512,-18.4344955900524,
6.1205648912246));
#162536=CARTESIAN_POINT('Ctrl Pts',(-20.8045716030756,-18.5050957593199,
6.11617672423098));
#162537=CARTESIAN_POINT('Ctrl Pts',(-20.8186976575299,-18.5765123291963,
6.11178855723736));
#162538=CARTESIAN_POINT('Ctrl Pts',(-20.8291072241906,-18.648331234493,
6.10740039024374));
#162539=CARTESIAN_POINT('Ctrl Pts',(-20.8314491053219,-18.6644886159353,
6.10641316706544));
#162540=CARTESIAN_POINT('Ctrl Pts',(-20.8336030915946,-18.6806663528588,
6.10542594388715));
#162541=CARTESIAN_POINT('Ctrl Pts',(-20.8355690425741,-18.6968597262404,
6.10443872070886));
#162542=CARTESIAN_POINT('Ctrl Pts',(-20.8457798800574,-18.7809655384569,
6.09931124014674));
#162543=CARTESIAN_POINT('Ctrl Pts',(-20.8509432233709,-18.8656963446802,
6.09418375958462));
#162544=CARTESIAN_POINT('Ctrl Pts',(-20.8509995343428,-18.9505958660381,
6.0890562790225));
#162545=CARTESIAN_POINT('Origin',(-18.734,-18.952,0.));
#162546=CARTESIAN_POINT('',(-20.7225806193429,-18.2258897326344,7.15616144973347));
#162547=CARTESIAN_POINT('',(-20.7193262654686,-18.2270707613317,6.9336185967496));
#162548=CARTESIAN_POINT('',(-20.7225805737622,-18.2258896078036,0.));
#162549=CARTESIAN_POINT('Ctrl Pts',(-20.722580619343,-18.2258897326345,
7.15616144973347));
#162550=CARTESIAN_POINT('Ctrl Pts',(-20.7474159485307,-18.2939056477337,
7.15141143636792));
#162551=CARTESIAN_POINT('Ctrl Pts',(-20.7687705305159,-18.3632196853033,
7.14660731423374));
#162552=CARTESIAN_POINT('Ctrl Pts',(-20.8048202395505,-18.5059446662293,
7.13689825333913));
#162553=CARTESIAN_POINT('Ctrl Pts',(-20.8192617789026,-18.579244489578,
7.13200648739265));
#162554=CARTESIAN_POINT('Ctrl Pts',(-20.8346727925628,-18.6873232489186,
7.12505663315095));
#162555=CARTESIAN_POINT('Ctrl Pts',(-20.8387085643111,-18.7216043817949,
7.12289068190063));
#162556=CARTESIAN_POINT('Ctrl Pts',(-20.8425871760633,-18.7633111958887,
7.1203142244639));
#162557=CARTESIAN_POINT('Ctrl Pts',(-20.8432314561933,-18.7706549925183,
7.11986276020787));
#162558=CARTESIAN_POINT('Ctrl Pts',(-20.8441775336876,-18.7821267974974,
7.11916111919254));
#162559=CARTESIAN_POINT('Ctrl Pts',(-20.8445056016048,-18.786252496608,
7.11890950763311));
#162560=CARTESIAN_POINT('Ctrl Pts',(-20.8450939761029,-18.7939368625231,
7.11844224978327));
#162561=CARTESIAN_POINT('Ctrl Pts',(-20.8453573821261,-18.7974951891836,
7.11822643729257));
#162562=CARTESIAN_POINT('Ctrl Pts',(-20.8459354331439,-18.8055816661404,
7.11773724110973));
#162563=CARTESIAN_POINT('Ctrl Pts',(-20.8462445116671,-18.8101101621952,
7.11746417234176));
#162564=CARTESIAN_POINT('Ctrl Pts',(-20.8470081047971,-18.8218538747789,
7.11675823947325));
#162565=CARTESIAN_POINT('Ctrl Pts',(-20.8474402333973,-18.8290705564333,
7.11632659938544));
#162566=CARTESIAN_POINT('Ctrl Pts',(-20.8499256633052,-18.874475134017,
7.11362371524834));
#162567=CARTESIAN_POINT('Ctrl Pts',(-20.8509809806051,-18.9127131807723,
7.11140447444166));
#162568=CARTESIAN_POINT('Ctrl Pts',(-20.85107929024,-19.1130991834192,7.09997632154619));
#162569=CARTESIAN_POINT('Ctrl Pts',(-20.832532272912,-19.2747232960159,
7.09141467905363));
#162570=CARTESIAN_POINT('Ctrl Pts',(-20.7706268575478,-19.5402576310947,
7.07645440730754));
#162571=CARTESIAN_POINT('Ctrl Pts',(-20.7371602834163,-19.6457147998709,
7.07026714313349));
#162572=CARTESIAN_POINT('Ctrl Pts',(-20.6902873299116,-19.7612157374525,
7.06296374493082));
#162573=CARTESIAN_POINT('Ctrl Pts',(-20.6848211896208,-19.7743058424031,
7.06212830387132));
#162574=CARTESIAN_POINT('Ctrl Pts',(-20.6758998531024,-19.7950806194622,
7.06078962050351));
#162575=CARTESIAN_POINT('Ctrl Pts',(-20.6725295620061,-19.802801448336,
7.06028926503449));
#162576=CARTESIAN_POINT('Ctrl Pts',(-20.6664968922424,-19.8163994380094,
7.05940291807479));
#162577=CARTESIAN_POINT('Ctrl Pts',(-20.6638535463615,-19.8222849620273,
7.05901758266764));
#162578=CARTESIAN_POINT('Ctrl Pts',(-20.6583232650024,-19.8344492783238,
7.05821758675019));
#162579=CARTESIAN_POINT('Ctrl Pts',(-20.6554324100129,-19.840726194637,
7.05780279464393));
#162580=CARTESIAN_POINT('Ctrl Pts',(-20.6479172891203,-19.856835716409,
7.05673306750295));
#162581=CARTESIAN_POINT('Ctrl Pts',(-20.6432480051394,-19.8666469872364,
7.05607657953998));
#162582=CARTESIAN_POINT('Ctrl Pts',(-20.6233051551381,-19.9077334582909,
7.05330608146364));
#162583=CARTESIAN_POINT('Ctrl Pts',(-20.6073377344372,-19.9386640357421,
7.05116799924515));
#162584=CARTESIAN_POINT('Ctrl Pts',(-20.5636050720558,-20.0184869853972,
7.04550815445178));
#162585=CARTESIAN_POINT('Ctrl Pts',(-20.5346433172842,-20.0666891878495,
7.04194616612573));
#162586=CARTESIAN_POINT('Ctrl Pts',(-20.4347648079773,-20.2188525683532,
7.03023634280935));
#162587=CARTESIAN_POINT('Ctrl Pts',(-20.3564958450735,-20.3176569597721,
7.02187690373839));
#162588=CARTESIAN_POINT('Ctrl Pts',(-20.2011025010974,-20.4814773474229,
7.00699941111169));
#162589=CARTESIAN_POINT('Ctrl Pts',(-20.1272128747746,-20.5490764986592,
7.00047982678317));
#162590=CARTESIAN_POINT('Ctrl Pts',(-20.0412146205106,-20.6172245824404,
6.99370044053259));
#162591=CARTESIAN_POINT('Ctrl Pts',(-20.0335754764066,-20.6231931556124,
6.99310480878766));
#162592=CARTESIAN_POINT('Ctrl Pts',(-20.0222359687522,-20.631928101703,
6.99223065053106));
#162593=CARTESIAN_POINT('Ctrl Pts',(-20.0185672425278,-20.6347350767237,
6.99194935860015));
#162594=CARTESIAN_POINT('Ctrl Pts',(-20.0120424365153,-20.6396934898453,
6.99145183254905));
#162595=CARTESIAN_POINT('Ctrl Pts',(-20.0091900671574,-20.6418497206862,
6.9912352635893));
#162596=CARTESIAN_POINT('Ctrl Pts',(-20.0030671641756,-20.6464539595855,
6.99077237128944));
#162597=CARTESIAN_POINT('Ctrl Pts',(-19.9997950130008,-20.6488997242191,
6.99052620416663));
#162598=CARTESIAN_POINT('Ctrl Pts',(-19.9907938696364,-20.6555870922754,
6.98985228578299));
#162599=CARTESIAN_POINT('Ctrl Pts',(-19.9850504412018,-20.6598093010002,
6.98942586664614));
#162600=CARTESIAN_POINT('Ctrl Pts',(-19.9542778896278,-20.6821928073414,
6.98715963469539));
#162601=CARTESIAN_POINT('Ctrl Pts',(-19.9288730094435,-20.6998340873346,
6.9853535566624));
#162602=CARTESIAN_POINT('Ctrl Pts',(-19.8508165922211,-20.7515391271985,
6.97996808211128));
#162603=CARTESIAN_POINT('Ctrl Pts',(-19.7970274466996,-20.7838280943938,
6.9764754350482));
#162604=CARTESIAN_POINT('Ctrl Pts',(-19.6236648957386,-20.8776833345748,
6.96564106410738));
#162605=CARTESIAN_POINT('Ctrl Pts',(-19.4996237104855,-20.9302772723831,
6.95847231608247));
#162606=CARTESIAN_POINT('Ctrl Pts',(-19.3325235273573,-20.9830399688898,
6.94874727225968));
#162607=CARTESIAN_POINT('Ctrl Pts',(-19.2932700247087,-20.9941974835814,
6.94646003972938));
#162608=CARTESIAN_POINT('Ctrl Pts',(-19.2066105209316,-21.0161438746866,
6.94137929796329));
#162609=CARTESIAN_POINT('Ctrl Pts',(-19.1591071754183,-21.0264478774865,
6.93857399067379));
#162610=CARTESIAN_POINT('Ctrl Pts',(-19.0988926671266,-21.0373539690993,
6.93497497217654));
#162611=CARTESIAN_POINT('Ctrl Pts',(-19.0864718578771,-21.0394892608184,
6.93423032762956));
#162612=CARTESIAN_POINT('Ctrl Pts',(-19.0667599300631,-21.0426970431307,
6.9330447211818));
#162613=CARTESIAN_POINT('Ctrl Pts',(-19.0594808803921,-21.0438426067955,
6.93260608202739));
#162614=CARTESIAN_POINT('Ctrl Pts',(-19.0459068967655,-21.0459062910415,
6.93178650567151));
#162615=CARTESIAN_POINT('Ctrl Pts',(-19.0396135015102,-21.046834087521,
6.93140588011488));
#162616=CARTESIAN_POINT('Ctrl Pts',(-19.0256263817557,-21.048831750755,
6.93055847586553));
#162617=CARTESIAN_POINT('Ctrl Pts',(-19.0179307857528,-21.0498876623651,
6.93009126087912));
#162618=CARTESIAN_POINT('Ctrl Pts',(-18.9955533574643,-21.0528326837023,
6.92872975066363));
#162619=CARTESIAN_POINT('Ctrl Pts',(-18.9808575305314,-21.0546101554663,
6.92783194711667));
#162620=CARTESIAN_POINT('Ctrl Pts',(-18.8639365396358,-21.0675091868573,
6.92065857951775));
#162621=CARTESIAN_POINT('Ctrl Pts',(-18.7610580881093,-21.0713218368246,
6.91415219518838));
#162622=CARTESIAN_POINT('Ctrl Pts',(-18.5026308447506,-21.0620777466229,
6.89736605972563));
#162623=CARTESIAN_POINT('Ctrl Pts',(-18.3480413664539,-21.0393408915334,
6.88689581572453));
#162624=CARTESIAN_POINT('Ctrl Pts',(-18.1465345399949,-20.9865350700021,
6.8734399181643));
#162625=CARTESIAN_POINT('Ctrl Pts',(-18.0962268340151,-20.9713303349522,
6.87010209097466));
#162626=CARTESIAN_POINT('Ctrl Pts',(-18.0383148645933,-20.951446595531,
6.86632516179938));
#162627=CARTESIAN_POINT('Ctrl Pts',(-18.0301142028517,-20.948574387927,
6.86579189077599));
#162628=CARTESIAN_POINT('Ctrl Pts',(-18.0177156751048,-20.9441460299063,
6.86498826630709));
#162629=CARTESIAN_POINT('Ctrl Pts',(-18.0135047940447,-20.942626960937,
6.8647157940955));
#162630=CARTESIAN_POINT('Ctrl Pts',(-18.0059505413455,-20.9398746650922,
6.8642278528222));
#162631=CARTESIAN_POINT('Ctrl Pts',(-18.0026054525391,-20.9386463487209,
6.86401209794063));
#162632=CARTESIAN_POINT('Ctrl Pts',(-17.9953385797544,-20.9359571114531,
6.86354406999329));
#162633=CARTESIAN_POINT('Ctrl Pts',(-17.9914180340214,-20.9344930109192,
6.86329198980055));
#162634=CARTESIAN_POINT('Ctrl Pts',(-17.9804047731397,-20.9303429314,6.86258499645883));
#162635=CARTESIAN_POINT('Ctrl Pts',(-17.9733220304437,-20.9276304185608,
6.86213164126668));
#162636=CARTESIAN_POINT('Ctrl Pts',(-17.9308016347848,-20.9110836085839,
6.85941705979401));
#162637=CARTESIAN_POINT('Ctrl Pts',(-17.8957251652699,-20.89633328074,6.85720736574715));
#162638=CARTESIAN_POINT('Ctrl Pts',(-17.7810025906549,-20.8444079089298,
6.85001930078642));
#162639=CARTESIAN_POINT('Ctrl Pts',(-17.7032696104921,-20.8032182657645,
6.84521027761111));
#162640=CARTESIAN_POINT('Ctrl Pts',(-17.4797370737944,-20.6663133912096,
6.83095059804825));
#162641=CARTESIAN_POINT('Ctrl Pts',(-17.342976576592,-20.5573326669932,
6.82157759891172));
#162642=CARTESIAN_POINT('Ctrl Pts',(-17.2049681163796,-20.416337177459,
6.81011402251051));
#162643=CARTESIAN_POINT('Ctrl Pts',(-17.1890923458789,-20.3995780286448,
6.80876171758984));
#162644=CARTESIAN_POINT('Ctrl Pts',(-17.1670331032444,-20.3755150738235,
6.80683260898806));
#162645=CARTESIAN_POINT('Ctrl Pts',(-17.1606198708755,-20.3684234485663,
6.80626558163055));
#162646=CARTESIAN_POINT('Ctrl Pts',(-17.1502809925065,-20.3568340619956,
6.80534123164458));
#162647=CARTESIAN_POINT('Ctrl Pts',(-17.1463258988312,-20.3523626615249,
6.80498515058715));
#162648=CARTESIAN_POINT('Ctrl Pts',(-17.1380892593073,-20.3429710448187,
6.80423836051389));
#162649=CARTESIAN_POINT('Ctrl Pts',(-17.133811439374,-20.3380476574585,
6.8038475020388));
#162650=CARTESIAN_POINT('Ctrl Pts',(-17.123693571454,-20.3262936256549,
6.80291582507786));
#162651=CARTESIAN_POINT('Ctrl Pts',(-17.1178741681609,-20.319445448675,
6.80237416370403));
#162652=CARTESIAN_POINT('Ctrl Pts',(-17.0984378001158,-20.2962756799691,
6.80054525595321));
#162653=CARTESIAN_POINT('Ctrl Pts',(-17.0850234339455,-20.2797865213732,
6.79924982052421));
#162654=CARTESIAN_POINT('Ctrl Pts',(-17.0134816434154,-20.189089704933,
6.7921551194847));
#162655=CARTESIAN_POINT('Ctrl Pts',(-16.9601191198161,-20.1112742846567,
6.78617080228864));
#162656=CARTESIAN_POINT('Ctrl Pts',(-16.8276090706388,-19.8873609752444,
6.76927188331487));
#162657=CARTESIAN_POINT('Ctrl Pts',(-16.7601844296791,-19.7351188456599,
6.75808913236996));
#162658=CARTESIAN_POINT('Ctrl Pts',(-16.698839032824,-19.536442191861,6.74476022370512));
#162659=CARTESIAN_POINT('Ctrl Pts',(-16.6876443902823,-19.4959504574135,
6.74210928349517));
#162660=CARTESIAN_POINT('Ctrl Pts',(-16.6758934706876,-19.4479252253436,
6.73906266115482));
#162661=CARTESIAN_POINT('Ctrl Pts',(-16.6741638656779,-19.4406915372785,
6.73860635273242));
#162662=CARTESIAN_POINT('Ctrl Pts',(-16.6714258300277,-19.4289674733244,
6.73787112906865));
#162663=CARTESIAN_POINT('Ctrl Pts',(-16.6703938737201,-19.4244827338115,
6.73759091379964));
#162664=CARTESIAN_POINT('Ctrl Pts',(-16.6685864847603,-19.416509185568,
6.73709457584128));
#162665=CARTESIAN_POINT('Ctrl Pts',(-16.6678052557828,-19.4130217479148,
6.73687812427595));
#162666=CARTESIAN_POINT('Ctrl Pts',(-16.666147553022,-19.4055328397193,
6.73641468769454));
#162667=CARTESIAN_POINT('Ctrl Pts',(-16.665273862861,-19.4015308102332,
6.73616786306043));
#162668=CARTESIAN_POINT('Ctrl Pts',(-16.6629010393419,-19.3905084118941,
6.73549028719701));
#162669=CARTESIAN_POINT('Ctrl Pts',(-16.6614259736264,-19.3834828394061,
6.73506089228671));
#162670=CARTESIAN_POINT('Ctrl Pts',(-16.6536451994359,-19.3454631958638,
6.73274993296016));
#162671=CARTESIAN_POINT('Ctrl Pts',(-16.6479985872231,-19.3143364880446,
6.73090370057324));
#162672=CARTESIAN_POINT('Ctrl Pts',(-16.6174872737227,-19.1216487199776,
6.71969112518278));
#162673=CARTESIAN_POINT('Ctrl Pts',(-16.6107040475629,-18.9577698631849,
6.71105294674226));
#162674=CARTESIAN_POINT('Ctrl Pts',(-16.6315477823811,-18.6779717712427,
6.69569422906591));
#162675=CARTESIAN_POINT('Ctrl Pts',(-16.6499148071755,-18.5621533353466,
6.689158963228));
#162676=CARTESIAN_POINT('Ctrl Pts',(-16.6811576415342,-18.4345721822288,
6.68146401857769));
#162677=CARTESIAN_POINT('Ctrl Pts',(-16.6846978352459,-18.4207242543374,
6.6806223194999));
#162678=CARTESIAN_POINT('Ctrl Pts',(-16.6905550899693,-18.3987429188184,
6.6792754909367));
#162679=CARTESIAN_POINT('Ctrl Pts',(-16.6927811668969,-18.3905855626823,
6.67877330437085));
#162680=CARTESIAN_POINT('Ctrl Pts',(-16.6967932184971,-18.3762229406559,
6.67788482677648));
#162681=CARTESIAN_POINT('Ctrl Pts',(-16.6985588353912,-18.370012064851,
6.67749920208878));
#162682=CARTESIAN_POINT('Ctrl Pts',(-16.7022693175634,-18.357183210052,
6.67669969994454));
#162683=CARTESIAN_POINT('Ctrl Pts',(-16.7042181670829,-18.3505664720304,
6.67628569628896));
#162684=CARTESIAN_POINT('Ctrl Pts',(-16.7093033190877,-18.333607612024,
6.67522031226337));
#162685=CARTESIAN_POINT('Ctrl Pts',(-16.7124865134754,-18.3232798617662,
6.67456740309062));
#162686=CARTESIAN_POINT('Ctrl Pts',(-16.7260999477913,-18.2802840126132,
6.67183179590795));
#162687=CARTESIAN_POINT('Ctrl Pts',(-16.7372436301281,-18.2478489006737,
6.66972577622967));
#162688=CARTESIAN_POINT('Ctrl Pts',(-16.7683257651038,-18.1640613433321,
6.6641709888208));
#162689=CARTESIAN_POINT('Ctrl Pts',(-16.7894883502945,-18.1131936166144,
6.66068383030605));
#162690=CARTESIAN_POINT('Ctrl Pts',(-16.8585268527179,-17.963945438486,
6.65011415425016));
#162691=CARTESIAN_POINT('Ctrl Pts',(-16.9120657266473,-17.8683933463588,
6.64288324632428));
#162692=CARTESIAN_POINT('Ctrl Pts',(-16.9983229424886,-17.7390531414224,
6.63261364002144));
#162693=CARTESIAN_POINT('Ctrl Pts',(-17.0251521824694,-17.7015383797828,
6.62957356358089));
#162694=CARTESIAN_POINT('Ctrl Pts',(-17.0664521983726,-17.6476037828493,
6.62513720610868));
#162695=CARTESIAN_POINT('Ctrl Pts',(-17.0799861851478,-17.6304843897788,
6.62371888947913));
#162696=CARTESIAN_POINT('Ctrl Pts',(-17.126476016809,-17.5735118039761,
6.61897158594626));
#162697=CARTESIAN_POINT('Ctrl Pts',(-17.1606293566649,-17.5346542989865,
6.61568756123581));
#162698=CARTESIAN_POINT('Ctrl Pts',(-17.2021187341105,-17.4908006308627,
6.61196399656109));
#162699=CARTESIAN_POINT('Ctrl Pts',(-17.2081015151472,-17.4845540456529,
6.61143318642979));
#162700=CARTESIAN_POINT('Ctrl Pts',(-17.2172326532883,-17.475136506644,
6.61063252802957));
#162701=CARTESIAN_POINT('Ctrl Pts',(-17.2203529583771,-17.4719386511729,
6.61036058386553));
#162702=CARTESIAN_POINT('Ctrl Pts',(-17.2259797304643,-17.4662084394985,
6.60987320464635));
#162703=CARTESIAN_POINT('Ctrl Pts',(-17.2284824748074,-17.4636725237711,
6.60965748672217));
#162704=CARTESIAN_POINT('Ctrl Pts',(-17.2339435489004,-17.4581669392718,
6.60918909743202));
#162705=CARTESIAN_POINT('Ctrl Pts',(-17.2369042902398,-17.4551997440116,
6.6089366213376));
#162706=CARTESIAN_POINT('Ctrl Pts',(-17.2452686041947,-17.4468668432311,
6.60822739699985));
#162707=CARTESIAN_POINT('Ctrl Pts',(-17.2506924063789,-17.4415214085732,
6.60777222252185));
#162708=CARTESIAN_POINT('Ctrl Pts',(-17.2837761102591,-17.4092657771348,
6.60502337312307));
#162709=CARTESIAN_POINT('Ctrl Pts',(-17.312140628635,-17.3830849088749,
6.6027827550018));
#162710=CARTESIAN_POINT('Ctrl Pts',(-17.4090490661397,-17.2984253421442,
6.59544164085161));
#162711=CARTESIAN_POINT('Ctrl Pts',(-17.4806105560092,-17.2435440871131,
6.59051881974452));
#162712=CARTESIAN_POINT('Ctrl Pts',(-17.6976217286544,-17.0981129854688,
6.5763138038528));
#162713=CARTESIAN_POINT('Ctrl Pts',(-17.8507966505464,-17.0204405360757,
6.56709270672974));
#162714=CARTESIAN_POINT('Ctrl Pts',(-18.0335325100814,-16.9541069793512,
6.55579954157498));
#162715=CARTESIAN_POINT('Ctrl Pts',(-18.0555496922783,-16.9465234124758,
6.55443559976432));
#162716=CARTESIAN_POINT('Ctrl Pts',(-18.0868088812237,-16.9363302068524,
6.55249271091416));
#162717=CARTESIAN_POINT('Ctrl Pts',(-18.0959508973042,-16.9334177259339,
6.55192373319032));
#162718=CARTESIAN_POINT('Ctrl Pts',(-18.1108182146862,-16.9287923558517,
6.55099706933841));
#162719=CARTESIAN_POINT('Ctrl Pts',(-18.1165315909493,-16.9270413654635,
6.55064063732268));
#162720=CARTESIAN_POINT('Ctrl Pts',(-18.128491341023,-16.9234313576681,
6.54989381294908));
#162721=CARTESIAN_POINT('Ctrl Pts',(-18.1347390306244,-16.9215769500281,
6.54950327423074));
#162722=CARTESIAN_POINT('Ctrl Pts',(-18.1495948171405,-16.9172420699767,
6.54857364889595));
#162723=CARTESIAN_POINT('Ctrl Pts',(-18.1582102405747,-16.9147873452604,
6.54803372924014));
#162724=CARTESIAN_POINT('Ctrl Pts',(-18.1871582354442,-16.9067377189396,
6.54621678123807));
#162725=CARTESIAN_POINT('Ctrl Pts',(-18.2075582674424,-16.9013920985435,
6.54493170895828));
#162726=CARTESIAN_POINT('Ctrl Pts',(-18.318213348977,-16.8741560662726,
6.53793396240243));
#162727=CARTESIAN_POINT('Ctrl Pts',(-18.4097434897625,-16.8579207924823,
6.53204185130024));
#162728=CARTESIAN_POINT('Ctrl Pts',(-18.6541350599363,-16.8309798409634,
6.51608371700417));
#162729=CARTESIAN_POINT('Ctrl Pts',(-18.8075946250902,-16.8307538985654,
6.50580706520825));
#162730=CARTESIAN_POINT('Ctrl Pts',(-18.9632351482536,-16.8474447845651,
6.49567693293862));
#162731=CARTESIAN_POINT('Ctrl Pts',(-18.9667366381847,-16.8478291263617,
6.4954492078278));
#162732=CARTESIAN_POINT('Ctrl Pts',(-19.0220450172929,-16.8540398083499,
6.49185506141242));
#162733=CARTESIAN_POINT('Ctrl Pts',(-19.0736251474451,-16.8617697178967,
6.48854338203455));
#162734=CARTESIAN_POINT('Ctrl Pts',(-19.133389701869,-16.8729973576294,
6.48479253461922));
#162735=CARTESIAN_POINT('Ctrl Pts',(-19.1418981825888,-16.8746499574007,
6.48426060598984));
#162736=CARTESIAN_POINT('Ctrl Pts',(-19.1547808663651,-16.8772343603836,
6.48345859933204));
#162737=CARTESIAN_POINT('Ctrl Pts',(-19.1591625423258,-16.8781278220961,
6.4831864150276));
#162738=CARTESIAN_POINT('Ctrl Pts',(-19.1670304680933,-16.8797581439452,
6.48269878038706));
#162739=CARTESIAN_POINT('Ctrl Pts',(-19.1705177009885,-16.8804899243351,
6.48248304583965));
#162740=CARTESIAN_POINT('Ctrl Pts',(-19.1781002693348,-16.8821010906249,
6.4820148217156));
#162741=CARTESIAN_POINT('Ctrl Pts',(-19.1821948343801,-16.8829838242807,
6.48176252631655));
#162742=CARTESIAN_POINT('Ctrl Pts',(-19.193712245762,-16.8855026190406,
6.48105432052355));
#162743=CARTESIAN_POINT('Ctrl Pts',(-19.2011290262645,-16.8871665318466,
6.48059997666856));
#162744=CARTESIAN_POINT('Ctrl Pts',(-19.2459000188025,-16.8974642290223,
6.47786684434423));
#162745=CARTESIAN_POINT('Ctrl Pts',(-19.2830255556427,-16.9070720752472,
6.47564041051448));
#162746=CARTESIAN_POINT('Ctrl Pts',(-19.4054604833123,-16.9423326758004,
6.4683698059703));
#162747=CARTESIAN_POINT('Ctrl Pts',(-19.4894150684498,-16.9723605058998,
6.46349944852714));
#162748=CARTESIAN_POINT('Ctrl Pts',(-19.7296489574193,-17.0758016402394,
6.44927415173421));
#162749=CARTESIAN_POINT('Ctrl Pts',(-19.8791157218193,-17.1631064012878,
6.43998766499431));
#162750=CARTESIAN_POINT('Ctrl Pts',(-20.034837646509,-17.2816553579202,
6.42861811600396));
#162751=CARTESIAN_POINT('Ctrl Pts',(-20.053107179289,-17.2960452927523,
6.42725593427173));
#162752=CARTESIAN_POINT('Ctrl Pts',(-20.0785701367534,-17.3167898882346,
6.42531513063309));
#162753=CARTESIAN_POINT('Ctrl Pts',(-20.0859634964498,-17.3228972831839,
6.42474644874198));
#162754=CARTESIAN_POINT('Ctrl Pts',(-20.0978954230114,-17.3328909941076,
6.42382013596474));
#162755=CARTESIAN_POINT('Ctrl Pts',(-20.1024595334296,-17.3367467065156,
6.42346375728607));
#162756=CARTESIAN_POINT('Ctrl Pts',(-20.1116179597681,-17.3445503273064,
6.42274446087752));
#162757=CARTESIAN_POINT('Ctrl Pts',(-20.1162117738043,-17.3484987357373,
6.42238152439874));
#162758=CARTESIAN_POINT('Ctrl Pts',(-20.1272067033567,-17.3580312931585,
6.42150766455482));
#162759=CARTESIAN_POINT('Ctrl Pts',(-20.1335912406369,-17.363634326575,
6.42099595856163));
#162760=CARTESIAN_POINT('Ctrl Pts',(-20.1538565176832,-17.3816360707754,
6.41935791814395));
#162761=CARTESIAN_POINT('Ctrl Pts',(-20.1676072518525,-17.3941792100084,
6.41822552815957));
#162762=CARTESIAN_POINT('Ctrl Pts',(-20.1994325006941,-17.423987797385,
6.41555440128884));
#162763=CARTESIAN_POINT('Ctrl Pts',(-20.2173698622435,-17.4413949973026,
6.41400970227844));
#162764=CARTESIAN_POINT('Ctrl Pts',(-20.2794071962141,-17.5037693195756,
6.40852584072723));
#162765=CARTESIAN_POINT('Ctrl Pts',(-20.3218016500598,-17.5503794252057,
6.40451740357261));
#162766=CARTESIAN_POINT('Ctrl Pts',(-20.4216783127836,-17.6705429157315,
6.39441378287514));
#162767=CARTESIAN_POINT('Ctrl Pts',(-20.4764941116557,-17.74613819415,6.38825018154735));
#162768=CARTESIAN_POINT('Ctrl Pts',(-20.5913660343305,-17.9288219018111,
6.37399161457688));
#162769=CARTESIAN_POINT('Ctrl Pts',(-20.6474684169153,-18.0380265199528,
6.3659192469899));
#162770=CARTESIAN_POINT('Ctrl Pts',(-20.6973852263465,-18.1602318655953,
6.35776677957427));
#162771=CARTESIAN_POINT('Ctrl Pts',(-20.7009005364253,-18.1690053556247,
6.35718624725605));
#162772=CARTESIAN_POINT('Ctrl Pts',(-20.7060289959388,-18.1820574430397,
6.35632996090637));
#162773=CARTESIAN_POINT('Ctrl Pts',(-20.7076871756968,-18.1863180586969,
6.35605159884923));
#162774=CARTESIAN_POINT('Ctrl Pts',(-20.7106159147882,-18.1939160487537,
6.3555572949701));
#162775=CARTESIAN_POINT('Ctrl Pts',(-20.7118918421534,-18.1972512914062,
6.3553410345474));
#162776=CARTESIAN_POINT('Ctrl Pts',(-20.7146202937716,-18.2044378330701,
6.35487661086278));
#162777=CARTESIAN_POINT('Ctrl Pts',(-20.7160700229184,-18.2082901328902,
6.35462861533865));
#162778=CARTESIAN_POINT('Ctrl Pts',(-20.719215033876,-18.2167217446924,
6.35408785900432));
#162779=CARTESIAN_POINT('Ctrl Pts',(-20.7209057282952,-18.2213027499434,
6.35379536866914));
#162780=CARTESIAN_POINT('Ctrl Pts',(-20.7225805737622,-18.2258896078036,
6.35350377396603));
#162781=CARTESIAN_POINT('',(-20.8509992748742,-18.9537521935255,6.8890562790225));
#162782=CARTESIAN_POINT('Ctrl Pts',(-20.8509992748742,-18.9537521935255,
6.8890562790225));
#162783=CARTESIAN_POINT('Ctrl Pts',(-20.8509006165464,-19.0729511321296,
6.88186870628082));
#162784=CARTESIAN_POINT('Ctrl Pts',(-20.8407310772906,-19.1917453566805,
6.87468113353914));
#162785=CARTESIAN_POINT('Ctrl Pts',(-20.8207141748805,-19.3088094062,6.86749356079746));
#162786=CARTESIAN_POINT('Ctrl Pts',(-20.8084933107471,-19.3802801969732,
6.86310535186656));
#162787=CARTESIAN_POINT('Ctrl Pts',(-20.7925724893355,-19.4512619171912,
6.85871714293567));
#162788=CARTESIAN_POINT('Ctrl Pts',(-20.7730042905686,-19.5213421669286,
6.85432893400477));
#162789=CARTESIAN_POINT('Ctrl Pts',(-20.7534651342531,-19.5913184059558,
6.8499472379035));
#162790=CARTESIAN_POINT('Ctrl Pts',(-20.7302894754046,-19.6603953697141,
6.84556554180223));
#162791=CARTESIAN_POINT('Ctrl Pts',(-20.7035811449958,-19.7281695132359,
6.84118384570097));
#162792=CARTESIAN_POINT('Ctrl Pts',(-20.6769041990008,-19.7958640167455,
6.83680729844133));
#162793=CARTESIAN_POINT('Ctrl Pts',(-20.6467030037517,-19.8622582946366,
6.83243075118168));
#162794=CARTESIAN_POINT('Ctrl Pts',(-20.6131310722287,-19.9269643139032,
6.82805420392204));
#162795=CARTESIAN_POINT('Ctrl Pts',(-20.5795804315367,-19.9916292975527,
6.82368043220507));
#162796=CARTESIAN_POINT('Ctrl Pts',(-20.5426635175973,-20.0546077198003,
6.81930666048809));
#162797=CARTESIAN_POINT('Ctrl Pts',(-20.5025812162808,-20.1155331887912,
6.81493288877111));
#162798=CARTESIAN_POINT('Ctrl Pts',(-20.4625111121433,-20.1764401179573,
6.81056044800756));
#162799=CARTESIAN_POINT('Ctrl Pts',(-20.4192777979153,-20.2352949313846,
6.806188007244));
#162800=CARTESIAN_POINT('Ctrl Pts',(-20.3731263263947,-20.2917588910397,
6.80181556648045));
#162801=CARTESIAN_POINT('Ctrl Pts',(-20.3269736747759,-20.3482242944844,
6.7974430139131));
#162802=CARTESIAN_POINT('Ctrl Pts',(-20.2779030245428,-20.4022983505562,
6.79307046134575));
#162803=CARTESIAN_POINT('Ctrl Pts',(-20.2261996115101,-20.4536755040318,
6.78869790877841));
#162804=CARTESIAN_POINT('Ctrl Pts',(-20.1744425387252,-20.5051059786551,
6.78432081821108));
#162805=CARTESIAN_POINT('Ctrl Pts',(-20.1200475906613,-20.5538336216567,
6.77994372764375));
#162806=CARTESIAN_POINT('Ctrl Pts',(-20.063336165121,-20.5995904709914,
6.77556663707642));
#162807=CARTESIAN_POINT('Ctrl Pts',(-20.0065937673663,-20.6453723098397,
6.77118715601747));
#162808=CARTESIAN_POINT('Ctrl Pts',(-19.9475327641504,-20.6881798414322,
6.76680767495853));
#162809=CARTESIAN_POINT('Ctrl Pts',(-19.8865046696906,-20.7277877086919,
6.76242819389958));
#162810=CARTESIAN_POINT('Ctrl Pts',(-19.8253684033431,-20.7674657806304,
6.75804095023986));
#162811=CARTESIAN_POINT('Ctrl Pts',(-19.7622585010735,-20.8039326211616,
6.75365370658014));
#162812=CARTESIAN_POINT('Ctrl Pts',(-19.6975517419863,-20.8370084987912,
6.74926646292041));
#162813=CARTESIAN_POINT('Ctrl Pts',(-19.6535573809358,-20.8594969083952,
6.74628355998562));
#162814=CARTESIAN_POINT('Ctrl Pts',(-19.6088253272205,-20.8804187619502,
6.74330065705082));
#162815=CARTESIAN_POINT('Ctrl Pts',(-19.5634785608968,-20.8997305555473,
6.74031775411602));
#162816=CARTESIAN_POINT('Ctrl Pts',(-19.4967680143858,-20.9281405262996,
6.73592954518512));
#162817=CARTESIAN_POINT('Ctrl Pts',(-19.4284659821153,-20.9531746938963,
6.73154133625421));
#162818=CARTESIAN_POINT('Ctrl Pts',(-19.3589476876738,-20.9746540454737,
6.72715312732331));
#162819=CARTESIAN_POINT('Ctrl Pts',(-19.2895325699076,-20.996101518132,
6.72277143122204));
#162820=CARTESIAN_POINT('Ctrl Pts',(-19.2189052304798,-21.014004507002,
6.71838973512076));
#162821=CARTESIAN_POINT('Ctrl Pts',(-19.1474611885819,-21.0282318862633,
6.71400803901949));
#162822=CARTESIAN_POINT('Ctrl Pts',(-19.0761010991189,-21.0424425472217,
6.70963149175985));
#162823=CARTESIAN_POINT('Ctrl Pts',(-19.0039266843573,-21.0529860848153,
6.70525494450021));
#162824=CARTESIAN_POINT('Ctrl Pts',(-18.9313473123123,-21.05978154426,6.70087839724056));
#162825=CARTESIAN_POINT('Ctrl Pts',(-18.8588139690502,-21.0665726941231,
6.69650462552358));
#162826=CARTESIAN_POINT('Ctrl Pts',(-18.7858766571606,-21.0696204372107,
6.6921308538066));
#162827=CARTESIAN_POINT('Ctrl Pts',(-18.7129521899221,-21.0688953657871,
6.68775708208963));
#162828=CARTESIAN_POINT('Ctrl Pts',(-18.6400499138438,-21.0681705150052,
6.68338464132607));
#162829=CARTESIAN_POINT('Ctrl Pts',(-18.5671609567207,-21.0636751337981,
6.67901220056251));
#162830=CARTESIAN_POINT('Ctrl Pts',(-18.4947027860638,-21.0554319203156,
6.67463975979895));
#162831=CARTESIAN_POINT('Ctrl Pts',(-18.4222427626436,-21.0471884960532,
6.67026720723161));
#162832=CARTESIAN_POINT('Ctrl Pts',(-18.3502140266194,-21.0351971057619,
6.66589465466426));
#162833=CARTESIAN_POINT('Ctrl Pts',(-18.2790278943154,-21.0195321963754,
6.66152210209691));
#162834=CARTESIAN_POINT('Ctrl Pts',(-18.2077678823583,-21.0038510293551,
6.65714501152958));
#162835=CARTESIAN_POINT('Ctrl Pts',(-18.1373526922054,-20.9844888351844,
6.65276792096224));
#162836=CARTESIAN_POINT('Ctrl Pts',(-18.0681816040656,-20.9615708157802,
6.64839083039491));
#162837=CARTESIAN_POINT('Ctrl Pts',(-17.9989727390273,-20.9386402799949,
6.64401134933596));
#162838=CARTESIAN_POINT('Ctrl Pts',(-17.9310097785365,-20.9121502278387,
6.63963186827702));
#162839=CARTESIAN_POINT('Ctrl Pts',(-17.8646724802103,-20.8822742456284,
6.63525238721807));
#162840=CARTESIAN_POINT('Ctrl Pts',(-17.798217599468,-20.8523453084401,
6.63086514355835));
#162841=CARTESIAN_POINT('Ctrl Pts',(-17.7333945644594,-20.8190186771211,
6.62647789989862));
#162842=CARTESIAN_POINT('Ctrl Pts',(-17.6705584443108,-20.7825138780226,
6.62209065623889));
#162843=CARTESIAN_POINT('Ctrl Pts',(-17.6278359374846,-20.7576941322301,
6.61910775330412));
#162844=CARTESIAN_POINT('Ctrl Pts',(-17.5860313573348,-20.7314061565717,
6.61612485036935));
#162845=CARTESIAN_POINT('Ctrl Pts',(-17.5452478505361,-20.7037298099721,
6.61314194743458));
#162846=CARTESIAN_POINT('Ctrl Pts',(-17.485250407548,-20.6630145758599,
6.60875373850369));
#162847=CARTESIAN_POINT('Ctrl Pts',(-17.4272300397248,-20.6191338958609,
6.60436552957279));
#162848=CARTESIAN_POINT('Ctrl Pts',(-17.3715403699669,-20.5723063773651,
6.5999773206419));
#162849=CARTESIAN_POINT('Ctrl Pts',(-17.3159333529124,-20.5255483586709,
6.59559562454064));
#162850=CARTESIAN_POINT('Ctrl Pts',(-17.2626505332034,-20.4758524915492,
6.59121392843937));
#162851=CARTESIAN_POINT('Ctrl Pts',(-17.2120162539404,-20.4234803691285,
6.58683223233811));
#162852=CARTESIAN_POINT('Ctrl Pts',(-17.1614414739852,-20.3711697881195,
6.58245568507847));
#162853=CARTESIAN_POINT('Ctrl Pts',(-17.1135093856056,-20.3161895440793,
6.57807913781884));
#162854=CARTESIAN_POINT('Ctrl Pts',(-17.0685096421061,-20.2588400314356,
6.5737025905592));
#162855=CARTESIAN_POINT('Ctrl Pts',(-17.0235384367899,-20.2015268890193,
6.56932881884223));
#162856=CARTESIAN_POINT('Ctrl Pts',(-16.9814961836088,-20.1418478378284,
6.56495504712526));
#162857=CARTESIAN_POINT('Ctrl Pts',(-16.9426332229367,-20.0801374340185,
6.56058127540829));
#162858=CARTESIAN_POINT('Ctrl Pts',(-16.9037820883941,-20.0184458088918,
6.55620883464474));
#162859=CARTESIAN_POINT('Ctrl Pts',(-16.8681085825374,-19.9547244662931,
6.55183639388119));
#162860=CARTESIAN_POINT('Ctrl Pts',(-16.8358195870607,-19.8893367164118,
6.54746395311764));
#162861=CARTESIAN_POINT('Ctrl Pts',(-16.8035297659509,-19.8239472945585,
6.5430914005503));
#162862=CARTESIAN_POINT('Ctrl Pts',(-16.7746248388303,-19.7568918142269,
6.53871884798296));
#162863=CARTESIAN_POINT('Ctrl Pts',(-16.7492648453343,-19.6885564240667,
6.53434629541562));
#162864=CARTESIAN_POINT('Ctrl Pts',(-16.7238785322805,-19.6201501128611,
6.5299692048483));
#162865=CARTESIAN_POINT('Ctrl Pts',(-16.7020446665442,-19.5504616929165,
6.52559211428097));
#162866=CARTESIAN_POINT('Ctrl Pts',(-16.6838740959313,-19.4798946651242,
6.52121502371365));
#162867=CARTESIAN_POINT('Ctrl Pts',(-16.6656936016954,-19.4092890980589,
6.51683554265471));
#162868=CARTESIAN_POINT('Ctrl Pts',(-16.6511804819229,-19.3378044408494,
6.51245606159577));
#162869=CARTESIAN_POINT('Ctrl Pts',(-16.6403943335874,-19.2658539685346,
6.50807658053683));
#162870=CARTESIAN_POINT('Ctrl Pts',(-16.6295890668764,-19.1937759644906,
6.50368933687712));
#162871=CARTESIAN_POINT('Ctrl Pts',(-16.6225240103777,-19.1212309770727,
6.4993020932174));
#162872=CARTESIAN_POINT('Ctrl Pts',(-16.6192067693546,-19.0486363886758,
6.49491484955768));
#162873=CARTESIAN_POINT('Ctrl Pts',(-16.6169513651074,-18.9992790637633,
6.49193194662284));
#162874=CARTESIAN_POINT('Ctrl Pts',(-16.6164273661252,-18.9498988449414,
6.488949043688));
#162875=CARTESIAN_POINT('Ctrl Pts',(-16.6176234550289,-18.9006256883613,
6.48596614075315));
#162876=CARTESIAN_POINT('Ctrl Pts',(-16.6193830456439,-18.8281389496101,
6.48157793182226));
#162877=CARTESIAN_POINT('Ctrl Pts',(-16.6248744285954,-18.7556012223724,
6.47718972289136));
#162878=CARTESIAN_POINT('Ctrl Pts',(-16.6341051990332,-18.6834281755797,
6.47280151396046));
#162879=CARTESIAN_POINT('Ctrl Pts',(-16.6433222694771,-18.6113622455548,
6.46841981785919));
#162880=CARTESIAN_POINT('Ctrl Pts',(-16.656267649465,-18.5396603960522,
6.46403812175793));
#162881=CARTESIAN_POINT('Ctrl Pts',(-16.6728969413429,-18.4687369436899,
6.45965642565666));
#162882=CARTESIAN_POINT('Ctrl Pts',(-16.6895066924793,-18.3978968320285,
6.45527987839702));
#162883=CARTESIAN_POINT('Ctrl Pts',(-16.709791646569,-18.3278337678025,
6.45090333113738));
#162884=CARTESIAN_POINT('Ctrl Pts',(-16.7336560032766,-18.2589539014086,
6.44652678387774));
#162885=CARTESIAN_POINT('Ctrl Pts',(-16.757505225556,-18.190117717625,6.44215301216076));
#162886=CARTESIAN_POINT('Ctrl Pts',(-16.7849291889405,-18.1224636975235,
6.43777924044379));
#162887=CARTESIAN_POINT('Ctrl Pts',(-16.815782089144,-18.0563834266432,
6.43340546872682));
#162888=CARTESIAN_POINT('Ctrl Pts',(-16.8466256007064,-17.9903232642113,
6.42903302796327));
#162889=CARTESIAN_POINT('Ctrl Pts',(-16.8808957735922,-17.9258363370627,
6.42466058719971));
#162890=CARTESIAN_POINT('Ctrl Pts',(-16.9183991025644,-17.8632932528771,
6.42028814643616));
#162891=CARTESIAN_POINT('Ctrl Pts',(-16.9559033905008,-17.8007485694579,
6.41591559386882));
#162892=CARTESIAN_POINT('Ctrl Pts',(-16.9966407488748,-17.7401482403576,
6.41154304130147));
#162893=CARTESIAN_POINT('Ctrl Pts',(-17.0403731142006,-17.6818358485229,
6.40717048873412));
#162894=CARTESIAN_POINT('Ctrl Pts',(-17.0841508666247,-17.6234629378885,
6.4027933981668));
#162895=CARTESIAN_POINT('Ctrl Pts',(-17.1309295419555,-17.5673830921179,
6.39841630759947));
#162896=CARTESIAN_POINT('Ctrl Pts',(-17.1804298596141,-17.5139079240531,
6.39403921703214));
#162897=CARTESIAN_POINT('Ctrl Pts',(-17.2299572112332,-17.4604035512143,
6.3896597359732));
#162898=CARTESIAN_POINT('Ctrl Pts',(-17.2822088187845,-17.4095070251029,
6.38528025491426));
#162899=CARTESIAN_POINT('Ctrl Pts',(-17.3368694420737,-17.3614921552823,
6.38090077385531));
#162900=CARTESIAN_POINT('Ctrl Pts',(-17.3916269509507,-17.3133921794274,
6.37651353019559));
#162901=CARTESIAN_POINT('Ctrl Pts',(-17.4488016237927,-17.2681843592166,
6.37212628653587));
#162902=CARTESIAN_POINT('Ctrl Pts',(-17.5080466246426,-17.226101010647,
6.36773904287615));
#162903=CARTESIAN_POINT('Ctrl Pts',(-17.5483275163857,-17.1974883887615,
6.36475613994134));
#162904=CARTESIAN_POINT('Ctrl Pts',(-17.5895648351148,-17.170319212664,
6.36177323700653));
#162905=CARTESIAN_POINT('Ctrl Pts',(-17.6316431823901,-17.1446543090297,
6.35879033407172));
#162906=CARTESIAN_POINT('Ctrl Pts',(-17.6935454914313,-17.1068981494094,
6.35440212514083));
#162907=CARTESIAN_POINT('Ctrl Pts',(-17.7575106221333,-17.0722522374745,
6.35001391620993));
#162908=CARTESIAN_POINT('Ctrl Pts',(-17.8231931738163,-17.0409479532527,
6.34562570727903));
#162909=CARTESIAN_POINT('Ctrl Pts',(-17.8887782417022,-17.009690129779,
6.34124401117776));
#162910=CARTESIAN_POINT('Ctrl Pts',(-17.9560752387291,-16.9817642944955,
6.33686231507649));
#162911=CARTESIAN_POINT('Ctrl Pts',(-18.0247117585802,-16.9573573777281,
6.33248061897523));
#162912=CARTESIAN_POINT('Ctrl Pts',(-18.093267625058,-16.9329791410304,
6.32810407171559));
#162913=CARTESIAN_POINT('Ctrl Pts',(-18.1631594352659,-16.9121117694419,
6.32372752445595));
#162914=CARTESIAN_POINT('Ctrl Pts',(-18.2339938260905,-16.8948945515476,
6.31935097719631));
#162915=CARTESIAN_POINT('Ctrl Pts',(-18.3047832947738,-16.8776882525628,
6.31497720547934));
#162916=CARTESIAN_POINT('Ctrl Pts',(-18.3765136904417,-16.8641276279119,
6.31060343376236));
#162917=CARTESIAN_POINT('Ctrl Pts',(-18.4487768305311,-16.8543020370897,
6.30622966204539));
#162918=CARTESIAN_POINT('Ctrl Pts',(-18.5210179807043,-16.8444794362278,
6.30185722128184));
#162919=CARTESIAN_POINT('Ctrl Pts',(-18.5937910757566,-16.838389677678,
6.29748478051829));
#162920=CARTESIAN_POINT('Ctrl Pts',(-18.6666797525648,-16.8360706570669,
6.29311233975473));
#162921=CARTESIAN_POINT('Ctrl Pts',(-18.7395702931445,-16.8337515771582,
6.28873978718739));
#162922=CARTESIAN_POINT('Ctrl Pts',(-18.8125759391505,-16.8352034399581,
6.28436723462004));
#162923=CARTESIAN_POINT('Ctrl Pts',(-18.8852789324484,-16.8404120466821,
6.2799946820527));
#162924=CARTESIAN_POINT('Ctrl Pts',(-18.958057379655,-16.8456260590946,
6.27561759148537));
#162925=CARTESIAN_POINT('Ctrl Pts',(-19.0305320648488,-16.8546045652848,
6.27124050091805));
#162926=CARTESIAN_POINT('Ctrl Pts',(-19.1022898016633,-16.8672814046038,
6.26686341035072));
#162927=CARTESIAN_POINT('Ctrl Pts',(-19.1740867280411,-16.8799651672152,
6.26248392929178));
#162928=CARTESIAN_POINT('Ctrl Pts',(-19.2451654560883,-16.8963511759145,
6.25810444823283));
#162929=CARTESIAN_POINT('Ctrl Pts',(-19.3151251217552,-16.9163225715097,
6.25372496717389));
#162930=CARTESIAN_POINT('Ctrl Pts',(-19.3852087904599,-16.9363293662695,
6.24933772351417));
#162931=CARTESIAN_POINT('Ctrl Pts',(-19.4541689789704,-16.9599340823955,
6.24495047985445));
#162932=CARTESIAN_POINT('Ctrl Pts',(-19.5216226105729,-16.9869708339787,
6.24056323619473));
#162933=CARTESIAN_POINT('Ctrl Pts',(-19.5674845802461,-17.0053532198001,
6.23758033325991));
#162934=CARTESIAN_POINT('Ctrl Pts',(-19.6126505362293,-17.0253211191867,
6.2345974303251));
#162935=CARTESIAN_POINT('Ctrl Pts',(-19.6570068699279,-17.0468104246386,
6.23161452739028));
#162936=CARTESIAN_POINT('Ctrl Pts',(-19.7222419452882,-17.0784148505164,
6.22722755755938));
#162937=CARTESIAN_POINT('Ctrl Pts',(-19.7859792078952,-17.1134353687254,
6.22284058772849));
#162938=CARTESIAN_POINT('Ctrl Pts',(-19.847837465415,-17.1517069403462,
6.21845361789759));
#162939=CARTESIAN_POINT('Ctrl Pts',(-19.9096117325667,-17.1899265473058,
6.21407260463944));
#162940=CARTESIAN_POINT('Ctrl Pts',(-19.9695116495773,-17.2313881992686,
6.2096915913813));
#162941=CARTESIAN_POINT('Ctrl Pts',(-20.0271786200073,-17.2758800589588,
6.20531057812316));
#162942=CARTESIAN_POINT('Ctrl Pts',(-20.0847863205803,-17.3203261901124,
6.20093406765105));
#162943=CARTESIAN_POINT('Ctrl Pts',(-20.1401652493144,-17.367796055159,
6.19655755717894));
#162944=CARTESIAN_POINT('Ctrl Pts',(-20.1929853613491,-17.4180343174083,
6.19218104670683));
#162945=CARTESIAN_POINT('Ctrl Pts',(-20.2457686121952,-17.4682375202457,
6.18780759043834));
#162946=CARTESIAN_POINT('Ctrl Pts',(-20.2959962435542,-17.521204952502,
6.18343413416985));
#162947=CARTESIAN_POINT('Ctrl Pts',(-20.3433722233308,-17.5766418478188,
6.17906067790137));
#162948=CARTESIAN_POINT('Ctrl Pts',(-20.3907430256997,-17.6320726848037,
6.17468769957901));
#162949=CARTESIAN_POINT('Ctrl Pts',(-20.4352624726777,-17.6899720904887,
6.17031472125666));
#162950=CARTESIAN_POINT('Ctrl Pts',(-20.4766732169276,-17.7500103748355,
6.1659417429343));
#162951=CARTESIAN_POINT('Ctrl Pts',(-20.5180810237586,-17.8100444004421,
6.16156907480366));
#162952=CARTESIAN_POINT('Ctrl Pts',(-20.5563802984018,-17.872216601689,
6.15719640667301));
#162953=CARTESIAN_POINT('Ctrl Pts',(-20.5913568209674,-17.9361680062108,
6.15282373854237));
#162954=CARTESIAN_POINT('Ctrl Pts',(-20.6263573793841,-18.0001633581098,
6.1484480655161));
#162955=CARTESIAN_POINT('Ctrl Pts',(-20.6580304037707,-18.0659399262137,
6.14407239248983));
#162956=CARTESIAN_POINT('Ctrl Pts',(-20.6862080122609,-18.1331148573429,
6.13969671946356));
#162957=CARTESIAN_POINT('Ctrl Pts',(-20.6990632498902,-18.1637615214382,
6.13770044229331));
#162958=CARTESIAN_POINT('Ctrl Pts',(-20.7111916196051,-18.1946989607123,
6.13570416512306));
#162959=CARTESIAN_POINT('Ctrl Pts',(-20.7225805737622,-18.2258896078036,
6.13370788795281));
#162960=CARTESIAN_POINT('Ctrl Pts',(-20.7193262654686,-18.2270707613317,
6.9336185967496));
#162961=CARTESIAN_POINT('Ctrl Pts',(-20.8041091853424,-18.460047360634,
6.91876474672015));
#162962=CARTESIAN_POINT('Ctrl Pts',(-20.8501556708863,-18.707244192998,
6.90391089669071));
#162963=CARTESIAN_POINT('Ctrl Pts',(-20.8523539331563,-18.9537405760439,
6.88905704666127));
#162964=CARTESIAN_POINT('Origin',(-18.734,-18.952,0.));
#162965=CARTESIAN_POINT('',(-20.7225806049454,-18.2258896932043,7.9573447159704));
#162966=CARTESIAN_POINT('',(-20.7225805631882,-18.2258895788448,7.73405224475123));
#162967=CARTESIAN_POINT('',(-20.7225805737622,-18.2258896078036,0.));
#162968=CARTESIAN_POINT('',(-20.8509992001554,-18.9539106864308,7.91072959189229));
#162969=CARTESIAN_POINT('Ctrl Pts',(-20.7225806049454,-18.2258896932043,
7.9573447159704));
#162970=CARTESIAN_POINT('Ctrl Pts',(-20.7291121646355,-18.2437775165808,
7.95624418976471));
#162971=CARTESIAN_POINT('Ctrl Pts',(-20.7354040725529,-18.2617581421778,
7.9551359376618));
#162972=CARTESIAN_POINT('Ctrl Pts',(-20.7459521244103,-18.2932600438301,
7.95318942672229));
#162973=CARTESIAN_POINT('Ctrl Pts',(-20.750315027364,-18.3067377458204,
7.95235510459761));
#162974=CARTESIAN_POINT('Ctrl Pts',(-20.7570545432907,-18.3282931851018,
7.95101787804382));
#162975=CARTESIAN_POINT('Ctrl Pts',(-20.7595188457556,-18.3363432137585,
7.9505178504801));
#162976=CARTESIAN_POINT('Ctrl Pts',(-20.763786514856,-18.350587230421,7.94963188454869));
#162977=CARTESIAN_POINT('Ctrl Pts',(-20.7656097187089,-18.3567751981563,
7.94924660042969));
#162978=CARTESIAN_POINT('Ctrl Pts',(-20.7693280461947,-18.3696113551058,
7.94844651352588));
#162979=CARTESIAN_POINT('Ctrl Pts',(-20.771218943158,-18.3762606794711,
7.94803157817029));
#162980=CARTESIAN_POINT('Ctrl Pts',(-20.7760009352766,-18.3933950639643,
7.94696106243246));
#162981=CARTESIAN_POINT('Ctrl Pts',(-20.7788438303318,-18.4038932614228,
7.94630392472707));
#162982=CARTESIAN_POINT('Ctrl Pts',(-20.7848191483326,-18.426652534329,
7.94487647843388));
#162983=CARTESIAN_POINT('Ctrl Pts',(-20.7879227668369,-18.4389206729892,
7.94410526548381));
#162984=CARTESIAN_POINT('Ctrl Pts',(-20.7966338678917,-18.4747005572732,
7.94185065864242));
#162985=CARTESIAN_POINT('Ctrl Pts',(-20.801948757875,-18.4982808240802,
7.94035804412167));
#162986=CARTESIAN_POINT('Ctrl Pts',(-20.8363442493001,-18.6640670291866,
7.92981464442311));
#162987=CARTESIAN_POINT('Ctrl Pts',(-20.851130049531,-18.8088169703404,
7.92031692626474));
#162988=CARTESIAN_POINT('Ctrl Pts',(-20.8509991383105,-18.9539100765585,
7.91072952400752));
#162989=CARTESIAN_POINT('Ctrl Pts',(-20.8509991377667,-18.9539106792569,
7.91072948418266));
#162990=CARTESIAN_POINT('Ctrl Pts',(-20.8508884779766,-19.0765197877048,
7.90262777016645));
#162991=CARTESIAN_POINT('Ctrl Pts',(-20.8401264221114,-19.198901967048,
7.89450607667186));
#162992=CARTESIAN_POINT('Ctrl Pts',(-20.8166444849761,-19.3320511155589,
7.88604145694026));
#162993=CARTESIAN_POINT('Ctrl Pts',(-20.8143518747477,-19.3444066702894,
7.88525971599234));
#162994=CARTESIAN_POINT('Ctrl Pts',(-20.8106712431876,-19.3633030964508,
7.88407060985964));
#162995=CARTESIAN_POINT('Ctrl Pts',(-20.8093620672279,-19.3698588063086,
7.88365927391941));
#162996=CARTESIAN_POINT('Ctrl Pts',(-20.8071513236229,-19.3806623897957,
7.88298350988733));
#162997=CARTESIAN_POINT('Ctrl Pts',(-20.8062677118098,-19.3849138325531,
7.88271812068513));
#162998=CARTESIAN_POINT('Ctrl Pts',(-20.8045210240075,-19.3931900179904,
7.88220258368105));
#162999=CARTESIAN_POINT('Ctrl Pts',(-20.8036592788117,-19.3972150189818,
7.88195236298181));
#163000=CARTESIAN_POINT('Ctrl Pts',(-20.8020280136667,-19.4047271656756,
7.88148633162137));
#163001=CARTESIAN_POINT('Ctrl Pts',(-20.8012614183712,-19.4082148399613,
7.88127036308551));
#163002=CARTESIAN_POINT('Ctrl Pts',(-20.7994932703404,-19.4161631715941,
7.88077906375489));
#163003=CARTESIAN_POINT('Ctrl Pts',(-20.7984860931884,-19.4206225257255,
7.88050405886988));
#163004=CARTESIAN_POINT('Ctrl Pts',(-20.7953527021961,-19.4342896849747,
7.87966306763098));
#163005=CARTESIAN_POINT('Ctrl Pts',(-20.7931792404429,-19.4434866898566,
7.87909972326578));
#163006=CARTESIAN_POINT('Ctrl Pts',(-20.7619486583876,-19.5717941388179,
7.87127271430771));
#163007=CARTESIAN_POINT('Ctrl Pts',(-20.7226548100719,-19.6881938883943,
7.86455357872539));
#163008=CARTESIAN_POINT('Ctrl Pts',(-20.6449227980636,-19.8658628497002,
7.85400328150231));
#163009=CARTESIAN_POINT('Ctrl Pts',(-20.6130671500829,-19.929690010207,
7.85014925697576));
#163010=CARTESIAN_POINT('Ctrl Pts',(-20.5342707230545,-20.069434682374,
7.84135941082986));
#163011=CARTESIAN_POINT('Ctrl Pts',(-20.4856322543038,-20.1442319974535,
7.83640110244062));
#163012=CARTESIAN_POINT('Ctrl Pts',(-20.4120584880257,-20.2431131116241,
7.82931016918979));
#163013=CARTESIAN_POINT('Ctrl Pts',(-20.3910310721284,-20.2699913462734,
7.827323909304));
#163014=CARTESIAN_POINT('Ctrl Pts',(-20.3624525905365,-20.3047563042614,
7.82467005732998));
#163015=CARTESIAN_POINT('Ctrl Pts',(-20.3554764305954,-20.3131104424966,
7.82402566957444));
#163016=CARTESIAN_POINT('Ctrl Pts',(-20.3439634281607,-20.3266834443802,
7.82296759052642));
#163017=CARTESIAN_POINT('Ctrl Pts',(-20.3394648312443,-20.3319345948855,
7.82255547151133));
#163018=CARTESIAN_POINT('Ctrl Pts',(-20.3307201304967,-20.3420415216623,
7.82175684321005));
#163019=CARTESIAN_POINT('Ctrl Pts',(-20.3264773960049,-20.3469001214652,
7.82137047621034));
#163020=CARTESIAN_POINT('Ctrl Pts',(-20.3166487568704,-20.3580521760454,
7.82047792666548));
#163021=CARTESIAN_POINT('Ctrl Pts',(-20.3110474281122,-20.364331836247,
7.81997110104062));
#163022=CARTESIAN_POINT('Ctrl Pts',(-20.2959253962986,-20.3810830457071,
7.81860760903631));
#163023=CARTESIAN_POINT('Ctrl Pts',(-20.2863370023308,-20.3914926575209,
7.81774808586631));
#163024=CARTESIAN_POINT('Ctrl Pts',(-20.2021849914205,-20.4810334416281,
7.81024647268885));
#163025=CARTESIAN_POINT('Ctrl Pts',(-20.1217436847516,-20.5543955644701,
7.80334484366058));
#163026=CARTESIAN_POINT('Ctrl Pts',(-19.959008586461,-20.6813311267264,
7.78990636276258));
#163027=CARTESIAN_POINT('Ctrl Pts',(-19.8779167312633,-20.7360082007562,
7.78342171273805));
#163028=CARTESIAN_POINT('Ctrl Pts',(-19.7310914805351,-20.8208679833736,
7.77224413309551));
#163029=CARTESIAN_POINT('Ctrl Pts',(-19.6670415366176,-20.8536555642205,
7.76753910418112));
#163030=CARTESIAN_POINT('Ctrl Pts',(-19.5707324088792,-20.8969167935079,
7.76082280057584));
#163031=CARTESIAN_POINT('Ctrl Pts',(-19.539694813602,-20.9099781973353,
7.75871088613623));
#163032=CARTESIAN_POINT('Ctrl Pts',(-19.5015761335029,-20.924959442176,
7.75619173333209));
#163033=CARTESIAN_POINT('Ctrl Pts',(-19.4947815122547,-20.9275894247936,
7.75574554216904));
#163034=CARTESIAN_POINT('Ctrl Pts',(-19.4840931107764,-20.9316632462458,
7.75504826522288));
#163035=CARTESIAN_POINT('Ctrl Pts',(-19.4802085035831,-20.9331307663138,
7.75479579832622));
#163036=CARTESIAN_POINT('Ctrl Pts',(-19.4729794620856,-20.9358374618164,
7.75432777358358));
#163037=CARTESIAN_POINT('Ctrl Pts',(-19.4696362468064,-20.9370796036796,
7.75411204444848));
#163038=CARTESIAN_POINT('Ctrl Pts',(-19.462049190355,-20.9398767073513,
7.75362408416469));
#163039=CARTESIAN_POINT('Ctrl Pts',(-19.4578035097067,-20.9414265272718,
7.75335216142913));
#163040=CARTESIAN_POINT('Ctrl Pts',(-19.4451919437508,-20.9459844670143,
7.75254770962068));
#163041=CARTESIAN_POINT('Ctrl Pts',(-19.4368119173993,-20.9489535424173,
7.75201744651799));
#163042=CARTESIAN_POINT('Ctrl Pts',(-19.3737829734597,-20.9708390347424,
7.74805940055269));
#163043=CARTESIAN_POINT('Ctrl Pts',(-19.3183930075901,-20.9875636520926,
7.74475096310306));
#163044=CARTESIAN_POINT('Ctrl Pts',(-19.1043534426584,-21.0427318428755,
7.73236527602057));
#163045=CARTESIAN_POINT('Ctrl Pts',(-18.9421390479485,-21.0650560415417,
7.72375961938505));
#163046=CARTESIAN_POINT('Ctrl Pts',(-18.7189084647188,-21.0697982257335,
7.71139187355725));
#163047=CARTESIAN_POINT('Ctrl Pts',(-18.6588315277271,-21.0685174176337,
7.70801705079311));
#163048=CARTESIAN_POINT('Ctrl Pts',(-18.5747507198067,-21.0631404303624,
7.70317892672398));
#163049=CARTESIAN_POINT('Ctrl Pts',(-18.5506370702587,-21.0611828319601,
7.70177822887931));
#163050=CARTESIAN_POINT('Ctrl Pts',(-18.5085811162129,-21.0570419965381,
7.69930932516665));
#163051=CARTESIAN_POINT('Ctrl Pts',(-18.4906231345173,-21.0550414051365,
7.69824679318016));
#163052=CARTESIAN_POINT('Ctrl Pts',(-18.464222180628,-21.0517575572766,
7.69667162738966));
#163053=CARTESIAN_POINT('Ctrl Pts',(-18.455757545468,-21.0506526640692,
7.69616461529144));
#163054=CARTESIAN_POINT('Ctrl Pts',(-18.4409127674991,-21.0486235790028,
7.69527187180842));
#163055=CARTESIAN_POINT('Ctrl Pts',(-18.4345296936801,-21.0477213774973,
7.69488684032161));
#163056=CARTESIAN_POINT('Ctrl Pts',(-18.4221316798874,-21.0459112097219,
7.69413668400826));
#163057=CARTESIAN_POINT('Ctrl Pts',(-18.4161163309557,-21.0450064440997,
7.69377166416281));
#163058=CARTESIAN_POINT('Ctrl Pts',(-18.4017269415461,-21.0427786801006,
7.69289593507089));
#163059=CARTESIAN_POINT('Ctrl Pts',(-18.3933568340568,-21.0414312873992,
7.69238445609245));
#163060=CARTESIAN_POINT('Ctrl Pts',(-18.3630705634205,-21.0363690818403,
7.69052606040096));
#163061=CARTESIAN_POINT('Ctrl Pts',(-18.341205753932,-21.0323595211849,
7.68916982520187));
#163062=CARTESIAN_POINT('Ctrl Pts',(-18.1386054449318,-20.9918989973368,
7.67646273917391));
#163063=CARTESIAN_POINT('Ctrl Pts',(-17.9633259877772,-20.9323325699457,
7.66432453444339));
#163064=CARTESIAN_POINT('Ctrl Pts',(-17.7253994061342,-20.8150535475416,
7.64680939966994));
#163065=CARTESIAN_POINT('Ctrl Pts',(-17.6548893923708,-20.7751197761543,
7.64148800580103));
#163066=CARTESIAN_POINT('Ctrl Pts',(-17.5563713087634,-20.7116004093602,
7.6340142357973));
#163067=CARTESIAN_POINT('Ctrl Pts',(-17.5264136361062,-20.6911775277672,
7.63173652456848));
#163068=CARTESIAN_POINT('Ctrl Pts',(-17.4909235300947,-20.6656235970081,
7.62904591514725));
#163069=CARTESIAN_POINT('Ctrl Pts',(-17.4848768797669,-20.6612209853006,
7.62858778168012));
#163070=CARTESIAN_POINT('Ctrl Pts',(-17.4755018529827,-20.654318635762,
7.62787807216377));
#163071=CARTESIAN_POINT('Ctrl Pts',(-17.4721573705127,-20.6518410228035,
7.62762500822957));
#163072=CARTESIAN_POINT('Ctrl Pts',(-17.4659614145795,-20.6472226576754,
7.62715644275172));
#163073=CARTESIAN_POINT('Ctrl Pts',(-17.4631080690923,-20.645084585437,
7.62694076638013));
#163074=CARTESIAN_POINT('Ctrl Pts',(-17.4566605511869,-20.6402278403329,
7.62645364408698));
#163075=CARTESIAN_POINT('Ctrl Pts',(-17.4530696591624,-20.6375049009582,
7.62618250213815));
#163076=CARTESIAN_POINT('Ctrl Pts',(-17.4422363136442,-20.6292354617392,
7.62536487854274));
#163077=CARTESIAN_POINT('Ctrl Pts',(-17.4350208804146,-20.6236535134842,
7.62482082970714));
#163078=CARTESIAN_POINT('Ctrl Pts',(-17.3795366093111,-20.580154018043,
7.62063936766184));
#163079=CARTESIAN_POINT('Ctrl Pts',(-17.3328966002781,-20.5401962516233,
7.61713648515878));
#163080=CARTESIAN_POINT('Ctrl Pts',(-17.1808017341162,-20.3979690574869,
7.60549960097017));
#163081=CARTESIAN_POINT('Ctrl Pts',(-17.0842703882613,-20.2867839309853,
7.5977131546074));
#163082=CARTESIAN_POINT('Ctrl Pts',(-16.9468070252436,-20.0905227558134,
7.58451580236484));
#163083=CARTESIAN_POINT('Ctrl Pts',(-16.8986499810703,-20.0111412667951,
7.57930739245145));
#163084=CARTESIAN_POINT('Ctrl Pts',(-16.8461310462591,-19.9101669778376,
7.57267773953802));
#163085=CARTESIAN_POINT('Ctrl Pts',(-16.8366863769089,-19.8913264141453,
7.57144086081967));
#163086=CARTESIAN_POINT('Ctrl Pts',(-16.8236312438081,-19.8642830841738,
7.56966433344511));
#163087=CARTESIAN_POINT('Ctrl Pts',(-16.8197889539165,-19.8561931638766,
7.56913275068293));
#163088=CARTESIAN_POINT('Ctrl Pts',(-16.813239783298,-19.8421750711511,
7.56821128690155));
#163089=CARTESIAN_POINT('Ctrl Pts',(-16.8105087096375,-19.8362582890758,
7.56782224848084));
#163090=CARTESIAN_POINT('Ctrl Pts',(-16.8053255422307,-19.8248914885335,
7.56707462125713));
#163091=CARTESIAN_POINT('Ctrl Pts',(-16.8028691187331,-19.8194435042612,
7.5667161862044));
#163092=CARTESIAN_POINT('Ctrl Pts',(-16.7965279868229,-19.8052193794704,
7.5657800376019));
#163093=CARTESIAN_POINT('Ctrl Pts',(-16.7926798648345,-19.7964271664299,
7.56520107726022));
#163094=CARTESIAN_POINT('Ctrl Pts',(-16.7796940204716,-19.7661990724295,
7.56320934949621));
#163095=CARTESIAN_POINT('Ctrl Pts',(-16.7708507582233,-19.744639248073,
7.56178663902572));
#163096=CARTESIAN_POINT('Ctrl Pts',(-16.7001129760838,-19.563731100552,
7.54982680060326));
#163097=CARTESIAN_POINT('Ctrl Pts',(-16.6573844864417,-19.3975980731648,
7.53862641072276));
#163098=CARTESIAN_POINT('Ctrl Pts',(-16.6233204444518,-19.13871544722,7.521371556759));
#163099=CARTESIAN_POINT('Ctrl Pts',(-16.6172799776276,-19.0485877072119,
7.51541663743598));
#163100=CARTESIAN_POINT('Ctrl Pts',(-16.6168937408165,-18.9197188059379,
7.50718327515759));
#163101=CARTESIAN_POINT('Ctrl Pts',(-16.6178351330105,-18.881093874975,
7.50475228711868));
#163102=CARTESIAN_POINT('Ctrl Pts',(-16.6202270189575,-18.8349068592937,
7.50190606007237));
#163103=CARTESIAN_POINT('Ctrl Pts',(-16.620662011859,-18.8273020813545,
7.50143940052899));
#163104=CARTESIAN_POINT('Ctrl Pts',(-16.6214000285952,-18.8155158094416,
7.50071938696682));
#163105=CARTESIAN_POINT('Ctrl Pts',(-16.6216744382275,-18.8113326788562,
7.50046447600715));
#163106=CARTESIAN_POINT('Ctrl Pts',(-16.6222050581317,-18.803595761432,
7.49999421090593));
#163107=CARTESIAN_POINT('Ctrl Pts',(-16.6224578121275,-18.8000418357937,
7.49977867105326));
#163108=CARTESIAN_POINT('Ctrl Pts',(-16.6230477069762,-18.7920332106285,
7.49929401966149));
#163109=CARTESIAN_POINT('Ctrl Pts',(-16.6233899758371,-18.7875789433532,
7.49902519886856));
#163110=CARTESIAN_POINT('Ctrl Pts',(-16.6244360954273,-18.7745066269026,
7.49823833715701));
#163111=CARTESIAN_POINT('Ctrl Pts',(-16.6251786580974,-18.7658916479788,
7.4977224174996));
#163112=CARTESIAN_POINT('Ctrl Pts',(-16.6307248349171,-18.7058487007593,
7.49414359651874));
#163113=CARTESIAN_POINT('Ctrl Pts',(-16.637356826807,-18.6546025879785,
7.49117567375488));
#163114=CARTESIAN_POINT('Ctrl Pts',(-16.6494413839244,-18.5821639457779,
7.48703966121493));
#163115=CARTESIAN_POINT('Ctrl Pts',(-16.6533565355493,-18.5607377479435,
7.48582376604037));
#163116=CARTESIAN_POINT('Ctrl Pts',(-16.6665994321883,-18.4940972211443,
7.48205523119524));
#163117=CARTESIAN_POINT('Ctrl Pts',(-16.6770760202979,-18.4491242202059,
7.47953085785205));
#163118=CARTESIAN_POINT('Ctrl Pts',(-16.7172948733586,-18.2988936293448,
7.47106361971575));
#163119=CARTESIAN_POINT('Ctrl Pts',(-16.7537170913693,-18.1956097449709,
7.46517527766237));
#163120=CARTESIAN_POINT('Ctrl Pts',(-16.8202493175692,-18.0452006129496,
7.45603035582364));
#163121=CARTESIAN_POINT('Ctrl Pts',(-16.8445041760552,-17.995688498136,
7.45292250372553));
#163122=CARTESIAN_POINT('Ctrl Pts',(-16.8869471288455,-17.9169821750941,
7.4477779865052));
#163123=CARTESIAN_POINT('Ctrl Pts',(-16.9039633479972,-17.8871845876408,
7.44578071920798));
#163124=CARTESIAN_POINT('Ctrl Pts',(-16.9272822671727,-17.8485613413166,
7.44311989438058));
#163125=CARTESIAN_POINT('Ctrl Pts',(-16.9329398000158,-17.8393509137813,
7.44247986918972));
#163126=CARTESIAN_POINT('Ctrl Pts',(-16.9423229786939,-17.8243342529338,
7.44142713928122));
#163127=CARTESIAN_POINT('Ctrl Pts',(-16.946006953364,-17.8185021176764,
7.44101597598107));
#163128=CARTESIAN_POINT('Ctrl Pts',(-16.953194210017,-17.8072461274672,
7.44021790521636));
#163129=CARTESIAN_POINT('Ctrl Pts',(-16.9566939348938,-17.8018200837174,
7.43983113315872));
#163130=CARTESIAN_POINT('Ctrl Pts',(-16.9648334160641,-17.7893263236327,
7.43893576594251));
#163131=CARTESIAN_POINT('Ctrl Pts',(-16.969490774961,-17.7822702573048,
7.43842651470706));
#163132=CARTESIAN_POINT('Ctrl Pts',(-16.9821331243412,-17.7633639598381,
7.43705224776383));
#163133=CARTESIAN_POINT('Ctrl Pts',(-16.9901959294063,-17.7515665225978,
7.43618430426384));
#163134=CARTESIAN_POINT('Ctrl Pts',(-17.0652574986312,-17.644089103529,
7.42817971778301));
#163135=CARTESIAN_POINT('Ctrl Pts',(-17.1399371276725,-17.5540414135516,
7.42074153172824));
#163136=CARTESIAN_POINT('Ctrl Pts',(-17.3354199595754,-17.3544713981144,
7.40249421335316));
#163137=CARTESIAN_POINT('Ctrl Pts',(-17.462189503704,-17.2518171049488,
7.39154536572418));
#163138=CARTESIAN_POINT('Ctrl Pts',(-17.6270394328668,-17.1471746298091,
7.37913638044254));
#163139=CARTESIAN_POINT('Ctrl Pts',(-17.6550249036619,-17.1303059181342,
7.37708855267636));
#163140=CARTESIAN_POINT('Ctrl Pts',(-17.6896861162014,-17.1104924425565,
7.37463342060822));
#163141=CARTESIAN_POINT('Ctrl Pts',(-17.695999445713,-17.1069264446045,
7.37418946343051));
#163142=CARTESIAN_POINT('Ctrl Pts',(-17.7059218426768,-17.1013889625903,
7.37349691308908));
#163143=CARTESIAN_POINT('Ctrl Pts',(-17.7095184758355,-17.0993954775349,
7.37324694390315));
#163144=CARTESIAN_POINT('Ctrl Pts',(-17.7162497599066,-17.0956901646851,
7.37278113149526));
#163145=CARTESIAN_POINT('Ctrl Pts',(-17.7193828999214,-17.0939758084574,
7.37256513191096));
#163146=CARTESIAN_POINT('Ctrl Pts',(-17.726541819582,-17.0900821795917,
7.37207343934817));
#163147=CARTESIAN_POINT('Ctrl Pts',(-17.7305703306298,-17.0879080347859,
7.3717980743213));
#163148=CARTESIAN_POINT('Ctrl Pts',(-17.7429638487952,-17.0812712022994,
7.37095488597408));
#163149=CARTESIAN_POINT('Ctrl Pts',(-17.7513519404872,-17.0768515562118,
7.37038972475761));
#163150=CARTESIAN_POINT('Ctrl Pts',(-17.8671859526874,-17.0168098893848,
7.36265700851703));
#163151=CARTESIAN_POINT('Ctrl Pts',(-17.9791944820619,-16.9704338124156,
7.35601949980941));
#163152=CARTESIAN_POINT('Ctrl Pts',(-18.2651924850981,-16.8798164794217,
7.33969354614841));
#163153=CARTESIAN_POINT('Ctrl Pts',(-18.4419637838506,-16.8476158030409,
7.33007486661242));
#163154=CARTESIAN_POINT('Ctrl Pts',(-18.6421236366903,-16.836885544938,
7.31840391301656));
#163155=CARTESIAN_POINT('Ctrl Pts',(-18.6635892708165,-16.8360622165588,
7.31714355834492));
#163156=CARTESIAN_POINT('Ctrl Pts',(-18.6940855953224,-16.8353570711439,
7.31533916911888));
#163157=CARTESIAN_POINT('Ctrl Pts',(-18.7031091702568,-16.8352061506196,
7.31480355573699));
#163158=CARTESIAN_POINT('Ctrl Pts',(-18.7186621466533,-16.8350454940509,
7.31387732129739));
#163159=CARTESIAN_POINT('Ctrl Pts',(-18.7251911837587,-16.835008258569,
7.31348756669342));
#163160=CARTESIAN_POINT('Ctrl Pts',(-18.7376819741543,-16.8349948074066,
7.31274010795831));
#163161=CARTESIAN_POINT('Ctrl Pts',(-18.7436436680062,-16.8350135709129,
7.31238256501264));
#163162=CARTESIAN_POINT('Ctrl Pts',(-18.7591228076153,-16.8351276762284,
7.31145213909697));
#163163=CARTESIAN_POINT('Ctrl Pts',(-18.7686397535281,-16.8352620205938,
7.31087803919449));
#163164=CARTESIAN_POINT('Ctrl Pts',(-18.8009696861401,-16.8359364892325,
7.30892062634389));
#163165=CARTESIAN_POINT('Ctrl Pts',(-18.8237740984467,-16.8367812718875,
7.30752782698009));
#163166=CARTESIAN_POINT('Ctrl Pts',(-19.0240757247027,-16.8474462844111,
7.29518352548989));
#163167=CARTESIAN_POINT('Ctrl Pts',(-19.1996626216888,-16.8792182317456,
7.28350747807423));
#163168=CARTESIAN_POINT('Ctrl Pts',(-19.4506665025062,-16.9581655027858,
7.26612453331546));
#163169=CARTESIAN_POINT('Ctrl Pts',(-19.5305375617882,-16.9887076973626,
7.26049822828394));
#163170=CARTESIAN_POINT('Ctrl Pts',(-19.6424270576734,-17.0394494875494,
7.25265703056099));
#163171=CARTESIAN_POINT('Ctrl Pts',(-19.6760922428569,-17.0558059736017,
7.25030390775852));
#163172=CARTESIAN_POINT('Ctrl Pts',(-19.7160080830397,-17.0765250988076,
7.24753660367672));
#163173=CARTESIAN_POINT('Ctrl Pts',(-19.7226892734233,-17.0800385942231,
7.24707418989989));
#163174=CARTESIAN_POINT('Ctrl Pts',(-19.7330383415198,-17.0855518112681,
7.24635930592242));
#163175=CARTESIAN_POINT('Ctrl Pts',(-19.7367192564454,-17.0875267385943,
7.24610531333593));
#163176=CARTESIAN_POINT('Ctrl Pts',(-19.7435300020198,-17.091206922238,
7.24563589824954));
#163177=CARTESIAN_POINT('Ctrl Pts',(-19.7466613441442,-17.0929091723117,
7.24542029543805));
#163178=CARTESIAN_POINT('Ctrl Pts',(-19.753724749806,-17.0967720993383,
7.2449344378523));
#163179=CARTESIAN_POINT('Ctrl Pts',(-19.7576542416068,-17.0989373666136,
7.24466448030701));
#163180=CARTESIAN_POINT('Ctrl Pts',(-19.7692143279946,-17.1053553116191,
7.24387119334701));
#163181=CARTESIAN_POINT('Ctrl Pts',(-19.7768256250847,-17.1096428056355,
7.24335003750475));
#163182=CARTESIAN_POINT('Ctrl Pts',(-19.8310962424684,-17.140657884197,
7.23964075177672));
#163183=CARTESIAN_POINT('Ctrl Pts',(-19.8767530093681,-17.1691099228594,
7.2365556509409));
#163184=CARTESIAN_POINT('Ctrl Pts',(-20.0608279427225,-17.2938004730959,
7.22405657322377));
#163185=CARTESIAN_POINT('Ctrl Pts',(-20.1885933942022,-17.4046590965979,
7.21518670302042));
#163186=CARTESIAN_POINT('Ctrl Pts',(-20.3564534555601,-17.5896733212733,
7.20134232228929));
#163187=CARTESIAN_POINT('Ctrl Pts',(-20.407528852064,-17.6529279118329,
7.19675121411317));
#163188=CARTESIAN_POINT('Ctrl Pts',(-20.4662740091775,-17.7349128619316,
7.19086736104466));
#163189=CARTESIAN_POINT('Ctrl Pts',(-20.4774847979088,-17.7510274500799,
7.18971407501103));
#163190=CARTESIAN_POINT('Ctrl Pts',(-20.4933402539565,-17.7745083341693,
7.18803712681663));
#163191=CARTESIAN_POINT('Ctrl Pts',(-20.4981663211925,-17.7817513341116,
7.18752032732416));
#163192=CARTESIAN_POINT('Ctrl Pts',(-20.5065035597332,-17.794432709391,
7.18661622670279));
#163193=CARTESIAN_POINT('Ctrl Pts',(-20.5100347288258,-17.7998578463907,
7.18622968179366));
#163194=CARTESIAN_POINT('Ctrl Pts',(-20.5168105233643,-17.8103730584787,
7.1854808746197));
#163195=CARTESIAN_POINT('Ctrl Pts',(-20.52005837287,-17.8154609890754,7.18511873755079));
#163196=CARTESIAN_POINT('Ctrl Pts',(-20.5277198372757,-17.8275770282756,
7.18425676978858));
#163197=CARTESIAN_POINT('Ctrl Pts',(-20.5321139475799,-17.8346172981343,
7.18375622322555));
#163198=CARTESIAN_POINT('Ctrl Pts',(-20.547545602996,-17.8596687434147,
7.18197612587293));
#163199=CARTESIAN_POINT('Ctrl Pts',(-20.5583545566611,-17.8778186237432,
7.18068824496313));
#163200=CARTESIAN_POINT('Ctrl Pts',(-20.6295618646363,-18.0015622251531,
7.17191704123909));
#163201=CARTESIAN_POINT('Ctrl Pts',(-20.6809596360427,-18.1119033527847,
7.1641218929178));
#163202=CARTESIAN_POINT('Ctrl Pts',(-20.722580619343,-18.2258897326345,
7.15616144973347));
#163203=CARTESIAN_POINT('',(-20.847808864184,-18.9524614626978,7.68893960118917));
#163204=CARTESIAN_POINT('Ctrl Pts',(-20.8476070359586,-18.9524685808987,
7.68905589349203));
#163205=CARTESIAN_POINT('Ctrl Pts',(-20.848239885686,-19.2779557825456,
7.66955339595671));
#163206=CARTESIAN_POINT('Ctrl Pts',(-20.6243346437841,-20.3101167079764,
7.6076589628609));
#163207=CARTESIAN_POINT('Ctrl Pts',(-19.0148744683191,-21.4394564387197,
7.50337259420462));
#163208=CARTESIAN_POINT('Ctrl Pts',(-16.794474806048,-20.5345839704445,
7.3761967875232));
#163209=CARTESIAN_POINT('Ctrl Pts',(-16.3534691287178,-18.1777889355253,
7.24902098084176));
#163210=CARTESIAN_POINT('Ctrl Pts',(-18.0964527733798,-16.5312844993037,
7.12184517416032));
#163211=CARTESIAN_POINT('Ctrl Pts',(-20.0208838101815,-17.0060915880697,
7.01671104612961));
#163212=CARTESIAN_POINT('Ctrl Pts',(-20.6031709119695,-17.9078852545191,
6.95396885365936));
#163213=CARTESIAN_POINT('Ctrl Pts',(-20.7193262654686,-18.2270707613317,
6.9336185967496));
#163214=CARTESIAN_POINT('Ctrl Pts',(-20.8509999712464,-18.9523489167874,
7.68710090301811));
#163215=CARTESIAN_POINT('Ctrl Pts',(-20.8510014360976,-18.9434611529801,
7.6876214684987));
#163216=CARTESIAN_POINT('Ctrl Pts',(-20.8509469309248,-18.9345735478661,
7.68814372234433));
#163217=CARTESIAN_POINT('Ctrl Pts',(-20.8507292584211,-18.9170624111266,
7.68917619302368));
#163218=CARTESIAN_POINT('Ctrl Pts',(-20.8505693532622,-18.9084390302998,
7.68968629804239));
#163219=CARTESIAN_POINT('Ctrl Pts',(-20.8502036146338,-18.893605983878,
7.69056668727183));
#163220=CARTESIAN_POINT('Ctrl Pts',(-20.8500231309564,-18.8873957609257,
7.69093617673417));
#163221=CARTESIAN_POINT('Ctrl Pts',(-20.8496088606408,-18.875017907279,
7.69167443940697));
#163222=CARTESIAN_POINT('Ctrl Pts',(-20.8493754333924,-18.8688503254636,
7.69204319777663));
#163223=CARTESIAN_POINT('Ctrl Pts',(-20.8488557235133,-18.8565429563131,
7.69278088374308));
#163224=CARTESIAN_POINT('Ctrl Pts',(-20.8485696657796,-18.8504032195806,
7.69314980073961));
#163225=CARTESIAN_POINT('Ctrl Pts',(-20.8477228782773,-18.8337853696163,
7.69415081943603));
#163226=CARTESIAN_POINT('Ctrl Pts',(-20.8471109811632,-18.8233101399852,
7.69478452060767));
#163227=CARTESIAN_POINT('Ctrl Pts',(-20.844514726168,-18.7838994926352,
7.69717908560958));
#163228=CARTESIAN_POINT('Ctrl Pts',(-20.8420137566289,-18.7550023837778,
7.69895605267754));
#163229=CARTESIAN_POINT('Ctrl Pts',(-20.8205675150906,-18.5551086828724,
7.71140108946184));
#163230=CARTESIAN_POINT('Ctrl Pts',(-20.7814502050678,-18.3871144038753,
7.72271554281783));
#163231=CARTESIAN_POINT('Ctrl Pts',(-20.722580563188,-18.2258895788442,
7.73405224475127));
#163232=CARTESIAN_POINT('Origin',(-18.734,-18.952,0.));
#163233=CARTESIAN_POINT('',(-20.7225806939367,-18.2258899369226,8.75434681593714));
#163234=CARTESIAN_POINT('',(-20.7225805426339,-18.2258895225534,8.53521110136663));
#163235=CARTESIAN_POINT('',(-20.7225805737622,-18.2258896078036,0.));
#163236=CARTESIAN_POINT('Ctrl Pts',(-20.7225806939367,-18.2258899369226,
8.75434681593714));
#163237=CARTESIAN_POINT('Ctrl Pts',(-20.7522189871416,-18.3070596392385,
8.74958609388981));
#163238=CARTESIAN_POINT('Ctrl Pts',(-20.7768869532507,-18.3900423068481,
8.74492446735276));
#163239=CARTESIAN_POINT('Ctrl Pts',(-20.8270296777673,-18.6065650054646,
8.732822301103));
#163240=CARTESIAN_POINT('Ctrl Pts',(-20.8448588566228,-18.741366397787,
8.7253255891255));
#163241=CARTESIAN_POINT('Ctrl Pts',(-20.8502665616911,-18.8937846453747,
8.71640102340825));
#163242=CARTESIAN_POINT('Ctrl Pts',(-20.8506630232942,-18.9106380729111,
8.715408521791));
#163243=CARTESIAN_POINT('Ctrl Pts',(-20.85095289411,-18.9356775534054,8.71392483201408));
#163244=CARTESIAN_POINT('Ctrl Pts',(-20.8510001744647,-18.9438614137362,
8.71343846151186));
#163245=CARTESIAN_POINT('Ctrl Pts',(-20.8509998627386,-18.9584435228824,
8.71256918852936));
#163246=CARTESIAN_POINT('Ctrl Pts',(-20.8509707194805,-18.964841701459,
8.71218686888589));
#163247=CARTESIAN_POINT('Ctrl Pts',(-20.8508481156784,-18.9783316693246,
8.71137882529349));
#163248=CARTESIAN_POINT('Ctrl Pts',(-20.8507480205219,-18.9854233058149,
8.71095289800032));
#163249=CARTESIAN_POINT('Ctrl Pts',(-20.8503886243636,-19.0041994779993,
8.70982210808948));
#163250=CARTESIAN_POINT('Ctrl Pts',(-20.8500681972762,-19.0158824759358,
8.70911533896458));
#163251=CARTESIAN_POINT('Ctrl Pts',(-20.8481220039195,-19.0703736722614,
8.70580369479496));
#163252=CARTESIAN_POINT('Ctrl Pts',(-20.8452939285419,-19.1131263546401,
8.70316145119592));
#163253=CARTESIAN_POINT('Ctrl Pts',(-20.833902049344,-19.2309338723355,
8.69575366709832));
#163254=CARTESIAN_POINT('Ctrl Pts',(-20.8226163014332,-19.3056562166429,
8.69090985328829));
#163255=CARTESIAN_POINT('Ctrl Pts',(-20.7814378526798,-19.5053193232467,
8.67762194617872));
#163256=CARTESIAN_POINT('Ctrl Pts',(-20.7441342285476,-19.6284041476841,
8.66904368299812));
#163257=CARTESIAN_POINT('Ctrl Pts',(-20.6896737654832,-19.7627435099994,
8.65959203219377));
#163258=CARTESIAN_POINT('Ctrl Pts',(-20.6832520940452,-19.7780636842366,
8.65851314531125));
#163259=CARTESIAN_POINT('Ctrl Pts',(-20.6554927754829,-19.8421623554157,
8.65399900269732));
#163260=CARTESIAN_POINT('Ctrl Pts',(-20.6324974129129,-19.8902068586563,
8.65061476691844));
#163261=CARTESIAN_POINT('Ctrl Pts',(-20.603657118634,-19.9450494385956,
8.64679243768987));
#163262=CARTESIAN_POINT('Ctrl Pts',(-20.5995537479213,-19.9527368027445,
8.64625762188909));
#163263=CARTESIAN_POINT('Ctrl Pts',(-20.5932681131467,-19.9643394539449,
8.6454521361562));
#163264=CARTESIAN_POINT('Ctrl Pts',(-20.5911207462444,-19.9682733988946,
8.64517933304397));
#163265=CARTESIAN_POINT('Ctrl Pts',(-20.5872434438664,-19.9753232327005,
8.6446910388086));
#163266=CARTESIAN_POINT('Ctrl Pts',(-20.585518126769,-19.978441585112,8.64447526001744));
#163267=CARTESIAN_POINT('Ctrl Pts',(-20.5817516576964,-19.9852087352868,
8.64400745508561));
#163268=CARTESIAN_POINT('Ctrl Pts',(-20.5797075756509,-19.9888558362048,
8.64375562032802));
#163269=CARTESIAN_POINT('Ctrl Pts',(-20.5739344548287,-19.9990852081065,
8.64305000892254));
#163270=CARTESIAN_POINT('Ctrl Pts',(-20.5701808751074,-20.0056536569985,
8.64259778047612));
#163271=CARTESIAN_POINT('Ctrl Pts',(-20.5475081043533,-20.0448399703605,
8.63990413633165));
#163272=CARTESIAN_POINT('Ctrl Pts',(-20.5277541350204,-20.0769699304541,
8.63771333291994));
#163273=CARTESIAN_POINT('Ctrl Pts',(-20.4598646273692,-20.1810532858221,
8.63061755555147));
#163274=CARTESIAN_POINT('Ctrl Pts',(-20.4081727363313,-20.2505871977334,
8.62587700674518));
#163275=CARTESIAN_POINT('Ctrl Pts',(-20.2388246733254,-20.4514033768187,
8.61158238343243));
#163276=CARTESIAN_POINT('Ctrl Pts',(-20.1089423701453,-20.5713315264266,
8.60211688859373));
#163277=CARTESIAN_POINT('Ctrl Pts',(-19.9470527619602,-20.6871422186922,
8.59054994190412));
#163278=CARTESIAN_POINT('Ctrl Pts',(-19.9281750744294,-20.700188020047,
8.58920559275252));
#163279=CARTESIAN_POINT('Ctrl Pts',(-19.9011552411323,-20.7182187381118,
8.58728589835375));
#163280=CARTESIAN_POINT('Ctrl Pts',(-19.8931852993571,-20.7234596876553,
8.58672019848798));
#163281=CARTESIAN_POINT('Ctrl Pts',(-19.8801738798225,-20.7318904529672,
8.58579742244521));
#163282=CARTESIAN_POINT('Ctrl Pts',(-19.8751538022231,-20.7351131724882,
8.58544157932636));
#163283=CARTESIAN_POINT('Ctrl Pts',(-19.8646137476526,-20.7418167895161,
8.58469480712144));
#163284=CARTESIAN_POINT('Ctrl Pts',(-19.8590911702102,-20.74529346278,8.5843037264495));
#163285=CARTESIAN_POINT('Ctrl Pts',(-19.8459086037695,-20.753507528335,
8.58337063104969));
#163286=CARTESIAN_POINT('Ctrl Pts',(-19.8382343304543,-20.7582216523207,
8.58282776661781));
#163287=CARTESIAN_POINT('Ctrl Pts',(-19.8122484270134,-20.7739566687607,
8.5809905649218));
#163288=CARTESIAN_POINT('Ctrl Pts',(-19.7938005161747,-20.7847489153051,
8.57968793716397));
#163289=CARTESIAN_POINT('Ctrl Pts',(-19.6922726404434,-20.8420984583779,
8.57252551833946));
#163290=CARTESIAN_POINT('Ctrl Pts',(-19.6062974776821,-20.883282350232,
8.5664766973249));
#163291=CARTESIAN_POINT('Ctrl Pts',(-19.3593953782732,-20.9816963774327,
8.54920519792616));
#163292=CARTESIAN_POINT('Ctrl Pts',(-19.1938962328857,-21.0254702954223,
8.53769565257752));
#163293=CARTESIAN_POINT('Ctrl Pts',(-18.9884995560309,-21.0539687658188,
8.52446063874565));
#163294=CARTESIAN_POINT('Ctrl Pts',(-18.9519275397863,-21.0580747093034,
8.52214624293066));
#163295=CARTESIAN_POINT('Ctrl Pts',(-18.9081487281184,-21.0618370152749,
8.51944039196791));
#163296=CARTESIAN_POINT('Ctrl Pts',(-18.9010296260911,-21.0624125468391,
8.51900241550412));
#163297=CARTESIAN_POINT('Ctrl Pts',(-18.8894081142736,-21.0632928929596,
8.51829091618393));
#163298=CARTESIAN_POINT('Ctrl Pts',(-18.8849074690118,-21.0636193545504,
8.51801622369394));
#163299=CARTESIAN_POINT('Ctrl Pts',(-18.8768483357869,-21.0641780391561,
8.51752590339475));
#163300=CARTESIAN_POINT('Ctrl Pts',(-18.873290286326,-21.0644156629017,
8.51730997738185));
#163301=CARTESIAN_POINT('Ctrl Pts',(-18.8655823236398,-21.0649108782469,
8.51684339699508));
#163302=CARTESIAN_POINT('Ctrl Pts',(-18.8614322600133,-21.0651652342161,
8.51659292568282));
#163303=CARTESIAN_POINT('Ctrl Pts',(-18.8498347035972,-21.0658417547009,
8.51589497574586));
#163304=CARTESIAN_POINT('Ctrl Pts',(-18.8423856045028,-21.0662367906572,
8.51544899174819));
#163305=CARTESIAN_POINT('Ctrl Pts',(-18.7990588277555,-21.0683048791342,
8.51286759802681));
#163306=CARTESIAN_POINT('Ctrl Pts',(-18.7631430029587,-21.069104159827,
8.51077801754748));
#163307=CARTESIAN_POINT('Ctrl Pts',(-18.6474957955114,-21.0687338852646,
8.5041620960288));
#163308=CARTESIAN_POINT('Ctrl Pts',(-18.5678412158585,-21.0639750380824,
8.49977578619877));
#163309=CARTESIAN_POINT('Ctrl Pts',(-18.3036801491088,-21.0331510336362,
8.48527562108297));
#163310=CARTESIAN_POINT('Ctrl Pts',(-18.1223981311488,-20.9872646006947,
8.47531905426197));
#163311=CARTESIAN_POINT('Ctrl Pts',(-17.9289803466747,-20.910090509261,
8.46320670677209));
#163312=CARTESIAN_POINT('Ctrl Pts',(-17.9086323605582,-20.9016008028846,
8.46191422976705));
#163313=CARTESIAN_POINT('Ctrl Pts',(-17.8806749270881,-20.8894201184571,
8.46011153633482));
#163314=CARTESIAN_POINT('Ctrl Pts',(-17.8729489924917,-20.8859988507716,
8.45961049806933));
#163315=CARTESIAN_POINT('Ctrl Pts',(-17.8597034183816,-20.880038225699,
8.4587464682755));
#163316=CARTESIAN_POINT('Ctrl Pts',(-17.854173809767,-20.8775211726134,
8.4583842448822));
#163317=CARTESIAN_POINT('Ctrl Pts',(-17.8427959033876,-20.872282756824,
8.45763575052938));
#163318=CARTESIAN_POINT('Ctrl Pts',(-17.836949060963,-20.8695584004975,
8.45724937916552));
#163319=CARTESIAN_POINT('Ctrl Pts',(-17.8233708417995,-20.863155890743,
8.45634800722608));
#163320=CARTESIAN_POINT('Ctrl Pts',(-17.815649186299,-20.8594574915572,
8.45583230835775));
#163321=CARTESIAN_POINT('Ctrl Pts',(-17.7910016155376,-20.8474678252563,
8.45417609692816));
#163322=CARTESIAN_POINT('Ctrl Pts',(-17.7741642716613,-20.8389975008534,
8.45302935925771));
#163323=CARTESIAN_POINT('Ctrl Pts',(-17.6906005878337,-20.7955515305975,
8.44725942685276));
#163324=CARTESIAN_POINT('Ctrl Pts',(-17.625668455206,-20.7572599801814,
8.44251982661224));
#163325=CARTESIAN_POINT('Ctrl Pts',(-17.4719767714351,-20.6552040417191,
8.43066394306269));
#163326=CARTESIAN_POINT('Ctrl Pts',(-17.3858467206001,-20.5878746591772,
8.42344782931245));
#163327=CARTESIAN_POINT('Ctrl Pts',(-17.2943200560022,-20.5041701034149,
8.4152543163928));
#163328=CARTESIAN_POINT('Ctrl Pts',(-17.2834467535492,-20.4940135063644,
8.41427197343938));
#163329=CARTESIAN_POINT('Ctrl Pts',(-17.1974992093132,-20.4120175456383,
8.40643936815063));
#163330=CARTESIAN_POINT('Ctrl Pts',(-17.1276903443813,-20.3348450158144,
8.39965269953485));
#163331=CARTESIAN_POINT('Ctrl Pts',(-17.0578732896386,-20.2452061300157,
8.39263281344571));
#163332=CARTESIAN_POINT('Ctrl Pts',(-17.051973056526,-20.2375225449252,
8.39203759938184));
#163333=CARTESIAN_POINT('Ctrl Pts',(-17.0433382645071,-20.2261166438656,
8.39116393487499));
#163334=CARTESIAN_POINT('Ctrl Pts',(-17.040562906277,-20.2224255730153,
8.39088272342314));
#163335=CARTESIAN_POINT('Ctrl Pts',(-17.0356601843566,-20.215860615268,
8.39038528633653));
#163336=CARTESIAN_POINT('Ctrl Pts',(-17.0335280033612,-20.2129903939172,
8.39016872630794));
#163337=CARTESIAN_POINT('Ctrl Pts',(-17.0289748072546,-20.2068285887528,
8.38970579404272));
#163338=CARTESIAN_POINT('Ctrl Pts',(-17.0265560534325,-20.2035354030259,
8.38945957833202));
#163339=CARTESIAN_POINT('Ctrl Pts',(-17.0199416512347,-20.1944748857733,
8.38878538982269));
#163340=CARTESIAN_POINT('Ctrl Pts',(-17.0157655443105,-20.1886932616161,
8.38835875092838));
#163341=CARTESIAN_POINT('Ctrl Pts',(-16.9936087030843,-20.1576892623538,
8.38608925195583));
#163342=CARTESIAN_POINT('Ctrl Pts',(-16.9761529312783,-20.1320942228667,
8.38428024199847));
#163343=CARTESIAN_POINT('Ctrl Pts',(-16.8701166337873,-19.9690385675996,
8.3730931893538));
#163344=CARTESIAN_POINT('Ctrl Pts',(-16.7971426030127,-19.8220715030235,
8.36445040393977));
#163345=CARTESIAN_POINT('Ctrl Pts',(-16.7019828385438,-19.5573573844441,
8.34905532959519));
#163346=CARTESIAN_POINT('Ctrl Pts',(-16.6714707864458,-19.443446031986,
8.34248547274969));
#163347=CARTESIAN_POINT('Ctrl Pts',(-16.6480483539502,-19.3135235243138,
8.33475159435991));
#163348=CARTESIAN_POINT('Ctrl Pts',(-16.6456537438723,-19.2994239886114,
8.33390942208875));
#163349=CARTESIAN_POINT('Ctrl Pts',(-16.6420705810909,-19.2769489874491,
8.33256197780976));
#163350=CARTESIAN_POINT('Ctrl Pts',(-16.6407890290309,-19.2685886384396,
8.33205965298254));
#163351=CARTESIAN_POINT('Ctrl Pts',(-16.6386174752184,-19.2538323582939,
8.33117101431345));
#163352=CARTESIAN_POINT('Ctrl Pts',(-16.6377065683066,-19.2474395784026,
8.33078536758771));
#163353=CARTESIAN_POINT('Ctrl Pts',(-16.6358832777938,-19.2342105354972,
8.32998590175462));
#163354=CARTESIAN_POINT('Ctrl Pts',(-16.6349750261165,-19.2273737888929,
8.32957195685239));
#163355=CARTESIAN_POINT('Ctrl Pts',(-16.6327299132914,-19.2098172290993,
8.32850689665191));
#163356=CARTESIAN_POINT('Ctrl Pts',(-16.6314416807036,-19.1990914974247,
8.32785425434452));
#163357=CARTESIAN_POINT('Ctrl Pts',(-16.6264111796692,-19.1543159671652,
8.32512123162497));
#163358=CARTESIAN_POINT('Ctrl Pts',(-16.6234136981773,-19.1201892783728,
8.32301758462311));
#163359=CARTESIAN_POINT('Ctrl Pts',(-16.6177644663944,-19.0311230801942,
8.31747054484192));
#163360=CARTESIAN_POINT('Ctrl Pts',(-16.616423491967,-18.9761290671421,
8.31398889466164));
#163361=CARTESIAN_POINT('Ctrl Pts',(-16.6188176927005,-18.8118575412607,
8.30342980202159));
#163362=CARTESIAN_POINT('Ctrl Pts',(-16.6288723228099,-18.7028612911686,
8.29620393433791));
#163363=CARTESIAN_POINT('Ctrl Pts',(-16.6537707620644,-18.5572707146935,
8.28644680181537));
#163364=CARTESIAN_POINT('Ctrl Pts',(-16.6612764451272,-18.5195857806304,
8.28391287315826));
#163365=CARTESIAN_POINT('Ctrl Pts',(-16.6768654437478,-18.4511020719063,
8.27931156440573));
#163366=CARTESIAN_POINT('Ctrl Pts',(-16.6846260405109,-18.4202408199611,
8.27723942090632));
#163367=CARTESIAN_POINT('Ctrl Pts',(-16.7062965662911,-18.3416044616206,
8.27198047353112));
#163368=CARTESIAN_POINT('Ctrl Pts',(-16.7212012470447,-18.2941200952936,
8.2688248791707));
#163369=CARTESIAN_POINT('Ctrl Pts',(-16.7403666535599,-18.2398370469197,
8.26527477879738));
#163370=CARTESIAN_POINT('Ctrl Pts',(-16.7430074693989,-18.23248715149,8.26479533853439));
#163371=CARTESIAN_POINT('Ctrl Pts',(-16.7472898090156,-18.2207727048025,
8.26403337285371));
#163372=CARTESIAN_POINT('Ctrl Pts',(-16.7489051545586,-18.2163987522008,
8.26374935641675));
#163373=CARTESIAN_POINT('Ctrl Pts',(-16.7517898959555,-18.2086662972588,
8.26324816923809));
#163374=CARTESIAN_POINT('Ctrl Pts',(-16.7530534007978,-18.2053056434818,
8.2630306512886));
#163375=CARTESIAN_POINT('Ctrl Pts',(-16.7557475569954,-18.1981947319117,
8.26257106179847));
#163376=CARTESIAN_POINT('Ctrl Pts',(-16.757180323144,-18.1944453311721,
8.26232911903495));
#163377=CARTESIAN_POINT('Ctrl Pts',(-16.7610713735858,-18.1843490635763,
8.26167860951522));
#163378=CARTESIAN_POINT('Ctrl Pts',(-16.763549640883,-18.1780098771641,
8.26127122451134));
#163379=CARTESIAN_POINT('Ctrl Pts',(-16.7759382354572,-18.1467661404363,
8.25926805224283));
#163380=CARTESIAN_POINT('Ctrl Pts',(-16.7862908387133,-18.1220381834663,
8.25769739569592));
#163381=CARTESIAN_POINT('Ctrl Pts',(-16.8174918675877,-18.0513140161821,
8.25322967169033));
#163382=CARTESIAN_POINT('Ctrl Pts',(-16.8395206619337,-18.0058565745763,
8.25038829739416));
#163383=CARTESIAN_POINT('Ctrl Pts',(-16.9254735306056,-17.8435544509589,
8.24020469132456));
#163384=CARTESIAN_POINT('Ctrl Pts',(-16.9987556897927,-17.7320208339459,
8.233113323117));
#163385=CARTESIAN_POINT('Ctrl Pts',(-17.1463019961067,-17.5479109261272,
8.22012759393819));
#163386=CARTESIAN_POINT('Ctrl Pts',(-17.2163181498419,-17.4725105796423,
8.21435056080368));
#163387=CARTESIAN_POINT('Ctrl Pts',(-17.301797446402,-17.3929356121952,
8.20750654813196));
#163388=CARTESIAN_POINT('Ctrl Pts',(-17.3121631560534,-17.3834765239503,
8.20667997387138));
#163389=CARTESIAN_POINT('Ctrl Pts',(-17.3288678445816,-17.3685345443103,
8.20535283851313));
#163390=CARTESIAN_POINT('Ctrl Pts',(-17.335146779248,-17.3629849317064,
8.20485508566195));
#163391=CARTESIAN_POINT('Ctrl Pts',(-17.3463126612305,-17.3532334800671,
8.2039717585113));
#163392=CARTESIAN_POINT('Ctrl Pts',(-17.3511861840082,-17.3490163805192,
8.20358682574884));
#163393=CARTESIAN_POINT('Ctrl Pts',(-17.3613395453493,-17.3403113533169,
8.20278608565162));
#163394=CARTESIAN_POINT('Ctrl Pts',(-17.3666223085158,-17.335826969454,
8.20237013890804));
#163395=CARTESIAN_POINT('Ctrl Pts',(-17.380310476479,-17.3243226352403,
8.2012940592386));
#163396=CARTESIAN_POINT('Ctrl Pts',(-17.3887484289872,-17.3173418909536,
8.20063233785863));
#163397=CARTESIAN_POINT('Ctrl Pts',(-17.4248203013454,-17.2879679700368,
8.19781002618102));
#163398=CARTESIAN_POINT('Ctrl Pts',(-17.4529607662872,-17.2662086959234,
8.19562422574354));
#163399=CARTESIAN_POINT('Ctrl Pts',(-17.5283393636975,-17.2109006007498,
8.18980676424299));
#163400=CARTESIAN_POINT('Ctrl Pts',(-17.5764272690172,-17.1785657281854,
8.18613203196921));
#163401=CARTESIAN_POINT('Ctrl Pts',(-17.7321239993493,-17.0829060098374,
8.17436007484872));
#163402=CARTESIAN_POINT('Ctrl Pts',(-17.8440352885071,-17.0271035539912,
8.16606298531998));
#163403=CARTESIAN_POINT('Ctrl Pts',(-18.0517389461217,-16.9455402139504,
8.15136548787617));
#163404=CARTESIAN_POINT('Ctrl Pts',(-18.1456854416631,-16.9160109065311,
8.14495948673951));
#163405=CARTESIAN_POINT('Ctrl Pts',(-18.2507828585176,-16.8908633776633,
8.13828278962362));
#163406=CARTESIAN_POINT('Ctrl Pts',(-18.2602267227462,-16.8886721366385,
8.13768713311243));
#163407=CARTESIAN_POINT('Ctrl Pts',(-18.2741924276083,-16.8855326435766,
8.13681294558019));
#163408=CARTESIAN_POINT('Ctrl Pts',(-18.2787026988469,-16.8845342306851,
8.13653164887833));
#163409=CARTESIAN_POINT('Ctrl Pts',(-18.2867098962466,-16.8827891967365,
8.13603411755249));
#163410=CARTESIAN_POINT('Ctrl Pts',(-18.2902054786241,-16.8820366648816,
8.13581754806249));
#163411=CARTESIAN_POINT('Ctrl Pts',(-18.2976987885946,-16.8804433532068,
8.13535465812819));
#163412=CARTESIAN_POINT('Ctrl Pts',(-18.3016970369502,-16.8796052893491,
8.13510849388291));
#163413=CARTESIAN_POINT('Ctrl Pts',(-18.3126783341471,-16.8773366869619,
8.13443459149671));
#163414=CARTESIAN_POINT('Ctrl Pts',(-18.3196662953568,-16.8759298198108,
8.13400818537423));
#163415=CARTESIAN_POINT('Ctrl Pts',(-18.3570042660396,-16.8686087005114,
8.13174214672186));
#163416=CARTESIAN_POINT('Ctrl Pts',(-18.387475715922,-16.8633242861216,
8.12993624215545));
#163417=CARTESIAN_POINT('Ctrl Pts',(-18.4800427207798,-16.8493528899776,
8.12455147563203));
#163418=CARTESIAN_POINT('Ctrl Pts',(-18.5424214181053,-16.8427541716602,
8.12105933631858));
#163419=CARTESIAN_POINT('Ctrl Pts',(-18.7637451850993,-16.8292431758982,
8.10887303959188));
#163420=CARTESIAN_POINT('Ctrl Pts',(-18.9230660517177,-16.8374703224713,
8.10043034806301));
#163421=CARTESIAN_POINT('Ctrl Pts',(-19.1420313286223,-16.8737417427372,
8.08794424482075));
#163422=CARTESIAN_POINT('Ctrl Pts',(-19.2036036178517,-16.8867837176131,
8.08433871609616));
#163423=CARTESIAN_POINT('Ctrl Pts',(-19.2765795790497,-16.9056735129481,
8.07991173654676));
#163424=CARTESIAN_POINT('Ctrl Pts',(-19.2886310067931,-16.9089069704164,
8.07917560545274));
#163425=CARTESIAN_POINT('Ctrl Pts',(-19.3083636106948,-16.9143887796491,
8.07796169024569));
#163426=CARTESIAN_POINT('Ctrl Pts',(-19.3160619743844,-16.9165745167466,
8.0774859405849));
#163427=CARTESIAN_POINT('Ctrl Pts',(-19.3298740587001,-16.920580841761,
8.07662840870397));
#163428=CARTESIAN_POINT('Ctrl Pts',(-19.3359923217147,-16.9223855209641,
8.07624714963469));
#163429=CARTESIAN_POINT('Ctrl Pts',(-19.3489988214337,-16.926285980401,
8.07543362036338));
#163430=CARTESIAN_POINT('Ctrl Pts',(-19.3558846960423,-16.9283893006809,
8.07500110721256));
#163431=CARTESIAN_POINT('Ctrl Pts',(-19.3743834357377,-16.9341431568496,
8.07383421152724));
#163432=CARTESIAN_POINT('Ctrl Pts',(-19.3859756338509,-16.9378587568447,
8.07309770024815));
#163433=CARTESIAN_POINT('Ctrl Pts',(-19.4428680027367,-16.9566368439457,
8.06945651097606));
#163434=CARTESIAN_POINT('Ctrl Pts',(-19.487678795483,-16.9731276782839,
8.06650496813699));
#163435=CARTESIAN_POINT('Ctrl Pts',(-19.6873900263417,-17.0543910295399,
8.05295881836857));
#163436=CARTESIAN_POINT('Ctrl Pts',(-19.8347920683046,-17.1359293467963,
8.04180809482539));
#163437=CARTESIAN_POINT('Ctrl Pts',(-20.0511529844362,-17.2917125524852,
8.02424610210403));
#163438=CARTESIAN_POINT('Ctrl Pts',(-20.1271874451664,-17.3549778438416,
8.01781051800602));
#163439=CARTESIAN_POINT('Ctrl Pts',(-20.2055328067276,-17.4300360762429,
8.01110703749204));
#163440=CARTESIAN_POINT('Ctrl Pts',(-20.2124872558412,-17.4367909619418,
8.0105113657937));
#163441=CARTESIAN_POINT('Ctrl Pts',(-20.222686653473,-17.4468347642197,
8.00963716030919));
#163442=CARTESIAN_POINT('Ctrl Pts',(-20.2259675191544,-17.4500867994614,
8.00935586068171));
#163443=CARTESIAN_POINT('Ctrl Pts',(-20.2317689984,-17.4558750678084,8.00885832612126));
#163444=CARTESIAN_POINT('Ctrl Pts',(-20.2342938548486,-17.4584069714019,
8.00864175630607));
#163445=CARTESIAN_POINT('Ctrl Pts',(-20.2396895475206,-17.4638452116159,
8.00817886782222));
#163446=CARTESIAN_POINT('Ctrl Pts',(-20.2425583820697,-17.4667534560756,
8.00793270534137));
#163447=CARTESIAN_POINT('Ctrl Pts',(-20.2484282710288,-17.4727385340698,
8.00742888691748));
#163448=CARTESIAN_POINT('Ctrl Pts',(-20.2514284117591,-17.4758162415899,
8.00717130164949));
#163449=CARTESIAN_POINT('Ctrl Pts',(-20.2651717970894,-17.4900011242649,
8.00599083471941));
#163450=CARTESIAN_POINT('Ctrl Pts',(-20.2758029232494,-17.5012169142555,
8.00507630456515));
#163451=CARTESIAN_POINT('Ctrl Pts',(-20.3409160821033,-17.571435220624,
7.99945873370742));
#163452=CARTESIAN_POINT('Ctrl Pts',(-20.39213258708,-17.6333880502048,7.99496712675279));
#163453=CARTESIAN_POINT('Ctrl Pts',(-20.4809155745372,-17.7541623327641,
7.98672646257819));
#163454=CARTESIAN_POINT('Ctrl Pts',(-20.519334737261,-17.8122152080738,
7.98296345890495));
#163455=CARTESIAN_POINT('Ctrl Pts',(-20.6215836030318,-17.984610550139,
7.97207000000856));
#163456=CARTESIAN_POINT('Ctrl Pts',(-20.6777317100981,-18.1030631176663,
7.96490146909176));
#163457=CARTESIAN_POINT('Ctrl Pts',(-20.7225806049454,-18.2258896932043,
7.9573447159704));
#163458=CARTESIAN_POINT('Ctrl Pts',(-20.722580563188,-18.2258895788442,
7.73405224475127));
#163459=CARTESIAN_POINT('Ctrl Pts',(-20.7064128399083,-18.1816114369415,
7.73716571128361));
#163460=CARTESIAN_POINT('Ctrl Pts',(-20.6887553875351,-18.1378434671757,
7.74027545263082));
#163461=CARTESIAN_POINT('Ctrl Pts',(-20.6434178114597,-18.0354839604616,
7.74757888317297));
#163462=CARTESIAN_POINT('Ctrl Pts',(-20.6145038161139,-17.9775334631239,
7.75173863385529));
#163463=CARTESIAN_POINT('Ctrl Pts',(-20.5765961428692,-17.9095509041066,
7.75657433186193));
#163464=CARTESIAN_POINT('Ctrl Pts',(-20.5701090062428,-17.8981668062722,
7.75738252215286));
#163465=CARTESIAN_POINT('Ctrl Pts',(-20.5608902039258,-17.8823325624502,
7.75850363688409));
#163466=CARTESIAN_POINT('Ctrl Pts',(-20.5582472891404,-17.8778314501188,
7.75882198702271));
#163467=CARTESIAN_POINT('Ctrl Pts',(-20.5537180050429,-17.8701826181471,
7.75936231920705));
#163468=CARTESIAN_POINT('Ctrl Pts',(-20.5518400585604,-17.8670299599633,
7.7595848423397));
#163469=CARTESIAN_POINT('Ctrl Pts',(-20.5482251303688,-17.8609970261551,
7.76001027891682));
#163470=CARTESIAN_POINT('Ctrl Pts',(-20.5464894768557,-17.8581159982644,
7.76021327947346));
#163471=CARTESIAN_POINT('Ctrl Pts',(-20.5418745762555,-17.8504968196842,
7.76074972697087));
#163472=CARTESIAN_POINT('Ctrl Pts',(-20.5389835463727,-17.845765784917,
7.76108240755892));
#163473=CARTESIAN_POINT('Ctrl Pts',(-20.5286654492863,-17.8290288404219,
7.76225803761003));
#163474=CARTESIAN_POINT('Ctrl Pts',(-20.5211367272519,-17.8170856234111,
7.76309458195114));
#163475=CARTESIAN_POINT('Ctrl Pts',(-20.4134239879594,-17.6499451696352,
7.7747813095825));
#163476=CARTESIAN_POINT('Ctrl Pts',(-20.2934511417893,-17.5084120593278,
7.7844807955985));
#163477=CARTESIAN_POINT('Ctrl Pts',(-20.0777212262056,-17.3126557582604,
7.80042941649284));
#163478=CARTESIAN_POINT('Ctrl Pts',(-19.9935533610791,-17.2471370468884,
7.80636528465145));
#163479=CARTESIAN_POINT('Ctrl Pts',(-19.891973940479,-17.1797068355112,
7.81345558541181));
#163480=CARTESIAN_POINT('Ctrl Pts',(-19.8790362014658,-17.1713206951283,
7.81435714305201));
#163481=CARTESIAN_POINT('Ctrl Pts',(-19.8582148828919,-17.1581452249403,
7.81580629229157));
#163482=CARTESIAN_POINT('Ctrl Pts',(-19.8503894576543,-17.1532647132715,
7.81635054159525));
#163483=CARTESIAN_POINT('Ctrl Pts',(-19.8354248252234,-17.1440669376494,
7.81739070243876));
#163484=CARTESIAN_POINT('Ctrl Pts',(-19.8282914839594,-17.1397404301115,
7.81788626429294));
#163485=CARTESIAN_POINT('Ctrl Pts',(-19.8157043192226,-17.1322074873853,
7.81876033434981));
#163486=CARTESIAN_POINT('Ctrl Pts',(-19.8102613169945,-17.128983105017,
7.81913818143699));
#163487=CARTESIAN_POINT('Ctrl Pts',(-19.7995714103964,-17.122715067949,
7.81988005997206));
#163488=CARTESIAN_POINT('Ctrl Pts',(-19.7943257125952,-17.1196694688725,
7.82024401600125));
#163489=CARTESIAN_POINT('Ctrl Pts',(-19.7817739058485,-17.112453966543,
7.82111469269163));
#163490=CARTESIAN_POINT('Ctrl Pts',(-19.7744559305445,-17.1083050088522,
7.82162216321626));
#163491=CARTESIAN_POINT('Ctrl Pts',(-19.7480707207454,-17.0935529177603,
7.82345144352715));
#163492=CARTESIAN_POINT('Ctrl Pts',(-19.7288650789912,-17.0832013476949,
7.82478219698052));
#163493=CARTESIAN_POINT('Ctrl Pts',(-19.5423649987559,-16.9863701229919,
7.83770155073751));
#163494=CARTESIAN_POINT('Ctrl Pts',(-19.3644237530526,-16.9222975968582,
7.85011675049619));
#163495=CARTESIAN_POINT('Ctrl Pts',(-19.1037882958569,-16.8660734356316,
7.86771526563253));
#163496=CARTESIAN_POINT('Ctrl Pts',(-19.0263027631822,-16.8538117887825,
7.87286101300327));
#163497=CARTESIAN_POINT('Ctrl Pts',(-18.9129431818249,-16.8422767521664,
7.88012149218994));
#163498=CARTESIAN_POINT('Ctrl Pts',(-18.8774876893382,-16.8395690608061,
7.88235431312799));
#163499=CARTESIAN_POINT('Ctrl Pts',(-18.834551196034,-16.8373762117033,
7.88499914338855));
#163500=CARTESIAN_POINT('Ctrl Pts',(-18.8271217958068,-16.8370360182797,
7.88545464626501));
#163501=CARTESIAN_POINT('Ctrl Pts',(-18.815541117558,-16.8365668781853,
7.88616117413427));
#163502=CARTESIAN_POINT('Ctrl Pts',(-18.8113910766774,-16.8364109877724,
7.88641366597596));
#163503=CARTESIAN_POINT('Ctrl Pts',(-18.8036761892909,-16.8361439206245,
7.88688171322755));
#163504=CARTESIAN_POINT('Ctrl Pts',(-18.8001115551385,-16.8360295411958,
7.88709744007462));
#163505=CARTESIAN_POINT('Ctrl Pts',(-18.7920294467235,-16.8357906517782,
7.88758536496168));
#163506=CARTESIAN_POINT('Ctrl Pts',(-18.7875118639231,-16.835671598386,
7.88785725477571));
#163507=CARTESIAN_POINT('Ctrl Pts',(-18.7741086738836,-16.8353613242715,
7.88866151892859));
#163508=CARTESIAN_POINT('Ctrl Pts',(-18.7652220780536,-16.8352115888903,
7.88919162886611));
#163509=CARTESIAN_POINT('Ctrl Pts',(-18.6985800938075,-16.8345084680831,
7.89314525863192));
#163510=CARTESIAN_POINT('Ctrl Pts',(-18.6408191802611,-16.8362628812182,
7.89644973370444));
#163511=CARTESIAN_POINT('Ctrl Pts',(-18.522535678257,-16.8447101683218,
7.90309500099272));
#163512=CARTESIAN_POINT('Ctrl Pts',(-18.4620860861765,-16.8516545308491,
7.90642560168815));
#163513=CARTESIAN_POINT('Ctrl Pts',(-18.2937982284971,-16.8783756448379,
7.9157039176958));
#163514=CARTESIAN_POINT('Ctrl Pts',(-18.1870778452132,-16.9039348484223,
7.92160300739493));
#163515=CARTESIAN_POINT('Ctrl Pts',(-18.0301233226179,-16.9546733587603,
7.93077292256164));
#163516=CARTESIAN_POINT('Ctrl Pts',(-17.978119045525,-16.9737686136473,
7.93389510610662));
#163517=CARTESIAN_POINT('Ctrl Pts',(-17.8950957247024,-17.008005644186,
7.939061225924));
#163518=CARTESIAN_POINT('Ctrl Pts',(-17.8635921539698,-17.0219055925997,
7.94106532902854));
#163519=CARTESIAN_POINT('Ctrl Pts',(-17.82265030938,-17.0411761258368,7.94373396937426));
#163520=CARTESIAN_POINT('Ctrl Pts',(-17.8128934636106,-17.0458602153299,
7.94437479746725));
#163521=CARTESIAN_POINT('Ctrl Pts',(-17.7969747400603,-17.053653274655,
7.94542851168193));
#163522=CARTESIAN_POINT('Ctrl Pts',(-17.7907913133493,-17.0567179631818,
7.94583985072366));
#163523=CARTESIAN_POINT('Ctrl Pts',(-17.7788529906393,-17.062707840171,
7.94663802249728));
#163524=CARTESIAN_POINT('Ctrl Pts',(-17.7730962658295,-17.0656292286755,
7.94702471855074));
#163525=CARTESIAN_POINT('Ctrl Pts',(-17.7598378968045,-17.0724339460696,
7.94791956038673));
#163526=CARTESIAN_POINT('Ctrl Pts',(-17.7523459908732,-17.0763359155957,
7.94842835982288));
#163527=CARTESIAN_POINT('Ctrl Pts',(-17.7322665289405,-17.0869470489114,
7.94980061753591));
#163528=CARTESIAN_POINT('Ctrl Pts',(-17.7197232635144,-17.0937386772582,
7.95066699030041));
#163529=CARTESIAN_POINT('Ctrl Pts',(-17.60473489066,-17.1575109197283,7.95869539967728));
#163530=CARTESIAN_POINT('Ctrl Pts',(-17.5071362210139,-17.222772388048,
7.9661612959015));
#163531=CARTESIAN_POINT('Ctrl Pts',(-17.2873294541717,-17.3977630813291,
7.98451540409503));
#163532=CARTESIAN_POINT('Ctrl Pts',(-17.1714785741788,-17.5142812876717,
7.99554622791961));
#163533=CARTESIAN_POINT('Ctrl Pts',(-17.0508657251224,-17.66758285754,8.00792657309285));
#163534=CARTESIAN_POINT('Ctrl Pts',(-17.0320614474767,-17.6926057853608,
8.00988633973082));
#163535=CARTESIAN_POINT('Ctrl Pts',(-17.0096473637285,-17.7238517277554,
8.01225054448643));
#163536=CARTESIAN_POINT('Ctrl Pts',(-17.005506320073,-17.7296867035592,
8.01268857134638));
#163537=CARTESIAN_POINT('Ctrl Pts',(-16.999044113337,-17.738890850831,8.013373934371));
#163538=CARTESIAN_POINT('Ctrl Pts',(-16.9967030428386,-17.7422458845879,
8.01362260085474));
#163539=CARTESIAN_POINT('Ctrl Pts',(-16.9923346023716,-17.7485452142585,
8.01408729386359));
#163540=CARTESIAN_POINT('Ctrl Pts',(-16.9903049875185,-17.7514878250175,
8.01430346888001));
#163541=CARTESIAN_POINT('Ctrl Pts',(-16.9856749524421,-17.7582371339606,
8.01479726494388));
#163542=CARTESIAN_POINT('Ctrl Pts',(-16.9830795111358,-17.7620471879733,
8.01507454717582));
#163543=CARTESIAN_POINT('Ctrl Pts',(-16.9750918462323,-17.7738556304619,
8.01592948649624));
#163544=CARTESIAN_POINT('Ctrl Pts',(-16.9697417411951,-17.7818825473233,
8.01650437258235));
#163545=CARTESIAN_POINT('Ctrl Pts',(-16.9155649449674,-17.8643819225728,
8.0223521707813));
#163546=CARTESIAN_POINT('Ctrl Pts',(-16.8714223613125,-17.9418378282073,
8.02734001015806));
#163547=CARTESIAN_POINT('Ctrl Pts',(-16.7827976071741,-18.1230338385824,
8.03842756445445));
#163548=CARTESIAN_POINT('Ctrl Pts',(-16.7414626885364,-18.2280031130629,
8.04446085537161));
#163549=CARTESIAN_POINT('Ctrl Pts',(-16.6802635317126,-18.4291406182582,
8.05601404036221));
#163550=CARTESIAN_POINT('Ctrl Pts',(-16.6583468034821,-18.5243599834351,
8.06147987673573));
#163551=CARTESIAN_POINT('Ctrl Pts',(-16.639688862379,-18.642131126821,8.06842134191135));
#163552=CARTESIAN_POINT('Ctrl Pts',(-16.6366291201695,-18.6635676838346,
8.06969165974116));
#163553=CARTESIAN_POINT('Ctrl Pts',(-16.6327571281325,-18.6940283645074,
8.07150786018356));
#163554=CARTESIAN_POINT('Ctrl Pts',(-16.631673088893,-18.703017016143,8.07204516853453));
#163555=CARTESIAN_POINT('Ctrl Pts',(-16.6299059921746,-18.7185045919187,
8.07297341329497));
#163556=CARTESIAN_POINT('Ctrl Pts',(-16.6291952998433,-18.7250002817536,
8.07336347317768));
#163557=CARTESIAN_POINT('Ctrl Pts',(-16.6278943491678,-18.7374226009045,
8.07411087865853));
#163558=CARTESIAN_POINT('Ctrl Pts',(-16.6272990048547,-18.7433486434325,
8.07446805998439));
#163559=CARTESIAN_POINT('Ctrl Pts',(-16.6258203597634,-18.7587189147403,
8.07539615226743));
#163560=CARTESIAN_POINT('Ctrl Pts',(-16.6249755189458,-18.7681666320788,
8.07596826803302));
#163561=CARTESIAN_POINT('Ctrl Pts',(-16.6223307566067,-18.8001652658668,
8.07791169720951));
#163562=CARTESIAN_POINT('Ctrl Pts',(-16.6208288713611,-18.8227386416877,
8.07929231384713));
#163563=CARTESIAN_POINT('Ctrl Pts',(-16.6106129269325,-19.0252314023213,
8.09176743605281));
#163564=CARTESIAN_POINT('Ctrl Pts',(-16.6245364211876,-19.2055224334481,
8.10360854106691));
#163565=CARTESIAN_POINT('Ctrl Pts',(-16.6781115165114,-19.4638939837152,
8.12103774288842));
#163566=CARTESIAN_POINT('Ctrl Pts',(-16.6999871318218,-19.5448797417938,
8.12655346853805));
#163567=CARTESIAN_POINT('Ctrl Pts',(-16.7383595416392,-19.6594441144297,
8.13426182023935));
#163568=CARTESIAN_POINT('Ctrl Pts',(-16.7510294389671,-19.6942170530984,
8.13658795499996));
#163569=CARTESIAN_POINT('Ctrl Pts',(-16.7673655328663,-19.7356418091579,
8.13932784163553));
#163570=CARTESIAN_POINT('Ctrl Pts',(-16.7701631744504,-19.7426266747962,
8.1397887431273));
#163571=CARTESIAN_POINT('Ctrl Pts',(-16.7745698409565,-19.7534610761508,
8.14050179926466));
#163572=CARTESIAN_POINT('Ctrl Pts',(-16.7761530733518,-19.7573209405335,
8.14075546406796));
#163573=CARTESIAN_POINT('Ctrl Pts',(-16.7791102230181,-19.7644701018884,
8.14122457811287));
#163574=CARTESIAN_POINT('Ctrl Pts',(-16.7804810253747,-19.7677605792623,
8.14144020573326));
#163575=CARTESIAN_POINT('Ctrl Pts',(-16.78359865396,-19.7751912176479,8.14192650445766));
#163576=CARTESIAN_POINT('Ctrl Pts',(-16.7853503498512,-19.779329277421,
8.14219687597448));
#163577=CARTESIAN_POINT('Ctrl Pts',(-16.7905589121293,-19.791525232701,
8.14299250876281));
#163578=CARTESIAN_POINT('Ctrl Pts',(-16.7940527268698,-19.7995673789466,
8.14351557720641));
#163579=CARTESIAN_POINT('Ctrl Pts',(-16.8196579410273,-19.8575182172999,
8.14727492078615));
#163580=CARTESIAN_POINT('Ctrl Pts',(-16.8436444222827,-19.9065813928319,
8.15040498466973));
#163581=CARTESIAN_POINT('Ctrl Pts',(-16.9483938022009,-20.1013668974881,
8.16283012690631));
#163582=CARTESIAN_POINT('Ctrl Pts',(-17.0443251215857,-20.2382503401946,
8.17160212536566));
#163583=CARTESIAN_POINT('Ctrl Pts',(-17.1953721150083,-20.407310071935,
8.18415921306798));
#163584=CARTESIAN_POINT('Ctrl Pts',(-17.237315371547,-20.4504116571376,
8.18753676215937));
#163585=CARTESIAN_POINT('Ctrl Pts',(-17.3076002275277,-20.5167386396994,
8.19308610234129));
#163586=CARTESIAN_POINT('Ctrl Pts',(-17.3348100063349,-20.5411162472607,
8.19520985096362));
#163587=CARTESIAN_POINT('Ctrl Pts',(-17.3710587847143,-20.5719390393808,
8.19801499843072));
#163588=CARTESIAN_POINT('Ctrl Pts',(-17.3795377741847,-20.5790351315997,
8.19866948196454));
#163589=CARTESIAN_POINT('Ctrl Pts',(-17.3934384697376,-20.5904847034837,
8.19973994790185));
#163590=CARTESIAN_POINT('Ctrl Pts',(-17.398826791147,-20.5948785227637,
8.20015428573892));
#163591=CARTESIAN_POINT('Ctrl Pts',(-17.4092449560198,-20.6032887401418,
8.20095428269114));
#163592=CARTESIAN_POINT('Ctrl Pts',(-17.4142716712209,-20.6073089037002,
8.20133978386204));
#163593=CARTESIAN_POINT('Ctrl Pts',(-17.4258434876823,-20.6164773600247,
8.20222614651633));
#163594=CARTESIAN_POINT('Ctrl Pts',(-17.4324007570282,-20.6216100593716,
8.20272762251858));
#163595=CARTESIAN_POINT('Ctrl Pts',(-17.4499464357885,-20.635177749541,
8.20406745434208));
#163596=CARTESIAN_POINT('Ctrl Pts',(-17.4609875035442,-20.6435436919763,
8.20490851402931));
#163597=CARTESIAN_POINT('Ctrl Pts',(-17.5485731123447,-20.7085651051935,
8.2115652898949));
#163598=CARTESIAN_POINT('Ctrl Pts',(-17.6287689212071,-20.7600978384549,
8.21757796912536));
#163599=CARTESIAN_POINT('Ctrl Pts',(-17.8666860067105,-20.8912241964742,
8.23516021750516));
#163600=CARTESIAN_POINT('Ctrl Pts',(-18.0312480610021,-20.956733889124,
8.24707830459643));
#163601=CARTESIAN_POINT('Ctrl Pts',(-18.2411031019634,-21.0112163482422,
8.26095040543944));
#163602=CARTESIAN_POINT('Ctrl Pts',(-18.2804700466945,-21.020243311074,
8.2634945107724));
#163603=CARTESIAN_POINT('Ctrl Pts',(-18.3276368306253,-21.029647093671,
8.26645492923893));
#163604=CARTESIAN_POINT('Ctrl Pts',(-18.3352080622418,-21.0311136250433,
8.26692746196168));
#163605=CARTESIAN_POINT('Ctrl Pts',(-18.3469272755842,-21.033317239552,
8.2676545660457));
#163606=CARTESIAN_POINT('Ctrl Pts',(-18.3510696362545,-21.0340833515683,
8.2679107426953));
#163607=CARTESIAN_POINT('Ctrl Pts',(-18.3587183347677,-21.0354743473582,
8.26838219448369));
#163608=CARTESIAN_POINT('Ctrl Pts',(-18.3622239363282,-21.0361027429494,
8.2685976627388));
#163609=CARTESIAN_POINT('Ctrl Pts',(-18.3701052891988,-21.0374949938178,
8.26908072072117));
#163610=CARTESIAN_POINT('Ctrl Pts',(-18.3744818546361,-21.038253923608,
8.26934802835015));
#163611=CARTESIAN_POINT('Ctrl Pts',(-18.3856745709076,-21.0401585588766,
8.27002932558514));
#163612=CARTESIAN_POINT('Ctrl Pts',(-18.392494063199,-21.0412846789427,
8.27044222896896));
#163613=CARTESIAN_POINT('Ctrl Pts',(-18.4321427621243,-21.0476326542295,
8.27283074398952));
#163614=CARTESIAN_POINT('Ctrl Pts',(-18.4650877743743,-21.0521144028249,
8.27476723001864));
#163615=CARTESIAN_POINT('Ctrl Pts',(-18.5166187648994,-21.057891890517,
8.27774022926928));
#163616=CARTESIAN_POINT('Ctrl Pts',(-18.5351378889324,-21.0597213178523,
8.27879745117047));
#163617=CARTESIAN_POINT('Ctrl Pts',(-18.584826517633,-21.0639691089502,
8.2816096837538));
#163618=CARTESIAN_POINT('Ctrl Pts',(-18.6160300361049,-21.0659416881649,
8.2833500780702));
#163619=CARTESIAN_POINT('Ctrl Pts',(-18.685727195702,-21.0687995721619,
8.28720181338053));
#163620=CARTESIAN_POINT('Ctrl Pts',(-18.724224353658,-21.0693273855509,
8.28930516530339));
#163621=CARTESIAN_POINT('Ctrl Pts',(-18.8719903821001,-21.0673228852339,
8.29735059947384));
#163622=CARTESIAN_POINT('Ctrl Pts',(-18.9809855977799,-21.0573810765956,
8.30323552927093));
#163623=CARTESIAN_POINT('Ctrl Pts',(-19.1429758788192,-21.0298489536488,
8.3123725185757));
#163624=CARTESIAN_POINT('Ctrl Pts',(-19.1968465462121,-21.0185163863954,
8.31547582423037));
#163625=CARTESIAN_POINT('Ctrl Pts',(-19.2834498509849,-20.9967416608092,
8.32061348617363));
#163626=CARTESIAN_POINT('Ctrl Pts',(-19.3164784119609,-20.9875791072288,
8.32260858218581));
#163627=CARTESIAN_POINT('Ctrl Pts',(-19.3596071828885,-20.9744790228416,
8.32526692416244));
#163628=CARTESIAN_POINT('Ctrl Pts',(-19.3699213128256,-20.9712597213976,
8.32590669380477));
#163629=CARTESIAN_POINT('Ctrl Pts',(-19.3867783020085,-20.9658562662151,
8.32695911045069));
#163630=CARTESIAN_POINT('Ctrl Pts',(-19.3933360107177,-20.963718816283,
8.32737021783749));
#163631=CARTESIAN_POINT('Ctrl Pts',(-19.4060125478574,-20.9595183264037,
8.32816825662581));
#163632=CARTESIAN_POINT('Ctrl Pts',(-19.4121326197196,-20.9574592601107,
8.32855505302561));
#163633=CARTESIAN_POINT('Ctrl Pts',(-19.4262461219506,-20.9526388544784,
8.32945058814828));
#163634=CARTESIAN_POINT('Ctrl Pts',(-19.4342325773197,-20.9498575659497,
8.32995998372255));
#163635=CARTESIAN_POINT('Ctrl Pts',(-19.455675830892,-20.9422455663165,
8.33133489276266));
#163636=CARTESIAN_POINT('Ctrl Pts',(-19.4691005302265,-20.9373263242738,
8.33220333827866));
#163637=CARTESIAN_POINT('Ctrl Pts',(-19.5923289341096,-20.8907502524256,
8.34024725615454));
#163638=CARTESIAN_POINT('Ctrl Pts',(-19.6985200913806,-20.8401668818351,
8.34772772085121));
#163639=CARTESIAN_POINT('Ctrl Pts',(-19.9414515005513,-20.6985882753817,
8.36609796588657));
#163640=CARTESIAN_POINT('Ctrl Pts',(-20.0728963838703,-20.599988625582,
8.3771289983232));
#163641=CARTESIAN_POINT('Ctrl Pts',(-20.2141769019647,-20.465845864836,
8.38949103861084));
#163642=CARTESIAN_POINT('Ctrl Pts',(-20.2362207773434,-20.4439738388089,
8.3914349759581));
#163643=CARTESIAN_POINT('Ctrl Pts',(-20.2627314453533,-20.4164862947188,
8.39378279081689));
#163644=CARTESIAN_POINT('Ctrl Pts',(-20.2676601582566,-20.4113239742267,
8.3942197195324));
#163645=CARTESIAN_POINT('Ctrl Pts',(-20.2753701279961,-20.4031663698583,
8.39490375109234));
#163646=CARTESIAN_POINT('Ctrl Pts',(-20.278168926037,-20.400187844515,8.39515217586332));
#163647=CARTESIAN_POINT('Ctrl Pts',(-20.2833998774868,-20.394588577113,
8.39561666395986));
#163648=CARTESIAN_POINT('Ctrl Pts',(-20.2858339895529,-20.3919698094932,
8.39583287430938));
#163649=CARTESIAN_POINT('Ctrl Pts',(-20.2913956837365,-20.3859557152884,
8.39632707339126));
#163650=CARTESIAN_POINT('Ctrl Pts',(-20.2945187973059,-20.3825563230121,
8.39660472123722));
#163651=CARTESIAN_POINT('Ctrl Pts',(-20.3041550132835,-20.3719985548134,
8.39746191207565));
#163652=CARTESIAN_POINT('Ctrl Pts',(-20.3106302724833,-20.36480559644,8.39803866294726));
#163653=CARTESIAN_POINT('Ctrl Pts',(-20.3791744960996,-20.2876059684725,
8.40415509886523));
#163654=CARTESIAN_POINT('Ctrl Pts',(-20.4365949716542,-20.2135931438384,
8.40937985143986));
#163655=CARTESIAN_POINT('Ctrl Pts',(-20.5627798944034,-20.0265630817037,
8.42175706785264));
#163656=CARTESIAN_POINT('Ctrl Pts',(-20.6262221693971,-19.910445244161,
8.42880643659293));
#163657=CARTESIAN_POINT('Ctrl Pts',(-20.7007281930072,-19.7373961374923,
8.43927197696545));
#163658=CARTESIAN_POINT('Ctrl Pts',(-20.7209425278633,-19.6847520627087,
8.442447726544));
#163659=CARTESIAN_POINT('Ctrl Pts',(-20.7502231670805,-19.5983354145247,
8.44769449782439));
#163660=CARTESIAN_POINT('Ctrl Pts',(-20.760596725774,-19.5650341201182,
8.44972403547661));
#163661=CARTESIAN_POINT('Ctrl Pts',(-20.7731190942457,-19.5210347587365,
8.45242173964668));
#163662=CARTESIAN_POINT('Ctrl Pts',(-20.7760149200363,-19.5105537546568,
8.45306553311528));
#163663=CARTESIAN_POINT('Ctrl Pts',(-20.7806193231252,-19.4933742952614,
8.45412288335269));
#163664=CARTESIAN_POINT('Ctrl Pts',(-20.7823760850546,-19.4866888756963,
8.45453487206151));
#163665=CARTESIAN_POINT('Ctrl Pts',(-20.7857090368825,-19.4737476843728,
8.45533342317431));
#163666=CARTESIAN_POINT('Ctrl Pts',(-20.7872894372081,-19.4674930686194,
8.45571984422475));
#163667=CARTESIAN_POINT('Ctrl Pts',(-20.7908666320066,-19.4530584371751,
8.45661277232929));
#163668=CARTESIAN_POINT('Ctrl Pts',(-20.7928432512142,-19.444873577154,
8.45711992420928));
#163669=CARTESIAN_POINT('Ctrl Pts',(-20.7980153370596,-19.4228826859008,
8.45848486374883));
#163670=CARTESIAN_POINT('Ctrl Pts',(-20.8011210529411,-19.4090561810748,
8.45934551768803));
#163671=CARTESIAN_POINT('Ctrl Pts',(-20.8354181895941,-19.2488618848786,
8.46934709518047));
#163672=CARTESIAN_POINT('Ctrl Pts',(-20.8511375064589,-19.0996426934846,
8.47899861842294));
#163673=CARTESIAN_POINT('Ctrl Pts',(-20.8508605238964,-18.8002697699751,
8.49872817936206));
#163674=CARTESIAN_POINT('Ctrl Pts',(-20.8348287879148,-18.6509266947224,
8.50874333683667));
#163675=CARTESIAN_POINT('Ctrl Pts',(-20.7998455024908,-18.4891628824865,
8.51906808111554));
#163676=CARTESIAN_POINT('Ctrl Pts',(-20.7963536193805,-18.4738437289619,
8.5200401730743));
#163677=CARTESIAN_POINT('Ctrl Pts',(-20.7913410447918,-18.452930476243,
8.52135814153985));
#163678=CARTESIAN_POINT('Ctrl Pts',(-20.7899675522461,-18.4473020803954,
8.52171194037775));
#163679=CARTESIAN_POINT('Ctrl Pts',(-20.7877485339626,-18.4383682263037,
8.52227199852567));
#163680=CARTESIAN_POINT('Ctrl Pts',(-20.7869181050291,-18.4350590999642,
8.52247911354343));
#163681=CARTESIAN_POINT('Ctrl Pts',(-20.7851867322695,-18.4282298288627,
8.52290584368497));
#163682=CARTESIAN_POINT('Ctrl Pts',(-20.7842847248074,-18.4247099942316,
8.52312539014692));
#163683=CARTESIAN_POINT('Ctrl Pts',(-20.7821142204911,-18.4163299804079,
8.52364718429002));
#163684=CARTESIAN_POINT('Ctrl Pts',(-20.7808374700019,-18.4114719224243,
8.52394895618862));
#163685=CARTESIAN_POINT('Ctrl Pts',(-20.7764750799278,-18.3951100607457,
8.52496302364301));
#163686=CARTESIAN_POINT('Ctrl Pts',(-20.7733095890909,-18.3836275243281,
8.52567085082336));
#163687=CARTESIAN_POINT('Ctrl Pts',(-20.7559961551047,-18.3228319585075,
8.52940111781873));
#163688=CARTESIAN_POINT('Ctrl Pts',(-20.740161981945,-18.2740393691834,
8.53233408680327));
#163689=CARTESIAN_POINT('Ctrl Pts',(-20.7225805426339,-18.2258895225534,
8.53521110136663));
#163690=CARTESIAN_POINT('Origin',(-18.734,-18.952,0.));
#163691=CARTESIAN_POINT('',(-20.7242503992901,-18.225264130614,9.55561792115202));
#163692=CARTESIAN_POINT('',(-20.7225805549386,-18.2258895562519,9.33206805306779));
#163693=CARTESIAN_POINT('',(-20.7225805737622,-18.2258896078036,0.));
#163694=CARTESIAN_POINT('',(-20.8516473698352,-18.9501064841217,9.51094372097752));
#163695=CARTESIAN_POINT('Ctrl Pts',(-20.8516473698352,-18.9501064841217,
9.51094372097752));
#163696=CARTESIAN_POINT('Ctrl Pts',(-20.8529700774227,-18.8071177722941,
9.51955279572483));
#163697=CARTESIAN_POINT('Ctrl Pts',(-20.8300641487808,-18.5602068596617,
9.53444419578299));
#163698=CARTESIAN_POINT('Ctrl Pts',(-20.7608945813314,-18.3228112333292,
9.54933559584116));
#163699=CARTESIAN_POINT('Ctrl Pts',(-20.7242503992901,-18.225264130614,
9.55561792115202));
#163700=CARTESIAN_POINT('Ctrl Pts',(-20.8509991358395,-18.9500871866797,
9.51057066838114));
#163701=CARTESIAN_POINT('Ctrl Pts',(-20.8511381041476,-19.1038898526281,
9.50220813078634));
#163702=CARTESIAN_POINT('Ctrl Pts',(-20.8345169833157,-19.2572409613586,
9.49391874038524));
#163703=CARTESIAN_POINT('Ctrl Pts',(-20.7961854588217,-19.4312433797309,
9.48368968190085));
#163704=CARTESIAN_POINT('Ctrl Pts',(-20.7905312722925,-19.4549534182221,
9.48227871564817));
#163705=CARTESIAN_POINT('Ctrl Pts',(-20.7813026756227,-19.4908903612793,
9.48011131877001));
#163706=CARTESIAN_POINT('Ctrl Pts',(-20.7780251063961,-19.5031918187829,
9.479364223302));
#163707=CARTESIAN_POINT('Ctrl Pts',(-20.7717280232907,-19.5259973356358,
9.47796915926823));
#163708=CARTESIAN_POINT('Ctrl Pts',(-20.768737719434,-19.5365090628525,
9.47732214536515));
#163709=CARTESIAN_POINT('Ctrl Pts',(-20.7637200154247,-19.5536424254093,
9.47626084521444));
#163710=CARTESIAN_POINT('Ctrl Pts',(-20.761741255831,-19.5602781820169,
9.47584814993044));
#163711=CARTESIAN_POINT('Ctrl Pts',(-20.75785750675,-19.573072742383,9.47504917587375));
#163712=CARTESIAN_POINT('Ctrl Pts',(-20.7559568686852,-19.5792327946707,
9.47466304349498));
#163713=CARTESIAN_POINT('Ctrl Pts',(-20.7515174988602,-19.5933911120992,
9.47377214713644));
#163714=CARTESIAN_POINT('Ctrl Pts',(-20.7489593002127,-19.6013831166627,
9.47326674770484));
#163715=CARTESIAN_POINT('Ctrl Pts',(-20.7419840095926,-19.6227363478494,
9.47190957728358));
#163716=CARTESIAN_POINT('Ctrl Pts',(-20.737481152593,-19.6360689199934,
9.47105499076286));
#163717=CARTESIAN_POINT('Ctrl Pts',(-20.6817078683167,-19.7959331739077,
9.46071961073483));
#163718=CARTESIAN_POINT('Ctrl Pts',(-20.6146125136166,-19.9364126033665,
9.45068614153466));
#163719=CARTESIAN_POINT('Ctrl Pts',(-20.4975435761416,-20.1250600647787,
9.43604111033634));
#163720=CARTESIAN_POINT('Ctrl Pts',(-20.4596328109739,-20.180147943552,
9.4316110303431));
#163721=CARTESIAN_POINT('Ctrl Pts',(-20.3826005136761,-20.2814576636098,
9.4232552919613));
#163722=CARTESIAN_POINT('Ctrl Pts',(-20.3439755690592,-20.3279800208125,
9.41932596895216));
#163723=CARTESIAN_POINT('Ctrl Pts',(-20.2831850000363,-20.395129591518,
9.41358312955422));
#163724=CARTESIAN_POINT('Ctrl Pts',(-20.2624837150291,-20.4170375189591,
9.41169737054865));
#163725=CARTESIAN_POINT('Ctrl Pts',(-20.2365531439382,-20.443331333503,
9.40942714190326));
#163726=CARTESIAN_POINT('Ctrl Pts',(-20.23176248186,-20.4481425892795,9.40901144210383));
#163727=CARTESIAN_POINT('Ctrl Pts',(-20.223992842341,-20.4558709090437,
9.40834335725904));
#163728=CARTESIAN_POINT('Ctrl Pts',(-20.2210282944535,-20.4588023206387,
9.40808986623123));
#163729=CARTESIAN_POINT('Ctrl Pts',(-20.2155127958052,-20.4642240390669,
9.40762091128048));
#163730=CARTESIAN_POINT('Ctrl Pts',(-20.2129642379326,-20.4667166374173,
9.40740527000457));
#163731=CARTESIAN_POINT('Ctrl Pts',(-20.20718628661,-20.4723392351493,9.40691873511417));
#163732=CARTESIAN_POINT('Ctrl Pts',(-20.2039532171942,-20.4754653803445,
9.40664814234676));
#163733=CARTESIAN_POINT('Ctrl Pts',(-20.1943749666198,-20.4846679810913,
9.40585125447342));
#163734=CARTESIAN_POINT('Ctrl Pts',(-20.1880018047704,-20.4907153541721,
9.40532716253214));
#163735=CARTESIAN_POINT('Ctrl Pts',(-20.1414361787023,-20.5343529410136,
9.40154057571614));
#163736=CARTESIAN_POINT('Ctrl Pts',(-20.0998255060236,-20.5704063838509,
9.39838604534943));
#163737=CARTESIAN_POINT('Ctrl Pts',(-20.0338650780997,-20.6231991996844,
9.3936413069055));
#163738=CARTESIAN_POINT('Ctrl Pts',(-20.0104948014801,-20.6411172572354,
9.39200641224539));
#163739=CARTESIAN_POINT('Ctrl Pts',(-19.8687657542256,-20.7451592964801,
9.38231535700458));
#163740=CARTESIAN_POINT('Ctrl Pts',(-19.7421104641031,-20.8193050860912,
9.37453712299876));
#163741=CARTESIAN_POINT('Ctrl Pts',(-19.5598230291656,-20.9020256416392,
9.36339458171594));
#163742=CARTESIAN_POINT('Ctrl Pts',(-19.5100026002917,-20.922381444268,
9.36035785293675));
#163743=CARTESIAN_POINT('Ctrl Pts',(-19.4279206572899,-20.9523225865046,
9.35532859778322));
#163744=CARTESIAN_POINT('Ctrl Pts',(-19.3961100711623,-20.9630759303931,
9.35337353151184));
#163745=CARTESIAN_POINT('Ctrl Pts',(-19.3537416006921,-20.9762841031516,
9.35075617822109));
#163746=CARTESIAN_POINT('Ctrl Pts',(-19.3434004072266,-20.9794212485368,
9.35011630906469));
#163747=CARTESIAN_POINT('Ctrl Pts',(-19.3264200364059,-20.9844308298599,
9.34906377043415));
#163748=CARTESIAN_POINT('Ctrl Pts',(-19.3197948436101,-20.9863502592151,
9.34865264127785));
#163749=CARTESIAN_POINT('Ctrl Pts',(-19.3069497415364,-20.9900037504982,
9.34785459005441));
#163750=CARTESIAN_POINT('Ctrl Pts',(-19.3007310394531,-20.9917418024982,
9.34746780314688));
#163751=CARTESIAN_POINT('Ctrl Pts',(-19.286350308711,-20.9956902016434,
9.3465723334617));
#163752=CARTESIAN_POINT('Ctrl Pts',(-19.2781828346788,-20.9978801389687,
9.34606299413454));
#163753=CARTESIAN_POINT('Ctrl Pts',(-19.2561739646419,-21.0036402411046,
9.34468833531461));
#163754=CARTESIAN_POINT('Ctrl Pts',(-19.2423093518582,-21.0071191973585,
9.34382008543131));
#163755=CARTESIAN_POINT('Ctrl Pts',(-19.1144643894697,-21.0378256544474,
9.33579182406495));
#163756=CARTESIAN_POINT('Ctrl Pts',(-18.9984611491077,-21.0556811168636,
9.32832819637869));
#163757=CARTESIAN_POINT('Ctrl Pts',(-18.7181701751453,-21.075270069993,
9.30997281786804));
#163758=CARTESIAN_POINT('Ctrl Pts',(-18.5539784407095,-21.0676840157774,
9.29893810294639));
#163759=CARTESIAN_POINT('Ctrl Pts',(-18.361482832506,-21.0362013693955,
9.28655902439747));
#163760=CARTESIAN_POINT('Ctrl Pts',(-18.3307745008561,-21.0304787285515,
9.28460334716877));
#163761=CARTESIAN_POINT('Ctrl Pts',(-18.2932036206526,-21.0226131168049,
9.28224337530656));
#163762=CARTESIAN_POINT('Ctrl Pts',(-18.2862123482478,-21.0211124546123,
9.28180563118817));
#163763=CARTESIAN_POINT('Ctrl Pts',(-18.2752341694001,-21.0186977623501,
9.28112061096522));
#163764=CARTESIAN_POINT('Ctrl Pts',(-18.2712421548218,-21.01780756742,9.28087200670439));
#163765=CARTESIAN_POINT('Ctrl Pts',(-18.263765793451,-21.0161176252269,
9.2804073665353));
#163766=CARTESIAN_POINT('Ctrl Pts',(-18.2602809326335,-21.0153206307328,
9.28019118251321));
#163767=CARTESIAN_POINT('Ctrl Pts',(-18.2523051187396,-21.0134752747015,
9.27969728310955));
#163768=CARTESIAN_POINT('Ctrl Pts',(-18.2478155691192,-21.0124210654451,
9.27941990707483));
#163769=CARTESIAN_POINT('Ctrl Pts',(-18.2360631289159,-21.0096208759835,
9.27869539730786));
#163770=CARTESIAN_POINT('Ctrl Pts',(-18.2288058989922,-21.0078510940494,
9.27824959650462));
#163771=CARTESIAN_POINT('Ctrl Pts',(-18.1802070805174,-20.9957266771959,
9.27527398984196));
#163772=CARTESIAN_POINT('Ctrl Pts',(-18.1391738450166,-20.9841633118678,
9.27280893696925));
#163773=CARTESIAN_POINT('Ctrl Pts',(-18.0895913035468,-20.9685599285352,
9.26985736773424));
#163774=CARTESIAN_POINT('Ctrl Pts',(-18.0806864686085,-20.9656926149575,
9.26932835920203));
#163775=CARTESIAN_POINT('Ctrl Pts',(-18.0582615546534,-20.9583074905242,
9.2679982349122));
#163776=CARTESIAN_POINT('Ctrl Pts',(-18.0447674411228,-20.9537119388753,
9.26719974487325));
#163777=CARTESIAN_POINT('Ctrl Pts',(-17.8963683822808,-20.9014946163468,
9.2584294569468));
#163778=CARTESIAN_POINT('Ctrl Pts',(-17.7665730417788,-20.840450405558,
9.25083404290633));
#163779=CARTESIAN_POINT('Ctrl Pts',(-17.5642102998977,-20.7188977232798,
9.23783370955003));
#163780=CARTESIAN_POINT('Ctrl Pts',(-17.4877481080449,-20.6658228708152,
9.23261305367473));
#163781=CARTESIAN_POINT('Ctrl Pts',(-17.3985207912997,-20.5947506203344,
9.22596857980004));
#163782=CARTESIAN_POINT('Ctrl Pts',(-17.3822125405451,-20.5813572151364,
9.22473009213701));
#163783=CARTESIAN_POINT('Ctrl Pts',(-17.3592686770775,-20.5619326337178,
9.22295165380776));
#163784=CARTESIAN_POINT('Ctrl Pts',(-17.3524666128674,-20.5560993709279,
9.22241979314118));
#163785=CARTESIAN_POINT('Ctrl Pts',(-17.3407814593065,-20.5459490507351,
9.22149800089068));
#163786=CARTESIAN_POINT('Ctrl Pts',(-17.3358808597868,-20.5416522722835,
9.22110891354562));
#163787=CARTESIAN_POINT('Ctrl Pts',(-17.3265256691613,-20.5333730460088,
9.2203612998821));
#163788=CARTESIAN_POINT('Ctrl Pts',(-17.3220679377208,-20.5293942287784,
9.220002927831));
#163789=CARTESIAN_POINT('Ctrl Pts',(-17.3104982747064,-20.5189792092125,
9.21906718185095));
#163790=CARTESIAN_POINT('Ctrl Pts',(-17.3034131946583,-20.5125135025574,
9.21848856323691));
#163791=CARTESIAN_POINT('Ctrl Pts',(-17.279292035105,-20.4901986724106,
9.21649923682406));
#163792=CARTESIAN_POINT('Ctrl Pts',(-17.2624739176394,-20.4741173870864,
9.21507861821106));
#163793=CARTESIAN_POINT('Ctrl Pts',(-17.1239722440033,-20.3372426230275,
9.20308976205596));
#163794=CARTESIAN_POINT('Ctrl Pts',(-17.0171345894265,-20.2023750407871,
9.19185378569772));
#163795=CARTESIAN_POINT('Ctrl Pts',(-16.8808718570458,-19.9794635054932,
9.17458946507389));
#163796=CARTESIAN_POINT('Ctrl Pts',(-16.8389276933185,-19.8998755760097,
9.16865950876779));
#163797=CARTESIAN_POINT('Ctrl Pts',(-16.7864056199242,-19.7826925966121,
9.16045580284078));
#163798=CARTESIAN_POINT('Ctrl Pts',(-16.7716060658502,-19.7471003323287,
9.15803060990445));
#163799=CARTESIAN_POINT('Ctrl Pts',(-16.7550559687385,-19.7040156008535,
9.15519024756636));
#163800=CARTESIAN_POINT('Ctrl Pts',(-16.7523647218982,-19.6968950069744,
9.15472389814967));
#163801=CARTESIAN_POINT('Ctrl Pts',(-16.7482513643726,-19.6858316703895,
9.1540042591649));
#163802=CARTESIAN_POINT('Ctrl Pts',(-16.746802488259,-19.6818990439752,
9.1537494151912));
#163803=CARTESIAN_POINT('Ctrl Pts',(-16.7441434536272,-19.6746151257614,
9.15327921241018));
#163804=CARTESIAN_POINT('Ctrl Pts',(-16.7429300871859,-19.6712651094804,
9.15306366828498));
#163805=CARTESIAN_POINT('Ctrl Pts',(-16.7402139558944,-19.663706526441,
9.15257893036685));
#163806=CARTESIAN_POINT('Ctrl Pts',(-16.7387160599745,-19.6594962678115,
9.15231002778688));
#163807=CARTESIAN_POINT('Ctrl Pts',(-16.734356889319,-19.6471196337873,
9.15152270458673));
#163808=CARTESIAN_POINT('Ctrl Pts',(-16.73153229896,-19.6389403085139,9.15100640896423));
#163809=CARTESIAN_POINT('Ctrl Pts',(-16.7121496273789,-19.5816772396143,
9.14741837822285));
#163810=CARTESIAN_POINT('Ctrl Pts',(-16.6973463967351,-19.5320132733231,
9.14444217897079));
#163811=CARTESIAN_POINT('Ctrl Pts',(-16.6790027014076,-19.4610545598867,
9.14031504517448));
#163812=CARTESIAN_POINT('Ctrl Pts',(-16.6739430224537,-19.4401759260615,
9.1391157729302));
#163813=CARTESIAN_POINT('Ctrl Pts',(-16.6387826487345,-19.284791865949,
9.13027867056794));
#163814=CARTESIAN_POINT('Ctrl Pts',(-16.6215637283688,-19.147708582813,
9.12294817445163));
#163815=CARTESIAN_POINT('Ctrl Pts',(-16.615309099425,-18.9191858084987,
9.11034446304863));
#163816=CARTESIAN_POINT('Ctrl Pts',(-16.6186638528939,-18.8283951773765,
9.10524206797293));
#163817=CARTESIAN_POINT('Ctrl Pts',(-16.6299380705484,-18.7173803260278,
9.0987406747198));
#163818=CARTESIAN_POINT('Ctrl Pts',(-16.6323486712366,-18.6966871702582,
9.09751780252641));
#163819=CARTESIAN_POINT('Ctrl Pts',(-16.6362262763969,-18.6671950257068,
9.09575791970911));
#163820=CARTESIAN_POINT('Ctrl Pts',(-16.6374441524653,-18.6583640974157,
9.09522876664305));
#163821=CARTESIAN_POINT('Ctrl Pts',(-16.6396477465044,-18.6430987063396,
9.09431017162974));
#163822=CARTESIAN_POINT('Ctrl Pts',(-16.6406074397981,-18.6366605664067,
9.09392155796625));
#163823=CARTESIAN_POINT('Ctrl Pts',(-16.6425065312993,-18.6243112852303,
9.09317379951298));
#163824=CARTESIAN_POINT('Ctrl Pts',(-16.643441336852,-18.618399493108,9.09281480392395));
#163825=CARTESIAN_POINT('Ctrl Pts',(-16.6459483158343,-18.6029695854948,
9.09187508268392));
#163826=CARTESIAN_POINT('Ctrl Pts',(-16.6475604889846,-18.5934581920447,
9.09129309150555));
#163827=CARTESIAN_POINT('Ctrl Pts',(-16.6533404890244,-18.560717538348,
9.0892801540355));
#163828=CARTESIAN_POINT('Ctrl Pts',(-16.6578315864026,-18.5375478157145,
9.08783897823118));
#163829=CARTESIAN_POINT('Ctrl Pts',(-16.6968556528412,-18.352810501556,
9.07621020717517));
#163830=CARTESIAN_POINT('Ctrl Pts',(-16.7498017832939,-18.1957441785992,
9.06540809439343));
#163831=CARTESIAN_POINT('Ctrl Pts',(-16.8749495067224,-17.9312866457703,
9.04607356575698));
#163832=CARTESIAN_POINT('Ctrl Pts',(-16.9397450201553,-17.8212567516476,
9.03764617730179));
#163833=CARTESIAN_POINT('Ctrl Pts',(-17.0210404729426,-17.7079733055976,
9.02899840108267));
#163834=CARTESIAN_POINT('Ctrl Pts',(-17.0281138238902,-17.6982914504789,
9.02825969768888));
#163835=CARTESIAN_POINT('Ctrl Pts',(-17.0382747907705,-17.6846285544052,
9.02721841419493));
#163836=CARTESIAN_POINT('Ctrl Pts',(-17.0412947946315,-17.680597838901,
9.0269113689375));
#163837=CARTESIAN_POINT('Ctrl Pts',(-17.0465196874146,-17.6736759353483,
9.0263843907951));
#163838=CARTESIAN_POINT('Ctrl Pts',(-17.0487176834492,-17.6707795919789,
9.02616398035468));
#163839=CARTESIAN_POINT('Ctrl Pts',(-17.0529903633942,-17.6651794157292,
9.02573801159993));
#163840=CARTESIAN_POINT('Ctrl Pts',(-17.0550641144242,-17.6624749296854,
9.02553238808375));
#163841=CARTESIAN_POINT('Ctrl Pts',(-17.0606692307923,-17.6552014487085,
9.02497958632524));
#163842=CARTESIAN_POINT('Ctrl Pts',(-17.0642128045286,-17.6506418366078,
9.02463326373037));
#163843=CARTESIAN_POINT('Ctrl Pts',(-17.0773899393621,-17.6338288985197,
9.02335682177934));
#163844=CARTESIAN_POINT('Ctrl Pts',(-17.087140349686,-17.6216672334073,
9.02243464057827));
#163845=CARTESIAN_POINT('Ctrl Pts',(-17.1836987557838,-17.5039188801019,
9.01350504256178));
#163846=CARTESIAN_POINT('Ctrl Pts',(-17.2804185889484,-17.4068513557522,
9.00612170206973));
#163847=CARTESIAN_POINT('Ctrl Pts',(-17.504977073461,-17.2213728878404,
8.99030511144564));
#163848=CARTESIAN_POINT('Ctrl Pts',(-17.6345175939576,-17.1363187132246,
8.98188562765167));
#163849=CARTESIAN_POINT('Ctrl Pts',(-17.7911005486999,-17.0564573234692,
8.97164911556871));
#163850=CARTESIAN_POINT('Ctrl Pts',(-17.8101924711805,-17.0470797877685,
8.97040094469934));
#163851=CARTESIAN_POINT('Ctrl Pts',(-17.8375492459361,-17.0341507222992,
8.96861100998308));
#163852=CARTESIAN_POINT('Ctrl Pts',(-17.8457008240836,-17.0303615385017,
8.96807748196929));
#163853=CARTESIAN_POINT('Ctrl Pts',(-17.8598084666157,-17.0239126813327,
8.96715371755052));
#163854=CARTESIAN_POINT('Ctrl Pts',(-17.8657531888928,-17.0212283876698,
8.96676433523984));
#163855=CARTESIAN_POINT('Ctrl Pts',(-17.8771616918953,-17.0161403087556,
8.96601679682546));
#163856=CARTESIAN_POINT('Ctrl Pts',(-17.8826234277886,-17.0137320717775,
8.96565879807748));
#163857=CARTESIAN_POINT('Ctrl Pts',(-17.8968576469632,-17.007527565476,
8.96472544240179));
#163858=CARTESIAN_POINT('Ctrl Pts',(-17.905645714064,-17.0037675856932,
8.96414885327789));
#163859=CARTESIAN_POINT('Ctrl Pts',(-17.9357273911675,-16.9911374510831,
8.96217383329906));
#163860=CARTESIAN_POINT('Ctrl Pts',(-17.9571397857485,-16.9825561101635,
8.96076568283578));
#163861=CARTESIAN_POINT('Ctrl Pts',(-18.1416936516153,-16.9120713442594,
8.9486048803617));
#163862=CARTESIAN_POINT('Ctrl Pts',(-18.3117422850142,-16.8702192482116,
8.93715757058177));
#163863=CARTESIAN_POINT('Ctrl Pts',(-18.5720581959768,-16.8393814125528,
8.9198371751882));
#163864=CARTESIAN_POINT('Ctrl Pts',(-18.6597241630551,-16.8344855422463,
8.91405468550886));
#163865=CARTESIAN_POINT('Ctrl Pts',(-18.7854445872254,-16.8352840464526,
8.9060266176787));
#163866=CARTESIAN_POINT('Ctrl Pts',(-18.8234329098846,-16.836548477608,
8.90363605743844));
#163867=CARTESIAN_POINT('Ctrl Pts',(-18.8689372456965,-16.8392912118718,
8.90083077414067));
#163868=CARTESIAN_POINT('Ctrl Pts',(-18.876502939195,-16.8397880314644,
8.90036629757931));
#163869=CARTESIAN_POINT('Ctrl Pts',(-18.888239837257,-16.8406221129123,
8.89964892102637));
#163870=CARTESIAN_POINT('Ctrl Pts',(-18.8924128972011,-16.8409311086135,
8.89939448190194));
#163871=CARTESIAN_POINT('Ctrl Pts',(-18.9001380751228,-16.841526157744,
8.89892465470663));
#163872=CARTESIAN_POINT('Ctrl Pts',(-18.9036903565058,-16.8418088043824,
8.89870908369598));
#163873=CARTESIAN_POINT('Ctrl Pts',(-18.9117040926966,-16.8424668051863,
8.89822381799846));
#163874=CARTESIAN_POINT('Ctrl Pts',(-18.9161650676632,-16.8428473422836,
8.8979544173659));
#163875=CARTESIAN_POINT('Ctrl Pts',(-18.9292829715273,-16.844008275337,
8.89716428121397));
#163876=CARTESIAN_POINT('Ctrl Pts',(-18.9379364610857,-16.8448278485328,
8.8966456935359));
#163877=CARTESIAN_POINT('Ctrl Pts',(-18.999056550301,-16.8509965841484,
8.89300001592043));
#163878=CARTESIAN_POINT('Ctrl Pts',(-19.0513168421041,-16.8582518445311,
8.88997199161438));
#163879=CARTESIAN_POINT('Ctrl Pts',(-19.1188003152317,-16.8702058393252,
8.88611580285936));
#163880=CARTESIAN_POINT('Ctrl Pts',(-19.1343136997619,-16.873133200655,
8.88523307620626));
#163881=CARTESIAN_POINT('Ctrl Pts',(-19.199644025459,-16.8862194061496,
8.88152631588851));
#163882=CARTESIAN_POINT('Ctrl Pts',(-19.2491207459418,-16.8979978613761,
8.87874487186873));
#163883=CARTESIAN_POINT('Ctrl Pts',(-19.4035796536921,-16.940701321278,
8.87001970660592));
#163884=CARTESIAN_POINT('Ctrl Pts',(-19.5066126375289,-16.9779867976233,
8.86412872711329));
#163885=CARTESIAN_POINT('Ctrl Pts',(-19.6565774913472,-17.0458035922493,
8.85497767308567));
#163886=CARTESIAN_POINT('Ctrl Pts',(-19.7059453799687,-17.0704964779932,
8.85186630565953));
#163887=CARTESIAN_POINT('Ctrl Pts',(-19.7843784777631,-17.1136384256498,
8.84671648862589));
#163888=CARTESIAN_POINT('Ctrl Pts',(-19.8140584803238,-17.1309174355497,
8.84471754338035));
#163889=CARTESIAN_POINT('Ctrl Pts',(-19.8525132559002,-17.1545757292901,
8.84205479995177));
#163890=CARTESIAN_POINT('Ctrl Pts',(-19.8616788922531,-17.1603119071771,
8.84141457744484));
#163891=CARTESIAN_POINT('Ctrl Pts',(-19.876619979032,-17.1698226296123,
8.84036160564818));
#163892=CARTESIAN_POINT('Ctrl Pts',(-19.8824217030079,-17.1735556836569,
8.83995039916686));
#163893=CARTESIAN_POINT('Ctrl Pts',(-19.8936175179121,-17.1808371337984,
8.83915230365066));
#163894=CARTESIAN_POINT('Ctrl Pts',(-19.8990138327789,-17.184381982876,
8.83876555033536));
#163895=CARTESIAN_POINT('Ctrl Pts',(-19.9114372705261,-17.192624564624,
8.83787031252863));
#163896=CARTESIAN_POINT('Ctrl Pts',(-19.9184526071277,-17.1973397859244,
8.83736117255716));
#163897=CARTESIAN_POINT('Ctrl Pts',(-19.9372457725075,-17.2101353045223,
8.83598740051634));
#163898=CARTESIAN_POINT('Ctrl Pts',(-19.9489702181702,-17.2182928852677,
8.83511984393464));
#163899=CARTESIAN_POINT('Ctrl Pts',(-20.0755780804865,-17.3082985336551,
8.82563486559488));
#163900=CARTESIAN_POINT('Ctrl Pts',(-20.1820673903348,-17.4012989519405,
8.81656774780422));
#163901=CARTESIAN_POINT('Ctrl Pts',(-20.3445946017893,-17.5746792090217,
8.80093336788623));
#163902=CARTESIAN_POINT('Ctrl Pts',(-20.4057792782527,-17.6496245639738,
8.79450519601258));
#163903=CARTESIAN_POINT('Ctrl Pts',(-20.4993339368746,-17.7817261076463,
8.78394205739131));
#163904=CARTESIAN_POINT('Ctrl Pts',(-20.5345603061946,-17.8366842997629,
8.77974793333697));
#163905=CARTESIAN_POINT('Ctrl Pts',(-20.5737749643587,-17.9045792771297,
8.77487649203968));
#163906=CARTESIAN_POINT('Ctrl Pts',(-20.58024894635,-17.9160333314806,8.77406490345128));
#163907=CARTESIAN_POINT('Ctrl Pts',(-20.5891459494667,-17.9321226344458,
8.77293990512952));
#163908=CARTESIAN_POINT('Ctrl Pts',(-20.5916590625786,-17.9367073608292,
8.7726210204753));
#163909=CARTESIAN_POINT('Ctrl Pts',(-20.595907905499,-17.9445272067099,
8.77208005258767));
#163910=CARTESIAN_POINT('Ctrl Pts',(-20.5976522428747,-17.947757600909,
8.77185742524005));
#163911=CARTESIAN_POINT('Ctrl Pts',(-20.6009776731519,-17.9539545762238,
8.77143199582076));
#163912=CARTESIAN_POINT('Ctrl Pts',(-20.6025601087192,-17.9569203949248,
8.77122910564776));
#163913=CARTESIAN_POINT('Ctrl Pts',(-20.6067291654024,-17.9647791009159,
8.77069335629071));
#163914=CARTESIAN_POINT('Ctrl Pts',(-20.609303695573,-17.969678422573,8.77036125971394));
#163915=CARTESIAN_POINT('Ctrl Pts',(-20.618348793068,-17.9870563708885,
8.76918983413319));
#163916=CARTESIAN_POINT('Ctrl Pts',(-20.6247144223299,-17.999589595726,
8.76835685001149));
#163917=CARTESIAN_POINT('Ctrl Pts',(-20.6654151825277,-18.0817414688069,
8.76296784094099));
#163918=CARTESIAN_POINT('Ctrl Pts',(-20.6959972252147,-18.1530864111672,
8.75861684946317));
#163919=CARTESIAN_POINT('Ctrl Pts',(-20.7225806939367,-18.2258899369226,
8.75434681593714));
#163920=CARTESIAN_POINT('',(-20.8509999019998,-18.9526441527879,9.29097295163941));
#163921=CARTESIAN_POINT('Ctrl Pts',(-20.7225805426339,-18.2258895225534,
8.53521110136663));
#163922=CARTESIAN_POINT('Ctrl Pts',(-20.6972665242699,-18.1565626557224,
8.53935346981564));
#163923=CARTESIAN_POINT('Ctrl Pts',(-20.6683303334796,-18.0885682846539,
8.54338079649807));
#163924=CARTESIAN_POINT('Ctrl Pts',(-20.5622083440441,-17.8715011606762,
8.55651370999459));
#163925=CARTESIAN_POINT('Ctrl Pts',(-20.4709010471761,-17.7301197687966,
8.56556717419578));
#163926=CARTESIAN_POINT('Ctrl Pts',(-20.3488895493943,-17.5829229611688,
8.57667158329379));
#163927=CARTESIAN_POINT('Ctrl Pts',(-20.3336077518508,-17.5650987164041,
8.57804658318816));
#163928=CARTESIAN_POINT('Ctrl Pts',(-20.3116465924116,-17.5403297476765,
8.58000258058673));
#163929=CARTESIAN_POINT('Ctrl Pts',(-20.3052110916489,-17.5331704215547,
8.58057342378957));
#163930=CARTESIAN_POINT('Ctrl Pts',(-20.2946981030954,-17.5216342392475,
8.58150230232897));
#163931=CARTESIAN_POINT('Ctrl Pts',(-20.2906504545105,-17.5172302833276,
8.58185907151936));
#163932=CARTESIAN_POINT('Ctrl Pts',(-20.2821570953286,-17.5080675159734,
8.58260593747009));
#163933=CARTESIAN_POINT('Ctrl Pts',(-20.2777079871463,-17.5033119524227,
8.58299617765471));
#163934=CARTESIAN_POINT('Ctrl Pts',(-20.2671051351112,-17.4920830789144,
8.58392387591232));
#163935=CARTESIAN_POINT('Ctrl Pts',(-20.2609322647377,-17.4856280734894,
8.58446215778479));
#163936=CARTESIAN_POINT('Ctrl Pts',(-20.2401569148386,-17.4641765992511,
8.58626791079944));
#163937=CARTESIAN_POINT('Ctrl Pts',(-20.2253732608154,-17.4493580361652,
8.58754329127387));
#163938=CARTESIAN_POINT('Ctrl Pts',(-20.1447383747647,-17.3708949945944,
8.59445101743442));
#163939=CARTESIAN_POINT('Ctrl Pts',(-20.0750376008408,-17.3113628780678,
8.60025767198204));
#163940=CARTESIAN_POINT('Ctrl Pts',(-19.9260794546773,-17.1999859093171,
8.61232141509067));
#163941=CARTESIAN_POINT('Ctrl Pts',(-19.8467532513525,-17.1485629253094,
8.61857370208974));
#163942=CARTESIAN_POINT('Ctrl Pts',(-19.69941499979,-17.0664832361175,8.62971091800337));
#163943=CARTESIAN_POINT('Ctrl Pts',(-19.6327063508674,-17.033790487146,
8.63459304918896));
#163944=CARTESIAN_POINT('Ctrl Pts',(-19.5255532143106,-16.9880963979304,
8.64206175425803));
#163945=CARTESIAN_POINT('Ctrl Pts',(-19.4862012034366,-16.9726900820359,
8.64472886806517));
#163946=CARTESIAN_POINT('Ctrl Pts',(-19.4393956540965,-16.9559635572666,
8.64779175402888));
#163947=CARTESIAN_POINT('Ctrl Pts',(-19.4323664130114,-16.953493340899,
8.64824887347503));
#163948=CARTESIAN_POINT('Ctrl Pts',(-19.4209708582735,-16.9495561797331,
8.64898514491787));
#163949=CARTESIAN_POINT('Ctrl Pts',(-19.4166126125074,-16.9480663095767,
8.64926560284719));
#163950=CARTESIAN_POINT('Ctrl Pts',(-19.4088636488684,-16.9454455325902,
8.64976220818604));
#163951=CARTESIAN_POINT('Ctrl Pts',(-19.4054748993097,-16.944308979072,
8.64997868581606));
#163952=CARTESIAN_POINT('Ctrl Pts',(-19.3981986904133,-16.9418890930745,
8.6504419979075));
#163953=CARTESIAN_POINT('Ctrl Pts',(-19.3943103934574,-16.9406084559607,
8.65068867293238));
#163954=CARTESIAN_POINT('Ctrl Pts',(-19.3836044849367,-16.937116782336,
8.65136541617538));
#163955=CARTESIAN_POINT('Ctrl Pts',(-19.3767792490089,-16.9349290522986,
8.65179413359938));
#163956=CARTESIAN_POINT('Ctrl Pts',(-19.3399295280785,-16.9233234458084,
8.65409481638683));
#163957=CARTESIAN_POINT('Ctrl Pts',(-19.3097072852235,-16.9145406716367,
8.65593182017731));
#163958=CARTESIAN_POINT('Ctrl Pts',(-19.1212225674714,-16.86429516803,8.66714519059627));
#163959=CARTESIAN_POINT('Ctrl Pts',(-18.9587779967234,-16.8406165954596,
8.67579052725774));
#163960=CARTESIAN_POINT('Ctrl Pts',(-18.6781394616569,-16.832498599573,
8.69115902284257));
#163961=CARTESIAN_POINT('Ctrl Pts',(-18.5610028698173,-16.8388333500567,
8.69769648655017));
#163962=CARTESIAN_POINT('Ctrl Pts',(-18.4308397096218,-16.8567703827533,
8.70539390519138));
#163963=CARTESIAN_POINT('Ctrl Pts',(-18.4167001908331,-16.8588650003329,
8.70623563542497));
#163964=CARTESIAN_POINT('Ctrl Pts',(-18.3942316636953,-16.8624263644267,
8.70758250453314));
#163965=CARTESIAN_POINT('Ctrl Pts',(-18.3858882073737,-16.8638001346833,
8.70808470020775));
#163966=CARTESIAN_POINT('Ctrl Pts',(-18.3711884697787,-16.866311028332,
8.70897318841858));
#163967=CARTESIAN_POINT('Ctrl Pts',(-18.3648287057149,-16.8674273226751,
8.70935881456289));
#163968=CARTESIAN_POINT('Ctrl Pts',(-18.3516858596697,-16.8697962451304,
8.71015831432772));
#163969=CARTESIAN_POINT('Ctrl Pts',(-18.3449036013917,-16.8710529633054,
8.71057231412069));
#163970=CARTESIAN_POINT('Ctrl Pts',(-18.3275114001116,-16.8743636489613,
8.71163767683571));
#163971=CARTESIAN_POINT('Ctrl Pts',(-18.3169109201649,-16.8764657358413,
8.71229056844244));
#163972=CARTESIAN_POINT('Ctrl Pts',(-18.2727439827485,-16.8855761077512,
8.71502600536989));
#163973=CARTESIAN_POINT('Ctrl Pts',(-18.2393357382228,-16.8933179293513,
8.71713186872803));
#163974=CARTESIAN_POINT('Ctrl Pts',(-18.1527992824592,-16.9155993415684,
8.72268614556567));
#163975=CARTESIAN_POINT('Ctrl Pts',(-18.100026993056,-16.9314061955281,
8.72617294103055));
#163976=CARTESIAN_POINT('Ctrl Pts',(-17.9444687753924,-16.9846945372803,
8.73674191965459));
#163977=CARTESIAN_POINT('Ctrl Pts',(-17.8439124925375,-17.0281000283955,
8.74397249551155));
#163978=CARTESIAN_POINT('Ctrl Pts',(-17.7067694966179,-17.100359753312,
8.75421242629077));
#163979=CARTESIAN_POINT('Ctrl Pts',(-17.6670694038645,-17.1229474026885,
8.75722324029487));
#163980=CARTESIAN_POINT('Ctrl Pts',(-17.6086454621591,-17.1587380864235,
8.76169862425411));
#163981=CARTESIAN_POINT('Ctrl Pts',(-17.5893548707656,-17.1709894140694,
8.76318384235468));
#163982=CARTESIAN_POINT('Ctrl Pts',(-17.5696699074774,-17.1839431726464,
8.76470463059978));
#163983=CARTESIAN_POINT('Ctrl Pts',(-17.5690740650417,-17.1843357006578,
8.76475066816479));
#163984=CARTESIAN_POINT('Ctrl Pts',(-17.5588413988646,-17.1910841790031,
8.76554137549075));
#163985=CARTESIAN_POINT('Ctrl Pts',(-17.5492563645857,-17.1975186539752,
8.76628331708627));
#163986=CARTESIAN_POINT('Ctrl Pts',(-17.5067680482133,-17.2265482153437,
8.76957635694986));
#163987=CARTESIAN_POINT('Ctrl Pts',(-17.4744526720219,-17.2499943813663,
8.77209231810606));
#163988=CARTESIAN_POINT('Ctrl Pts',(-17.4370127209066,-17.2788094399821,
8.7750028301279));
#163989=CARTESIAN_POINT('Ctrl Pts',(-17.4312311912743,-17.2833070723325,
8.77545214324752));
#163990=CARTESIAN_POINT('Ctrl Pts',(-17.4218822397499,-17.2906581180568,
8.77617832313805));
#163991=CARTESIAN_POINT('Ctrl Pts',(-17.4183005616039,-17.2934931853711,
8.77645643948385));
#163992=CARTESIAN_POINT('Ctrl Pts',(-17.4119355667385,-17.2985649745377,
8.77695047475222));
#163993=CARTESIAN_POINT('Ctrl Pts',(-17.4091487116816,-17.3007971615793,
8.77716671091171));
#163994=CARTESIAN_POINT('Ctrl Pts',(-17.4031593394883,-17.3056193939515,
8.77763127042905));
#163995=CARTESIAN_POINT('Ctrl Pts',(-17.3999587389038,-17.3082117295707,
8.7778794250553));
#163996=CARTESIAN_POINT('Ctrl Pts',(-17.3911214010762,-17.3154123680795,
8.77856441327161));
#163997=CARTESIAN_POINT('Ctrl Pts',(-17.3855007783683,-17.3200404842148,
8.77899984091943));
#163998=CARTESIAN_POINT('Ctrl Pts',(-17.3544490049284,-17.3458790008428,
8.78140483755214));
#163999=CARTESIAN_POINT('Ctrl Pts',(-17.3294928417276,-17.3676561201549,
8.78333558814122));
#164000=CARTESIAN_POINT('Ctrl Pts',(-17.1853821468889,-17.4994919240165,
8.79454282715386));
#164001=CARTESIAN_POINT('Ctrl Pts',(-17.0786739900886,-17.6223743399111,
8.80311685693869));
#164002=CARTESIAN_POINT('Ctrl Pts',(-16.9211382245734,-17.8525301244748,
8.81838643560507));
#164003=CARTESIAN_POINT('Ctrl Pts',(-16.8633175490734,-17.954080290613,
8.82490033117783));
#164004=CARTESIAN_POINT('Ctrl Pts',(-16.8081379465477,-18.0728251063192,
8.83257121970849));
#164005=CARTESIAN_POINT('Ctrl Pts',(-16.8022482983483,-18.085842686997,
8.83341260847234));
#164006=CARTESIAN_POINT('Ctrl Pts',(-16.7930842465057,-18.1066559813539,
8.83475903324848));
#164007=CARTESIAN_POINT('Ctrl Pts',(-16.789723934019,-18.1144135578259,
8.835261129134));
#164008=CARTESIAN_POINT('Ctrl Pts',(-16.7838793432726,-18.1281310094465,
8.83614950110599));
#164009=CARTESIAN_POINT('Ctrl Pts',(-16.7813756822984,-18.1340825457999,
8.8365351113601));
#164010=CARTESIAN_POINT('Ctrl Pts',(-16.7762534857181,-18.1464162526112,
8.83733463740967));
#164011=CARTESIAN_POINT('Ctrl Pts',(-16.7736388436888,-18.1527999478767,
8.83774867966963));
#164012=CARTESIAN_POINT('Ctrl Pts',(-16.7670071750608,-18.1692196452377,
8.83881427643071));
#164013=CARTESIAN_POINT('Ctrl Pts',(-16.7630357701188,-18.1792737516399,
8.83946736091313));
#164014=CARTESIAN_POINT('Ctrl Pts',(-16.7467787879333,-18.221371124696,
8.84220466712063));
#164015=CARTESIAN_POINT('Ctrl Pts',(-16.7351968440456,-18.2536788515808,
8.84431224676059));
#164016=CARTESIAN_POINT('Ctrl Pts',(-16.7070678086544,-18.3385878264479,
8.84987212998108));
#164017=CARTESIAN_POINT('Ctrl Pts',(-16.691782216499,-18.3915766728047,
8.85336291221959));
#164018=CARTESIAN_POINT('Ctrl Pts',(-16.6523833652625,-18.5513336122024,
8.86393954887878));
#164019=CARTESIAN_POINT('Ctrl Pts',(-16.6344613551274,-18.6594331156954,
8.87117377045224));
#164020=CARTESIAN_POINT('Ctrl Pts',(-16.6206253038515,-18.8183891045912,
8.88171361671619));
#164021=CARTESIAN_POINT('Ctrl Pts',(-16.6180530156316,-18.8684948705913,
8.88501984760389));
#164022=CARTESIAN_POINT('Ctrl Pts',(-16.617005625155,-18.9349649137186,
8.88935317982335));
#164023=CARTESIAN_POINT('Ctrl Pts',(-16.6169372026051,-18.9512866916918,
8.89041298416674));
#164024=CARTESIAN_POINT('Ctrl Pts',(-16.6174479434466,-19.0205597976937,
8.89488902191761));
#164025=CARTESIAN_POINT('Ctrl Pts',(-16.6198250184815,-19.0734834067384,
8.89825443247823));
#164026=CARTESIAN_POINT('Ctrl Pts',(-16.6249008382123,-19.1349354757757,
8.90205801412985));
#164027=CARTESIAN_POINT('Ctrl Pts',(-16.6256703084449,-19.1436000527463,
8.90259188014106));
#164028=CARTESIAN_POINT('Ctrl Pts',(-16.6269168264498,-19.1567182375816,
8.90339622155706));
#164029=CARTESIAN_POINT('Ctrl Pts',(-16.6273546269492,-19.1611753573282,
8.90366882127507));
#164030=CARTESIAN_POINT('Ctrl Pts',(-16.6281661843242,-19.1691765181999,
8.90415689849131));
#164031=CARTESIAN_POINT('Ctrl Pts',(-16.6285347469306,-19.1727210184805,
8.90437266252171));
#164032=CARTESIAN_POINT('Ctrl Pts',(-16.6293554309751,-19.1804244700756,
8.90484060423676));
#164033=CARTESIAN_POINT('Ctrl Pts',(-16.6298109287508,-19.1845830036479,
8.90509258962364));
#164034=CARTESIAN_POINT('Ctrl Pts',(-16.63112605805,-19.1962695082469,8.90579904903957));
#164035=CARTESIAN_POINT('Ctrl Pts',(-16.632013791217,-19.2037943414982,
8.90625196888426));
#164036=CARTESIAN_POINT('Ctrl Pts',(-16.6375858540321,-19.2489411931032,
8.90895843494798));
#164037=CARTESIAN_POINT('Ctrl Pts',(-16.6432400411717,-19.2864391426249,
8.91116080654894));
#164038=CARTESIAN_POINT('Ctrl Pts',(-16.6652407742255,-19.4097736293278,
8.91831299186595));
#164039=CARTESIAN_POINT('Ctrl Pts',(-16.6858932767267,-19.4947547301422,
8.92309538048254));
#164040=CARTESIAN_POINT('Ctrl Pts',(-16.763495831235,-19.745356798926,8.93736847304226));
#164041=CARTESIAN_POINT('Ctrl Pts',(-16.8357632696252,-19.9054108668867,
8.94677735806602));
#164042=CARTESIAN_POINT('Ctrl Pts',(-16.9388898723586,-20.0744077204743,
8.95828106971673));
#164043=CARTESIAN_POINT('Ctrl Pts',(-16.9512068063274,-20.0938703204419,
8.95963036120592));
#164044=CARTESIAN_POINT('Ctrl Pts',(-16.9690779963049,-20.121115296918,
8.96155590349463));
#164045=CARTESIAN_POINT('Ctrl Pts',(-16.9743714528139,-20.1290673846456,
8.96212242766494));
#164046=CARTESIAN_POINT('Ctrl Pts',(-16.9830590879283,-20.1419287962921,
8.96304618095787));
#164047=CARTESIAN_POINT('Ctrl Pts',(-16.9864205631454,-20.146860129292,
8.96340217173849));
#164048=CARTESIAN_POINT('Ctrl Pts',(-16.9934999693978,-20.1571519409755,
8.96414895452421));
#164049=CARTESIAN_POINT('Ctrl Pts',(-16.9972219110428,-20.1625095727018,
8.96453989679305));
#164050=CARTESIAN_POINT('Ctrl Pts',(-17.0061341818268,-20.1752128234663,
8.96547210932044));
#164051=CARTESIAN_POINT('Ctrl Pts',(-17.0113466462856,-20.1825426917169,
8.96601422503982));
#164052=CARTESIAN_POINT('Ctrl Pts',(-17.0290598810954,-20.2071182701556,
8.96784626185972));
#164053=CARTESIAN_POINT('Ctrl Pts',(-17.0417738558071,-20.2242080435245,
8.96914441020569));
#164054=CARTESIAN_POINT('Ctrl Pts',(-17.0726278652181,-20.2644001943252,
8.97225650732696));
#164055=CARTESIAN_POINT('Ctrl Pts',(-17.0909947202393,-20.2873221174331,
8.97407916674035));
#164056=CARTESIAN_POINT('Ctrl Pts',(-17.2192724498348,-20.4407588338659,
8.98661309298643));
#164057=CARTESIAN_POINT('Ctrl Pts',(-17.344124772451,-20.5579362855098,
8.99793934014697));
#164058=CARTESIAN_POINT('Ctrl Pts',(-17.5621774958484,-20.717926519405,
9.01575850137952));
#164059=CARTESIAN_POINT('Ctrl Pts',(-17.646794521526,-20.7712452944192,
9.0222690312874));
#164060=CARTESIAN_POINT('Ctrl Pts',(-17.7434050317032,-20.8229634804211,
9.02903939677775));
#164061=CARTESIAN_POINT('Ctrl Pts',(-17.7519721099496,-20.827474331368,
9.02963426525452));
#164062=CARTESIAN_POINT('Ctrl Pts',(-17.7646699202641,-20.8340492853774,
9.0305075212119));
#164063=CARTESIAN_POINT('Ctrl Pts',(-17.7687768017727,-20.8361588294532,
9.03078866605437));
#164064=CARTESIAN_POINT('Ctrl Pts',(-17.7760762831955,-20.8398781571396,
9.03128602953067));
#164065=CARTESIAN_POINT('Ctrl Pts',(-17.779266089384,-20.8414933035127,
9.03150258218964));
#164066=CARTESIAN_POINT('Ctrl Pts',(-17.7861106075726,-20.8449372415195,
9.0319655476308));
#164067=CARTESIAN_POINT('Ctrl Pts',(-17.7897665173152,-20.8467635291599,
9.03221180363128));
#164068=CARTESIAN_POINT('Ctrl Pts',(-17.799819868541,-20.8517492968098,
9.03288621613829));
#164069=CARTESIAN_POINT('Ctrl Pts',(-17.8062280981861,-20.8548870723841,
9.03331303726331));
#164070=CARTESIAN_POINT('Ctrl Pts',(-17.8405784776352,-20.8714918850825,
9.03558524960531));
#164071=CARTESIAN_POINT('Ctrl Pts',(-17.868799776498,-20.8843767530646,
9.03739669474941));
#164072=CARTESIAN_POINT('Ctrl Pts',(-18.0476276331995,-20.9613196485517,
9.04859337053058));
#164073=CARTESIAN_POINT('Ctrl Pts',(-18.2049688965256,-21.008358657409,
9.05724256507398));
#164074=CARTESIAN_POINT('Ctrl Pts',(-18.4819453022129,-21.0572262993895,
9.07263611203104));
#164075=CARTESIAN_POINT('Ctrl Pts',(-18.5992018174828,-21.0679710445371,
9.07919659528085));
#164076=CARTESIAN_POINT('Ctrl Pts',(-18.7310339027525,-21.0690462132869,
9.08691992389703));
#164077=CARTESIAN_POINT('Ctrl Pts',(-18.7453331649165,-21.0690179525362,
9.08776197155815));
#164078=CARTESIAN_POINT('Ctrl Pts',(-18.7680875685534,-21.0687424418896,
9.08910925370239));
#164079=CARTESIAN_POINT('Ctrl Pts',(-18.7765435644007,-21.0685893719823,
9.08961154212731));
#164080=CARTESIAN_POINT('Ctrl Pts',(-18.7914537212469,-21.0682300834907,
9.09050013839054));
#164081=CARTESIAN_POINT('Ctrl Pts',(-18.7979083173903,-21.0680449952444,
9.09088577931689));
#164082=CARTESIAN_POINT('Ctrl Pts',(-18.8112551886689,-21.0676011452183,
9.09168525471415));
#164083=CARTESIAN_POINT('Ctrl Pts',(-18.8181472404011,-21.0673382259126,
9.0920992150863));
#164084=CARTESIAN_POINT('Ctrl Pts',(-18.8358317954272,-21.0665770289049,
9.09316436053081));
#164085=CARTESIAN_POINT('Ctrl Pts',(-18.8466218940324,-21.0660298077227,
9.09381707308453));
#164086=CARTESIAN_POINT('Ctrl Pts',(-18.8916136183037,-21.0634026185412,
9.09655077581213));
#164087=CARTESIAN_POINT('Ctrl Pts',(-18.9257648339233,-21.0605751357702,
9.09865504706032));
#164088=CARTESIAN_POINT('Ctrl Pts',(-19.0145326257989,-21.0510514923447,
9.10420412485287));
#164089=CARTESIAN_POINT('Ctrl Pts',(-19.0689807092927,-21.0430530430561,
9.10768722385823));
#164090=CARTESIAN_POINT('Ctrl Pts',(-19.2305112592769,-21.0128533863834,
9.11824910053011));
#164091=CARTESIAN_POINT('Ctrl Pts',(-19.3362455142208,-20.9844706599363,
9.12547629431187));
#164092=CARTESIAN_POINT('Ctrl Pts',(-19.5511457289884,-20.9085356315324,
9.14053240744068));
#164093=CARTESIAN_POINT('Ctrl Pts',(-19.6594797923219,-20.859682499988,
9.14833328767873));
#164094=CARTESIAN_POINT('Ctrl Pts',(-19.7714859151094,-20.7973733340795,
9.15624992791604));
#164095=CARTESIAN_POINT('Ctrl Pts',(-19.7797803067769,-20.7926855581377,
9.15683517993781));
#164096=CARTESIAN_POINT('Ctrl Pts',(-19.7920207576151,-20.7856581237635,
9.15769705759438));
#164097=CARTESIAN_POINT('Ctrl Pts',(-19.7959911808868,-20.7833614528601,
9.15797633999935));
#164098=CARTESIAN_POINT('Ctrl Pts',(-19.8029416813128,-20.7793107668733,
9.15846470105924));
#164099=CARTESIAN_POINT('Ctrl Pts',(-19.8059249533905,-20.7775623384858,
9.15867413608979));
#164100=CARTESIAN_POINT('Ctrl Pts',(-19.8123267211063,-20.7737893036738,
9.15912316835793));
#164101=CARTESIAN_POINT('Ctrl Pts',(-19.8157437961051,-20.7717623868565,
9.15936261225378));
#164102=CARTESIAN_POINT('Ctrl Pts',(-19.8227901980065,-20.7675557901736,
9.15985592728705));
#164103=CARTESIAN_POINT('Ctrl Pts',(-19.8264187367879,-20.7653748169426,
9.16010971397258));
#164104=CARTESIAN_POINT('Ctrl Pts',(-19.8355355022818,-20.7598577892884,
9.16074680186396));
#164105=CARTESIAN_POINT('Ctrl Pts',(-19.8410151779466,-20.7565075913407,
9.16112921779166));
#164106=CARTESIAN_POINT('Ctrl Pts',(-19.856582747576,-20.7468921943585,
9.16221444566273));
#164107=CARTESIAN_POINT('Ctrl Pts',(-19.8666334554969,-20.7405668798271,
9.16291364173717));
#164108=CARTESIAN_POINT('Ctrl Pts',(-19.9002908818686,-20.7189874100909,
9.16525205714589));
#164109=CARTESIAN_POINT('Ctrl Pts',(-19.9236478065596,-20.7033472453639,
9.16686977446889));
#164110=CARTESIAN_POINT('Ctrl Pts',(-20.1082442683675,-20.5743408558051,
9.17967248577959));
#164111=CARTESIAN_POINT('Ctrl Pts',(-20.2532531562015,-20.4394214355165,
9.18992556716932));
#164112=CARTESIAN_POINT('Ctrl Pts',(-20.424216879423,-20.2288501391307,
9.20507586942558));
#164113=CARTESIAN_POINT('Ctrl Pts',(-20.4678646576284,-20.1689186553657,
9.20929909783092));
#164114=CARTESIAN_POINT('Ctrl Pts',(-20.5154192149796,-20.0958557325202,
9.2144143817794));
#164115=CARTESIAN_POINT('Ctrl Pts',(-20.52245796629,-20.0848188061811,9.21518616584822));
#164116=CARTESIAN_POINT('Ctrl Pts',(-20.5337330179475,-20.0667722321823,
9.2164469468045));
#164117=CARTESIAN_POINT('Ctrl Pts',(-20.5380318602532,-20.0598019271727,
9.21693362989756));
#164118=CARTESIAN_POINT('Ctrl Pts',(-20.5456174344879,-20.0473411418383,
9.21780325239325));
#164119=CARTESIAN_POINT('Ctrl Pts',(-20.5489199361723,-20.0418603441908,
9.21818560719888));
#164120=CARTESIAN_POINT('Ctrl Pts',(-20.5558288515399,-20.030275890477,
9.21899350842704));
#164121=CARTESIAN_POINT('Ctrl Pts',(-20.5594295488909,-20.0241689327805,
9.21941925709593));
#164122=CARTESIAN_POINT('Ctrl Pts',(-20.568878182378,-20.0079580215597,
9.22054906880048));
#164123=CARTESIAN_POINT('Ctrl Pts',(-20.5746732706276,-19.997823689589,
9.22125503246142));
#164124=CARTESIAN_POINT('Ctrl Pts',(-20.6012714515754,-19.9504033889682,
9.22455717259818));
#164125=CARTESIAN_POINT('Ctrl Pts',(-20.621026107921,-19.9125436243246,
9.22719045690848));
#164126=CARTESIAN_POINT('Ctrl Pts',(-20.6723571652418,-19.8064639927248,
9.23456546314183));
#164127=CARTESIAN_POINT('Ctrl Pts',(-20.7014639807055,-19.7371246888076,
9.2393846086122));
#164128=CARTESIAN_POINT('Ctrl Pts',(-20.7861203341855,-19.5009724167288,
9.25573273733217));
#164129=CARTESIAN_POINT('Ctrl Pts',(-20.8245915849777,-19.3288216746901,
9.26760507180113));
#164130=CARTESIAN_POINT('Ctrl Pts',(-20.8438467733349,-19.1278429675792,
9.28035989561479));
#164131=CARTESIAN_POINT('Ctrl Pts',(-20.8458598051352,-19.1017413250874,
9.28199389695891));
#164132=CARTESIAN_POINT('Ctrl Pts',(-20.8477953014005,-19.068649097798,
9.28403148483617));
#164133=CARTESIAN_POINT('Ctrl Pts',(-20.8481679332311,-19.0616883834093,
9.28445817244142));
#164134=CARTESIAN_POINT('Ctrl Pts',(-20.8487046762094,-19.0506400795561,
9.28513226954702));
#164135=CARTESIAN_POINT('Ctrl Pts',(-20.8488913281585,-19.0465537075487,
9.28538090892678));
#164136=CARTESIAN_POINT('Ctrl Pts',(-20.8492163337547,-19.0389552462421,
9.28584193904148));
#164137=CARTESIAN_POINT('Ctrl Pts',(-20.8493577838962,-19.0354433924935,
9.28605449553826));
#164138=CARTESIAN_POINT('Ctrl Pts',(-20.84962182659,-19.0284551283484,9.28647643894481));
#164139=CARTESIAN_POINT('Ctrl Pts',(-20.8497445963614,-19.0249787856908,
9.28668583429858));
#164140=CARTESIAN_POINT('Ctrl Pts',(-20.8500062525391,-19.0170131658696,
9.2871645199004));
#164141=CARTESIAN_POINT('Ctrl Pts',(-20.8501394224102,-19.012523700077,
9.28743349581219));
#164142=CARTESIAN_POINT('Ctrl Pts',(-20.8504746950153,-18.9998612810662,
9.28818992515464));
#164143=CARTESIAN_POINT('Ctrl Pts',(-20.8506437464059,-18.9916874338215,
9.28867561948215));
#164144=CARTESIAN_POINT('Ctrl Pts',(-20.8509186141028,-18.9732240514811,
9.28976727070073));
#164145=CARTESIAN_POINT('Ctrl Pts',(-20.8509967709608,-18.9629342724791,
9.29037183225924));
#164146=CARTESIAN_POINT('Ctrl Pts',(-20.8509999019998,-18.9526441527879,
9.29097295163941));
#164147=CARTESIAN_POINT('Ctrl Pts',(-20.8509999014167,-18.952646066426,
9.2909728398501));
#164148=CARTESIAN_POINT('Ctrl Pts',(-20.8510612391861,-18.7516573651538,
9.30271403367758));
#164149=CARTESIAN_POINT('Ctrl Pts',(-20.8225007118581,-18.5516402133368,
9.31315827211277));
#164150=CARTESIAN_POINT('Ctrl Pts',(-20.7530794613129,-18.3138951311856,
9.32683237017865));
#164151=CARTESIAN_POINT('Ctrl Pts',(-20.7385514247039,-18.2696285787851,
9.32943044125517));
#164152=CARTESIAN_POINT('Ctrl Pts',(-20.7225805549386,-18.2258895562519,
9.33206805306779));
#164153=CARTESIAN_POINT('Origin',(-18.734,-18.952,0.));
#164154=CARTESIAN_POINT('',(-20.7225805737622,-18.2258896078036,10.3555828745111));
#164155=CARTESIAN_POINT('',(-20.7225805600179,-18.2258895701625,10.1325349275789));
#164156=CARTESIAN_POINT('',(-20.7225805737622,-18.2258896078036,0.));
#164157=CARTESIAN_POINT('',(-20.8533534905797,-18.9530771009818,10.310943726863));
#164158=CARTESIAN_POINT('Ctrl Pts',(-20.8509997268492,-18.9530754164219,
10.3109437563757));
#164159=CARTESIAN_POINT('Ctrl Pts',(-20.8510361522915,-18.8813704936462,
10.3152783077124));
#164160=CARTESIAN_POINT('Ctrl Pts',(-20.8474252680863,-18.809517619068,
10.319612859049));
#164161=CARTESIAN_POINT('Ctrl Pts',(-20.84014825964,-18.7379240592327,10.3239474103857));
#164162=CARTESIAN_POINT('Ctrl Pts',(-20.8328800282403,-18.6664168508176,
10.328276733673));
#164163=CARTESIAN_POINT('Ctrl Pts',(-20.8219544852784,-18.5951688251049,
10.3326060569603));
#164164=CARTESIAN_POINT('Ctrl Pts',(-20.8074048164118,-18.5245874741187,
10.3369353802477));
#164165=CARTESIAN_POINT('Ctrl Pts',(-20.7928691087987,-18.4540738500436,
10.3412605492975));
#164166=CARTESIAN_POINT('Ctrl Pts',(-20.7747162754983,-18.3842261135468,
10.3455857183473));
#164167=CARTESIAN_POINT('Ctrl Pts',(-20.7530311027464,-18.3154448915115,
10.3499108873972));
#164168=CARTESIAN_POINT('Ctrl Pts',(-20.7435518570418,-18.2853785364498,
10.3518015497685));
#164169=CARTESIAN_POINT('Ctrl Pts',(-20.7333983034435,-18.2555158565498,
10.3536922121398));
#164170=CARTESIAN_POINT('Ctrl Pts',(-20.7225805737622,-18.2258896078036,
10.3555828745111));
#164171=CARTESIAN_POINT('Ctrl Pts',(-20.7242503992901,-18.225264130614,
9.55561792115202));
#164172=CARTESIAN_POINT('Ctrl Pts',(-20.5136266149504,-17.6645819491398,
9.59172753140163));
#164173=CARTESIAN_POINT('Ctrl Pts',(-19.5197098403558,-16.6327270633957,
9.67022907721175));
#164174=CARTESIAN_POINT('Ctrl Pts',(-17.2597753314279,-16.928885683341,
9.7911225585823));
#164175=CARTESIAN_POINT('Ctrl Pts',(-16.234911172256,-19.0965162369475,
9.91829836526374));
#164176=CARTESIAN_POINT('Ctrl Pts',(-17.5028059015931,-21.1315621128439,
10.0454741719452));
#164177=CARTESIAN_POINT('Ctrl Pts',(-19.9002447996946,-21.1669950290873,
10.1726499786266));
#164178=CARTESIAN_POINT('Ctrl Pts',(-20.823916190907,-19.7776853379838,
10.2611398283041));
#164179=CARTESIAN_POINT('Ctrl Pts',(-20.8542039878978,-19.0144660717243,
10.307237742421));
#164180=CARTESIAN_POINT('Ctrl Pts',(-20.8538228835136,-18.9530774369206,
10.3109437209775));
#164181=CARTESIAN_POINT('Ctrl Pts',(-20.7225805549386,-18.2258895562519,
9.33206805306779));
#164182=CARTESIAN_POINT('Ctrl Pts',(-20.7083722868681,-18.1869777270011,
9.33441456870847));
#164183=CARTESIAN_POINT('Ctrl Pts',(-20.693022084485,-18.1484834091484,
9.33679231958261));
#164184=CARTESIAN_POINT('Ctrl Pts',(-20.6684009409741,-18.0916500373935,
9.34040228155194));
#164185=CARTESIAN_POINT('Ctrl Pts',(-20.6599812432231,-18.0729634445399,
9.34160564671993));
#164186=CARTESIAN_POINT('Ctrl Pts',(-20.6475367865955,-18.0463817588176,
9.34334232161629));
#164187=CARTESIAN_POINT('Ctrl Pts',(-20.6437315490788,-18.0383847422257,
9.34386805941979));
#164188=CARTESIAN_POINT('Ctrl Pts',(-20.6370470760901,-18.0245610188386,
9.34478263147945));
#164189=CARTESIAN_POINT('Ctrl Pts',(-20.6341909604698,-18.018723219035,
9.34517065749221));
#164190=CARTESIAN_POINT('Ctrl Pts',(-20.6286470865644,-18.0075226843942,
9.34591864013509));
#164191=CARTESIAN_POINT('Ctrl Pts',(-20.6259633240403,-18.0021580333254,
9.34627845405013));
#164192=CARTESIAN_POINT('Ctrl Pts',(-20.6188715792595,-17.9881314462617,
9.34722336186107));
#164193=CARTESIAN_POINT('Ctrl Pts',(-20.6144267212519,-17.9794884061054,
9.34780974861588));
#164194=CARTESIAN_POINT('Ctrl Pts',(-20.5987863527489,-17.9495837948224,
9.34985325187573));
#164195=CARTESIAN_POINT('Ctrl Pts',(-20.5872888088139,-17.9284830698622,
9.35132101656207));
#164196=CARTESIAN_POINT('Ctrl Pts',(-20.5034337443168,-17.7806362921786,
9.36179370081421));
#164197=CARTESIAN_POINT('Ctrl Pts',(-20.4185109288099,-17.661497100169,
9.37126612649183));
#164198=CARTESIAN_POINT('Ctrl Pts',(-20.2315225656315,-17.4493862964996,
9.38992778565965));
#164199=CARTESIAN_POINT('Ctrl Pts',(-20.1312641286651,-17.355729239754,
9.39904487547204));
#164200=CARTESIAN_POINT('Ctrl Pts',(-20.0125804274804,-17.2646700196703,
9.40841273773673));
#164201=CARTESIAN_POINT('Ctrl Pts',(-20.0024322036148,-17.2570279843549,
9.40920319335917));
#164202=CARTESIAN_POINT('Ctrl Pts',(-19.986797717762,-17.2454736267136,
9.41040415758955));
#164203=CARTESIAN_POINT('Ctrl Pts',(-19.9813607286224,-17.2414955130815,
9.41081872957315));
#164204=CARTESIAN_POINT('Ctrl Pts',(-19.9723708049154,-17.2349834620866,
9.41149904499264));
#164205=CARTESIAN_POINT('Ctrl Pts',(-19.9688289060965,-17.2324344690082,
9.4117657678084));
#164206=CARTESIAN_POINT('Ctrl Pts',(-19.9619672187143,-17.2275284619199,
9.41227991712364));
#164207=CARTESIAN_POINT('Ctrl Pts',(-19.9586484656496,-17.2251700396066,
9.4125274378999));
#164208=CARTESIAN_POINT('Ctrl Pts',(-19.9553132035222,-17.2228143364453,
9.4127750168183));
#164209=CARTESIAN_POINT('Ctrl Pts',(-19.9553035097842,-17.2228074898584,
9.41277573638156));
#164210=CARTESIAN_POINT('Ctrl Pts',(-19.9552840880669,-17.2227937727453,
9.41277717802993));
#164211=CARTESIAN_POINT('Ctrl Pts',(-19.9552743598493,-17.2227869020515,
9.41277790013266));
#164212=CARTESIAN_POINT('Ctrl Pts',(-19.9552548689621,-17.2227731365783,
9.41277934687539));
#164213=CARTESIAN_POINT('Ctrl Pts',(-19.9552451061013,-17.2227662416647,
9.41278007152951));
#164214=CARTESIAN_POINT('Ctrl Pts',(-19.9552249124328,-17.2227519803636,
9.4127815703957));
#164215=CARTESIAN_POINT('Ctrl Pts',(-19.9552144819454,-17.2227446142198,
9.41278234458257));
#164216=CARTESIAN_POINT('Ctrl Pts',(-19.9551934527626,-17.2227297634267,
9.41278390541815));
#164217=CARTESIAN_POINT('Ctrl Pts',(-19.9551828540166,-17.2227222787464,
9.41278469207022));
#164218=CARTESIAN_POINT('Ctrl Pts',(-19.9551614847679,-17.2227071883879,
9.41278627809847));
#164219=CARTESIAN_POINT('Ctrl Pts',(-19.955150714365,-17.2226995827851,
9.41278707746685));
#164220=CARTESIAN_POINT('Ctrl Pts',(-19.9551289980691,-17.2226842479598,
9.4127886892036));
#164221=CARTESIAN_POINT('Ctrl Pts',(-19.9551180522886,-17.2226765188218,
9.41278950156323));
#164222=CARTESIAN_POINT('Ctrl Pts',(-19.9550959819521,-17.222660934621,
9.41279113952513));
#164223=CARTESIAN_POINT('Ctrl Pts',(-19.9550848567631,-17.2226530791165,
9.41279196517394));
#164224=CARTESIAN_POINT('Ctrl Pts',(-19.9550624232963,-17.2226372391527,
9.41279363003305));
#164225=CARTESIAN_POINT('Ctrl Pts',(-19.9550511154003,-17.2226292549683,
9.41279446921457));
#164226=CARTESIAN_POINT('Ctrl Pts',(-19.9550283126131,-17.2226131549028,
9.41279616142769));
#164227=CARTESIAN_POINT('Ctrl Pts',(-19.9550168174606,-17.2226050388427,
9.41279701447822));
#164228=CARTESIAN_POINT('Ctrl Pts',(-19.9549936360609,-17.2225886721478,
9.41279873473222));
#164229=CARTESIAN_POINT('Ctrl Pts',(-19.954981949856,-17.2225804215488,
9.41279960193207));
#164230=CARTESIAN_POINT('Ctrl Pts',(-19.9549583818049,-17.2225637825835,
9.41280135082069));
#164231=CARTESIAN_POINT('Ctrl Pts',(-19.9549465003227,-17.2225553944803,
9.41280223248196));
#164232=CARTESIAN_POINT('Ctrl Pts',(-19.9549225375747,-17.2225384776004,
9.41280401059931));
#164233=CARTESIAN_POINT('Ctrl Pts',(-19.9549104561934,-17.2225299487484,
9.41280490706346));
#164234=CARTESIAN_POINT('Ctrl Pts',(-19.9548860894242,-17.2225127474085,
9.41280671509841));
#164235=CARTESIAN_POINT('Ctrl Pts',(-19.9548738037708,-17.2225040747396,
9.41280762668838));
#164236=CARTESIAN_POINT('Ctrl Pts',(-19.954849023501,-17.2224865822866,
9.41280946534114));
#164237=CARTESIAN_POINT('Ctrl Pts',(-19.9548365292056,-17.2224777627359,
9.41281039237957));
#164238=CARTESIAN_POINT('Ctrl Pts',(-19.9548113270583,-17.2224599732969,
9.41281226226843));
#164239=CARTESIAN_POINT('Ctrl Pts',(-19.9547986189937,-17.2224510032656,
9.41281320513407));
#164240=CARTESIAN_POINT('Ctrl Pts',(-19.9547729843128,-17.2224329093608,
9.41281510704624));
#164241=CARTESIAN_POINT('Ctrl Pts',(-19.9547600578991,-17.2224237856375,
9.41281606607716));
#164242=CARTESIAN_POINT('Ctrl Pts',(-19.9547339816052,-17.2224053809018,
9.41281800068272));
#164243=CARTESIAN_POINT('Ctrl Pts',(-19.9547208315242,-17.2223960997552,
9.41281897627167));
#164244=CARTESIAN_POINT('Ctrl Pts',(-19.951870266171,-17.2203842585756,
9.41303045238298));
#164245=CARTESIAN_POINT('Ctrl Pts',(-19.9490279680683,-17.2183887119179,
9.41324046161644));
#164246=CARTESIAN_POINT('Ctrl Pts',(-19.9424087532231,-17.2137657082699,
9.41372757341653));
#164247=CARTESIAN_POINT('Ctrl Pts',(-19.938628177307,-17.2111435661814,
9.41400431194887));
#164248=CARTESIAN_POINT('Ctrl Pts',(-19.9269336109555,-17.2030887548029,
9.4148559093759));
#164249=CARTESIAN_POINT('Ctrl Pts',(-19.9189910687996,-17.1976974837754,
9.41542802846367));
#164250=CARTESIAN_POINT('Ctrl Pts',(-19.8165021452211,-17.1291432850232,
9.4227343206875));
#164251=CARTESIAN_POINT('Ctrl Pts',(-19.7170385839675,-17.0736336969328,
9.42900129176324));
#164252=CARTESIAN_POINT('Ctrl Pts',(-19.5099110081263,-16.9790220714055,
9.44141172097439));
#164253=CARTESIAN_POINT('Ctrl Pts',(-19.4025859821442,-16.9401173508394,
9.44753902465469));
#164254=CARTESIAN_POINT('Ctrl Pts',(-19.2395033464369,-16.8955001555529,
9.45694031242375));
#164255=CARTESIAN_POINT('Ctrl Pts',(-19.1858102281003,-16.883040813327,
9.46004739935269));
#164256=CARTESIAN_POINT('Ctrl Pts',(-19.0980015787013,-16.8662462709348,
9.46519076290448));
#164257=CARTESIAN_POINT('Ctrl Pts',(-19.0641581411941,-16.8606221831351,
9.46718766487111));
#164258=CARTESIAN_POINT('Ctrl Pts',(-19.0194921615275,-16.854310783408,
9.46984807196404));
#164259=CARTESIAN_POINT('Ctrl Pts',(-19.0087787034061,-16.8528805462059,
9.47048805418126));
#164260=CARTESIAN_POINT('Ctrl Pts',(-18.9912106967492,-16.8506720291598,
9.47154073141431));
#164261=CARTESIAN_POINT('Ctrl Pts',(-18.9843623816266,-16.849845091414,
9.47195188531553));
#164262=CARTESIAN_POINT('Ctrl Pts',(-18.971096197473,-16.8483089380086,
9.47274995070855));
#164263=CARTESIAN_POINT('Ctrl Pts',(-18.9646788776244,-16.8475955842225,
9.47313672686161));
#164264=CARTESIAN_POINT('Ctrl Pts',(-18.9498510739405,-16.846015954469,
9.47403212231116));
#164265=CARTESIAN_POINT('Ctrl Pts',(-18.9414385054595,-16.8451706881274,
9.47454139781465));
#164266=CARTESIAN_POINT('Ctrl Pts',(-18.9187937471432,-16.8430323624584,
9.47591577269443));
#164267=CARTESIAN_POINT('Ctrl Pts',(-18.9045533446997,-16.8418330004304,
9.47678380057848));
#164268=CARTESIAN_POINT('Ctrl Pts',(-18.7737124648666,-16.8321463301725,
9.48479481068193));
#164269=CARTESIAN_POINT('Ctrl Pts',(-18.6566273911351,-16.8331884646397,
9.49223989754308));
#164270=CARTESIAN_POINT('Ctrl Pts',(-18.3780211176261,-16.8587952442312,
9.51051541238347));
#164271=CARTESIAN_POINT('Ctrl Pts',(-18.2180669964656,-16.892378590209,
9.52148636061821));
#164272=CARTESIAN_POINT('Ctrl Pts',(-18.0329154722312,-16.9541981160818,
9.53388725072007));
#164273=CARTESIAN_POINT('Ctrl Pts',(-18.0025201118048,-16.9651257414575,
9.53591097297362));
#164274=CARTESIAN_POINT('Ctrl Pts',(-17.9656436836677,-16.9793444875725,
9.53834125681395));
#164275=CARTESIAN_POINT('Ctrl Pts',(-17.9589157453101,-16.9819782739377,
9.53878362011833));
#164276=CARTESIAN_POINT('Ctrl Pts',(-17.9483851474728,-16.9861629858148,
9.53947423925572));
#164277=CARTESIAN_POINT('Ctrl Pts',(-17.9445733661544,-16.9876905912537,
9.53972385876421));
#164278=CARTESIAN_POINT('Ctrl Pts',(-17.9374539198243,-16.9905678436766,
9.54018936826387));
#164279=CARTESIAN_POINT('Ctrl Pts',(-17.9341452627771,-16.9919147566312,
9.54040541251055));
#164280=CARTESIAN_POINT('Ctrl Pts',(-17.9265966060468,-16.9950100171784,
9.54089765860845));
#164281=CARTESIAN_POINT('Ctrl Pts',(-17.9223588764044,-16.9967637685364,
9.54117352963987));
#164282=CARTESIAN_POINT('Ctrl Pts',(-17.9093381867666,-17.0022019059693,
9.5420198104028));
#164283=CARTESIAN_POINT('Ctrl Pts',(-17.900574225172,-17.0059318616222,
9.54258752958714));
#164284=CARTESIAN_POINT('Ctrl Pts',(-17.7829225667688,-17.0569451505327,
9.55018714534813));
#164285=CARTESIAN_POINT('Ctrl Pts',(-17.6781579354447,-17.113253995431,
9.55670911330969));
#164286=CARTESIAN_POINT('Ctrl Pts',(-17.4871063525511,-17.2376833368706,
9.56912161114755));
#164287=CARTESIAN_POINT('Ctrl Pts',(-17.4003110645262,-17.304305150168,
9.57500500383094));
#164288=CARTESIAN_POINT('Ctrl Pts',(-17.2781424346921,-17.4140818850209,
9.58413842023623));
#164289=CARTESIAN_POINT('Ctrl Pts',(-17.2386866174734,-17.4524165161774,
9.58723967848758));
#164290=CARTESIAN_POINT('Ctrl Pts',(-17.1771493661918,-17.5170510364593,
9.59237425294312));
#164291=CARTESIAN_POINT('Ctrl Pts',(-17.1541356542176,-17.5424288321776,
9.59436837072523));
#164292=CARTESIAN_POINT('Ctrl Pts',(-17.1246880112075,-17.5765289442296,
9.59702559403794));
#164293=CARTESIAN_POINT('Ctrl Pts',(-17.1176901501293,-17.5847589220637,
9.59766524846115));
#164294=CARTESIAN_POINT('Ctrl Pts',(-17.1063284108698,-17.5983302601747,
9.59871752386693));
#164295=CARTESIAN_POINT('Ctrl Pts',(-17.1019270493646,-17.6036400893478,
9.59912860604435));
#164296=CARTESIAN_POINT('Ctrl Pts',(-17.0934551872237,-17.6139628499704,
9.59992663043414));
#164297=CARTESIAN_POINT('Ctrl Pts',(-17.0893815171522,-17.6189730902832,
9.60031343782762));
#164298=CARTESIAN_POINT('Ctrl Pts',(-17.0800251602083,-17.6305887215608,
9.60120904874766));
#164299=CARTESIAN_POINT('Ctrl Pts',(-17.0747590356788,-17.6372072571977,
9.60171850947502));
#164300=CARTESIAN_POINT('Ctrl Pts',(-17.060695731012,-17.6551012576845,
9.60309370839287));
#164301=CARTESIAN_POINT('Ctrl Pts',(-17.0519730297208,-17.6664344513281,
9.60396238055695));
#164302=CARTESIAN_POINT('Ctrl Pts',(-16.9725011987249,-17.7718838106393,
9.61202503360709));
#164303=CARTESIAN_POINT('Ctrl Pts',(-16.9096159195966,-17.8716449675874,
9.6195256589858));
#164304=CARTESIAN_POINT('Ctrl Pts',(-16.7799641013343,-18.1212299050466,
9.63790280092094));
#164305=CARTESIAN_POINT('Ctrl Pts',(-16.7216460278061,-18.2746026979024,
9.64891778688076));
#164306=CARTESIAN_POINT('Ctrl Pts',(-16.673972600071,-18.4631896181054,
9.66125994868755));
#164307=CARTESIAN_POINT('Ctrl Pts',(-16.667040583935,-18.4933852546187,
9.6631992582693));
#164308=CARTESIAN_POINT('Ctrl Pts',(-16.6593305632245,-18.530708422663,
9.66554227879331));
#164309=CARTESIAN_POINT('Ctrl Pts',(-16.657923022374,-18.5377002880341,
9.66597888455284));
#164310=CARTESIAN_POINT('Ctrl Pts',(-16.6557647001057,-18.5487088727017,
9.66666252450698));
#164311=CARTESIAN_POINT('Ctrl Pts',(-16.6549901826835,-18.5527208054027,
9.66691087816413));
#164312=CARTESIAN_POINT('Ctrl Pts',(-16.6535596877785,-18.5602476652057,
9.66737530614509));
#164313=CARTESIAN_POINT('Ctrl Pts',(-16.652901007267,-18.5637619709658,
9.66759152706062));
#164314=CARTESIAN_POINT('Ctrl Pts',(-16.6514119893932,-18.5718191166709,
9.66808584549477));
#164315=CARTESIAN_POINT('Ctrl Pts',(-16.6505876122524,-18.5763630083733,
9.66836360151432));
#164316=CARTESIAN_POINT('Ctrl Pts',(-16.6480800127015,-18.5904468920974,
9.66922145916228));
#164317=CARTESIAN_POINT('Ctrl Pts',(-16.6464473706886,-18.5999959216786,
9.66979876239972));
#164318=CARTESIAN_POINT('Ctrl Pts',(-16.6280527697977,-18.7122143456564,
9.67653585815283));
#164319=CARTESIAN_POINT('Ctrl Pts',(-16.6188126508804,-18.8159881285185,
9.68230549738156));
#164320=CARTESIAN_POINT('Ctrl Pts',(-16.6155502458532,-19.0320130549256,
9.69411211035283));
#164321=CARTESIAN_POINT('Ctrl Pts',(-16.6227475512994,-19.1439489123726,
9.70012213012779));
#164322=CARTESIAN_POINT('Ctrl Pts',(-16.6477177264939,-19.3167366506037,
9.70977486139479));
#164323=CARTESIAN_POINT('Ctrl Pts',(-16.6594120857905,-19.3782518614796,
9.71328513596411));
#164324=CARTESIAN_POINT('Ctrl Pts',(-16.6824641905068,-19.4757394758118,
9.71903241786779));
#164325=CARTESIAN_POINT('Ctrl Pts',(-16.6920873804407,-19.512084648973,
9.72121677335223));
#164326=CARTESIAN_POINT('Ctrl Pts',(-16.7058182040965,-19.5588709717385,
9.72409087483164));
#164327=CARTESIAN_POINT('Ctrl Pts',(-16.709048499029,-19.5695639117193,
9.72475200050965));
#164328=CARTESIAN_POINT('Ctrl Pts',(-16.7144339173746,-19.5868941073688,
9.725830621063));
#164329=CARTESIAN_POINT('Ctrl Pts',(-16.716537527734,-19.5935472397802,
9.72624642314144));
#164330=CARTESIAN_POINT('Ctrl Pts',(-16.7206422381173,-19.6063094427599,
9.72704737572249));
#164331=CARTESIAN_POINT('Ctrl Pts',(-16.7226383501965,-19.6124200455045,
9.72743235816625));
#164332=CARTESIAN_POINT('Ctrl Pts',(-16.7272668326533,-19.6263733625366,
9.72831488785078));
#164333=CARTESIAN_POINT('Ctrl Pts',(-16.7299173925248,-19.634209891756,
9.72881303188787));
#164334=CARTESIAN_POINT('Ctrl Pts',(-16.7370684358692,-19.6549510003284,
9.7301381978387));
#164335=CARTESIAN_POINT('Ctrl Pts',(-16.7416480114709,-19.6678277172201,
9.73096783087606));
#164336=CARTESIAN_POINT('Ctrl Pts',(-16.7766618073855,-19.7633389375787,
9.73717419648778));
#164337=CARTESIAN_POINT('Ctrl Pts',(-16.812097029624,-19.8440365347385,
9.74271836954522));
#164338=CARTESIAN_POINT('Ctrl Pts',(-16.9364588089905,-20.0851954432848,
9.76021705858079));
#164339=CARTESIAN_POINT('Ctrl Pts',(-17.0412592928378,-20.2364869505178,
9.77261274122918));
#164340=CARTESIAN_POINT('Ctrl Pts',(-17.191737782315,-20.4027921293093,
9.78696996107506));
#164341=CARTESIAN_POINT('Ctrl Pts',(-17.2201307774278,-20.4323955688644,
9.7895547854379));
#164342=CARTESIAN_POINT('Ctrl Pts',(-17.2548888246814,-20.4665887591102,
9.79255618039699));
#164343=CARTESIAN_POINT('Ctrl Pts',(-17.2604395906209,-20.471989704681,
9.79303074643446));
#164344=CARTESIAN_POINT('Ctrl Pts',(-17.2690603341368,-20.4802861579751,
9.79376030383381));
#164345=CARTESIAN_POINT('Ctrl Pts',(-17.2721094725527,-20.4832030863847,
9.79401691737003));
#164346=CARTESIAN_POINT('Ctrl Pts',(-17.2777479272629,-20.4885648642243,
9.79448878269691));
#164347=CARTESIAN_POINT('Ctrl Pts',(-17.2803346721282,-20.491012279418,
9.79470423015101));
#164348=CARTESIAN_POINT('Ctrl Pts',(-17.2861556263775,-20.4964919305224,
9.79518675590144));
#164349=CARTESIAN_POINT('Ctrl Pts',(-17.2893931816891,-20.4995205313635,
9.79545355501102));
#164350=CARTESIAN_POINT('Ctrl Pts',(-17.2976821399734,-20.5072258331796,
9.79613268854724));
#164351=CARTESIAN_POINT('Ctrl Pts',(-17.3027469278445,-20.5118881477864,
9.79654394849598));
#164352=CARTESIAN_POINT('Ctrl Pts',(-17.3321057823056,-20.5386506264751,
9.79890719523391));
#164353=CARTESIAN_POINT('Ctrl Pts',(-17.3568902072886,-20.5602090953013,
9.80082100703645));
#164354=CARTESIAN_POINT('Ctrl Pts',(-17.3964519373815,-20.5930358616361,
9.80376971246546));
#164355=CARTESIAN_POINT('Ctrl Pts',(-17.4108917784791,-20.6047002723072,
9.80482473092535));
#164356=CARTESIAN_POINT('Ctrl Pts',(-17.4266454598076,-20.6170871721849,
9.80595529142207));
#164357=CARTESIAN_POINT('Ctrl Pts',(-17.4278083413471,-20.6179995605097,
9.80603862655496));
#164358=CARTESIAN_POINT('Ctrl Pts',(-17.4470160553447,-20.6330373190721,
9.80741315832312));
#164359=CARTESIAN_POINT('Ctrl Pts',(-17.4652885787107,-20.6468703561365,
9.80869249735971));
#164360=CARTESIAN_POINT('Ctrl Pts',(-17.5206414204066,-20.6873777984211,
9.81249581259531));
#164361=CARTESIAN_POINT('Ctrl Pts',(-17.55836466111,-20.7131521604237,9.81499332195534));
#164362=CARTESIAN_POINT('Ctrl Pts',(-17.6891295565142,-20.796421901009,
9.82343362746429));
#164363=CARTESIAN_POINT('Ctrl Pts',(-17.7857773243761,-20.8479217458387,
9.82932172188505));
#164364=CARTESIAN_POINT('Ctrl Pts',(-17.93646187295,-20.9137999556882,9.83846606798689));
#164365=CARTESIAN_POINT('Ctrl Pts',(-17.9877968341766,-20.9338946289288,
9.84157359006515));
#164366=CARTESIAN_POINT('Ctrl Pts',(-18.0722657369381,-20.9632120182653,
9.84671760971191));
#164367=CARTESIAN_POINT('Ctrl Pts',(-18.1049439369301,-20.9736711627375,
9.84871471944941));
#164368=CARTESIAN_POINT('Ctrl Pts',(-18.148232057548,-20.9863750269638,
9.85137536412097));
#164369=CARTESIAN_POINT('Ctrl Pts',(-18.1586265816501,-20.9893392588462,
9.85201537078315));
#164370=CARTESIAN_POINT('Ctrl Pts',(-18.1756912088485,-20.9940646117463,
9.85306807798253));
#164371=CARTESIAN_POINT('Ctrl Pts',(-18.1823481078044,-20.9958729835606,
9.85347923723297));
#164372=CARTESIAN_POINT('Ctrl Pts',(-18.1952528776695,-20.9993109751234,
9.85427730568879));
#164373=CARTESIAN_POINT('Ctrl Pts',(-18.2014996065773,-21.0009446113187,
9.85466407951666));
#164374=CARTESIAN_POINT('Ctrl Pts',(-18.2159429958744,-21.0046513154476,
9.8555594589186));
#164375=CARTESIAN_POINT('Ctrl Pts',(-18.2241447559066,-21.0067038981721,
9.85606872062577));
#164376=CARTESIAN_POINT('Ctrl Pts',(-18.246241475799,-21.0120934020021,
9.85744303413447));
#164377=CARTESIAN_POINT('Ctrl Pts',(-18.260158105327,-21.0153388102875,
9.85831101403678));
#164378=CARTESIAN_POINT('Ctrl Pts',(-18.3881654428184,-21.0438272672115,
9.86631836257877));
#164379=CARTESIAN_POINT('Ctrl Pts',(-18.5041115851046,-21.0597206566284,
9.87375951567205));
#164380=CARTESIAN_POINT('Ctrl Pts',(-18.7832505341023,-21.0746733398998,
9.89201886651903));
#164381=CARTESIAN_POINT('Ctrl Pts',(-18.9461977362871,-21.0646144742368,
9.90297711948184));
#164382=CARTESIAN_POINT('Ctrl Pts',(-19.13838591786,-21.0302728115179,9.91538262553902));
#164383=CARTESIAN_POINT('Ctrl Pts',(-19.1702543746321,-21.023817617185,
9.91742016143153));
#164384=CARTESIAN_POINT('Ctrl Pts',(-19.2090240487272,-21.0150301904209,
9.91986468832512));
#164385=CARTESIAN_POINT('Ctrl Pts',(-19.2160765319396,-21.0133936145963,
9.9203079676584));
#164386=CARTESIAN_POINT('Ctrl Pts',(-19.227119094561,-21.0107713443097,
9.92099969674291));
#164387=CARTESIAN_POINT('Ctrl Pts',(-19.2311148580123,-21.0098101730185,
9.92124951725988));
#164388=CARTESIAN_POINT('Ctrl Pts',(-19.2385782094178,-21.0079918747214,
9.92171520067195));
#164389=CARTESIAN_POINT('Ctrl Pts',(-19.2420463889075,-21.0071376171167,
9.92193121903391));
#164390=CARTESIAN_POINT('Ctrl Pts',(-19.2499580327486,-21.0051676251089,
9.92242314597205));
#164391=CARTESIAN_POINT('Ctrl Pts',(-19.2544000391822,-21.0040462442347,
9.92269872538134));
#164392=CARTESIAN_POINT('Ctrl Pts',(-19.2680411717368,-21.0005554089983,
9.92354322312421));
#164393=CARTESIAN_POINT('Ctrl Pts',(-19.2772281640435,-20.9981384132661,
9.92410946732902));
#164394=CARTESIAN_POINT('Ctrl Pts',(-19.359553736834,-20.9758859085876,
9.92916366286775));
#164395=CARTESIAN_POINT('Ctrl Pts',(-19.4316028334109,-20.9521961229144,
9.93344583061162));
#164396=CARTESIAN_POINT('Ctrl Pts',(-19.542054282036,-20.909182534394,9.9400066127025));
#164397=CARTESIAN_POINT('Ctrl Pts',(-19.5813975995392,-20.8924722853381,
9.94234267543521));
#164398=CARTESIAN_POINT('Ctrl Pts',(-19.7194907212765,-20.8288186372802,
9.95062118388836));
#164399=CARTESIAN_POINT('Ctrl Pts',(-19.8150774026979,-20.7754338269768,
9.9565078831916));
#164400=CARTESIAN_POINT('Ctrl Pts',(-19.9519739514086,-20.6844150185626,
9.96564898592232));
#164401=CARTESIAN_POINT('Ctrl Pts',(-19.9966274788677,-20.6521451550111,
9.96875464900143));
#164402=CARTESIAN_POINT('Ctrl Pts',(-20.0669593893852,-20.5970179989424,
9.97389586568113));
#164403=CARTESIAN_POINT('Ctrl Pts',(-20.0934296045401,-20.5752116019047,
9.97589208771736));
#164404=CARTESIAN_POINT('Ctrl Pts',(-20.1275293215633,-20.5457006695304,
9.97855171732225));
#164405=CARTESIAN_POINT('Ctrl Pts',(-20.1356467600953,-20.5385661497325,
9.97919161952712));
#164406=CARTESIAN_POINT('Ctrl Pts',(-20.1488551361408,-20.5267766581802,
9.98024419867555));
#164407=CARTESIAN_POINT('Ctrl Pts',(-20.1539786414091,-20.5221583473088,
9.98065533506835));
#164408=CARTESIAN_POINT('Ctrl Pts',(-20.1638543634474,-20.5131685341615,
9.98145339044124));
#164409=CARTESIAN_POINT('Ctrl Pts',(-20.1686093357178,-20.5088001622443,
9.98184017420952));
#164410=CARTESIAN_POINT('Ctrl Pts',(-20.1795448204575,-20.4986611363548,
9.98273562220575));
#164411=CARTESIAN_POINT('Ctrl Pts',(-20.185710861493,-20.4928750987813,
9.983244942883));
#164412=CARTESIAN_POINT('Ctrl Pts',(-20.2022061746189,-20.4772094698592,
9.98461951871922));
#164413=CARTESIAN_POINT('Ctrl Pts',(-20.2124701892517,-20.4672620835693,
9.98548770371838));
#164414=CARTESIAN_POINT('Ctrl Pts',(-20.3058954028151,-20.374865905961,
9.993510868046));
#164415=CARTESIAN_POINT('Ctrl Pts',(-20.3821685934173,-20.2857672119175,
10.0009690164536));
#164416=CARTESIAN_POINT('Ctrl Pts',(-20.5463777589345,-20.0582193214209,
10.0193001074059));
#164417=CARTESIAN_POINT('Ctrl Pts',(-20.6263877603084,-19.9149657795901,
10.0303152447319));
#164418=CARTESIAN_POINT('Ctrl Pts',(-20.7012121944736,-19.7347904123535,
10.0427007793794));
#164419=CARTESIAN_POINT('Ctrl Pts',(-20.7126617703775,-19.7053807093284,
10.0446771132839));
#164420=CARTESIAN_POINT('Ctrl Pts',(-20.7259025060463,-19.6689831676142,
10.0470584570095));
#164421=CARTESIAN_POINT('Ctrl Pts',(-20.7283205551941,-19.6622295282239,
10.0474976225049));
#164422=CARTESIAN_POINT('Ctrl Pts',(-20.7320650322533,-19.6516012410794,
10.0481843659083));
#164423=CARTESIAN_POINT('Ctrl Pts',(-20.7334145990411,-19.6477348858806,
10.0484332828604));
#164424=CARTESIAN_POINT('Ctrl Pts',(-20.7359210084457,-19.640486782705,
10.0488981891431));
#164425=CARTESIAN_POINT('Ctrl Pts',(-20.7370804929386,-19.637106059703,
10.0491143284831));
#164426=CARTESIAN_POINT('Ctrl Pts',(-20.7397139282448,-19.6293638844503,
10.0496077112137));
#164427=CARTESIAN_POINT('Ctrl Pts',(-20.7411822149267,-19.6250005578846,
10.049884617916));
#164428=CARTESIAN_POINT('Ctrl Pts',(-20.7456726550282,-19.6115108429495,
10.0507372482103));
#164429=CARTESIAN_POINT('Ctrl Pts',(-20.748646933026,-19.6023684848468,
10.0513102223729));
#164430=CARTESIAN_POINT('Ctrl Pts',(-20.7774525867324,-19.5117313046548,
10.0569454585948));
#164431=CARTESIAN_POINT('Ctrl Pts',(-20.7983905120187,-19.4287525255262,
10.0617451793867));
#164432=CARTESIAN_POINT('Ctrl Pts',(-20.8385991730742,-19.215768687721,
10.0736795592272));
#164433=CARTESIAN_POINT('Ctrl Pts',(-20.8509009167197,-19.084827760392,
10.080678612438));
#164434=CARTESIAN_POINT('Ctrl Pts',(-20.8510686213948,-18.8613529327797,
10.093037908689));
#164435=CARTESIAN_POINT('Ctrl Pts',(-20.8451100147201,-18.7692216670311,
10.098249111993));
#164436=CARTESIAN_POINT('Ctrl Pts',(-20.8313804902798,-18.6641219290087,
10.1044627695678));
#164437=CARTESIAN_POINT('Ctrl Pts',(-20.8294631848653,-18.650482616976,
10.1052742662429));
#164438=CARTESIAN_POINT('Ctrl Pts',(-20.8261768230356,-18.6286517394469,
10.1065817451484));
#164439=CARTESIAN_POINT('Ctrl Pts',(-20.8248923983709,-18.6204476935897,
10.1070750504501));
#164440=CARTESIAN_POINT('Ctrl Pts',(-20.8225273356136,-18.6059018162024,
10.107953241767));
#164441=CARTESIAN_POINT('Ctrl Pts',(-20.8214659899547,-18.5995569211838,
10.108337511021));
#164442=CARTESIAN_POINT('Ctrl Pts',(-20.8191956396225,-18.5863545005389,
10.1091396443378));
#164443=CARTESIAN_POINT('Ctrl Pts',(-20.8179816892408,-18.5794979142568,
10.1095576615708));
#164444=CARTESIAN_POINT('Ctrl Pts',(-20.8147441180365,-18.561722890938,
10.1106451137707));
#164445=CARTESIAN_POINT('Ctrl Pts',(-20.812668397939,-18.5508142691322,
10.111316201506));
#164446=CARTESIAN_POINT('Ctrl Pts',(-20.8033102379476,-18.5036573840885,
10.1142336751931));
#164447=CARTESIAN_POINT('Ctrl Pts',(-20.7951650834556,-18.4675888208255,
10.1165074352853));
#164448=CARTESIAN_POINT('Ctrl Pts',(-20.7710540903731,-18.3724844626009,
10.1226194797501));
#164449=CARTESIAN_POINT('Ctrl Pts',(-20.7534686062404,-18.3138988507035,
10.1265064549792));
#164450=CARTESIAN_POINT('Ctrl Pts',(-20.7298520795935,-18.2460408765856,
10.131146311054));
#164451=CARTESIAN_POINT('Ctrl Pts',(-20.7262541483525,-18.2359503350921,
10.1318398744086));
#164452=CARTESIAN_POINT('Ctrl Pts',(-20.7225805600179,-18.2258895701625,
10.1325349275789));
#164453=CARTESIAN_POINT('Origin',(-18.734,-18.952,0.));
#164454=CARTESIAN_POINT('',(-20.7225806572512,-18.2258898364529,11.1558809418218));
#164455=CARTESIAN_POINT('',(-20.7225805737622,-18.2258896078036,10.9336112541758));
#164456=CARTESIAN_POINT('',(-20.7225805737622,-18.2258896078036,0.));
#164457=CARTESIAN_POINT('',(-20.8509995968923,-18.9533064294668,11.1109437209282));
#164458=CARTESIAN_POINT('Ctrl Pts',(-20.7225806572512,-18.2258898364528,
11.1558809418218));
#164459=CARTESIAN_POINT('Ctrl Pts',(-20.7445653490361,-18.2860987896308,
11.1523876980793));
#164460=CARTESIAN_POINT('Ctrl Pts',(-20.7638236207115,-18.3473280257859,
11.148866803256));
#164461=CARTESIAN_POINT('Ctrl Pts',(-20.7906145474701,-18.4483623738006,
11.1430185087508));
#164462=CARTESIAN_POINT('Ctrl Pts',(-20.7998318209922,-18.4876155904459,
11.1407374682932));
#164463=CARTESIAN_POINT('Ctrl Pts',(-20.8091426747966,-18.5330622494928,
11.1380746906879));
#164464=CARTESIAN_POINT('Ctrl Pts',(-20.810337182083,-18.5390231667149,
11.1377250092448));
#164465=CARTESIAN_POINT('Ctrl Pts',(-20.8121465830655,-18.5482588933868,
11.1371825191121));
#164466=CARTESIAN_POINT('Ctrl Pts',(-20.8127794549061,-18.5515301764636,
11.1369902339572));
#164467=CARTESIAN_POINT('Ctrl Pts',(-20.8188276134209,-18.5831934728326,
11.1351277156095));
#164468=CARTESIAN_POINT('Ctrl Pts',(-20.823668421393,-18.6116910202044,
11.1334407929339));
#164469=CARTESIAN_POINT('Ctrl Pts',(-20.8294677003248,-18.6506463745914,
11.1311168585548));
#164470=CARTESIAN_POINT('Ctrl Pts',(-20.8309342166764,-18.6610261599489,
11.1304959174231));
#164471=CARTESIAN_POINT('Ctrl Pts',(-20.8331379335402,-18.6775064847892,
11.1295071452202));
#164472=CARTESIAN_POINT('Ctrl Pts',(-20.8339257801148,-18.6836001663461,
11.1291409180549));
#164473=CARTESIAN_POINT('Ctrl Pts',(-20.8354516398553,-18.6958202156194,
11.1284052142221));
#164474=CARTESIAN_POINT('Ctrl Pts',(-20.8361894177609,-18.7019465513535,
11.128035733981));
#164475=CARTESIAN_POINT('Ctrl Pts',(-20.8376163916899,-18.7142486771566,
11.1272924615129));
#164476=CARTESIAN_POINT('Ctrl Pts',(-20.8383052007869,-18.7204244495701,
11.1269186609687));
#164477=CARTESIAN_POINT('Ctrl Pts',(-20.8398173182982,-18.7345460163079,
11.1260623577006));
#164478=CARTESIAN_POINT('Ctrl Pts',(-20.8406228592429,-18.7424935818593,
11.125579299856));
#164479=CARTESIAN_POINT('Ctrl Pts',(-20.8425678107231,-18.7628293077294,
11.1243403135426));
#164480=CARTESIAN_POINT('Ctrl Pts',(-20.8436430278982,-18.7752231697907,
11.1235823826888));
#164481=CARTESIAN_POINT('Ctrl Pts',(-20.8489047513537,-18.8427850253306,
11.1194349460567));
#164482=CARTESIAN_POINT('Ctrl Pts',(-20.8510362032082,-18.8980864433055,
11.1159820573408));
#164483=CARTESIAN_POINT('Ctrl Pts',(-20.850999534888,-18.9534033118454,
11.1124694222872));
#164484=CARTESIAN_POINT('Ctrl Pts',(-20.7225805737622,-18.2258896078036,
10.3555828745111));
#164485=CARTESIAN_POINT('Ctrl Pts',(-20.6978476781926,-18.1581542383733,
10.3599055518532));
#164486=CARTESIAN_POINT('Ctrl Pts',(-20.6696396795271,-18.091656105465,
10.3642282291954));
#164487=CARTESIAN_POINT('Ctrl Pts',(-20.6381130015161,-18.0267742559477,
10.3685509065375));
#164488=CARTESIAN_POINT('Ctrl Pts',(-20.6065862617782,-17.9618922793962,
10.3728735923432));
#164489=CARTESIAN_POINT('Ctrl Pts',(-20.5717410483334,-17.8986270362431,
10.3771962781488));
#164490=CARTESIAN_POINT('Ctrl Pts',(-20.5337805560412,-17.837334601732,
10.3815189639545));
#164491=CARTESIAN_POINT('Ctrl Pts',(-20.4957820527404,-17.7759807932207,
10.3858459781984));
#164492=CARTESIAN_POINT('Ctrl Pts',(-20.4546623064218,-17.7166041567963,
10.3901729924423));
#164493=CARTESIAN_POINT('Ctrl Pts',(-20.4106682665917,-17.6595323896498,
10.3945000066862));
#164494=CARTESIAN_POINT('Ctrl Pts',(-20.3666496648147,-17.6024287592391,
10.3988294367095));
#164495=CARTESIAN_POINT('Ctrl Pts',(-20.3197538997825,-17.54763293286,10.4031588667328));
#164496=CARTESIAN_POINT('Ctrl Pts',(-20.270266850603,-17.495437895681,10.4074882967561));
#164497=CARTESIAN_POINT('Ctrl Pts',(-20.2206957041927,-17.4431541593742,
10.41182508412));
#164498=CARTESIAN_POINT('Ctrl Pts',(-20.1685248454057,-17.3934803710856,
10.4161618714839));
#164499=CARTESIAN_POINT('Ctrl Pts',(-20.1140747903873,-17.3466705718334,
10.4204986588478));
#164500=CARTESIAN_POINT('Ctrl Pts',(-20.0868591706488,-17.3232737599101,
10.4226663032283));
#164501=CARTESIAN_POINT('Ctrl Pts',(-20.0590746273095,-17.3005917894749,
10.4248339476089));
#164502=CARTESIAN_POINT('Ctrl Pts',(-20.0307638001156,-17.2786522636613,
10.4270015919895));
#164503=CARTESIAN_POINT('Ctrl Pts',(-19.9734509743369,-17.2342375875375,
10.4313898009204));
#164504=CARTESIAN_POINT('Ctrl Pts',(-19.9137418045022,-17.1926841015565,
10.4357780098513));
#164505=CARTESIAN_POINT('Ctrl Pts',(-19.8519537768686,-17.1542602099344,
10.4401662187822));
#164506=CARTESIAN_POINT('Ctrl Pts',(-19.7902574529128,-17.1158933457383,
10.4445479148834));
#164507=CARTESIAN_POINT('Ctrl Pts',(-19.7264888022834,-17.0806471078962,
10.4489296109847));
#164508=CARTESIAN_POINT('Ctrl Pts',(-19.6609970987602,-17.0487487346937,
10.453311307086));
#164509=CARTESIAN_POINT('Ctrl Pts',(-19.5955823532006,-17.0168878446182,
10.4576878543456));
#164510=CARTESIAN_POINT('Ctrl Pts',(-19.5284490083957,-16.9883672144277,
10.4620644016052));
#164511=CARTESIAN_POINT('Ctrl Pts',(-19.4599724698898,-16.9633690707016,
10.4664409488649));
#164512=CARTESIAN_POINT('Ctrl Pts',(-19.3915393582094,-16.938386780435,
10.4708147205818));
#164513=CARTESIAN_POINT('Ctrl Pts',(-19.3217651949897,-16.9169227092788,
10.4751884922988));
#164514=CARTESIAN_POINT('Ctrl Pts',(-19.2510456730811,-16.8991111155379,
10.4795622640158));
#164515=CARTESIAN_POINT('Ctrl Pts',(-19.1803476713603,-16.8813049419248,
10.4839347047793));
#164516=CARTESIAN_POINT('Ctrl Pts',(-19.108705349564,-16.8671491568768,
10.4883071455429));
#164517=CARTESIAN_POINT('Ctrl Pts',(-19.0365282611611,-16.8567277858954,
10.4926795863065));
#164518=CARTESIAN_POINT('Ctrl Pts',(-18.9643493271821,-16.8463061484384,
10.4970521388738));
#164519=CARTESIAN_POINT('Ctrl Pts',(-18.8916360771606,-16.8396191815878,
10.5014246914411));
#164520=CARTESIAN_POINT('Ctrl Pts',(-18.818805252056,-16.8366992957918,
10.5057972440085));
#164521=CARTESIAN_POINT('Ctrl Pts',(-18.745898840374,-16.8337763796282,
10.5101743345758));
#164522=CARTESIAN_POINT('Ctrl Pts',(-18.6728750930018,-16.8346283697016,
10.5145514251431));
#164523=CARTESIAN_POINT('Ctrl Pts',(-18.6001519939616,-16.8392355286782,
10.5189285157105));
#164524=CARTESIAN_POINT('Ctrl Pts',(-18.5273891781379,-16.8438452037953,
10.5233079967694));
#164525=CARTESIAN_POINT('Ctrl Pts',(-18.4549278170817,-16.8522140756297,
10.5276874778284));
#164526=CARTESIAN_POINT('Ctrl Pts',(-18.3831792948531,-16.8642706514397,
10.5320669588873));
#164527=CARTESIAN_POINT('Ctrl Pts',(-18.3113035988504,-16.8763485974493,
10.536454202547));
#164528=CARTESIAN_POINT('Ctrl Pts',(-18.2401437361919,-16.892127195905,
10.5408414462067));
#164529=CARTESIAN_POINT('Ctrl Pts',(-18.1700988737757,-16.9114842515082,
10.5452286898665));
#164530=CARTESIAN_POINT('Ctrl Pts',(-18.1224751168397,-16.9246451840769,
10.5482115928013));
#164531=CARTESIAN_POINT('Ctrl Pts',(-18.0753664841788,-16.9394592758344,
10.5511944957361));
#164532=CARTESIAN_POINT('Ctrl Pts',(-18.0288930166916,-16.9558754692931,
10.5541773986709));
#164533=CARTESIAN_POINT('Ctrl Pts',(-17.9605249572761,-16.9800256640268,
10.5585656076018));
#164534=CARTESIAN_POINT('Ctrl Pts',(-17.8932656103903,-17.0077395128394,
10.5629538165327));
#164535=CARTESIAN_POINT('Ctrl Pts',(-17.8275125107935,-17.0388953421435,
10.5673420254636));
#164536=CARTESIAN_POINT('Ctrl Pts',(-17.7618569996984,-17.0700049310313,
10.5717237215648));
#164537=CARTESIAN_POINT('Ctrl Pts',(-17.6977037303936,-17.1045461545567,
10.5761054176661));
#164538=CARTESIAN_POINT('Ctrl Pts',(-17.6354328295885,-17.1423483285189,
10.5804871137674));
#164539=CARTESIAN_POINT('Ctrl Pts',(-17.5732351020476,-17.1801060819184,
10.584863661027));
#164540=CARTESIAN_POINT('Ctrl Pts',(-17.5129157592867,-17.2211169246315,
10.5892402082867));
#164541=CARTESIAN_POINT('Ctrl Pts',(-17.4548312249221,-17.2651638357962,
10.5936167555463));
#164542=CARTESIAN_POINT('Ctrl Pts',(-17.3967835269251,-17.30918281305,10.5979905272633));
#164543=CARTESIAN_POINT('Ctrl Pts',(-17.3409682086665,-17.3562337476984,
10.6023642989803));
#164544=CARTESIAN_POINT('Ctrl Pts',(-17.2877123411689,-17.4060565961482,
10.6067380706972));
#164545=CARTESIAN_POINT('Ctrl Pts',(-17.2344726796106,-17.455864283338,
10.6111105114608));
#164546=CARTESIAN_POINT('Ctrl Pts',(-17.1837912746026,-17.5084418803646,
10.6154829522243));
#164547=CARTESIAN_POINT('Ctrl Pts',(-17.1359604618193,-17.5634904989842,
10.6198553929879));
#164548=CARTESIAN_POINT('Ctrl Pts',(-17.0881284259966,-17.6185405252032,
10.6242279455552));
#164549=CARTESIAN_POINT('Ctrl Pts',(-17.0431474419898,-17.6760613330222,
10.6286004981226));
#164550=CARTESIAN_POINT('Ctrl Pts',(-17.001270335834,-17.735720052406,10.63297305069));
#164551=CARTESIAN_POINT('Ctrl Pts',(-16.959349768038,-17.7954406878589,
10.6373501412573));
#164552=CARTESIAN_POINT('Ctrl Pts',(-16.9205397874117,-17.8573032692078,
10.6417272318246));
#164553=CARTESIAN_POINT('Ctrl Pts',(-16.8850500448045,-17.920945654593,
10.6461043223919));
#164554=CARTESIAN_POINT('Ctrl Pts',(-16.8495409199317,-17.984622797447,
10.6504838034509));
#164555=CARTESIAN_POINT('Ctrl Pts',(-16.8173558563404,-18.0500812464321,
10.6548632845098));
#164556=CARTESIAN_POINT('Ctrl Pts',(-16.788657414338,-18.1169363949914,
10.6592427655688));
#164557=CARTESIAN_POINT('Ctrl Pts',(-16.7599081045399,-18.1839100438526,
10.6636300092285));
#164558=CARTESIAN_POINT('Ctrl Pts',(-16.7346579248204,-18.2522848831352,
10.6680172528882));
#164559=CARTESIAN_POINT('Ctrl Pts',(-16.7130201897422,-18.3216591346498,
10.6724044965479));
#164560=CARTESIAN_POINT('Ctrl Pts',(-16.6983086148962,-18.3688269407928,
10.6753873994828));
#164561=CARTESIAN_POINT('Ctrl Pts',(-16.68526591231,-18.4164564326548,10.6783703024176));
#164562=CARTESIAN_POINT('Ctrl Pts',(-16.673914126578,-18.4644190383875,
10.6813532053524));
#164563=CARTESIAN_POINT('Ctrl Pts',(-16.6572142846389,-18.5349777992407,
10.6857414142833));
#164564=CARTESIAN_POINT('Ctrl Pts',(-16.6441110368839,-18.6065332466769,
10.6901296232142));
#164565=CARTESIAN_POINT('Ctrl Pts',(-16.6347172531062,-18.6786852572695,
10.6945178321451));
#164566=CARTESIAN_POINT('Ctrl Pts',(-16.6253374112611,-18.7507301823154,
10.6988995282463));
#164567=CARTESIAN_POINT('Ctrl Pts',(-16.6196561660671,-18.8233694384938,
10.7032812243476));
#164568=CARTESIAN_POINT('Ctrl Pts',(-16.6177357545009,-18.8961910112779,
10.7076629204489));
#164569=CARTESIAN_POINT('Ctrl Pts',(-16.6158175995711,-18.9689270129187,
10.7120394677085));
#164570=CARTESIAN_POINT('Ctrl Pts',(-16.6176515119966,-19.0418444257662,
10.7164160149681));
#164571=CARTESIAN_POINT('Ctrl Pts',(-16.6232479369201,-19.1145260846876,
10.7207925622278));
#164572=CARTESIAN_POINT('Ctrl Pts',(-16.6288408126722,-19.1871616499573,
10.7251663339447));
#164573=CARTESIAN_POINT('Ctrl Pts',(-16.6381914295875,-19.2595612781808,
10.7295401056617));
#164574=CARTESIAN_POINT('Ctrl Pts',(-16.6512581694981,-19.3313091977234,
10.7339138773787));
#164575=CARTESIAN_POINT('Ctrl Pts',(-16.6643209331558,-19.4030352841331,
10.7382863181422));
#164576=CARTESIAN_POINT('Ctrl Pts',(-16.6810974883881,-19.474109581296,
10.7426587589058));
#164577=CARTESIAN_POINT('Ctrl Pts',(-16.7014947532379,-19.5441244986356,
10.7470311996693));
#164578=CARTESIAN_POINT('Ctrl Pts',(-16.7218925396479,-19.6141412062643,
10.7514037522366));
#164579=CARTESIAN_POINT('Ctrl Pts',(-16.7459110826473,-19.6830980177226,
10.755776304804));
#164580=CARTESIAN_POINT('Ctrl Pts',(-16.7734073411518,-19.7506021700889,
10.7601488573713));
#164581=CARTESIAN_POINT('Ctrl Pts',(-16.8009321363106,-19.8181763808109,
10.7645259479386));
#164582=CARTESIAN_POINT('Ctrl Pts',(-16.8319416708358,-19.8842944746724,
10.7689030385059));
#164583=CARTESIAN_POINT('Ctrl Pts',(-16.8662449207617,-19.9485841479673,
10.7732801290733));
#164584=CARTESIAN_POINT('Ctrl Pts',(-16.9005669049657,-20.0129089322389,
10.7776596101322));
#164585=CARTESIAN_POINT('Ctrl Pts',(-16.938185937054,-20.0754028942404,
10.7820390911911));
#164586=CARTESIAN_POINT('Ctrl Pts',(-16.9788666145888,-20.1357211662445,
10.7864185722501));
#164587=CARTESIAN_POINT('Ctrl Pts',(-17.0196193983515,-20.1961463519807,
10.7908058159098));
#164588=CARTESIAN_POINT('Ctrl Pts',(-17.0634443742606,-20.2543877608696,
10.7951930595695));
#164589=CARTESIAN_POINT('Ctrl Pts',(-17.1100650454653,-20.3101326383827,
10.7995803032292));
#164590=CARTESIAN_POINT('Ctrl Pts',(-17.1417626095276,-20.3480337835284,
10.8025632061641));
#164591=CARTESIAN_POINT('Ctrl Pts',(-17.1747517071179,-20.3847815729316,
10.8055461090989));
#164592=CARTESIAN_POINT('Ctrl Pts',(-17.2089361619795,-20.4202878770739,
10.8085290120338));
#164593=CARTESIAN_POINT('Ctrl Pts',(-17.259225605987,-20.4725219203344,
10.8129172209647));
#164594=CARTESIAN_POINT('Ctrl Pts',(-17.3122998738987,-20.5222712846034,
10.8173054298956));
#164595=CARTESIAN_POINT('Ctrl Pts',(-17.3678836195123,-20.5692244850246,
10.8216936388265));
#164596=CARTESIAN_POINT('Ctrl Pts',(-17.4233848696315,-20.6161079991116,
10.8260753349277));
#164597=CARTESIAN_POINT('Ctrl Pts',(-17.4813878383961,-20.6602032789002,
10.830457031029));
#164598=CARTESIAN_POINT('Ctrl Pts',(-17.5415797744867,-20.7012349772934,
10.8348387271303));
#164599=CARTESIAN_POINT('Ctrl Pts',(-17.601700980262,-20.7422184601755,
10.8392152743899));
#164600=CARTESIAN_POINT('Ctrl Pts',(-17.6640056470489,-20.7801452426348,
10.8435918216496));
#164601=CARTESIAN_POINT('Ctrl Pts',(-17.7281486587465,-20.8147807383851,
10.8479683689092));
#164602=CARTESIAN_POINT('Ctrl Pts',(-17.7922509918783,-20.8493942688073,
10.8523421406262));
#164603=CARTESIAN_POINT('Ctrl Pts',(-17.8581889333125,-20.8807204253386,
10.8567159123431));
#164604=CARTESIAN_POINT('Ctrl Pts',(-17.9255903577767,-20.9085691529717,
10.8610896840601));
#164605=CARTESIAN_POINT('Ctrl Pts',(-17.992971271761,-20.9364094061434,
10.8654621248237));
#164606=CARTESIAN_POINT('Ctrl Pts',(-18.0618143390785,-20.9607741471641,
10.8698345655872));
#164607=CARTESIAN_POINT('Ctrl Pts',(-18.1317264570587,-20.9815210221806,
10.8742070063508));
#164608=CARTESIAN_POINT('Ctrl Pts',(-18.2016403626996,-21.002268427697,
10.8785795589181));
#164609=CARTESIAN_POINT('Ctrl Pts',(-18.2726229102622,-21.0193976482243,
10.8829521114855));
#164610=CARTESIAN_POINT('Ctrl Pts',(-18.3442664228595,-21.0328163635576,
10.8873246640528));
#164611=CARTESIAN_POINT('Ctrl Pts',(-18.4159842897964,-21.0462490053399,
10.8917017546201));
#164612=CARTESIAN_POINT('Ctrl Pts',(-18.488364016215,-21.0559633643478,
10.8960788451875));
#164613=CARTESIAN_POINT('Ctrl Pts',(-18.5609891559669,-21.0619185405714,
10.9004559357548));
#164614=CARTESIAN_POINT('Ctrl Pts',(-18.6336539590032,-21.0678769691378,
10.9048354168137));
#164615=CARTESIAN_POINT('Ctrl Pts',(-18.7065639597306,-21.070072112832,
10.9092148978727));
#164616=CARTESIAN_POINT('Ctrl Pts',(-18.7793017600921,-21.0685152374912,
10.9135943789316));
#164617=CARTESIAN_POINT('Ctrl Pts',(-18.8521684877164,-21.0669556025994,
10.9179816225913));
#164618=CARTESIAN_POINT('Ctrl Pts',(-18.9248619239424,-21.0616307033084,
10.9223688662511));
#164619=CARTESIAN_POINT('Ctrl Pts',(-18.996969429205,-21.052603741619,10.9267561099108));
#164620=CARTESIAN_POINT('Ctrl Pts',(-19.0459955845206,-21.0464662775061,
10.9297390128456));
#164621=CARTESIAN_POINT('Ctrl Pts',(-19.0947510327821,-21.0386185484977,
10.9327219157804));
#164622=CARTESIAN_POINT('Ctrl Pts',(-19.1431096126278,-21.0290937207684,
10.9357048187152));
#164623=CARTESIAN_POINT('Ctrl Pts',(-19.2142508990198,-21.0150815537551,
10.9400930276461));
#164624=CARTESIAN_POINT('Ctrl Pts',(-19.2848103359499,-20.9973828809338,
10.944481236577));
#164625=CARTESIAN_POINT('Ctrl Pts',(-19.3543769742706,-20.9760606240414,
10.9488694455079));
#164626=CARTESIAN_POINT('Ctrl Pts',(-19.4238403641657,-20.9547700129135,
10.9532511416092));
#164627=CARTESIAN_POINT('Ctrl Pts',(-19.4923134231176,-20.9298666339678,
10.9576328377105));
#164628=CARTESIAN_POINT('Ctrl Pts',(-19.5593953414347,-20.9014644214086,
10.9620145338117));
#164629=CARTESIAN_POINT('Ctrl Pts',(-19.6263984331591,-20.8730955837095,
10.9663910810714));
#164630=CARTESIAN_POINT('Ctrl Pts',(-19.6920131895943,-20.8412362668758,
10.970767628331));
#164631=CARTESIAN_POINT('Ctrl Pts',(-19.7558555559977,-20.8060496818254,
10.9751441755906));
#164632=CARTESIAN_POINT('Ctrl Pts',(-19.8196574345001,-20.7708854115958,
10.9795179473076));
#164633=CARTESIAN_POINT('Ctrl Pts',(-19.8816887317575,-20.7323982921379,
10.9838917190246));
#164634=CARTESIAN_POINT('Ctrl Pts',(-19.9415882172335,-20.6907983487451,
10.9882654907416));
#164635=CARTESIAN_POINT('Ctrl Pts',(-20.0014694750949,-20.6492110643549,
10.9926379315051));
#164636=CARTESIAN_POINT('Ctrl Pts',(-20.0592198131162,-20.6045131115933,
10.9970103722687));
#164637=CARTESIAN_POINT('Ctrl Pts',(-20.1145067552154,-20.5569579741553,
11.0013828130322));
#164638=CARTESIAN_POINT('Ctrl Pts',(-20.1697951110076,-20.5094016207273,
11.0057553655995));
#164639=CARTESIAN_POINT('Ctrl Pts',(-20.2226195814182,-20.4589882536492,
11.0101279181669));
#164640=CARTESIAN_POINT('Ctrl Pts',(-20.2726818719978,-20.4060106934907,
11.0145004707342));
#164641=CARTESIAN_POINT('Ctrl Pts',(-20.3227961191111,-20.3529781512218,
11.0188775613015));
#164642=CARTESIAN_POINT('Ctrl Pts',(-20.3701421308265,-20.2973764539275,
11.0232546518688));
#164643=CARTESIAN_POINT('Ctrl Pts',(-20.4144601023065,-20.2395336285146,
11.0276317424362));
#164644=CARTESIAN_POINT('Ctrl Pts',(-20.4588022774756,-20.181659212988,
11.0320112234951));
#164645=CARTESIAN_POINT('Ctrl Pts',(-20.5001128464796,-20.1215416302817,
11.036390704554));
#164646=CARTESIAN_POINT('Ctrl Pts',(-20.5381753524531,-20.0595379440908,
11.040770185613));
#164647=CARTESIAN_POINT('Ctrl Pts',(-20.5763053239628,-19.9974243567824,
11.0451574292727));
#164648=CARTESIAN_POINT('Ctrl Pts',(-20.6111755046318,-19.9334184139106,
11.0495446729324));
#164649=CARTESIAN_POINT('Ctrl Pts',(-20.6426156833703,-19.8679012900924,
11.0539319165921));
#164650=CARTESIAN_POINT('Ctrl Pts',(-20.6639919753443,-19.8233559591105,
11.056914819527));
#164651=CARTESIAN_POINT('Ctrl Pts',(-20.6837836766023,-19.7781125159706,
11.0598977224618));
#164652=CARTESIAN_POINT('Ctrl Pts',(-20.7019503858964,-19.7322949946336,
11.0628806253966));
#164653=CARTESIAN_POINT('Ctrl Pts',(-20.7321363776461,-19.6561641280754,
11.0678370477142));
#164654=CARTESIAN_POINT('Ctrl Pts',(-20.7579328257802,-19.5781989207149,
11.0727934700317));
#164655=CARTESIAN_POINT('Ctrl Pts',(-20.7791414399036,-19.4988870914449,
11.0777498923493));
#164656=CARTESIAN_POINT('Ctrl Pts',(-20.8002681015214,-19.4198817321354,
11.0826871624853));
#164657=CARTESIAN_POINT('Ctrl Pts',(-20.8168421753552,-19.339540355719,
11.0876244326213));
#164658=CARTESIAN_POINT('Ctrl Pts',(-20.8287143558559,-19.2583670468105,
11.0925617027573));
#164659=CARTESIAN_POINT('Ctrl Pts',(-20.8405099564276,-19.1777173355875,
11.0974671256858));
#164660=CARTESIAN_POINT('Ctrl Pts',(-20.8476640072491,-19.0962466252352,
11.1023725486143));
#164661=CARTESIAN_POINT('Ctrl Pts',(-20.8500781623711,-19.014467677533,
11.1072779715428));
#164662=CARTESIAN_POINT('Ctrl Pts',(-20.8506795164088,-18.9940969482639,
11.1084998880046));
#164663=CARTESIAN_POINT('Ctrl Pts',(-20.8509870073137,-18.9737071731892,
11.1097218044664));
#164664=CARTESIAN_POINT('Ctrl Pts',(-20.8509995968923,-18.9533064294668,
11.1109437209282));
#164665=CARTESIAN_POINT('',(-20.8509995968923,-18.9506935705329,10.8890562790718));
#164666=CARTESIAN_POINT('Ctrl Pts',(-20.7225805600179,-18.2258895701625,
10.1325349275789));
#164667=CARTESIAN_POINT('Ctrl Pts',(-20.6722698958125,-18.088105006425,
10.1420538457234));
#164668=CARTESIAN_POINT('Ctrl Pts',(-20.6077706502394,-17.9559073673189,
10.1518904366065));
#164669=CARTESIAN_POINT('Ctrl Pts',(-20.4974380565785,-17.7790617276431,
10.1654299361682));
#164670=CARTESIAN_POINT('Ctrl Pts',(-20.4624923458656,-17.7281480080467,
10.1693726022095));
#164671=CARTESIAN_POINT('Ctrl Pts',(-20.4198756844308,-17.6715330590799,
10.1737463730103));
#164672=CARTESIAN_POINT('Ctrl Pts',(-20.4143358467208,-17.6642718224488,
10.1743071185396));
#164673=CARTESIAN_POINT('Ctrl Pts',(-20.4059911886323,-17.6534797680504,
10.1751399143807));
#164674=CARTESIAN_POINT('Ctrl Pts',(-20.4032218823126,-17.6499218010714,
10.1754143728493));
#164675=CARTESIAN_POINT('Ctrl Pts',(-20.3982421186946,-17.6435658654405,
10.1759044412346));
#164676=CARTESIAN_POINT('Ctrl Pts',(-20.3960359481097,-17.6407646199431,
10.1761203480514));
#164677=CARTESIAN_POINT('Ctrl Pts',(-20.3912401600177,-17.6347068046313,
10.1765870757212));
#164678=CARTESIAN_POINT('Ctrl Pts',(-20.3886480248973,-17.6314523011539,
10.1768377124984));
#164679=CARTESIAN_POINT('Ctrl Pts',(-20.3813738002108,-17.6223743398601,
10.1775365908366));
#164680=CARTESIAN_POINT('Ctrl Pts',(-20.376670395407,-17.6165679315093,
10.1779833313244));
#164681=CARTESIAN_POINT('Ctrl Pts',(-20.3490476777093,-17.5828341155106,
10.1805779934644));
#164682=CARTESIAN_POINT('Ctrl Pts',(-20.3254457425266,-17.5554703653355,
10.1826795335719));
#164683=CARTESIAN_POINT('Ctrl Pts',(-20.24702547635,-17.4691227784648,10.1893509179404));
#164684=CARTESIAN_POINT('Ctrl Pts',(-20.1895372441879,-17.4126545856934,
10.1937780147657));
#164685=CARTESIAN_POINT('Ctrl Pts',(-20.0272905113737,-17.2705243031735,
10.2055350940063));
#164686=CARTESIAN_POINT('Ctrl Pts',(-19.9173219580414,-17.1914011543586,
10.212786593459));
#164687=CARTESIAN_POINT('Ctrl Pts',(-19.7460915794008,-17.091533388075,
10.2239369731859));
#164688=CARTESIAN_POINT('Ctrl Pts',(-19.6902328207078,-17.0622161322878,
10.227550613479));
#164689=CARTESIAN_POINT('Ctrl Pts',(-19.621846285762,-17.0301326941873,
10.2319867652531));
#164690=CARTESIAN_POINT('Ctrl Pts',(-19.6104934592948,-17.0249286017124,
10.2327235424176));
#164691=CARTESIAN_POINT('Ctrl Pts',(-19.5917883367819,-17.0165537294021,
10.2339383079784));
#164692=CARTESIAN_POINT('Ctrl Pts',(-19.5844628210791,-17.0133236256764,
10.2344142570031));
#164693=CARTESIAN_POINT('Ctrl Pts',(-19.5712677593889,-17.0075945912745,
10.2352720066905));
#164694=CARTESIAN_POINT('Ctrl Pts',(-19.5654048801239,-17.0050804797521,
10.235653283083));
#164695=CARTESIAN_POINT('Ctrl Pts',(-19.552902804297,-16.9997861271749,
10.2364666969055));
#164696=CARTESIAN_POINT('Ctrl Pts',(-19.5462606255731,-16.9970131759301,
10.2368990764962));
#164697=CARTESIAN_POINT('Ctrl Pts',(-19.5283563830478,-16.9896455771835,
10.2380652387579));
#164698=CARTESIAN_POINT('Ctrl Pts',(-19.5170687757731,-16.9851140788629,
10.2388011455585));
#164699=CARTESIAN_POINT('Ctrl Pts',(-19.4607285948192,-16.9630577206836,
10.2424782923465));
#164700=CARTESIAN_POINT('Ctrl Pts',(-19.4151270607714,-16.9469834991392,
10.2454676788553));
#164701=CARTESIAN_POINT('Ctrl Pts',(-19.2825598929839,-16.9052989597354,
10.2542017552102));
#164702=CARTESIAN_POINT('Ctrl Pts',(-19.1944542502738,-16.8836958992287,
10.2600638150178));
#164703=CARTESIAN_POINT('Ctrl Pts',(-18.9466725317166,-16.8395601520931,
10.2765862455825));
#164704=CARTESIAN_POINT('Ctrl Pts',(-18.7853924176671,-16.829502754587,
10.2874125079016));
#164705=CARTESIAN_POINT('Ctrl Pts',(-18.6045470186046,-16.8388669619853,
10.2987725610644));
#164706=CARTESIAN_POINT('Ctrl Pts',(-18.5845808398868,-16.8401848346858,
10.3000153438669));
#164707=CARTESIAN_POINT('Ctrl Pts',(-18.5582739519772,-16.84229620884,10.3016351049439));
#164708=CARTESIAN_POINT('Ctrl Pts',(-18.5519146187816,-16.8428355572064,
10.3020252934116));
#164709=CARTESIAN_POINT('Ctrl Pts',(-18.5416540709389,-16.843752527851,
10.3026525347584));
#164710=CARTESIAN_POINT('Ctrl Pts',(-18.5377513528179,-16.8441122351258,
10.3028905726005));
#164711=CARTESIAN_POINT('Ctrl Pts',(-18.5302454883645,-16.8448250651861,
10.3033473066581));
#164712=CARTESIAN_POINT('Ctrl Pts',(-18.5266422456396,-16.8451765928858,
10.3035660868237));
#164713=CARTESIAN_POINT('Ctrl Pts',(-18.5181199735707,-16.8460300898083,
10.3040824375918));
#164714=CARTESIAN_POINT('Ctrl Pts',(-18.5132017326801,-16.846540056253,
10.3043795592571));
#164715=CARTESIAN_POINT('Ctrl Pts',(-18.4968937250302,-16.8482887855668,
10.3053620191345));
#164716=CARTESIAN_POINT('Ctrl Pts',(-18.4855120018367,-16.8496027998366,
10.3060432596486));
#164717=CARTESIAN_POINT('Ctrl Pts',(-18.3863820814095,-16.8618635767563,
10.3119421836834));
#164718=CARTESIAN_POINT('Ctrl Pts',(-18.2993781328926,-16.8782073210213,
10.3168859421917));
#164719=CARTESIAN_POINT('Ctrl Pts',(-18.1191969458372,-16.9238974976155,
10.3270941912273));
#164720=CARTESIAN_POINT('Ctrl Pts',(-18.0265165640879,-16.9543387867889,
10.332330621597));
#164721=CARTESIAN_POINT('Ctrl Pts',(-17.8257067310208,-17.0360309412018,
10.3441890971973));
#164722=CARTESIAN_POINT('Ctrl Pts',(-17.7191682471214,-17.0902682509176,
10.3508437354321));
#164723=CARTESIAN_POINT('Ctrl Pts',(-17.6044270454248,-17.1614691647971,
10.3587543846365));
#164724=CARTESIAN_POINT('Ctrl Pts',(-17.5911731047225,-17.1698994419165,
10.3596798221563));
#164725=CARTESIAN_POINT('Ctrl Pts',(-17.5712616922301,-17.1828777316155,
10.3610884326554));
#164726=CARTESIAN_POINT('Ctrl Pts',(-17.5645341859119,-17.1873176830426,
10.3615675737536));
#164727=CARTESIAN_POINT('Ctrl Pts',(-17.5525237270254,-17.1953430672374,
10.3624288249267));
#164728=CARTESIAN_POINT('Ctrl Pts',(-17.5472313030677,-17.1989142001527,
10.3628103928089));
#164729=CARTESIAN_POINT('Ctrl Pts',(-17.5360350484277,-17.2065429556181,
10.3636220262905));
#164730=CARTESIAN_POINT('Ctrl Pts',(-17.5301355085513,-17.2106067063289,
10.3640523216783));
#164731=CARTESIAN_POINT('Ctrl Pts',(-17.5144013886891,-17.2215629304622,
10.3652070469168));
#164732=CARTESIAN_POINT('Ctrl Pts',(-17.5046047509211,-17.2285092003234,
10.3659335294753));
#164733=CARTESIAN_POINT('Ctrl Pts',(-17.457180036748,-17.2627456105679,
10.3694876167285));
#164734=CARTESIAN_POINT('Ctrl Pts',(-17.4204010254147,-17.2911848955679,
10.3723595748265));
#164735=CARTESIAN_POINT('Ctrl Pts',(-17.2543809878062,-17.4285257944055,
10.3858828288633));
#164736=CARTESIAN_POINT('Ctrl Pts',(-17.1375539378973,-17.5514326334662,
10.3971043873977));
#164737=CARTESIAN_POINT('Ctrl Pts',(-16.9772917657285,-17.7664563697633,
10.4147714372532));
#164738=CARTESIAN_POINT('Ctrl Pts',(-16.9236474072575,-17.8501081331215,
10.4212384656095));
#164739=CARTESIAN_POINT('Ctrl Pts',(-16.8714188430713,-17.9457324311004,
10.4279703856484));
#164740=CARTESIAN_POINT('Ctrl Pts',(-16.8668301438752,-17.9542727211565,
10.4285660569338));
#164741=CARTESIAN_POINT('Ctrl Pts',(-16.8601417705764,-17.9669285938369,
10.4294402619331));
#164742=CARTESIAN_POINT('Ctrl Pts',(-16.8579967152668,-17.9710198698124,
10.4297215614841));
#164743=CARTESIAN_POINT('Ctrl Pts',(-16.8542150737047,-17.9782903840641,
10.4302190959633));
#164744=CARTESIAN_POINT('Ctrl Pts',(-16.8525731348201,-17.9814667769973,
10.4304356657734));
#164745=CARTESIAN_POINT('Ctrl Pts',(-16.8490725670424,-17.9882810263389,
10.4308985543064));
#164746=CARTESIAN_POINT('Ctrl Pts',(-16.8472164226835,-17.991920096696,
10.4311447168412));
#164747=CARTESIAN_POINT('Ctrl Pts',(-16.8421505126772,-18.0019235167467,
10.431818609706));
#164748=CARTESIAN_POINT('Ctrl Pts',(-16.8389623039613,-18.0082988075681,
10.4322450080803));
#164749=CARTESIAN_POINT('Ctrl Pts',(-16.8221168459389,-18.0424133997934,
10.4345109315879));
#164750=CARTESIAN_POINT('Ctrl Pts',(-16.8090355584501,-18.0704348556229,
10.4363167328191));
#164751=CARTESIAN_POINT('Ctrl Pts',(-16.7713065040379,-18.1561025858176,
10.4417010775681));
#164752=CARTESIAN_POINT('Ctrl Pts',(-16.7485995112676,-18.2145689859085,
10.445192914413));
#164753=CARTESIAN_POINT('Ctrl Pts',(-16.6854703523919,-18.4012902075537,
10.456025536414));
#164754=CARTESIAN_POINT('Ctrl Pts',(-16.65464547695,-18.5324282384631,10.4631933055997));
#164755=CARTESIAN_POINT('Ctrl Pts',(-16.6309427723183,-18.7060252921972,
10.4729167940072));
#164756=CARTESIAN_POINT('Ctrl Pts',(-16.626593581554,-18.7465950294605,
10.4752036207267));
#164757=CARTESIAN_POINT('Ctrl Pts',(-16.6196346571376,-18.8357518755165,
10.4802860732568));
#164758=CARTESIAN_POINT('Ctrl Pts',(-16.6175223170951,-18.8843530252401,
10.4830935736719));
#164759=CARTESIAN_POINT('Ctrl Pts',(-16.6169721783228,-18.9455871747464,
10.486695070223));
#164760=CARTESIAN_POINT('Ctrl Pts',(-16.6169715281791,-18.9581936451916,
10.4874399163679));
#164761=CARTESIAN_POINT('Ctrl Pts',(-16.617148912416,-18.9781683387249,
10.4886257726986));
#164762=CARTESIAN_POINT('Ctrl Pts',(-16.6172528319408,-18.9855370446611,
10.4890644584691));
#164763=CARTESIAN_POINT('Ctrl Pts',(-16.6175181386771,-18.9992651874869,
10.4898840780203));
#164764=CARTESIAN_POINT('Ctrl Pts',(-16.6176697203885,-19.0056247469814,
10.4902646998807));
#164765=CARTESIAN_POINT('Ctrl Pts',(-16.6180700260682,-19.0197470848625,
10.4911120401309));
#164766=CARTESIAN_POINT('Ctrl Pts',(-16.6183328100806,-19.0275093443341,
10.491579194487));
#164767=CARTESIAN_POINT('Ctrl Pts',(-16.619220365993,-19.0500565280489,
10.4929403550887));
#164768=CARTESIAN_POINT('Ctrl Pts',(-16.6199574445897,-19.0648363397659,
10.4938378668877));
#164769=CARTESIAN_POINT('Ctrl Pts',(-16.6270369902696,-19.1820725058894,
10.5010001774815));
#164770=CARTESIAN_POINT('Ctrl Pts',(-16.6406680022971,-19.2839370731793,
10.5074949742385));
#164771=CARTESIAN_POINT('Ctrl Pts',(-16.6931329952607,-19.5353872176744,
10.5241676617908));
#164772=CARTESIAN_POINT('Ctrl Pts',(-16.741039872768,-19.6824690138303,
10.5345293706769));
#164773=CARTESIAN_POINT('Ctrl Pts',(-16.8267781797308,-19.872394814259,
10.548004025483));
#164774=CARTESIAN_POINT('Ctrl Pts',(-16.8509477519544,-19.9208844078065,
10.5514482833337));
#164775=CARTESIAN_POINT('Ctrl Pts',(-16.8811561096825,-19.9760777169471,
10.5553298831095));
#164776=CARTESIAN_POINT('Ctrl Pts',(-16.8854072393869,-19.9837317789636,
10.5558672718623));
#164777=CARTESIAN_POINT('Ctrl Pts',(-16.8919105706579,-19.9952716332977,
10.5566758566068));
#164778=CARTESIAN_POINT('Ctrl Pts',(-16.8941277931071,-19.9991768855835,
10.5569492098837));
#164779=CARTESIAN_POINT('Ctrl Pts',(-16.8981271548686,-20.0061691522531,
10.5574380922266));
#164780=CARTESIAN_POINT('Ctrl Pts',(-16.8999046715142,-20.0092587344969,
10.5576539120312));
#164781=CARTESIAN_POINT('Ctrl Pts',(-16.903780660933,-20.0159565748604,
10.5581213519162));
#164782=CARTESIAN_POINT('Ctrl Pts',(-16.9058819975309,-20.0195631091523,
10.5583727830689));
#164783=CARTESIAN_POINT('Ctrl Pts',(-16.911805962269,-20.0296616568609,
10.5590761238205));
#164784=CARTESIAN_POINT('Ctrl Pts',(-16.9156526423605,-20.0361395890955,
10.5595265011856));
#164785=CARTESIAN_POINT('Ctrl Pts',(-16.9386800343948,-20.0744511048151,
10.5621862115086));
#164786=CARTESIAN_POINT('Ctrl Pts',(-16.9586630301275,-20.1057977662017,
10.5643464045908));
#164787=CARTESIAN_POINT('Ctrl Pts',(-17.0267137532656,-20.2065888709176,
10.5712945173517));
#164788=CARTESIAN_POINT('Ctrl Pts',(-17.0781140338294,-20.2736896301121,
10.5759257334966));
#164789=CARTESIAN_POINT('Ctrl Pts',(-17.2506581557071,-20.4730162841514,
10.5902792368159));
#164790=CARTESIAN_POINT('Ctrl Pts',(-17.3846355336124,-20.5930370498418,
10.5998939651431));
#164791=CARTESIAN_POINT('Ctrl Pts',(-17.5508115398299,-20.7076393325562,
10.6116272333925));
#164792=CARTESIAN_POINT('Ctrl Pts',(-17.5697060862666,-20.7202262361048,
10.6129575213388));
#164793=CARTESIAN_POINT('Ctrl Pts',(-17.5967877348927,-20.7376448382678,
10.614860577841));
#164794=CARTESIAN_POINT('Ctrl Pts',(-17.6048109811919,-20.7427292870994,
10.6154239303715));
#164795=CARTESIAN_POINT('Ctrl Pts',(-17.6179222192687,-20.7509149197118,
10.6163439252608));
#164796=CARTESIAN_POINT('Ctrl Pts',(-17.6229896219742,-20.7540489559957,
10.6166993495682));
#164797=CARTESIAN_POINT('Ctrl Pts',(-17.6336402254532,-20.7605740342824,
10.6174461013302));
#164798=CARTESIAN_POINT('Ctrl Pts',(-17.6392260183593,-20.7639607055782,
10.6178375841665));
#164799=CARTESIAN_POINT('Ctrl Pts',(-17.6525808019803,-20.7719734270524,
10.6187732325132));
#164800=CARTESIAN_POINT('Ctrl Pts',(-17.6603638841503,-20.7765756338942,
10.619318260011));
#164801=CARTESIAN_POINT('Ctrl Pts',(-17.6868238543261,-20.7919937301016,
10.6211704423554));
#164802=CARTESIAN_POINT('Ctrl Pts',(-17.7056360977903,-20.8025735428203,
10.6224860725914));
#164803=CARTESIAN_POINT('Ctrl Pts',(-17.8098762366445,-20.8591168286656,
10.6297718146139));
#164804=CARTESIAN_POINT('Ctrl Pts',(-17.8982128622423,-20.8994482620257,
10.6359383220046));
#164805=CARTESIAN_POINT('Ctrl Pts',(-18.121404318156,-20.9833607784153,
10.6514460292614));
#164806=CARTESIAN_POINT('Ctrl Pts',(-18.2584637581474,-21.0197433723829,
10.6609235987738));
#164807=CARTESIAN_POINT('Ctrl Pts',(-18.4591174948786,-21.0519869038313,
10.6741249126858));
#164808=CARTESIAN_POINT('Ctrl Pts',(-18.5205181290289,-21.0591147097923,
10.6780715520071));
#164809=CARTESIAN_POINT('Ctrl Pts',(-18.5912594754872,-21.064202070666,
10.6824491631104));
#164810=CARTESIAN_POINT('Ctrl Pts',(-18.6003750853159,-21.0647983419468,
10.6830100260713));
#164811=CARTESIAN_POINT('Ctrl Pts',(-18.6139956483926,-21.0656007869646,
10.6838429615622));
#164812=CARTESIAN_POINT('Ctrl Pts',(-18.6184977255407,-21.065851592834,
10.6841174434136));
#164813=CARTESIAN_POINT('Ctrl Pts',(-18.6265614269687,-21.0662749743925,
10.6846075369578));
#164814=CARTESIAN_POINT('Ctrl Pts',(-18.6301227040379,-21.0664529368859,
10.684823445681));
#164815=CARTESIAN_POINT('Ctrl Pts',(-18.6378401379202,-21.0668190440643,
10.6852901585808));
#164816=CARTESIAN_POINT('Ctrl Pts',(-18.6419963916222,-21.0670039349708,
10.6855407787833));
#164817=CARTESIAN_POINT('Ctrl Pts',(-18.6536176828466,-21.0674865864939,
10.6862395641056));
#164818=CARTESIAN_POINT('Ctrl Pts',(-18.6610838763265,-21.0677570884272,
10.6866862287983));
#164819=CARTESIAN_POINT('Ctrl Pts',(-18.7046408023064,-21.0691043251046,
10.6892795575349));
#164820=CARTESIAN_POINT('Ctrl Pts',(-18.740755245574,-21.069297192962,10.6913798956955));
#164821=CARTESIAN_POINT('Ctrl Pts',(-18.8572742825499,-21.0669377469551,
10.6980456916112));
#164822=CARTESIAN_POINT('Ctrl Pts',(-18.9375377343523,-21.0607277292522,
10.702468676844));
#164823=CARTESIAN_POINT('Ctrl Pts',(-19.2007449267228,-21.0251905831569,
10.7169459827154));
#164824=CARTESIAN_POINT('Ctrl Pts',(-19.3801672616446,-20.9764584051596,
10.7268511112178));
#164825=CARTESIAN_POINT('Ctrl Pts',(-19.571394849294,-20.8964663667563,
10.7389062784494));
#164826=CARTESIAN_POINT('Ctrl Pts',(-19.5916922970075,-20.887598991046,
10.7402046340292));
#164827=CARTESIAN_POINT('Ctrl Pts',(-19.6195497484071,-20.8749046540006,
10.7420142327873));
#164828=CARTESIAN_POINT('Ctrl Pts',(-19.6272319532677,-20.871348154916,
10.7425162042258));
#164829=CARTESIAN_POINT('Ctrl Pts',(-19.6403943259379,-20.8651584590622,
10.7433814166704));
#164830=CARTESIAN_POINT('Ctrl Pts',(-19.6458848998638,-20.8625475371704,
10.7437438846988));
#164831=CARTESIAN_POINT('Ctrl Pts',(-19.657058947053,-20.8571748237869,
10.7444847614002));
#164832=CARTESIAN_POINT('Ctrl Pts',(-19.6627414502739,-20.8544111664218,
10.7448632322053));
#164833=CARTESIAN_POINT('Ctrl Pts',(-19.6758282027507,-20.8479738802264,
10.7457388236822));
#164834=CARTESIAN_POINT('Ctrl Pts',(-19.6832234443535,-20.8442822642674,
10.7462365696697));
#164835=CARTESIAN_POINT('Ctrl Pts',(-19.698752716199,-20.836416297489,10.7472881003529));
#164836=CARTESIAN_POINT('Ctrl Pts',(-19.7068816860658,-20.8322323809728,
10.7478422145986));
#164837=CARTESIAN_POINT('Ctrl Pts',(-19.7284727436111,-20.8209421304386,
10.7493239179516));
#164838=CARTESIAN_POINT('Ctrl Pts',(-19.7418855258113,-20.8137431274456,
10.7502547604062));
#164839=CARTESIAN_POINT('Ctrl Pts',(-19.7826080439514,-20.7913172142988,
10.7531131738256));
#164840=CARTESIAN_POINT('Ctrl Pts',(-19.8096581337974,-20.7756299139956,
10.755056821481));
#164841=CARTESIAN_POINT('Ctrl Pts',(-19.9115933758983,-20.7134569534753,
10.7625562930663));
#164842=CARTESIAN_POINT('Ctrl Pts',(-19.9838897543784,-20.6629147966443,
10.768249228799));
#164843=CARTESIAN_POINT('Ctrl Pts',(-20.1501754307354,-20.5304883149296,
10.7821903337796));
#164844=CARTESIAN_POINT('Ctrl Pts',(-20.2405030026954,-20.4445237217131,
10.7905059498207));
#164845=CARTESIAN_POINT('Ctrl Pts',(-20.3265463925974,-20.3468182249581,
10.7989321283601));
#164846=CARTESIAN_POINT('Ctrl Pts',(-20.3303193418767,-20.3424986346499,
10.7993026986361));
#164847=CARTESIAN_POINT('Ctrl Pts',(-20.3456139976044,-20.32484372755,10.8008091845524));
#164848=CARTESIAN_POINT('Ctrl Pts',(-20.3569868081859,-20.3113797962197,
10.8019393528701));
#164849=CARTESIAN_POINT('Ctrl Pts',(-20.3899140874462,-20.2713958151356,
10.8052375596493));
#164850=CARTESIAN_POINT('Ctrl Pts',(-20.4109972825622,-20.2444926318388,
10.8073832829217));
#164851=CARTESIAN_POINT('Ctrl Pts',(-20.4355884802939,-20.2114976279042,
10.8099164130435));
#164852=CARTESIAN_POINT('Ctrl Pts',(-20.4397282118522,-20.2058855216293,
10.8103439275266));
#164853=CARTESIAN_POINT('Ctrl Pts',(-20.4464704608535,-20.1966500792647,
10.8110418530585));
#164854=CARTESIAN_POINT('Ctrl Pts',(-20.4490893537915,-20.1930388424476,
10.8113133619646));
#164855=CARTESIAN_POINT('Ctrl Pts',(-20.4537791936258,-20.1865287427941,
10.8118002790251));
#164856=CARTESIAN_POINT('Ctrl Pts',(-20.4558542443182,-20.1836329215729,
10.8120159676145));
#164857=CARTESIAN_POINT('Ctrl Pts',(-20.460358134635,-20.1773139220428,
10.8124846598887));
#164858=CARTESIAN_POINT('Ctrl Pts',(-20.4627840992379,-20.1738887655987,
10.8127374663054));
#164859=CARTESIAN_POINT('Ctrl Pts',(-20.4695975818573,-20.1642080741141,
10.8134485538441));
#164860=CARTESIAN_POINT('Ctrl Pts',(-20.4739614946099,-20.1579358948144,
10.8139052479421));
#164861=CARTESIAN_POINT('Ctrl Pts',(-20.5004231915003,-20.1194602633663,
10.8166831680809));
#164862=CARTESIAN_POINT('Ctrl Pts',(-20.5216618107861,-20.0866717784964,
10.8189500255668));
#164863=CARTESIAN_POINT('Ctrl Pts',(-20.6270022752281,-19.9137383238074,
10.8304965834505));
#164864=CARTESIAN_POINT('Ctrl Pts',(-20.6955814745115,-19.7647772513501,
10.8391212131246));
#164865=CARTESIAN_POINT('Ctrl Pts',(-20.7656532888853,-19.5502820287956,
10.8515090133897));
#164866=CARTESIAN_POINT('Ctrl Pts',(-20.7823497632473,-19.4903483736763,
10.8549621547645));
#164867=CARTESIAN_POINT('Ctrl Pts',(-20.8079993458133,-19.3796270822072,
10.8614076387259));
#164868=CARTESIAN_POINT('Ctrl Pts',(-20.8177820311267,-19.3290809298379,
10.8643744138636));
#164869=CARTESIAN_POINT('Ctrl Pts',(-20.8276939265967,-19.2655283584958,
10.8681560229178));
#164870=CARTESIAN_POINT('Ctrl Pts',(-20.8295593324667,-19.252807850628,
10.8689154551197));
#164871=CARTESIAN_POINT('Ctrl Pts',(-20.8323193599981,-19.232713419598,
10.8701193860392));
#164872=CARTESIAN_POINT('Ctrl Pts',(-20.8332912550207,-19.2253502970991,
10.8705614382008));
#164873=CARTESIAN_POINT('Ctrl Pts',(-20.8349476974874,-19.2122708513839,
10.8713483300385));
#164874=CARTESIAN_POINT('Ctrl Pts',(-20.8356477136965,-19.2065565362713,
10.8716926770491));
#164875=CARTESIAN_POINT('Ctrl Pts',(-20.8370323024389,-19.1948588156978,
10.8723987589714));
#164876=CARTESIAN_POINT('Ctrl Pts',(-20.8377146681132,-19.1888752065147,
10.8727605602234));
#164877=CARTESIAN_POINT('Ctrl Pts',(-20.8391674074184,-19.1756346206786,
10.8735625742349));
#164878=CARTESIAN_POINT('Ctrl Pts',(-20.8399258046106,-19.1683764317348,
10.8740031604327));
#164879=CARTESIAN_POINT('Ctrl Pts',(-20.8417118990209,-19.1503830876938,
10.8750977751567));
#164880=CARTESIAN_POINT('Ctrl Pts',(-20.8426951156183,-19.139643815158,
10.8757531931529));
#164881=CARTESIAN_POINT('Ctrl Pts',(-20.8485694989575,-19.0695887482446,
10.8800427237244));
#164882=CARTESIAN_POINT('Ctrl Pts',(-20.8510389800155,-19.0101025990038,
10.8837519461892));
#164883=CARTESIAN_POINT('Ctrl Pts',(-20.8509995348883,-18.9505966887089,
10.8875305864451));
#164884=CARTESIAN_POINT('Ctrl Pts',(-20.7225805737622,-18.2258896078036,
10.9336112541758));
#164885=CARTESIAN_POINT('Ctrl Pts',(-20.7506609300752,-18.3027925851862,
10.9286590766383));
#164886=CARTESIAN_POINT('Ctrl Pts',(-20.774308399499,-18.3814140088411,
10.9237068991007));
#164887=CARTESIAN_POINT('Ctrl Pts',(-20.7933360861973,-18.4612618986816,
10.9187547215632));
#164888=CARTESIAN_POINT('Ctrl Pts',(-20.8123544087724,-18.5410704928639,
10.9138049811479));
#164889=CARTESIAN_POINT('Ctrl Pts',(-20.8267573247981,-18.6221041354718,
10.9088552407327));
#164890=CARTESIAN_POINT('Ctrl Pts',(-20.8364059167827,-18.7038501237617,
10.9039055003175));
#164891=CARTESIAN_POINT('Ctrl Pts',(-20.8460545087673,-18.7855961120516,
10.8989557599023));
#164892=CARTESIAN_POINT('Ctrl Pts',(-20.8509485990149,-18.8680542176316,
10.894006019487));
#164893=CARTESIAN_POINT('Ctrl Pts',(-20.8509995968923,-18.9506935705329,
10.8890562790718));
#164894=CARTESIAN_POINT('Origin',(-18.734,-18.952,0.));
#164895=CARTESIAN_POINT('',(-20.7225805737639,-18.2258896078082,11.9535388216361));
#164896=CARTESIAN_POINT('',(-20.7219729293148,-18.2261210096956,11.7337477406533));
#164897=CARTESIAN_POINT('',(-20.7225805737622,-18.2258896078036,0.));
#164898=CARTESIAN_POINT('Ctrl Pts',(-20.7225805737639,-18.2258896078082,
11.9535388216361));
#164899=CARTESIAN_POINT('Ctrl Pts',(-20.7228709312506,-18.2266848026764,
11.9534867202617));
#164900=CARTESIAN_POINT('Ctrl Pts',(-20.7231608131558,-18.227480175522,
11.9534346446637));
#164901=CARTESIAN_POINT('Ctrl Pts',(-20.725902506219,-18.2350168328669,
11.9529415517011));
#164902=CARTESIAN_POINT('Ctrl Pts',(-20.7283205553233,-18.2417704721402,
11.9525023862134));
#164903=CARTESIAN_POINT('Ctrl Pts',(-20.7320650323148,-18.2523987590967,
11.9518156428223));
#164904=CARTESIAN_POINT('Ctrl Pts',(-20.7334145990786,-18.2562651142276,
11.9515667258745));
#164905=CARTESIAN_POINT('Ctrl Pts',(-20.7359210084393,-18.2635132172769,
11.9511018196));
#164906=CARTESIAN_POINT('Ctrl Pts',(-20.7370804929103,-18.2668939402145,
11.9508856802641));
#164907=CARTESIAN_POINT('Ctrl Pts',(-20.7397139281656,-18.2746361153159,
11.9503922975431));
#164908=CARTESIAN_POINT('Ctrl Pts',(-20.741182214819,-18.2789994417947,
11.9501153908462));
#164909=CARTESIAN_POINT('Ctrl Pts',(-20.7456726548253,-18.2924891564348,
11.9492627605705));
#164910=CARTESIAN_POINT('Ctrl Pts',(-20.748646932759,-18.3016315143292,
11.9486897864207));
#164911=CARTESIAN_POINT('Ctrl Pts',(-20.7774525836471,-18.3922686854927,
11.9430545507576));
#164912=CARTESIAN_POINT('Ctrl Pts',(-20.7983905072509,-18.475247455487,
11.9382548304568));
#164913=CARTESIAN_POINT('Ctrl Pts',(-20.8385991713034,-18.6882312932793,
11.9263204505388));
#164914=CARTESIAN_POINT('Ctrl Pts',(-20.8509009167449,-18.8191722303356,
11.9193213968354));
#164915=CARTESIAN_POINT('Ctrl Pts',(-20.8510686213727,-19.0426470678854,
11.9069621000412));
#164916=CARTESIAN_POINT('Ctrl Pts',(-20.8451100146564,-19.1347783337778,
11.9017508967304));
#164917=CARTESIAN_POINT('Ctrl Pts',(-20.8313804901704,-19.2398780717802,
11.8955372391559));
#164918=CARTESIAN_POINT('Ctrl Pts',(-20.8294631847735,-19.2535173836545,
11.8947257424901));
#164919=CARTESIAN_POINT('Ctrl Pts',(-20.8261768229805,-19.2753482609065,
11.8934182636011));
#164920=CARTESIAN_POINT('Ctrl Pts',(-20.8248923983335,-19.2835523066434,
11.8929249583066));
#164921=CARTESIAN_POINT('Ctrl Pts',(-20.822527335613,-19.2980981837992,
11.8920467670036));
#164922=CARTESIAN_POINT('Ctrl Pts',(-20.8214659899728,-19.3044430787071,
11.8916624977564));
#164923=CARTESIAN_POINT('Ctrl Pts',(-20.8191956396849,-19.3176454991027,
11.8908603644548));
#164924=CARTESIAN_POINT('Ctrl Pts',(-20.8179816893291,-19.3245020852471,
11.8904423472302));
#164925=CARTESIAN_POINT('Ctrl Pts',(-20.814744118203,-19.3422771081671,
11.8893548950549));
#164926=CARTESIAN_POINT('Ctrl Pts',(-20.8126683981604,-19.3531857297131,
11.8886838073358));
#164927=CARTESIAN_POINT('Ctrl Pts',(-20.8033102385072,-19.4003426132209,
11.8857663337448));
#164928=CARTESIAN_POINT('Ctrl Pts',(-20.7951650843611,-19.4364111752216,
11.8834925737344));
#164929=CARTESIAN_POINT('Ctrl Pts',(-20.7710540925085,-19.5315155296063,
11.8773805295259));
#164930=CARTESIAN_POINT('Ctrl Pts',(-20.7534686094193,-19.5901011389758,
11.8734935544757));
#164931=CARTESIAN_POINT('Ctrl Pts',(-20.6816192014538,-19.7965478971811,
11.8593775533143));
#164932=CARTESIAN_POINT('Ctrl Pts',(-20.6134415276801,-19.939003132821,
11.8488054745441));
#164933=CARTESIAN_POINT('Ctrl Pts',(-20.4974380103206,-20.1249383399141,
11.834570067347));
#164934=CARTESIAN_POINT('Ctrl Pts',(-20.4624923195146,-20.175852027263,
11.8306274038046));
#164935=CARTESIAN_POINT('Ctrl Pts',(-20.4198756814308,-20.2324669448607,
11.8262536354274));
#164936=CARTESIAN_POINT('Ctrl Pts',(-20.4143358444966,-20.2397281804442,
11.8256928899791));
#164937=CARTESIAN_POINT('Ctrl Pts',(-20.4059911873827,-20.2505202335576,
11.8248600942372));
#164938=CARTESIAN_POINT('Ctrl Pts',(-20.40322188125,-20.2540782002897,11.8245856357877));
#164939=CARTESIAN_POINT('Ctrl Pts',(-20.3982421178699,-20.2604341356083,
11.8240955674265));
#164940=CARTESIAN_POINT('Ctrl Pts',(-20.3960359473336,-20.2632353810404,
11.8238796606147));
#164941=CARTESIAN_POINT('Ctrl Pts',(-20.3912401592339,-20.269293196355,
11.8234129329448));
#164942=CARTESIAN_POINT('Ctrl Pts',(-20.3886480240565,-20.2725476999,11.8231622961623));
#164943=CARTESIAN_POINT('Ctrl Pts',(-20.3813737989229,-20.2816256617391,
11.8224634177822));
#164944=CARTESIAN_POINT('Ctrl Pts',(-20.3766703937245,-20.2874320705638,
11.8220166772581));
#164945=CARTESIAN_POINT('Ctrl Pts',(-20.349047668151,-20.3211658960738,
11.8194220143871));
#164946=CARTESIAN_POINT('Ctrl Pts',(-20.3254457250298,-20.3485296549071,
11.817320473616));
#164947=CARTESIAN_POINT('Ctrl Pts',(-20.2470254196683,-20.4348772817698,
11.8106490861315));
#164948=CARTESIAN_POINT('Ctrl Pts',(-20.1895371530908,-20.4913455027572,
11.8062219870092));
#164949=CARTESIAN_POINT('Ctrl Pts',(-20.0272904009265,-20.6334757790618,
11.7944649073733));
#164950=CARTESIAN_POINT('Ctrl Pts',(-19.9173218706877,-20.7125989017598,
11.7872134095763));
#164951=CARTESIAN_POINT('Ctrl Pts',(-19.7460915352509,-20.8124666352626,
11.7760630327267));
#164952=CARTESIAN_POINT('Ctrl Pts',(-19.6902327937904,-20.8417838806634,
11.7724493935458));
#164953=CARTESIAN_POINT('Ctrl Pts',(-19.6218462783899,-20.8738673092074,
11.7680132430391));
#164954=CARTESIAN_POINT('Ctrl Pts',(-19.6104934534501,-20.8790714009349,
11.7672764659737));
#164955=CARTESIAN_POINT('Ctrl Pts',(-19.5917883330134,-20.8874462722656,
11.7660617005476));
#164956=CARTESIAN_POINT('Ctrl Pts',(-19.58446281785,-20.8906763757377,11.7655857515579));
#164957=CARTESIAN_POINT('Ctrl Pts',(-19.5712677568455,-20.8964054098201,
11.764728001915));
#164958=CARTESIAN_POINT('Ctrl Pts',(-19.5654048777231,-20.8989195212726,
11.7643467255317));
#164959=CARTESIAN_POINT('Ctrl Pts',(-19.5529028018915,-20.9042138738347,
11.7635333117088));
#164960=CARTESIAN_POINT('Ctrl Pts',(-19.5462606230191,-20.9069868251316,
11.7631009321083));
#164961=CARTESIAN_POINT('Ctrl Pts',(-19.5283563793399,-20.9143544243242,
11.7619347697713));
#164962=CARTESIAN_POINT('Ctrl Pts',(-19.5170687710539,-20.9188859230227,
11.7611988629045));
#164963=CARTESIAN_POINT('Ctrl Pts',(-19.4607285749817,-20.9409422869315,
11.757521715128));
#164964=CARTESIAN_POINT('Ctrl Pts',(-19.4151270264761,-20.957016512875,
11.7545323276651));
#164965=CARTESIAN_POINT('Ctrl Pts',(-19.2825598008812,-20.9987010669186,
11.745798247469));
#164966=CARTESIAN_POINT('Ctrl Pts',(-19.1944541136651,-21.0203041331306,
11.7399361846457));
#164967=CARTESIAN_POINT('Ctrl Pts',(-18.9466719648108,-21.0644399346196,
11.7234137253526));
#164968=CARTESIAN_POINT('Ctrl Pts',(-18.7853914552946,-21.074497298231,
11.7125874362613));
#164969=CARTESIAN_POINT('Ctrl Pts',(-18.604546034287,-21.0651329742962,
11.7012273863597));
#164970=CARTESIAN_POINT('Ctrl Pts',(-18.5845802163514,-21.0638151177757,
11.6999846263648));
#164971=CARTESIAN_POINT('Ctrl Pts',(-18.5582737333368,-21.0617037728127,
11.6983648903738));
#164972=CARTESIAN_POINT('Ctrl Pts',(-18.5519144449285,-21.0611644276489,
11.6979747046831));
#164973=CARTESIAN_POINT('Ctrl Pts',(-18.5416539518808,-21.060247461268,
11.6973474667173));
#164974=CARTESIAN_POINT('Ctrl Pts',(-18.5377512437939,-21.0598877547051,
11.6971094294979));
#164975=CARTESIAN_POINT('Ctrl Pts',(-18.5302453855069,-21.0591749248747,
11.6966526958337));
#164976=CARTESIAN_POINT('Ctrl Pts',(-18.52664213892,-21.0588233966174,11.6964339154428));
#164977=CARTESIAN_POINT('Ctrl Pts',(-18.5181198390236,-21.0579698964561,
11.6959175630112));
#164978=CARTESIAN_POINT('Ctrl Pts',(-18.5132015741813,-21.057459927182,
11.6956204399158));
#164979=CARTESIAN_POINT('Ctrl Pts',(-18.4968934055338,-21.0557111791746,
11.6946379704072));
#164980=CARTESIAN_POINT('Ctrl Pts',(-18.4855115455229,-21.0543971469823,
11.6939567218025));
#164981=CARTESIAN_POINT('Ctrl Pts',(-18.3830528668735,-21.0417246268513,
11.6878597145945));
#164982=CARTESIAN_POINT('Ctrl Pts',(-18.292782373007,-21.0245453062832,
11.6827394478474));
#164983=CARTESIAN_POINT('Ctrl Pts',(-18.0905383908386,-20.9722369445543,
11.6712834801344));
#164984=CARTESIAN_POINT('Ctrl Pts',(-17.9798030325778,-20.9335618779371,
11.6650138234529));
#164985=CARTESIAN_POINT('Ctrl Pts',(-17.7841420945091,-20.8464352044565,
11.6531957025434));
#164986=CARTESIAN_POINT('Ctrl Pts',(-17.6982834873898,-20.8008922787253,
11.647723227365));
#164987=CARTESIAN_POINT('Ctrl Pts',(-17.6040552742434,-20.7422813026597,
11.6412189246558));
#164988=CARTESIAN_POINT('Ctrl Pts',(-17.5923245977831,-20.734823459614,
11.6404000339324));
#164989=CARTESIAN_POINT('Ctrl Pts',(-17.57367366098,-20.7227064591146,11.6390829124332));
#164990=CARTESIAN_POINT('Ctrl Pts',(-17.5667058970322,-20.7181209051227,
11.6385874226187));
#164991=CARTESIAN_POINT('Ctrl Pts',(-17.554407978302,-20.7099229562399,
11.6377067127351));
#164992=CARTESIAN_POINT('Ctrl Pts',(-17.5490668339413,-20.7063271782335,
11.637322121584));
#164993=CARTESIAN_POINT('Ctrl Pts',(-17.5379977207763,-20.6988015916346,
11.6365206923166));
#164994=CARTESIAN_POINT('Ctrl Pts',(-17.5322725312649,-20.6948678497073,
11.6361037078559));
#164995=CARTESIAN_POINT('Ctrl Pts',(-17.5175084250336,-20.6846161910314,
11.6350219256616));
#164996=CARTESIAN_POINT('Ctrl Pts',(-17.5084994158515,-20.6782557540619,
11.6343555073403));
#164997=CARTESIAN_POINT('Ctrl Pts',(-17.470078750806,-20.6506780988765,
11.6314858721419));
#164998=CARTESIAN_POINT('Ctrl Pts',(-17.4411666651739,-20.6287784352367,
11.6292563809623));
#164999=CARTESIAN_POINT('Ctrl Pts',(-17.366328946895,-20.5690055797999,
11.6232932602904));
#165000=CARTESIAN_POINT('Ctrl Pts',(-17.3214159490521,-20.529921555662,
11.6195138303613));
#165001=CARTESIAN_POINT('Ctrl Pts',(-17.1558768544209,-20.3731292376476,
11.6048076785868));
#165002=CARTESIAN_POINT('Ctrl Pts',(-17.0478256862569,-20.2430808675952,
11.5934626031465));
#165003=CARTESIAN_POINT('Ctrl Pts',(-16.9272027772928,-20.0565592035218,
11.5791037003395));
#165004=CARTESIAN_POINT('Ctrl Pts',(-16.8997895125758,-20.0104139918105,
11.57569255942));
#165005=CARTESIAN_POINT('Ctrl Pts',(-16.8699806882701,-19.9555922688549,
11.571842977358));
#165006=CARTESIAN_POINT('Ctrl Pts',(-16.8658518619861,-19.9478855240929,
11.5713063541948));
#165007=CARTESIAN_POINT('Ctrl Pts',(-16.8596759196141,-19.9361841212052,
11.5704986914318));
#165008=CARTESIAN_POINT('Ctrl Pts',(-16.8575936268885,-19.9322082771287,
11.570225501732));
#165009=CARTESIAN_POINT('Ctrl Pts',(-16.8538803728326,-19.9250631486774,
11.5697367944129));
#165010=CARTESIAN_POINT('Ctrl Pts',(-16.8522447644358,-19.9218963541476,
11.5695209869676));
#165011=CARTESIAN_POINT('Ctrl Pts',(-16.8487101505957,-19.9150101883395,
11.5690534392953));
#165012=CARTESIAN_POINT('Ctrl Pts',(-16.8468141561918,-19.9112893362976,
11.5688018887232));
#165013=CARTESIAN_POINT('Ctrl Pts',(-16.8415244148065,-19.9008319435131,
11.5680978763587));
#165014=CARTESIAN_POINT('Ctrl Pts',(-16.8381556045682,-19.8940827616384,
11.5676469515149));
#165015=CARTESIAN_POINT('Ctrl Pts',(-16.8183324160605,-19.8538313792483,
11.5649772640497));
#165016=CARTESIAN_POINT('Ctrl Pts',(-16.8027292152315,-19.8199145519605,
11.5628080718355));
#165017=CARTESIAN_POINT('Ctrl Pts',(-16.7545367183236,-19.707413250753,
11.5558167842105));
#165018=CARTESIAN_POINT('Ctrl Pts',(-16.725783323603,-19.6272718910687,
11.551153630289));
#165019=CARTESIAN_POINT('Ctrl Pts',(-16.6519385130739,-19.3744840995508,
11.5368176931546));
#165020=CARTESIAN_POINT('Ctrl Pts',(-16.6237691651234,-19.1977480782823,
11.5272467262133));
#165021=CARTESIAN_POINT('Ctrl Pts',(-16.6173518026154,-18.996812513012,
11.5155621957774));
#165022=CARTESIAN_POINT('Ctrl Pts',(-16.616992205476,-18.9740384092867,
11.5142276513877));
#165023=CARTESIAN_POINT('Ctrl Pts',(-16.6170034365873,-18.9417527538923,
11.5123195573282));
#165024=CARTESIAN_POINT('Ctrl Pts',(-16.6170708372447,-18.9322421928686,
11.5117554928235));
#165025=CARTESIAN_POINT('Ctrl Pts',(-16.6172847240138,-18.9167726308347,
11.5108346546508));
#165026=CARTESIAN_POINT('Ctrl Pts',(-16.6173922965961,-18.9108131586095,
11.5104791035797));
#165027=CARTESIAN_POINT('Ctrl Pts',(-16.6176704649905,-18.898325571687,
11.5097323471504));
#165028=CARTESIAN_POINT('Ctrl Pts',(-16.6178461020897,-18.8917976422054,
11.5093409875668));
#165029=CARTESIAN_POINT('Ctrl Pts',(-16.6183366062704,-18.8762440375105,
11.5084061197012));
#165030=CARTESIAN_POINT('Ctrl Pts',(-16.6186790291309,-18.8672194145403,
11.5078617531892));
#165031=CARTESIAN_POINT('Ctrl Pts',(-16.6200326343453,-18.8367003582321,
11.5060141579507));
#165032=CARTESIAN_POINT('Ctrl Pts',(-16.6213137594955,-18.8152197895042,
11.5047025106788));
#165033=CARTESIAN_POINT('Ctrl Pts',(-16.6363972790706,-18.6139868128247,
11.4923054145702));
#165034=CARTESIAN_POINT('Ctrl Pts',(-16.6727791395181,-18.4367010598517,
11.4804684396029));
#165035=CARTESIAN_POINT('Ctrl Pts',(-16.7699001797035,-18.1530603222483,
11.4606622851455));
#165036=CARTESIAN_POINT('Ctrl Pts',(-16.8181667966911,-18.0433843038417,
11.4527932201824));
#165037=CARTESIAN_POINT('Ctrl Pts',(-16.88000589595,-17.9299992120614,11.4448159967796));
#165038=CARTESIAN_POINT('Ctrl Pts',(-16.8846236158346,-17.9216666821436,
11.4442308027965));
#165039=CARTESIAN_POINT('Ctrl Pts',(-16.8915477729611,-17.9093687958875,
11.4433689938721));
#165040=CARTESIAN_POINT('Ctrl Pts',(-16.8938110301694,-17.9053794417563,
11.4430897227625));
#165041=CARTESIAN_POINT('Ctrl Pts',(-16.8978601059011,-17.8982960325788,
11.4425944228796));
#165042=CARTESIAN_POINT('Ctrl Pts',(-16.8996408051028,-17.8951991169496,
11.4423780704635));
#165043=CARTESIAN_POINT('Ctrl Pts',(-16.9034851807604,-17.8885521369334,
11.4419141391035));
#165044=CARTESIAN_POINT('Ctrl Pts',(-16.9055513430801,-17.8850035751779,
11.4416667242589));
#165045=CARTESIAN_POINT('Ctrl Pts',(-16.9112808458405,-17.8752288687222,
11.4409858614255));
#165046=CARTESIAN_POINT('Ctrl Pts',(-16.9149657894449,-17.8690153609838,
11.4405537916633));
#165047=CARTESIAN_POINT('Ctrl Pts',(-16.9352893954879,-17.8351423353129,
11.4382017068095));
#165048=CARTESIAN_POINT('Ctrl Pts',(-16.9525281500796,-17.8078456458654,
11.436318527035));
#165049=CARTESIAN_POINT('Ctrl Pts',(-17.060495493342,-17.6452452935144,
11.4251087104377));
#165050=CARTESIAN_POINT('Ctrl Pts',(-17.1659769765886,-17.5203782157972,
11.4164988834854));
#165051=CARTESIAN_POINT('Ctrl Pts',(-17.3700049986271,-17.3287666348621,
11.4011763020977));
#165052=CARTESIAN_POINT('Ctrl Pts',(-17.4617397747621,-17.2559110975352,
11.3946470605129));
#165053=CARTESIAN_POINT('Ctrl Pts',(-17.570876237423,-17.1830920053328,
11.386960646138));
#165054=CARTESIAN_POINT('Ctrl Pts',(-17.5828186112244,-17.1752969364621,
11.386120807448));
#165055=CARTESIAN_POINT('Ctrl Pts',(-17.6019578968922,-17.1630782526814,
11.3847763998458));
#165056=CARTESIAN_POINT('Ctrl Pts',(-17.6091042323647,-17.1585759424942,
11.3842747571289));
#165057=CARTESIAN_POINT('Ctrl Pts',(-17.6217596106978,-17.1507082442188,
11.3833869128543));
#165058=CARTESIAN_POINT('Ctrl Pts',(-17.6272574932249,-17.1473250444158,
11.383001374589));
#165059=CARTESIAN_POINT('Ctrl Pts',(-17.6386650397899,-17.1403769827243,
11.3822017283011));
#165060=CARTESIAN_POINT('Ctrl Pts',(-17.6445768277832,-17.1368157719217,
11.3817874924848));
#165061=CARTESIAN_POINT('Ctrl Pts',(-17.6598051375919,-17.1277435581502,
11.3807208291417));
#165062=CARTESIAN_POINT('Ctrl Pts',(-17.6691466195901,-17.1222750372067,
11.3800668657194));
#165063=CARTESIAN_POINT('Ctrl Pts',(-17.708386380808,-17.099706280852,11.3773210252668));
#165064=CARTESIAN_POINT('Ctrl Pts',(-17.7386564142118,-17.0832661384781,
11.3752056077944));
#165065=CARTESIAN_POINT('Ctrl Pts',(-17.81863541282,-17.042322815823,11.3696200971174));
#165066=CARTESIAN_POINT('Ctrl Pts',(-17.8689267494071,-17.0190212850063,
11.3661110815783));
#165067=CARTESIAN_POINT('Ctrl Pts',(-18.0212914076408,-16.955563607542,
11.3554994428696));
#165068=CARTESIAN_POINT('Ctrl Pts',(-18.1256274505189,-16.9213372537294,
11.3482485731389));
#165069=CARTESIAN_POINT('Ctrl Pts',(-18.29350956687,-16.880370614754,11.3368339890718));
#165070=CARTESIAN_POINT('Ctrl Pts',(-18.3555262760965,-16.8681481787254,
11.332672471414));
#165071=CARTESIAN_POINT('Ctrl Pts',(-18.4213590370903,-16.8582100926892,
11.3283638131055));
#165072=CARTESIAN_POINT('Ctrl Pts',(-18.4247203799251,-16.8577109405697,
11.3281441181102));
#165073=CARTESIAN_POINT('Ctrl Pts',(-18.4797755059873,-16.849670811192,
11.3245508054879));
#165074=CARTESIAN_POINT('Ctrl Pts',(-18.5317346620249,-16.8440370436972,
11.3212320853524));
#165075=CARTESIAN_POINT('Ctrl Pts',(-18.5925033426384,-16.839716189436,
11.3174742935894));
#165076=CARTESIAN_POINT('Ctrl Pts',(-18.6011571902866,-16.8391542900071,
11.3169420802446));
#165077=CARTESIAN_POINT('Ctrl Pts',(-18.6142794835943,-16.8383831937566,
11.316139730426));
#165078=CARTESIAN_POINT('Ctrl Pts',(-18.618745420425,-16.8381349644739,
11.31586748503));
#165079=CARTESIAN_POINT('Ctrl Pts',(-18.6267705205871,-16.8377144148757,
11.3153797853612));
#165080=CARTESIAN_POINT('Ctrl Pts',(-18.6303293450097,-16.8375369256974,
11.3151640465357));
#165081=CARTESIAN_POINT('Ctrl Pts',(-18.6380718132848,-16.8371703802019,
11.3146958642062));
#165082=CARTESIAN_POINT('Ctrl Pts',(-18.6422555616313,-16.8369847526536,
11.3144436146022));
#165083=CARTESIAN_POINT('Ctrl Pts',(-18.6540307580913,-16.8364973078251,
11.3137356668708));
#165084=CARTESIAN_POINT('Ctrl Pts',(-18.6616234083277,-16.8362239359533,
11.3132815334538));
#165085=CARTESIAN_POINT('Ctrl Pts',(-18.707474970354,-16.8348201708283,
11.3105523638864));
#165086=CARTESIAN_POINT('Ctrl Pts',(-18.7457599095072,-16.834686578804,
11.308329506119));
#165087=CARTESIAN_POINT('Ctrl Pts',(-18.8728173637419,-16.8376901034067,
11.3010765949882));
#165088=CARTESIAN_POINT('Ctrl Pts',(-18.9613920415912,-16.8453742712031,
11.2962193926562));
#165089=CARTESIAN_POINT('Ctrl Pts',(-19.2202180231406,-16.884348779317,
11.2819832346259));
#165090=CARTESIAN_POINT('Ctrl Pts',(-19.3873884125689,-16.9309442580225,
11.272674686867));
#165091=CARTESIAN_POINT('Ctrl Pts',(-19.5684222982214,-17.0062442706738,
11.2612834044764));
#165092=CARTESIAN_POINT('Ctrl Pts',(-19.5896688836689,-17.0154937053638,
11.2599260374505));
#165093=CARTESIAN_POINT('Ctrl Pts',(-19.6194748279846,-17.0290556360585,
11.2579909361443));
#165094=CARTESIAN_POINT('Ctrl Pts',(-19.6281637658312,-17.0330805506472,
11.2574230619284));
#165095=CARTESIAN_POINT('Ctrl Pts',(-19.6422269228757,-17.0397111817477,
11.2564977074545));
#165096=CARTESIAN_POINT('Ctrl Pts',(-19.647618009958,-17.0422809634389,
11.2561414742079));
#165097=CARTESIAN_POINT('Ctrl Pts',(-19.6587540335295,-17.0476471437192,
11.2554024813631));
#165098=CARTESIAN_POINT('Ctrl Pts',(-19.6644973223784,-17.050446804475,
11.2550196109674));
#165099=CARTESIAN_POINT('Ctrl Pts',(-19.67800895145,-17.0571091412742,11.2541147126182));
#165100=CARTESIAN_POINT('Ctrl Pts',(-19.6857663512819,-17.0609936340756,
11.2535919252617));
#165101=CARTESIAN_POINT('Ctrl Pts',(-19.7021571666019,-17.069327688443,
11.2524802998627));
#165102=CARTESIAN_POINT('Ctrl Pts',(-19.7107842552369,-17.0737891902844,
11.2518910496806));
#165103=CARTESIAN_POINT('Ctrl Pts',(-19.7340897893561,-17.0860456524255,
11.2502877835504));
#165104=CARTESIAN_POINT('Ctrl Pts',(-19.7487074053523,-17.093954233381,
11.249269778892));
#165105=CARTESIAN_POINT('Ctrl Pts',(-19.7941068259137,-17.1192122365549,
11.2460685218741));
#165106=CARTESIAN_POINT('Ctrl Pts',(-19.8245471448638,-17.1371600171479,
11.2438644214309));
#165107=CARTESIAN_POINT('Ctrl Pts',(-19.9427199517914,-17.2108821895701,
11.2350763602771));
#165108=CARTESIAN_POINT('Ctrl Pts',(-20.0267351210617,-17.2723194690709,
11.2283027994222));
#165109=CARTESIAN_POINT('Ctrl Pts',(-20.2181072730451,-17.435153238626,
11.2117354014159));
#165110=CARTESIAN_POINT('Ctrl Pts',(-20.3200567163725,-17.5420961393826,
11.2018925055787));
#165111=CARTESIAN_POINT('Ctrl Pts',(-20.4195625264171,-17.6710593147378,
11.191733433425));
#165112=CARTESIAN_POINT('Ctrl Pts',(-20.4289121067432,-17.6834563262121,
11.190772937982));
#165113=CARTESIAN_POINT('Ctrl Pts',(-20.4415454570355,-17.7005964870405,
11.1894681003514));
#165114=CARTESIAN_POINT('Ctrl Pts',(-20.4449472322576,-17.70525150479,11.1891160338837));
#165115=CARTESIAN_POINT('Ctrl Pts',(-20.4503284718,-17.7126787425664,11.1885580386074));
#165116=CARTESIAN_POINT('Ctrl Pts',(-20.4523203065535,-17.7154419032232,
11.1883512650601));
#165117=CARTESIAN_POINT('Ctrl Pts',(-20.4564251791198,-17.7211654332352,
11.1879246694373));
#165118=CARTESIAN_POINT('Ctrl Pts',(-20.458537258717,-17.7241264430484,
11.1877049184263));
#165119=CARTESIAN_POINT('Ctrl Pts',(-20.4635596999673,-17.7312061281343,
11.1871817153378));
#165120=CARTESIAN_POINT('Ctrl Pts',(-20.4664630181722,-17.7353298206995,
11.1868787460013));
#165121=CARTESIAN_POINT('Ctrl Pts',(-20.4762414008545,-17.749324399551,
11.1858564246949));
#165122=CARTESIAN_POINT('Ctrl Pts',(-20.483047206855,-17.7592437038189,
11.1851416406802));
#165123=CARTESIAN_POINT('Ctrl Pts',(-20.499217713228,-17.7832478970739,
11.1834340304655));
#165124=CARTESIAN_POINT('Ctrl Pts',(-20.5084990254507,-17.7973882476143,
11.1824461894464));
#165125=CARTESIAN_POINT('Ctrl Pts',(-20.5428019498615,-17.8510405840154,
11.1787595408908));
#165126=CARTESIAN_POINT('Ctrl Pts',(-20.5666828365081,-17.8912689725686,
11.1761190721565));
#165127=CARTESIAN_POINT('Ctrl Pts',(-20.6411145223748,-18.0266822471018,
11.1675225730271));
#165128=CARTESIAN_POINT('Ctrl Pts',(-20.6856867898319,-18.12484947811,11.1617431696283));
#165129=CARTESIAN_POINT('Ctrl Pts',(-20.7225806572512,-18.2258898364528,
11.1558809418218));
#165130=CARTESIAN_POINT('',(-20.8510159085425,-18.9509245719999,11.689056243827));
#165131=CARTESIAN_POINT('Ctrl Pts',(-20.8509997268492,-18.9509245835809,
11.6890562436241));
#165132=CARTESIAN_POINT('Ctrl Pts',(-20.851036160924,-19.0226464998528,
11.6847206650332));
#165133=CARTESIAN_POINT('Ctrl Pts',(-20.8474235543286,-19.094516438247,
11.6803850864424));
#165134=CARTESIAN_POINT('Ctrl Pts',(-20.8401430852434,-19.1661268420388,
11.6760495078516));
#165135=CARTESIAN_POINT('Ctrl Pts',(-20.8328737172097,-19.2376280563309,
11.6717205400272));
#165136=CARTESIAN_POINT('Ctrl Pts',(-20.8219476405722,-19.3088700336357,
11.6673915722028));
#165137=CARTESIAN_POINT('Ctrl Pts',(-20.8073980430312,-19.3794453826564,
11.6630626043785));
#165138=CARTESIAN_POINT('Ctrl Pts',(-20.7928607647321,-19.4499609750556,
11.6587373019202));
#165139=CARTESIAN_POINT('Ctrl Pts',(-20.7747061465264,-19.519810575807,
11.6544119994619));
#165140=CARTESIAN_POINT('Ctrl Pts',(-20.7530189912495,-19.5885935225668,
11.6500866970037));
#165141=CARTESIAN_POINT('Ctrl Pts',(-20.7313426461036,-19.6573421839323,
11.645763550526));
#165142=CARTESIAN_POINT('Ctrl Pts',(-20.7061374043849,-19.7250247747427,
11.6414404040484));
#165143=CARTESIAN_POINT('Ctrl Pts',(-20.6775383611409,-19.7912542158213,
11.6371172575707));
#165144=CARTESIAN_POINT('Ctrl Pts',(-20.6489436148248,-19.8574737061077,
11.632794760634));
#165145=CARTESIAN_POINT('Ctrl Pts',(-20.6169562761289,-19.9222400264192,
11.6284722636973));
#165146=CARTESIAN_POINT('Ctrl Pts',(-20.5817594783951,-19.9851862900761,
11.6241497667606));
#165147=CARTESIAN_POINT('Ctrl Pts',(-20.546531034035,-20.0481891508387,
11.6198233833213));
#165148=CARTESIAN_POINT('Ctrl Pts',(-20.5080876068702,-20.1093682524657,
11.615496999882));
#165149=CARTESIAN_POINT('Ctrl Pts',(-20.466657721841,-20.1683824312052,
11.6111706164427));
#165150=CARTESIAN_POINT('Ctrl Pts',(-20.4252103606757,-20.2274215035649,
11.6068424080293));
#165151=CARTESIAN_POINT('Ctrl Pts',(-20.3807743381557,-20.2842934442376,
11.6025141996159));
#165152=CARTESIAN_POINT('Ctrl Pts',(-20.3336191165972,-20.3386894684164,
11.5981859912025));
#165153=CARTESIAN_POINT('Ctrl Pts',(-20.2863774057491,-20.3931852625322,
11.5938498442479));
#165154=CARTESIAN_POINT('Ctrl Pts',(-20.2364068762127,-20.4451957108582,
11.5895136972933));
#165155=CARTESIAN_POINT('Ctrl Pts',(-20.1840141561295,-20.4944486853779,
11.5851775503387));
#165156=CARTESIAN_POINT('Ctrl Pts',(-20.1349615139615,-20.5405617432795,
11.5811178362293));
#165157=CARTESIAN_POINT('Ctrl Pts',(-20.0837862726385,-20.5842578770899,
11.5770581221199));
#165158=CARTESIAN_POINT('Ctrl Pts',(-20.0307638001156,-20.6253477363387,
11.5729984080105));
#165159=CARTESIAN_POINT('Ctrl Pts',(-19.973450974337,-20.6697624124625,
11.5686101990796));
#165160=CARTESIAN_POINT('Ctrl Pts',(-19.9137418045024,-20.7113158984434,
11.5642219901487));
#165161=CARTESIAN_POINT('Ctrl Pts',(-19.8519537768689,-20.7497397900654,
11.5598337812178));
#165162=CARTESIAN_POINT('Ctrl Pts',(-19.790257452913,-20.7881066542616,
11.5554520851166));
#165163=CARTESIAN_POINT('Ctrl Pts',(-19.7264888022836,-20.8233528921037,
11.5510703890153));
#165164=CARTESIAN_POINT('Ctrl Pts',(-19.6609970987604,-20.8552512653062,
11.5466886929141));
#165165=CARTESIAN_POINT('Ctrl Pts',(-19.5955823532009,-20.8871121553817,
11.5423121456544));
#165166=CARTESIAN_POINT('Ctrl Pts',(-19.528449008396,-20.9156327855722,
11.5379355983948));
#165167=CARTESIAN_POINT('Ctrl Pts',(-19.4599724698901,-20.9406309292982,
11.5335590511351));
#165168=CARTESIAN_POINT('Ctrl Pts',(-19.3915393582098,-20.9656132195649,
11.5291852794182));
#165169=CARTESIAN_POINT('Ctrl Pts',(-19.3217651949901,-20.9870772907211,
11.5248115077012));
#165170=CARTESIAN_POINT('Ctrl Pts',(-19.2510456730815,-21.004888884462,
11.5204377359842));
#165171=CARTESIAN_POINT('Ctrl Pts',(-19.1803476713609,-21.0226950580751,
11.5160652952207));
#165172=CARTESIAN_POINT('Ctrl Pts',(-19.1087053495646,-21.0368508431231,
11.5116928544571));
#165173=CARTESIAN_POINT('Ctrl Pts',(-19.0365282611618,-21.0472722141045,
11.5073204136936));
#165174=CARTESIAN_POINT('Ctrl Pts',(-18.9643493271831,-21.0576938515615,
11.5029478611263));
#165175=CARTESIAN_POINT('Ctrl Pts',(-18.8916360771617,-21.0643808184121,
11.4985753085589));
#165176=CARTESIAN_POINT('Ctrl Pts',(-18.8188052520574,-21.0673007042082,
11.4942027559916));
#165177=CARTESIAN_POINT('Ctrl Pts',(-18.7458988403754,-21.0702236203718,
11.4898256654243));
#165178=CARTESIAN_POINT('Ctrl Pts',(-18.6728750930033,-21.0693716302984,
11.4854485748569));
#165179=CARTESIAN_POINT('Ctrl Pts',(-18.6001519939632,-21.0647644713219,
11.4810714842896));
#165180=CARTESIAN_POINT('Ctrl Pts',(-18.5273891781395,-21.0601547962048,
11.4766920032307));
#165181=CARTESIAN_POINT('Ctrl Pts',(-18.4549278170834,-21.0517859243705,
11.4723125221717));
#165182=CARTESIAN_POINT('Ctrl Pts',(-18.3831792948548,-21.0397293485606,
11.4679330411128));
#165183=CARTESIAN_POINT('Ctrl Pts',(-18.3113035988522,-21.0276514025511,
11.4635457974531));
#165184=CARTESIAN_POINT('Ctrl Pts',(-18.2401437361938,-21.0118728040954,
11.4591585537934));
#165185=CARTESIAN_POINT('Ctrl Pts',(-18.1700988737776,-20.9925157484923,
11.4547713101337));
#165186=CARTESIAN_POINT('Ctrl Pts',(-18.1224751168409,-20.9793548159235,
11.4517884071988));
#165187=CARTESIAN_POINT('Ctrl Pts',(-18.0753664841794,-20.9645407241658,
11.448805504264));
#165188=CARTESIAN_POINT('Ctrl Pts',(-18.0288930166914,-20.9481245307068,
11.4458226013291));
#165189=CARTESIAN_POINT('Ctrl Pts',(-17.9605249572759,-20.9239743359732,
11.4414343923982));
#165190=CARTESIAN_POINT('Ctrl Pts',(-17.89326561039,-20.8962604871604,11.4370461834673));
#165191=CARTESIAN_POINT('Ctrl Pts',(-17.8275125107931,-20.8651046578563,
11.4326579745364));
#165192=CARTESIAN_POINT('Ctrl Pts',(-17.7618569996981,-20.8339950689686,
11.4282762784351));
#165193=CARTESIAN_POINT('Ctrl Pts',(-17.6977037303935,-20.7994538454432,
11.4238945823339));
#165194=CARTESIAN_POINT('Ctrl Pts',(-17.6354328295885,-20.761651671481,
11.4195128862326));
#165195=CARTESIAN_POINT('Ctrl Pts',(-17.5732351020475,-20.7238939180816,
11.415136338973));
#165196=CARTESIAN_POINT('Ctrl Pts',(-17.5129157592866,-20.6828830753684,
11.4107597917133));
#165197=CARTESIAN_POINT('Ctrl Pts',(-17.4548312249219,-20.6388361642037,
11.4063832444537));
#165198=CARTESIAN_POINT('Ctrl Pts',(-17.3967835269248,-20.5948171869498,
11.4020094727367));
#165199=CARTESIAN_POINT('Ctrl Pts',(-17.3409682086662,-20.5477662523014,
11.3976357010197));
#165200=CARTESIAN_POINT('Ctrl Pts',(-17.2877123411685,-20.4979434038514,
11.3932619293027));
#165201=CARTESIAN_POINT('Ctrl Pts',(-17.2344726796102,-20.4481357166616,
11.3888894885392));
#165202=CARTESIAN_POINT('Ctrl Pts',(-17.1837912746022,-20.3955581196349,
11.3845170477756));
#165203=CARTESIAN_POINT('Ctrl Pts',(-17.1359604618188,-20.3405095010152,
11.3801446070121));
#165204=CARTESIAN_POINT('Ctrl Pts',(-17.0881284259963,-20.2854594747964,
11.3757720544447));
#165205=CARTESIAN_POINT('Ctrl Pts',(-17.0431474419896,-20.2279386669774,
11.3713995018774));
#165206=CARTESIAN_POINT('Ctrl Pts',(-17.0012703358339,-20.1682799475938,
11.36702694931));
#165207=CARTESIAN_POINT('Ctrl Pts',(-16.9593497680378,-20.1085593121409,
11.3626498587427));
#165208=CARTESIAN_POINT('Ctrl Pts',(-16.9205397874116,-20.046696730792,
11.3582727681754));
#165209=CARTESIAN_POINT('Ctrl Pts',(-16.8850500448044,-19.9830543454068,
11.353895677608));
#165210=CARTESIAN_POINT('Ctrl Pts',(-16.8495409199316,-19.9193772025528,
11.3495161965491));
#165211=CARTESIAN_POINT('Ctrl Pts',(-16.8173558563403,-19.8539187535678,
11.3451367154901));
#165212=CARTESIAN_POINT('Ctrl Pts',(-16.788657414338,-19.7870636050085,
11.3407572344312));
#165213=CARTESIAN_POINT('Ctrl Pts',(-16.7599081045398,-19.7200899561471,
11.3363699907715));
#165214=CARTESIAN_POINT('Ctrl Pts',(-16.7346579248203,-19.6517151168644,
11.3319827471118));
#165215=CARTESIAN_POINT('Ctrl Pts',(-16.7130201897421,-19.5823408653497,
11.327595503452));
#165216=CARTESIAN_POINT('Ctrl Pts',(-16.6983086148961,-19.5351730592069,
11.3246126005172));
#165217=CARTESIAN_POINT('Ctrl Pts',(-16.6852659123099,-19.487543567345,
11.3216296975824));
#165218=CARTESIAN_POINT('Ctrl Pts',(-16.673914126578,-19.4395809616125,
11.3186467946476));
#165219=CARTESIAN_POINT('Ctrl Pts',(-16.657214284639,-19.3690222007594,
11.3142585857167));
#165220=CARTESIAN_POINT('Ctrl Pts',(-16.6441110368839,-19.2974667533233,
11.3098703767858));
#165221=CARTESIAN_POINT('Ctrl Pts',(-16.6347172531062,-19.2253147427308,
11.3054821678549));
#165222=CARTESIAN_POINT('Ctrl Pts',(-16.6253374112611,-19.1532698176848,
11.3011004717537));
#165223=CARTESIAN_POINT('Ctrl Pts',(-16.6196561660671,-19.0806305615062,
11.2967187756524));
#165224=CARTESIAN_POINT('Ctrl Pts',(-16.6177357545009,-19.0078089887219,
11.2923370795511));
#165225=CARTESIAN_POINT('Ctrl Pts',(-16.6158175995711,-18.9350729870811,
11.2879605322915));
#165226=CARTESIAN_POINT('Ctrl Pts',(-16.6176515119966,-18.8621555742337,
11.2835839850319));
#165227=CARTESIAN_POINT('Ctrl Pts',(-16.6232479369201,-18.7894739153122,
11.2792074377722));
#165228=CARTESIAN_POINT('Ctrl Pts',(-16.6288408126722,-18.7168383500425,
11.2748336660552));
#165229=CARTESIAN_POINT('Ctrl Pts',(-16.6381914295876,-18.644438721819,
11.2704598943383));
#165230=CARTESIAN_POINT('Ctrl Pts',(-16.6512581694981,-18.5726908022763,
11.2660861226213));
#165231=CARTESIAN_POINT('Ctrl Pts',(-16.6643209331559,-18.5009647158666,
11.2617136818578));
#165232=CARTESIAN_POINT('Ctrl Pts',(-16.6810974883882,-18.4298904187035,
11.2573412410942));
#165233=CARTESIAN_POINT('Ctrl Pts',(-16.7014947532381,-18.3598755013638,
11.2529688003307));
#165234=CARTESIAN_POINT('Ctrl Pts',(-16.7218925396482,-18.2898587937348,
11.2485962477633));
#165235=CARTESIAN_POINT('Ctrl Pts',(-16.7459110826478,-18.2209019822761,
11.244223695196));
#165236=CARTESIAN_POINT('Ctrl Pts',(-16.7734073411525,-18.1533978299095,
11.2398511426286));
#165237=CARTESIAN_POINT('Ctrl Pts',(-16.8009321363114,-18.0858236191875,
11.2354740520613));
#165238=CARTESIAN_POINT('Ctrl Pts',(-16.8319416708366,-18.0197055253259,
11.231096961494));
#165239=CARTESIAN_POINT('Ctrl Pts',(-16.8662449207626,-17.9554158520311,
11.2267198709266));
#165240=CARTESIAN_POINT('Ctrl Pts',(-16.9005669049666,-17.8910910677596,
11.2223403898677));
#165241=CARTESIAN_POINT('Ctrl Pts',(-16.9381859370549,-17.8285971057583,
11.2179609088088));
#165242=CARTESIAN_POINT('Ctrl Pts',(-16.9788666145897,-17.7682788337543,
11.2135814277498));
#165243=CARTESIAN_POINT('Ctrl Pts',(-17.0196193983524,-17.7078536480181,
11.2091941840901));
#165244=CARTESIAN_POINT('Ctrl Pts',(-17.0634443742615,-17.6496122391292,
11.2048069404304));
#165245=CARTESIAN_POINT('Ctrl Pts',(-17.1100650454663,-17.5938673616161,
11.2004196967707));
#165246=CARTESIAN_POINT('Ctrl Pts',(-17.1417626095283,-17.5559662164709,
11.1974367938359));
#165247=CARTESIAN_POINT('Ctrl Pts',(-17.1747517071182,-17.5192184270681,
11.1944538909011));
#165248=CARTESIAN_POINT('Ctrl Pts',(-17.2089361619794,-17.4837121229262,
11.1914709879662));
#165249=CARTESIAN_POINT('Ctrl Pts',(-17.2592256059869,-17.4314780796657,
11.1870827790353));
#165250=CARTESIAN_POINT('Ctrl Pts',(-17.3122998738986,-17.3817287153967,
11.1826945701044));
#165251=CARTESIAN_POINT('Ctrl Pts',(-17.3678836195122,-17.3347755149755,
11.1783063611735));
#165252=CARTESIAN_POINT('Ctrl Pts',(-17.4233848696313,-17.2878920008886,
11.1739246650723));
#165253=CARTESIAN_POINT('Ctrl Pts',(-17.4813878383958,-17.2437967211,11.169542968971));
#165254=CARTESIAN_POINT('Ctrl Pts',(-17.5415797744863,-17.2027650227069,
11.1651612728697));
#165255=CARTESIAN_POINT('Ctrl Pts',(-17.6017009802615,-17.1617815398248,
11.1607847256101));
#165256=CARTESIAN_POINT('Ctrl Pts',(-17.6640056470484,-17.1238547573655,
11.1564081783505));
#165257=CARTESIAN_POINT('Ctrl Pts',(-17.7281486587459,-17.0892192616152,
11.1520316310908));
#165258=CARTESIAN_POINT('Ctrl Pts',(-17.7922509918777,-17.0546057311929,
11.1476578593739));
#165259=CARTESIAN_POINT('Ctrl Pts',(-17.858188933312,-17.0232795746617,
11.1432840876569));
#165260=CARTESIAN_POINT('Ctrl Pts',(-17.9255903577762,-16.9954308470285,
11.1389103159399));
#165261=CARTESIAN_POINT('Ctrl Pts',(-17.9929712717606,-16.9675905938567,
11.1345378751764));
#165262=CARTESIAN_POINT('Ctrl Pts',(-18.0618143390781,-16.943225852836,
11.1301654344128));
#165263=CARTESIAN_POINT('Ctrl Pts',(-18.1317264570585,-16.9224789778195,
11.1257929936492));
#165264=CARTESIAN_POINT('Ctrl Pts',(-18.2016403626994,-16.9017315723031,
11.1214204410819));
#165265=CARTESIAN_POINT('Ctrl Pts',(-18.2726229102619,-16.8846023517757,
11.1170478885146));
#165266=CARTESIAN_POINT('Ctrl Pts',(-18.3442664228592,-16.8711836364424,
11.1126753359472));
#165267=CARTESIAN_POINT('Ctrl Pts',(-18.4159842897962,-16.8577509946602,
11.1082982453799));
#165268=CARTESIAN_POINT('Ctrl Pts',(-18.4883640162148,-16.8480366356522,
11.1039211548126));
#165269=CARTESIAN_POINT('Ctrl Pts',(-18.5609891559668,-16.8420814594286,
11.0995440642452));
#165270=CARTESIAN_POINT('Ctrl Pts',(-18.633653959003,-16.8361230308623,
11.0951645831863));
#165271=CARTESIAN_POINT('Ctrl Pts',(-18.7065639597304,-16.833927887168,
11.0907851021273));
#165272=CARTESIAN_POINT('Ctrl Pts',(-18.7793017600918,-16.8354847625088,
11.0864056210684));
#165273=CARTESIAN_POINT('Ctrl Pts',(-18.8521684877161,-16.8370443974006,
11.0820183774087));
#165274=CARTESIAN_POINT('Ctrl Pts',(-18.9248619239421,-16.8423692966916,
11.077631133749));
#165275=CARTESIAN_POINT('Ctrl Pts',(-18.9969694292046,-16.851396258381,
11.0732438900892));
#165276=CARTESIAN_POINT('Ctrl Pts',(-19.0459955845204,-16.8575337224938,
11.0702609871544));
#165277=CARTESIAN_POINT('Ctrl Pts',(-19.094751032782,-16.8653814515023,
11.0672780842196));
#165278=CARTESIAN_POINT('Ctrl Pts',(-19.1431096126278,-16.8749062792316,
11.0642951812848));
#165279=CARTESIAN_POINT('Ctrl Pts',(-19.2142508990197,-16.8889184462449,
11.0599069723539));
#165280=CARTESIAN_POINT('Ctrl Pts',(-19.2848103359496,-16.9066171190662,
11.055518763423));
#165281=CARTESIAN_POINT('Ctrl Pts',(-19.3543769742702,-16.9279393759585,
11.0511305544921));
#165282=CARTESIAN_POINT('Ctrl Pts',(-19.4238403641655,-16.9492299870864,
11.0467488583909));
#165283=CARTESIAN_POINT('Ctrl Pts',(-19.4923134231175,-16.9741333660322,
11.0423671622896));
#165284=CARTESIAN_POINT('Ctrl Pts',(-19.5593953414347,-17.0025355785914,
11.0379854661883));
#165285=CARTESIAN_POINT('Ctrl Pts',(-19.6263984331591,-17.0309044162905,
11.0336089189286));
#165286=CARTESIAN_POINT('Ctrl Pts',(-19.6920131895943,-17.0627637331242,
11.029232371669));
#165287=CARTESIAN_POINT('Ctrl Pts',(-19.7558555559977,-17.0979503181747,
11.0248558244094));
#165288=CARTESIAN_POINT('Ctrl Pts',(-19.8196574345001,-17.1331145884042,
11.0204820526924));
#165289=CARTESIAN_POINT('Ctrl Pts',(-19.8816887317574,-17.1716017078621,
11.0161082809754));
#165290=CARTESIAN_POINT('Ctrl Pts',(-19.9415882172335,-17.2132016512548,
11.0117345092584));
#165291=CARTESIAN_POINT('Ctrl Pts',(-20.001469475095,-17.2547889356452,
11.0073620684949));
#165292=CARTESIAN_POINT('Ctrl Pts',(-20.0592198131165,-17.299486888407,
11.0029896277313));
#165293=CARTESIAN_POINT('Ctrl Pts',(-20.1145067552159,-17.3470420258451,
10.9986171869678));
#165294=CARTESIAN_POINT('Ctrl Pts',(-20.1697951110086,-17.3945983792735,
10.9942446344004));
#165295=CARTESIAN_POINT('Ctrl Pts',(-20.2226195814196,-17.4450117463521,
10.989872081833));
#165296=CARTESIAN_POINT('Ctrl Pts',(-20.2726818719996,-17.4979893065112,
10.9854995292657));
#165297=CARTESIAN_POINT('Ctrl Pts',(-20.3227961191128,-17.5510218487802,
10.9811224386983));
#165298=CARTESIAN_POINT('Ctrl Pts',(-20.3701421308281,-17.6066235460745,
10.976745348131));
#165299=CARTESIAN_POINT('Ctrl Pts',(-20.4144601023081,-17.6644663714874,
10.9723682575637));
#165300=CARTESIAN_POINT('Ctrl Pts',(-20.4588022774772,-17.7223407870142,
10.9679887765047));
#165301=CARTESIAN_POINT('Ctrl Pts',(-20.5001128464812,-17.7824583697207,
10.9636092954458));
#165302=CARTESIAN_POINT('Ctrl Pts',(-20.5381753524546,-17.8444620559118,
10.9592298143869));
#165303=CARTESIAN_POINT('Ctrl Pts',(-20.5763053239643,-17.9065756432203,
10.9548425707271));
#165304=CARTESIAN_POINT('Ctrl Pts',(-20.6111755046332,-17.9705815860921,
10.9504553270674));
#165305=CARTESIAN_POINT('Ctrl Pts',(-20.6426156833716,-18.0360987099104,
10.9460680834077));
#165306=CARTESIAN_POINT('Ctrl Pts',(-20.6639919753451,-18.0806440408914,
10.9430851804729));
#165307=CARTESIAN_POINT('Ctrl Pts',(-20.6837836766027,-18.1258874840305,
10.9401022775381));
#165308=CARTESIAN_POINT('Ctrl Pts',(-20.7019503858964,-18.1717050053665,
10.9371193746033));
#165309=CARTESIAN_POINT('Ctrl Pts',(-20.7090721959102,-18.1896666338036,
10.9359500011275));
#165310=CARTESIAN_POINT('Ctrl Pts',(-20.7159498696698,-18.207730262489,
10.9347806276517));
#165311=CARTESIAN_POINT('Ctrl Pts',(-20.7225805737622,-18.2258896078036,
10.9336112541758));
#165312=CARTESIAN_POINT('Ctrl Pts',(-20.7219729293147,-18.2261210096953,
11.7337477406533));
#165313=CARTESIAN_POINT('Ctrl Pts',(-20.7875397462696,-18.4003672652382,
11.7225565653328));
#165314=CARTESIAN_POINT('Ctrl Pts',(-20.8444160987049,-18.6428894722044,
11.7076594114559));
#165315=CARTESIAN_POINT('Ctrl Pts',(-20.8542040030872,-18.8895339278279,
11.692762257579));
#165316=CARTESIAN_POINT('Ctrl Pts',(-20.8538228987003,-18.9509225630713,
11.6890562790225));
#165317=CARTESIAN_POINT('Origin',(-18.734,-18.952,0.));
#165318=CARTESIAN_POINT('',(-20.7225806094135,-18.2258897054408,12.7565302021861));
#165319=CARTESIAN_POINT('',(-20.722580563326,-18.2258895792221,12.5316746529861));
#165320=CARTESIAN_POINT('',(-20.7225805737622,-18.2258896078036,0.));
#165321=CARTESIAN_POINT('',(-20.850999902,-18.9513558477209,12.7090270570735));
#165322=CARTESIAN_POINT('Ctrl Pts',(-20.7225806094134,-18.2258897054408,
12.7565302021861));
#165323=CARTESIAN_POINT('Ctrl Pts',(-20.7842551302578,-18.3947962161526,
12.7448317476997));
#165324=CARTESIAN_POINT('Ctrl Pts',(-20.8241856933643,-18.5709417764268,
12.7326638034165));
#165325=CARTESIAN_POINT('Ctrl Pts',(-20.8438467731545,-18.7761570303496,
12.7196401132585));
#165326=CARTESIAN_POINT('Ctrl Pts',(-20.8458598049362,-18.8022586722148,
12.7180061119518));
#165327=CARTESIAN_POINT('Ctrl Pts',(-20.8477953012514,-18.8353508994641,
12.7159685240739));
#165328=CARTESIAN_POINT('Ctrl Pts',(-20.8481679331215,-18.8423116144406,
12.7155418364321));
#165329=CARTESIAN_POINT('Ctrl Pts',(-20.8487046761409,-18.8533599189729,
12.7148677392846));
#165330=CARTESIAN_POINT('Ctrl Pts',(-20.848891328097,-18.8574462910722,
12.714619099899));
#165331=CARTESIAN_POINT('Ctrl Pts',(-20.8492163337029,-18.8650447524985,
12.7141580697768));
#165332=CARTESIAN_POINT('Ctrl Pts',(-20.8493577838477,-18.8685566062754,
12.7139455132782));
#165333=CARTESIAN_POINT('Ctrl Pts',(-20.849621826542,-18.8755448703287,
12.7135235698769));
#165334=CARTESIAN_POINT('Ctrl Pts',(-20.8497445963114,-18.8790212128661,
12.7133141745303));
#165335=CARTESIAN_POINT('Ctrl Pts',(-20.8500062524825,-18.8869868323075,
12.712835488951));
#165336=CARTESIAN_POINT('Ctrl Pts',(-20.8501394223501,-18.891476297842,
12.7125665130544));
#165337=CARTESIAN_POINT('Ctrl Pts',(-20.8504746949752,-18.9041387170784,
12.7118100836978));
#165338=CARTESIAN_POINT('Ctrl Pts',(-20.850643746382,-18.9123125648082,
12.7113243893412));
#165339=CARTESIAN_POINT('Ctrl Pts',(-20.8509186141009,-18.9307759480992,
12.7102327380662));
#165340=CARTESIAN_POINT('Ctrl Pts',(-20.8509967709633,-18.9410657275654,
12.7096281764806));
#165341=CARTESIAN_POINT('Ctrl Pts',(-20.850999902,-18.9513558477209,12.7090270570735));
#165342=CARTESIAN_POINT('Ctrl Pts',(-20.8509999014168,-18.9513539340914,
12.7090271688623));
#165343=CARTESIAN_POINT('Ctrl Pts',(-20.8510612391395,-19.1523426431075,
12.6972859745878));
#165344=CARTESIAN_POINT('Ctrl Pts',(-20.8225007095598,-19.3523598025333,
12.686841735807));
#165345=CARTESIAN_POINT('Ctrl Pts',(-20.7414616181698,-19.6298921790064,
12.6708792396687));
#165346=CARTESIAN_POINT('Ctrl Pts',(-20.7115396446143,-19.7127722168093,
12.6659227412855));
#165347=CARTESIAN_POINT('Ctrl Pts',(-20.6684009395749,-19.8123499657298,
12.6595977270179));
#165348=CARTESIAN_POINT('Ctrl Pts',(-20.6599812421858,-19.8310365577107,
12.6583943619046));
#165349=CARTESIAN_POINT('Ctrl Pts',(-20.6475367860491,-19.8576182423343,
12.6566576870789));
#165350=CARTESIAN_POINT('Ctrl Pts',(-20.6437315486392,-19.8656152586905,
12.6561319492906));
#165351=CARTESIAN_POINT('Ctrl Pts',(-20.6370470758175,-19.8794389817198,
12.6552173772543));
#165352=CARTESIAN_POINT('Ctrl Pts',(-20.6341909602551,-19.8852767814013,
12.6548293512496));
#165353=CARTESIAN_POINT('Ctrl Pts',(-20.6286470864462,-19.8964773158425,
12.6540813686199));
#165354=CARTESIAN_POINT('Ctrl Pts',(-20.6259633239602,-19.9018419668335,
12.6537215547101));
#165355=CARTESIAN_POINT('Ctrl Pts',(-20.6188715792426,-19.9158685537708,
12.6527766469076));
#165356=CARTESIAN_POINT('Ctrl Pts',(-20.6144267212606,-19.9245115938773,
12.6521902601561));
#165357=CARTESIAN_POINT('Ctrl Pts',(-20.59878635266,-19.9544162053493,12.6501467568832));
#165358=CARTESIAN_POINT('Ctrl Pts',(-20.5872888085937,-19.9755169305429,
12.6486789921802));
#165359=CARTESIAN_POINT('Ctrl Pts',(-20.5034337899779,-20.1233636272135,
12.6382063136606));
#165360=CARTESIAN_POINT('Ctrl Pts',(-20.4185110369099,-20.2425027481767,
12.6287338943812));
#165361=CARTESIAN_POINT('Ctrl Pts',(-20.2315227060658,-20.4546135714325,
12.6100722358669));
#165362=CARTESIAN_POINT('Ctrl Pts',(-20.1312642119496,-20.5482706947719,
12.6009551399618));
#165363=CARTESIAN_POINT('Ctrl Pts',(-20.0125804401966,-20.6393299707194,
12.5915872719988));
#165364=CARTESIAN_POINT('Ctrl Pts',(-20.0024322136796,-20.6469720081385,
12.5907968161615));
#165365=CARTESIAN_POINT('Ctrl Pts',(-19.9867977241588,-20.6585263685953,
12.5895958516412));
#165366=CARTESIAN_POINT('Ctrl Pts',(-19.9813607340329,-20.6625044829779,
12.5891812795801));
#165367=CARTESIAN_POINT('Ctrl Pts',(-19.9723708089455,-20.669016535008,
12.5885009640533));
#165368=CARTESIAN_POINT('Ctrl Pts',(-19.9688289097377,-20.6715655283782,
12.5882342412073));
#165369=CARTESIAN_POINT('Ctrl Pts',(-19.961967221705,-20.6764715359513,
12.5877200918417));
#165370=CARTESIAN_POINT('Ctrl Pts',(-19.9586484683809,-20.6788299584572,
12.5874725710454));
#165371=CARTESIAN_POINT('Ctrl Pts',(-19.9553132060688,-20.6811856617561,
12.5872249921127));
#165372=CARTESIAN_POINT('Ctrl Pts',(-19.955303512298,-20.6811925083661,
12.587224272547));
#165373=CARTESIAN_POINT('Ctrl Pts',(-19.9552840912867,-20.6812062249807,
12.587222830951));
#165374=CARTESIAN_POINT('Ctrl Pts',(-19.9552743627046,-20.6812130959319,
12.5872221088213));
#165375=CARTESIAN_POINT('Ctrl Pts',(-19.9552548707649,-20.6812268621485,
12.5872206620004));
#165376=CARTESIAN_POINT('Ctrl Pts',(-19.9552451082536,-20.6812337568153,
12.5872199373722));
#165377=CARTESIAN_POINT('Ctrl Pts',(-19.9552249152373,-20.6812480176559,
12.5872184385544));
#165378=CARTESIAN_POINT('Ctrl Pts',(-19.9552144846205,-20.681255383891,
12.587217664358));
#165379=CARTESIAN_POINT('Ctrl Pts',(-19.9551934551847,-20.6812702348628,
12.5872161035036));
#165380=CARTESIAN_POINT('Ctrl Pts',(-19.9551828565233,-20.6812777194835,
12.5872153168578));
#165381=CARTESIAN_POINT('Ctrl Pts',(-19.9551614878196,-20.6812928094571,
12.58721373087));
#165382=CARTESIAN_POINT('Ctrl Pts',(-19.9551507172095,-20.6813004152062,
12.5872129314862));
#165383=CARTESIAN_POINT('Ctrl Pts',(-19.955129000285,-20.6813157504755,
12.5872113197028));
#165384=CARTESIAN_POINT('Ctrl Pts',(-19.9551180547392,-20.6813234794478,
12.5872105073606));
#165385=CARTESIAN_POINT('Ctrl Pts',(-19.9550959841774,-20.6813390638077,
12.587208869382));
#165386=CARTESIAN_POINT('Ctrl Pts',(-19.9550848592426,-20.6813469191327,
12.5872080437521));
#165387=CARTESIAN_POINT('Ctrl Pts',(-19.9550624268276,-20.681362758354,
12.587206378971));
#165388=CARTESIAN_POINT('Ctrl Pts',(-19.9550511185571,-20.6813707428027,
12.5872055397617));
#165389=CARTESIAN_POINT('Ctrl Pts',(-19.955028315119,-20.6813868433279,
12.5872038475003));
#165390=CARTESIAN_POINT('Ctrl Pts',(-19.95501682013,-20.6813949592727,12.5872029944619));
#165391=CARTESIAN_POINT('Ctrl Pts',(-19.9549936383322,-20.6814113262486,
12.5872012741783));
#165392=CARTESIAN_POINT('Ctrl Pts',(-19.9549819524341,-20.6814195766311,
12.5872004070012));
#165393=CARTESIAN_POINT('Ctrl Pts',(-19.9549583850607,-20.681436215118,
12.5871986581629));
#165394=CARTESIAN_POINT('Ctrl Pts',(-19.954946503419,-20.6814446033338,
12.5871977764898));
#165395=CARTESIAN_POINT('Ctrl Pts',(-19.9549225406218,-20.6814615202485,
12.5871959983688));
#165396=CARTESIAN_POINT('Ctrl Pts',(-19.9549104592121,-20.6814700491206,
12.5871951019025));
#165397=CARTESIAN_POINT('Ctrl Pts',(-19.9548860920947,-20.6814872507064,
12.5871932938417));
#165398=CARTESIAN_POINT('Ctrl Pts',(-19.9548738066287,-20.681495923243,
12.5871923822657));
#165399=CARTESIAN_POINT('Ctrl Pts',(-19.954849027269,-20.6815134150535,
12.5871905436804));
#165400=CARTESIAN_POINT('Ctrl Pts',(-19.95483653264,-20.6815222348399,12.5871896166172));
#165401=CARTESIAN_POINT('Ctrl Pts',(-19.9548113297571,-20.6815400247982,
12.5871877466738));
#165402=CARTESIAN_POINT('Ctrl Pts',(-19.9547986219221,-20.6815489946674,
12.5871868038252));
#165403=CARTESIAN_POINT('Ctrl Pts',(-19.9547729872369,-20.6815670885754,
12.5871849019127));
#165404=CARTESIAN_POINT('Ctrl Pts',(-19.9547600609693,-20.6815762121955,
12.5871839428926));
#165405=CARTESIAN_POINT('Ctrl Pts',(-19.9547339853479,-20.6815946164566,
12.5871820083369));
#165406=CARTESIAN_POINT('Ctrl Pts',(-19.9547208350335,-20.681603897768,
12.5871810327307));
#165407=CARTESIAN_POINT('Ctrl Pts',(-19.951870269543,-20.6836157390526,
12.5869695566085));
#165408=CARTESIAN_POINT('Ctrl Pts',(-19.9490279715372,-20.6856112856507,
12.5867595473815));
#165409=CARTESIAN_POINT('Ctrl Pts',(-19.9424087574977,-20.6902342887562,
12.5862724356391));
#165410=CARTESIAN_POINT('Ctrl Pts',(-19.9386281822933,-20.6928564303659,
12.5859956971577));
#165411=CARTESIAN_POINT('Ctrl Pts',(-19.9269336200905,-20.7009112389434,
12.5851441000283));
#165412=CARTESIAN_POINT('Ctrl Pts',(-19.9189910813986,-20.7063025076916,
12.5845719811846));
#165413=CARTESIAN_POINT('Ctrl Pts',(-19.8165018853544,-20.774856890051,
12.5772656694361));
#165414=CARTESIAN_POINT('Ctrl Pts',(-19.7170380195521,-20.8303666186062,
12.5709986813682));
#165415=CARTESIAN_POINT('Ctrl Pts',(-19.5099096779756,-20.9249784783313,
12.5585882098859));
#165416=CARTESIAN_POINT('Ctrl Pts',(-19.4025841859592,-20.9638832721718,
12.5524608812122));
#165417=CARTESIAN_POINT('Ctrl Pts',(-19.2395015422013,-21.0085002744369,
12.5430595920196));
#165418=CARTESIAN_POINT('Ctrl Pts',(-19.1858089059056,-21.0209594619883,
12.5399525323494));
#165419=CARTESIAN_POINT('Ctrl Pts',(-19.0980009687977,-21.0377538317525,
12.5348092099037));
#165420=CARTESIAN_POINT('Ctrl Pts',(-19.0641577550619,-21.0433778740814,
12.5328123209596));
#165421=CARTESIAN_POINT('Ctrl Pts',(-19.0194920268192,-21.0496892347899,
12.5301519287645));
#165422=CARTESIAN_POINT('Ctrl Pts',(-19.0087785947121,-21.0511194678868,
12.5295119480867));
#165423=CARTESIAN_POINT('Ctrl Pts',(-18.9912106199051,-21.053327980227,
12.5284592727455));
#165424=CARTESIAN_POINT('Ctrl Pts',(-18.9843623105729,-21.0541549170291,
12.5280481191861));
#165425=CARTESIAN_POINT('Ctrl Pts',(-18.97109613001,-21.0556910696015,12.527250053999));
#165426=CARTESIAN_POINT('Ctrl Pts',(-18.9646788079533,-21.0564044234214,
12.5268632777076));
#165427=CARTESIAN_POINT('Ctrl Pts',(-18.9498509881428,-21.0579840543809,
12.5259678812714));
#165428=CARTESIAN_POINT('Ctrl Pts',(-18.9414384057287,-21.0588293217481,
12.5254586049149));
#165429=CARTESIAN_POINT('Ctrl Pts',(-18.9187935851571,-21.0609676520636,
12.524084226225));
#165430=CARTESIAN_POINT('Ctrl Pts',(-18.9045531343256,-21.0621670169011,
12.5232161953583));
#165431=CARTESIAN_POINT('Ctrl Pts',(-18.7737085188745,-21.0718539475933,
12.5152049561027));
#165432=CARTESIAN_POINT('Ctrl Pts',(-18.6566197340488,-21.0708114595135,
12.5077596230227));
#165433=CARTESIAN_POINT('Ctrl Pts',(-18.3779984381195,-21.0452017959662,
12.489483089061));
#165434=CARTESIAN_POINT('Ctrl Pts',(-18.2180333724804,-21.0116138990888,
12.478511338309));
#165435=CARTESIAN_POINT('Ctrl Pts',(-18.0328851287785,-20.9497910157762,
12.4661107371694));
#165436=CARTESIAN_POINT('Ctrl Pts',(-18.0025026881001,-20.9388676230098,
12.464087885336));
#165437=CARTESIAN_POINT('Ctrl Pts',(-17.9656398434069,-20.9246540132009,
12.461658499323));
#165438=CARTESIAN_POINT('Ctrl Pts',(-17.9589127810326,-20.922020556364,
12.4612161939852));
#165439=CARTESIAN_POINT('Ctrl Pts',(-17.9483832486745,-20.9178362549301,
12.4605256450925));
#165440=CARTESIAN_POINT('Ctrl Pts',(-17.9445716598825,-20.9163087225898,
12.4602760383103));
#165441=CARTESIAN_POINT('Ctrl Pts',(-17.9374523788119,-20.9134315305656,
12.4598105398065));
#165442=CARTESIAN_POINT('Ctrl Pts',(-17.9341436950112,-20.9120846036624,
12.459594493906));
#165443=CARTESIAN_POINT('Ctrl Pts',(-17.9265947240782,-20.9089892071009,
12.4591022275286));
#165444=CARTESIAN_POINT('Ctrl Pts',(-17.9223567076918,-20.9072353319371,
12.4588263379766));
#165445=CARTESIAN_POINT('Ctrl Pts',(-17.909334266407,-20.9017964437046,
12.4579799438881));
#165446=CARTESIAN_POINT('Ctrl Pts',(-17.9005688474748,-20.8980658431091,
12.4574121309444));
#165447=CARTESIAN_POINT('Ctrl Pts',(-17.7831681757499,-20.8471608908244,
12.4498287387907));
#165448=CARTESIAN_POINT('Ctrl Pts',(-17.6786363507224,-20.7910028952994,
12.4433207111902));
#165449=CARTESIAN_POINT('Ctrl Pts',(-17.4876881413444,-20.6667456969204,
12.4309173567455));
#165450=CARTESIAN_POINT('Ctrl Pts',(-17.400796255379,-20.6000937308301,
12.425029338071));
#165451=CARTESIAN_POINT('Ctrl Pts',(-17.2784448505951,-20.4902084161776,
12.4158851680527));
#165452=CARTESIAN_POINT('Ctrl Pts',(-17.2389006551485,-20.451801062896,
12.4127777468981));
#165453=CARTESIAN_POINT('Ctrl Pts',(-17.177243440619,-20.3870522548753,
12.4076338794243));
#165454=CARTESIAN_POINT('Ctrl Pts',(-17.1541937093006,-20.3616374876838,
12.4056368178807));
#165455=CARTESIAN_POINT('Ctrl Pts',(-17.1247079047787,-20.3274943776321,
12.4029762283239));
#165456=CARTESIAN_POINT('Ctrl Pts',(-17.1177060961681,-20.319259975468,
12.4023362273389));
#165457=CARTESIAN_POINT('Ctrl Pts',(-17.1063395962732,-20.3056831958284,
12.4012835271038));
#165458=CARTESIAN_POINT('Ctrl Pts',(-17.1019373622001,-20.3003724000048,
12.4008723691006));
#165459=CARTESIAN_POINT('Ctrl Pts',(-17.0934649359626,-20.2900491001653,
12.4000743013691));
#165460=CARTESIAN_POINT('Ctrl Pts',(-17.0893915608178,-20.2850392984183,
12.3996875270095));
#165461=CARTESIAN_POINT('Ctrl Pts',(-17.0800374552795,-20.2734266471797,
12.3987921439049));
#165462=CARTESIAN_POINT('Ctrl Pts',(-17.074773260848,-20.2668106738457,
12.3982828790098));
#165463=CARTESIAN_POINT('Ctrl Pts',(-17.0607185547714,-20.2489280678248,
12.3969085513041));
#165464=CARTESIAN_POINT('Ctrl Pts',(-17.0520023744138,-20.2376038191693,
12.3960405602985));
#165465=CARTESIAN_POINT('Ctrl Pts',(-16.973063263971,-20.1328674174481,
12.3880323656874));
#165466=CARTESIAN_POINT('Ctrl Pts',(-16.9105846302004,-20.0338939991308,
12.3805903036596));
#165467=CARTESIAN_POINT('Ctrl Pts',(-16.7813812202447,-19.7859431800545,
12.3623272407322));
#165468=CARTESIAN_POINT('Ctrl Pts',(-16.7230648940813,-19.6334113338907,
12.3513660787218));
#165469=CARTESIAN_POINT('Ctrl Pts',(-16.6747700494817,-19.44425465347,12.3389616388116));
#165470=CARTESIAN_POINT('Ctrl Pts',(-16.6674640221976,-19.4126212683758,
12.336927276411));
#165471=CARTESIAN_POINT('Ctrl Pts',(-16.6594221529178,-19.3737441414188,
12.3344860207624));
#165472=CARTESIAN_POINT('Ctrl Pts',(-16.6579926439531,-19.3666502448422,
12.3340429512458));
#165473=CARTESIAN_POINT('Ctrl Pts',(-16.6558084900638,-19.35551695315,12.3333514763866));
#165474=CARTESIAN_POINT('Ctrl Pts',(-16.6550291990208,-19.3514825312694,
12.3331017019038));
#165475=CARTESIAN_POINT('Ctrl Pts',(-16.6535944205046,-19.3439367090584,
12.3326360583764));
#165476=CARTESIAN_POINT('Ctrl Pts',(-16.6529360810056,-19.3404259574133,
12.3324200341421));
#165477=CARTESIAN_POINT('Ctrl Pts',(-16.6514534371299,-19.3324074291078,
12.3319280343614));
#165478=CARTESIAN_POINT('Ctrl Pts',(-16.6506348827829,-19.3278986404755,
12.3316523883594));
#165479=CARTESIAN_POINT('Ctrl Pts',(-16.648163490553,-19.3140295587745,
12.3308074836315));
#165480=CARTESIAN_POINT('Ctrl Pts',(-16.6465590202981,-19.3046606151112,
12.3302409027775));
#165481=CARTESIAN_POINT('Ctrl Pts',(-16.6325556183956,-19.2194451203275,
12.3251228479428));
#165482=CARTESIAN_POINT('Ctrl Pts',(-16.6242309300783,-19.1429778656906,
12.3207831191346));
#165483=CARTESIAN_POINT('Ctrl Pts',(-16.6125055597645,-18.9259703485235,
12.3087614966779));
#165484=CARTESIAN_POINT('Ctrl Pts',(-16.6189032404143,-18.785314413875,
12.3012942278611));
#165485=CARTESIAN_POINT('Ctrl Pts',(-16.6481295180311,-18.585024370231,
12.2900977769894));
#165486=CARTESIAN_POINT('Ctrl Pts',(-16.6597603175682,-18.5241499605522,
12.2866218511884));
#165487=CARTESIAN_POINT('Ctrl Pts',(-16.6826474542289,-18.4275627398131,
12.2809257168568));
#165488=CARTESIAN_POINT('Ctrl Pts',(-16.6922104990834,-18.391484977906,
12.2787569445543));
#165489=CARTESIAN_POINT('Ctrl Pts',(-16.7058599115212,-18.3449901898627,
12.2759005606723));
#165490=CARTESIAN_POINT('Ctrl Pts',(-16.7090824974773,-18.3343251430565,
12.2752411258006));
#165491=CARTESIAN_POINT('Ctrl Pts',(-16.7144581452528,-18.3170289003503,
12.2741645814064));
#165492=CARTESIAN_POINT('Ctrl Pts',(-16.7165600712629,-18.3103819417936,
12.2737491523528));
#165493=CARTESIAN_POINT('Ctrl Pts',(-16.7206638549152,-18.2976240245678,
12.2729484469735));
#165494=CARTESIAN_POINT('Ctrl Pts',(-16.7226608024148,-18.2915115586397,
12.2725633361454));
#165495=CARTESIAN_POINT('Ctrl Pts',(-16.7272947159195,-18.2775435031022,
12.2716798478149));
#165496=CARTESIAN_POINT('Ctrl Pts',(-16.7299500056479,-18.2696941444976,
12.2711808690808));
#165497=CARTESIAN_POINT('Ctrl Pts',(-16.7371217747854,-18.2488965892592,
12.2698520341522));
#165498=CARTESIAN_POINT('Ctrl Pts',(-16.7417180434729,-18.235976505735,
12.269019543779));
#165499=CARTESIAN_POINT('Ctrl Pts',(-16.7773883480091,-18.1387106159658,
12.2626984910875));
#165500=CARTESIAN_POINT('Ctrl Pts',(-16.8136765303748,-18.0563868726964,
12.2570352034524));
#165501=CARTESIAN_POINT('Ctrl Pts',(-16.9387267606208,-17.8154953874751,
12.2395150988989));
#165502=CARTESIAN_POINT('Ctrl Pts',(-17.0427411391216,-17.6658100853745,
12.2272413147993));
#165503=CARTESIAN_POINT('Ctrl Pts',(-17.1919832629446,-17.5009513709122,
12.2130076623627));
#165504=CARTESIAN_POINT('Ctrl Pts',(-17.2202717120241,-17.4714646512346,
12.2104329629849));
#165505=CARTESIAN_POINT('Ctrl Pts',(-17.2549130830892,-17.4373875924457,
12.2074417507908));
#165506=CARTESIAN_POINT('Ctrl Pts',(-17.2604581246782,-17.4319923688335,
12.2069676864878));
#165507=CARTESIAN_POINT('Ctrl Pts',(-17.2690718494115,-17.423702808949,
12.206238734394));
#165508=CARTESIAN_POINT('Ctrl Pts',(-17.2721197482174,-17.4207871079681,
12.2059822286026));
#165509=CARTESIAN_POINT('Ctrl Pts',(-17.277757044485,-17.415426494905,12.205510465449));
#165510=CARTESIAN_POINT('Ctrl Pts',(-17.2803438779467,-17.4129790250947,
12.2052950130511));
#165511=CARTESIAN_POINT('Ctrl Pts',(-17.2861664713532,-17.4074978971642,
12.204812356883));
#165512=CARTESIAN_POINT('Ctrl Pts',(-17.2894055859539,-17.4044678833482,
12.2045454330141));
#165513=CARTESIAN_POINT('Ctrl Pts',(-17.2977011590739,-17.3967565718223,
12.203865768786));
#165514=CARTESIAN_POINT('Ctrl Pts',(-17.3027710387789,-17.3920896997441,
12.20345410578));
#165515=CARTESIAN_POINT('Ctrl Pts',(-17.3322075198944,-17.3652574669085,
12.2010846896061));
#165516=CARTESIAN_POINT('Ctrl Pts',(-17.3570674655592,-17.3436371402183,
12.1991653423855));
#165517=CARTESIAN_POINT('Ctrl Pts',(-17.396620213705,-17.310828303685,12.1962180080169));
#165518=CARTESIAN_POINT('Ctrl Pts',(-17.4109707383532,-17.299237815461,
12.195169621709));
#165519=CARTESIAN_POINT('Ctrl Pts',(-17.4266368427481,-17.2869195894767,
12.1940453348911));
#165520=CARTESIAN_POINT('Ctrl Pts',(-17.4278033640929,-17.2860043376977,
12.1939617384597));
#165521=CARTESIAN_POINT('Ctrl Pts',(-17.4470154902811,-17.2709631000707,
12.1925868894683));
#165522=CARTESIAN_POINT('Ctrl Pts',(-17.4652887999205,-17.2571294649188,
12.1913074953054));
#165523=CARTESIAN_POINT('Ctrl Pts',(-17.5206421305975,-17.2166217158637,
12.187504149114));
#165524=CARTESIAN_POINT('Ctrl Pts',(-17.5583650388148,-17.1908475981306,
12.185006662383));
#165525=CARTESIAN_POINT('Ctrl Pts',(-17.689129584563,-17.1075780833495,
12.1765663795622));
#165526=CARTESIAN_POINT('Ctrl Pts',(-17.7857773494415,-17.0560782418667,
12.1706782853511));
#165527=CARTESIAN_POINT('Ctrl Pts',(-17.9364618904714,-16.990200037325,
12.1615339397195));
#165528=CARTESIAN_POINT('Ctrl Pts',(-17.9877968473332,-16.9701053662525,
12.1584264179042));
#165529=CARTESIAN_POINT('Ctrl Pts',(-18.0722657434502,-16.9407879796317,
12.1532823986603));
#165530=CARTESIAN_POINT('Ctrl Pts',(-18.1049439412612,-16.9303288359542,
12.1512852890553));
#165531=CARTESIAN_POINT('Ctrl Pts',(-18.1482320592959,-16.917624972535,
12.1486246445422));
#165532=CARTESIAN_POINT('Ctrl Pts',(-18.1586265830274,-16.9146607407668,
12.1479846379027));
#165533=CARTESIAN_POINT('Ctrl Pts',(-18.1756912096942,-16.909935388023,
12.1469319307361));
#165534=CARTESIAN_POINT('Ctrl Pts',(-18.1823481084893,-16.9081270162551,
12.1465207714955));
#165535=CARTESIAN_POINT('Ctrl Pts',(-18.1952528780968,-16.9046890247645,
12.1457227030556));
#165536=CARTESIAN_POINT('Ctrl Pts',(-18.2014996069073,-16.9030553885958,
12.1453359292337));
#165537=CARTESIAN_POINT('Ctrl Pts',(-18.2159429960573,-16.8993486845064,
12.1444405498408));
#165538=CARTESIAN_POINT('Ctrl Pts',(-18.2241447560392,-16.8972961017953,
12.1439312881368));
#165539=CARTESIAN_POINT('Ctrl Pts',(-18.2462414759635,-16.8919065979584,
12.142556974626));
#165540=CARTESIAN_POINT('Ctrl Pts',(-18.2601581055755,-16.8886611896549,
12.1416889947183));
#165541=CARTESIAN_POINT('Ctrl Pts',(-18.3881654620941,-16.8601727285179,
12.1336816449845));
#165542=CARTESIAN_POINT('Ctrl Pts',(-18.5041116239165,-16.8442793380637,
12.1262404905973));
#165543=CARTESIAN_POINT('Ctrl Pts',(-18.7832506382352,-16.8293266590199,
12.1079811353664));
#165544=CARTESIAN_POINT('Ctrl Pts',(-18.9461978858044,-16.8393855372662,
12.0970228792225));
#165545=CARTESIAN_POINT('Ctrl Pts',(-19.138386052334,-16.8737272155504,
12.0846173746019));
#165546=CARTESIAN_POINT('Ctrl Pts',(-19.1702544521889,-16.8801824000517,
12.0825798424081));
#165547=CARTESIAN_POINT('Ctrl Pts',(-19.2090240659695,-16.8889698135634,
12.0801353193325));
#165548=CARTESIAN_POINT('Ctrl Pts',(-19.2160765452415,-16.8906063885287,
12.079692040249));
#165549=CARTESIAN_POINT('Ctrl Pts',(-19.2271191030206,-16.8932286577184,
12.0790003114699));
#165550=CARTESIAN_POINT('Ctrl Pts',(-19.2311148655619,-16.8941898288071,
12.0787504910105));
#165551=CARTESIAN_POINT('Ctrl Pts',(-19.2385782161104,-16.896008126921,
12.0782848076529));
#165552=CARTESIAN_POINT('Ctrl Pts',(-19.2420463956531,-16.8968623845508,
12.0780687892881));
#165553=CARTESIAN_POINT('Ctrl Pts',(-19.2499580407104,-16.8988323768892,
12.0775768622755));
#165554=CARTESIAN_POINT('Ctrl Pts',(-19.2544000483055,-16.8999537580763,
12.0773012827949));
#165555=CARTESIAN_POINT('Ctrl Pts',(-19.2680411881867,-16.9034445952605,
12.0764567846013));
#165556=CARTESIAN_POINT('Ctrl Pts',(-19.2772281866383,-16.9058615927029,
12.0758905400213));
#165557=CARTESIAN_POINT('Ctrl Pts',(-19.3595540168945,-16.9281141682154,
12.0708363287185));
#165558=CARTESIAN_POINT('Ctrl Pts',(-19.4316033569615,-16.9518040498019,
12.0665541470102));
#165559=CARTESIAN_POINT('Ctrl Pts',(-19.5420547864612,-16.9948176796213,
12.0599933660978));
#165560=CARTESIAN_POINT('Ctrl Pts',(-19.5813978578913,-17.0115278332892,
12.0576573178351));
#165561=CARTESIAN_POINT('Ctrl Pts',(-19.7194907374371,-17.0751813713442,
12.0493788238817));
#165562=CARTESIAN_POINT('Ctrl Pts',(-19.8150774163368,-17.1285661812524,
12.0434921246998));
#165563=CARTESIAN_POINT('Ctrl Pts',(-19.9519739602529,-17.2195849877405,
12.0343510222341));
#165564=CARTESIAN_POINT('Ctrl Pts',(-19.9966274853965,-17.2518548499242,
12.0312453593004));
#165565=CARTESIAN_POINT('Ctrl Pts',(-20.0669593926149,-17.3069820037024,
12.0261041428463));
#165566=CARTESIAN_POINT('Ctrl Pts',(-20.0934296067029,-17.3287883999349,
12.0241079208864));
#165567=CARTESIAN_POINT('Ctrl Pts',(-20.1275293224879,-17.35829933128,12.0214482913757));
#165568=CARTESIAN_POINT('Ctrl Pts',(-20.1356467608099,-17.3654338509006,
12.020808389187));
#165569=CARTESIAN_POINT('Ctrl Pts',(-20.1488551365414,-17.3772233421804,
12.0197558100631));
#165570=CARTESIAN_POINT('Ctrl Pts',(-20.1539786417032,-17.3818416529578,
12.0193446736788));
#165571=CARTESIAN_POINT('Ctrl Pts',(-20.163854363553,-17.3908314659357,
12.018546618321));
#165572=CARTESIAN_POINT('Ctrl Pts',(-20.1686093357417,-17.3951998377782,
12.0181598345593));
#165573=CARTESIAN_POINT('Ctrl Pts',(-20.1795448203177,-17.4053388635151,
12.0172643865765));
#165574=CARTESIAN_POINT('Ctrl Pts',(-20.1857108612714,-17.4111249010105,
12.0167550659061));
#165575=CARTESIAN_POINT('Ctrl Pts',(-20.2022061742281,-17.4267905297658,
12.0153804900842));
#165576=CARTESIAN_POINT('Ctrl Pts',(-20.2124701887747,-17.4367379159664,
12.0145123050927));
#165577=CARTESIAN_POINT('Ctrl Pts',(-20.3058954048566,-17.5291340959966,
12.0064891405521));
#165578=CARTESIAN_POINT('Ctrl Pts',(-20.3821685976282,-17.6182327929685,
11.9990309919019));
#165579=CARTESIAN_POINT('Ctrl Pts',(-20.5463777626565,-17.8457806850625,
11.9806999008511));
#165580=CARTESIAN_POINT('Ctrl Pts',(-20.6263877623316,-17.9890342248282,
11.9696847637001));
#165581=CARTESIAN_POINT('Ctrl Pts',(-20.700887556571,-18.1684278677764,
11.9573529660037));
#165582=CARTESIAN_POINT('Ctrl Pts',(-20.7120470190104,-18.1970416219089,
11.9554289491706));
#165583=CARTESIAN_POINT('Ctrl Pts',(-20.7225805737639,-18.2258896078082,
11.9535388216361));
#165584=CARTESIAN_POINT('',(-20.8516473850063,-18.9538935158916,12.4890562790225));
#165585=CARTESIAN_POINT('Ctrl Pts',(-20.8516473850063,-18.9538935158916,
12.4890562790225));
#165586=CARTESIAN_POINT('Ctrl Pts',(-20.8529700926033,-19.0968822287437,
12.4804472042752));
#165587=CARTESIAN_POINT('Ctrl Pts',(-20.7745204165097,-19.942518370496,
12.4294461939675));
#165588=CARTESIAN_POINT('Ctrl Pts',(-19.6371491297831,-21.2866630700929,
12.336053248099));
#165589=CARTESIAN_POINT('Ctrl Pts',(-17.2597753208662,-20.9751143311526,
12.2088774414178));
#165590=CARTESIAN_POINT('Ctrl Pts',(-16.2349111543522,-18.8074837620172,
12.0817016347362));
#165591=CARTESIAN_POINT('Ctrl Pts',(-17.5028058927726,-16.7724378715414,
11.9545258280549));
#165592=CARTESIAN_POINT('Ctrl Pts',(-19.6892757572449,-16.7401229693189,
11.8385411966939));
#165593=CARTESIAN_POINT('Ctrl Pts',(-20.5391740295624,-17.7403261323705,
11.7649485008933));
#165594=CARTESIAN_POINT('Ctrl Pts',(-20.7219729293147,-18.2261210096953,
11.7337477406533));
#165595=CARTESIAN_POINT('Ctrl Pts',(-20.8509991358391,-18.9539128137851,
12.4894293403473));
#165596=CARTESIAN_POINT('Ctrl Pts',(-20.8511381828998,-18.8000230260387,
12.4977966149232));
#165597=CARTESIAN_POINT('Ctrl Pts',(-20.834498149614,-18.6465855779713,
12.5060906968582));
#165598=CARTESIAN_POINT('Ctrl Pts',(-20.7961362977383,-18.472547451059,
12.5163227455566));
#165599=CARTESIAN_POINT('Ctrl Pts',(-20.7904905713577,-18.448882400777,
12.5177311312538));
#165600=CARTESIAN_POINT('Ctrl Pts',(-20.7812755038438,-18.413006824194,
12.5198949244517));
#165601=CARTESIAN_POINT('Ctrl Pts',(-20.7780017676535,-18.4007220341299,
12.520641034919));
#165602=CARTESIAN_POINT('Ctrl Pts',(-20.7717115976596,-18.3779445800159,
12.5220344202404));
#165603=CARTESIAN_POINT('Ctrl Pts',(-20.7687242523026,-18.3674442791432,
12.5226807443555));
#165604=CARTESIAN_POINT('Ctrl Pts',(-20.7637102971677,-18.3503248196281,
12.5237411983776));
#165605=CARTESIAN_POINT('Ctrl Pts',(-20.7617321768065,-18.3436915827488,
12.5241537422371));
#165606=CARTESIAN_POINT('Ctrl Pts',(-20.7578487254815,-18.3308986332124,
12.5249526247701));
#165607=CARTESIAN_POINT('Ctrl Pts',(-20.7559477130758,-18.3247376819708,
12.525338818126));
#165608=CARTESIAN_POINT('Ctrl Pts',(-20.7515060164025,-18.3105726907948,
12.5262301456732));
#165609=CARTESIAN_POINT('Ctrl Pts',(-20.7489458046995,-18.3025749310625,
12.526735917306));
#165610=CARTESIAN_POINT('Ctrl Pts',(-20.7419616197391,-18.2811961882013,
12.5280947365095));
#165611=CARTESIAN_POINT('Ctrl Pts',(-20.7374515549886,-18.267843971008,
12.5289506103441));
#165612=CARTESIAN_POINT('Ctrl Pts',(-20.7294672453927,-18.2449622838481,
12.5304300016819));
#165613=CARTESIAN_POINT('Ctrl Pts',(-20.7260577868628,-18.2354125649028,
12.5310512601322));
#165614=CARTESIAN_POINT('Ctrl Pts',(-20.722580563326,-18.2258895792221,
12.5316746529861));
#165615=CARTESIAN_POINT('Origin',(-18.734,-18.952,0.));
#165616=CARTESIAN_POINT('',(-20.7225805759573,-18.2258896138153,13.5571445817067));
#165617=CARTESIAN_POINT('',(-20.7225805383928,-18.2258895109384,13.3344632701429));
#165618=CARTESIAN_POINT('',(-20.7225805737622,-18.2258896078036,0.));
#165619=CARTESIAN_POINT('Ctrl Pts',(-20.7225805759573,-18.2258896138153,
13.5571445817067));
#165620=CARTESIAN_POINT('Ctrl Pts',(-20.7282458896856,-18.2414050685604,
13.5562053219367));
#165621=CARTESIAN_POINT('Ctrl Pts',(-20.7337298095941,-18.2569873464273,
13.555260940775));
#165622=CARTESIAN_POINT('Ctrl Pts',(-20.7502231681677,-18.3056645889277,
13.5523055107353));
#165623=CARTESIAN_POINT('Ctrl Pts',(-20.7605967264764,-18.3389658822682,
13.5502759731478));
#165624=CARTESIAN_POINT('Ctrl Pts',(-20.7731190945415,-18.3829652423284,
13.5475782690586));
#165625=CARTESIAN_POINT('Ctrl Pts',(-20.7760149202605,-18.3934462461678,
13.5469344756048));
#165626=CARTESIAN_POINT('Ctrl Pts',(-20.7806193232447,-18.410625705192,
13.5458771253902));
#165627=CARTESIAN_POINT('Ctrl Pts',(-20.7823760851381,-18.4173111246253,
13.5454651366894));
#165628=CARTESIAN_POINT('Ctrl Pts',(-20.7857090369026,-18.4302523157076,
13.5446665855915));
#165629=CARTESIAN_POINT('Ctrl Pts',(-20.7872894372007,-18.4365069313526,
13.5442801645478));
#165630=CARTESIAN_POINT('Ctrl Pts',(-20.7908666319417,-18.4509415625605,
13.5433872364578));
#165631=CARTESIAN_POINT('Ctrl Pts',(-20.7928432511205,-18.4591264224568,
13.5428800845856));
#165632=CARTESIAN_POINT('Ctrl Pts',(-20.7980153369036,-18.4811173134203,
13.541515145064));
#165633=CARTESIAN_POINT('Ctrl Pts',(-20.8011210527526,-18.4949438180779,
13.5406544911353));
#165634=CARTESIAN_POINT('Ctrl Pts',(-20.8354181895579,-18.6551381146017,
13.5306529136224));
#165635=CARTESIAN_POINT('Ctrl Pts',(-20.8511375064961,-18.8043573065181,
13.5210013903412));
#165636=CARTESIAN_POINT('Ctrl Pts',(-20.8508605238589,-19.1037302303994,
13.5012718293646));
#165637=CARTESIAN_POINT('Ctrl Pts',(-20.8348287878723,-19.2530733054988,
13.4912566718935));
#165638=CARTESIAN_POINT('Ctrl Pts',(-20.799845502466,-19.4148371176257,
13.4809319276196));
#165639=CARTESIAN_POINT('Ctrl Pts',(-20.7963536193457,-19.4301562711893,
13.4799598356582));
#165640=CARTESIAN_POINT('Ctrl Pts',(-20.7913410447585,-19.4510695238938,
13.4786418671935));
#165641=CARTESIAN_POINT('Ctrl Pts',(-20.7899675522255,-19.4566979196881,
13.478288068359));
#165642=CARTESIAN_POINT('Ctrl Pts',(-20.787748533968,-19.4656317736744,
13.4777280102177));
#165643=CARTESIAN_POINT('Ctrl Pts',(-20.7869181050469,-19.4689408999646,
13.477520895203));
#165644=CARTESIAN_POINT('Ctrl Pts',(-20.7851867323183,-19.4757701709458,
13.4770941650689));
#165645=CARTESIAN_POINT('Ctrl Pts',(-20.7842847248748,-19.479290005506,
13.4768746186114));
#165646=CARTESIAN_POINT('Ctrl Pts',(-20.7821142206126,-19.4876700191264,
13.4763528244809));
#165647=CARTESIAN_POINT('Ctrl Pts',(-20.7808374701592,-19.4925280769787,
13.4760510525904));
#165648=CARTESIAN_POINT('Ctrl Pts',(-20.7764750802482,-19.508889938069,
13.4750369851723));
#165649=CARTESIAN_POINT('Ctrl Pts',(-20.773309589546,-19.5203724740291,
13.47432915802));
#165650=CARTESIAN_POINT('Ctrl Pts',(-20.7357651550015,-19.6522085472362,
13.4662400195074));
#165651=CARTESIAN_POINT('Ctrl Pts',(-20.6908691177103,-19.7693297597466,
13.4594084552319));
#165652=CARTESIAN_POINT('Ctrl Pts',(-20.5622083975088,-20.0324987574117,
13.4434863039871));
#165653=CARTESIAN_POINT('Ctrl Pts',(-20.4709010751107,-20.1738801990557,
13.4344328370744));
#165654=CARTESIAN_POINT('Ctrl Pts',(-20.348889543169,-20.321077046124,13.4233284249157));
#165655=CARTESIAN_POINT('Ctrl Pts',(-20.3336077474604,-20.3389012886101,
13.4219534251899));
#165656=CARTESIAN_POINT('Ctrl Pts',(-20.3116465903077,-20.3636702546708,
13.4199974279973));
#165657=CARTESIAN_POINT('Ctrl Pts',(-20.3052110899289,-20.3708295803461,
13.4194265848289));
#165658=CARTESIAN_POINT('Ctrl Pts',(-20.2946981018856,-20.3823657620718,
13.4184977063352));
#165659=CARTESIAN_POINT('Ctrl Pts',(-20.2906504534217,-20.3867697178529,
13.4181409371556));
#165660=CARTESIAN_POINT('Ctrl Pts',(-20.2821570943999,-20.395932485022,
13.4173940712192));
#165661=CARTESIAN_POINT('Ctrl Pts',(-20.2777079862541,-20.4006880485277,
13.4170038310379));
#165662=CARTESIAN_POINT('Ctrl Pts',(-20.2671051341271,-20.4119169221202,
13.4160761327725));
#165663=CARTESIAN_POINT('Ctrl Pts',(-20.2609322636243,-20.4183719276711,
13.415537850889));
#165664=CARTESIAN_POINT('Ctrl Pts',(-20.2401569124612,-20.4398234031783,
13.4137320977651));
#165665=CARTESIAN_POINT('Ctrl Pts',(-20.2253732572712,-20.4546419673749,
13.4124567171911));
#165666=CARTESIAN_POINT('Ctrl Pts',(-20.1447383594956,-20.5331050198639,
13.405548990035));
#165667=CARTESIAN_POINT('Ctrl Pts',(-20.0750375737915,-20.5926371448456,
13.3997423345331));
#165668=CARTESIAN_POINT('Ctrl Pts',(-19.926079420694,-20.7040141133195,
13.3876785909804));
#165669=CARTESIAN_POINT('Ctrl Pts',(-19.8467532240746,-20.7554370910499,
13.3814263045622));
#165670=CARTESIAN_POINT('Ctrl Pts',(-19.699414986957,-20.8375167701171,
13.370289089809));
#165671=CARTESIAN_POINT('Ctrl Pts',(-19.6327063455631,-20.8702095150086,
13.3654069591936));
#165672=CARTESIAN_POINT('Ctrl Pts',(-19.5255532159929,-20.9159036014132,
13.3579382545991));
#165673=CARTESIAN_POINT('Ctrl Pts',(-19.4862012041878,-20.9313099177001,
13.3552711407261));
#165674=CARTESIAN_POINT('Ctrl Pts',(-19.4393956539296,-20.9480364427922,
13.3522082547023));
#165675=CARTESIAN_POINT('Ctrl Pts',(-19.4323664128775,-20.9505066591476,
13.3517511352583));
#165676=CARTESIAN_POINT('Ctrl Pts',(-19.4209708582227,-20.9544438202842,
13.3510148638208));
#165677=CARTESIAN_POINT('Ctrl Pts',(-19.4166126125071,-20.9559336904233,
13.3507344058948));
#165678=CARTESIAN_POINT('Ctrl Pts',(-19.4088636489768,-20.9585544673733,
13.3502378005628));
#165679=CARTESIAN_POINT('Ctrl Pts',(-19.4054748994773,-20.9596910208718,
13.3500213229366));
#165680=CARTESIAN_POINT('Ctrl Pts',(-19.3981986907339,-20.9621109068194,
13.3495580108548));
#165681=CARTESIAN_POINT('Ctrl Pts',(-19.3943103938717,-20.9633915439031,
13.3493113358358));
#165682=CARTESIAN_POINT('Ctrl Pts',(-19.3836044856681,-20.9668832174273,
13.3486345926127));
#165683=CARTESIAN_POINT('Ctrl Pts',(-19.3767792499663,-20.9690709473955,
13.3482058752027));
#165684=CARTESIAN_POINT('Ctrl Pts',(-19.3399295312855,-20.9806765532009,
13.3459051925544));
#165685=CARTESIAN_POINT('Ctrl Pts',(-19.3097072904794,-20.9894593268456,
13.3440681888844));
#165686=CARTESIAN_POINT('Ctrl Pts',(-19.1212225761425,-21.039704830265,
13.332854818634));
#165687=CARTESIAN_POINT('Ctrl Pts',(-18.9587780067321,-21.0633834033794,
13.3242094820363));
#165688=CARTESIAN_POINT('Ctrl Pts',(-18.6781394689246,-21.0715014008406,
13.3088409863284));
#165689=CARTESIAN_POINT('Ctrl Pts',(-18.5610028730379,-21.0651666504295,
13.3023035224113));
#165690=CARTESIAN_POINT('Ctrl Pts',(-18.4308397089869,-21.047229617154,
13.2946061035415));
#165691=CARTESIAN_POINT('Ctrl Pts',(-18.416700190316,-21.0451349995879,
13.2937643733148));
#165692=CARTESIAN_POINT('Ctrl Pts',(-18.3942316634065,-21.0415736355259,
13.2924175042202));
#165693=CARTESIAN_POINT('Ctrl Pts',(-18.3858882071947,-21.0401998652864,
13.2919153085522));
#165694=CARTESIAN_POINT('Ctrl Pts',(-18.3711884698204,-21.037688971675,
13.2910268203547));
#165695=CARTESIAN_POINT('Ctrl Pts',(-18.3648287058661,-21.0365726773513,
13.2906411942171));
#165696=CARTESIAN_POINT('Ctrl Pts',(-18.3516858600685,-21.0342037549424,
13.2898416944674));
#165697=CARTESIAN_POINT('Ctrl Pts',(-18.3449036019305,-21.0329470367948,
13.289427694683));
#165698=CARTESIAN_POINT('Ctrl Pts',(-18.3275114010612,-21.029636351223,
13.2883623319934));
#165699=CARTESIAN_POINT('Ctrl Pts',(-18.3169109213849,-21.0275342644025,
13.2877094404035));
#165700=CARTESIAN_POINT('Ctrl Pts',(-18.2727439855553,-21.018423892853,
13.2849740035755));
#165701=CARTESIAN_POINT('Ctrl Pts',(-18.2393357423336,-21.010682071614,
13.2828681403017));
#165702=CARTESIAN_POINT('Ctrl Pts',(-18.1527992904461,-20.9884006606378,
13.2773138637222));
#165703=CARTESIAN_POINT('Ctrl Pts',(-18.1000270035709,-20.9725938076971,
13.2738270684348));
#165704=CARTESIAN_POINT('Ctrl Pts',(-17.9444687904138,-20.9193054686138,
13.2632580901603));
#165705=CARTESIAN_POINT('Ctrl Pts',(-17.8439125094339,-20.8758999792841,
13.2560275144735));
#165706=CARTESIAN_POINT('Ctrl Pts',(-17.7067697269938,-20.8036403685822,
13.2457875996755));
#165707=CARTESIAN_POINT('Ctrl Pts',(-17.6670698386887,-20.78105284497,13.2427768014387));
#165708=CARTESIAN_POINT('Ctrl Pts',(-17.6086456024531,-20.7452620088863,
13.2383013954012));
#165709=CARTESIAN_POINT('Ctrl Pts',(-17.5893545300633,-20.7330103742832,
13.2368161402139));
#165710=CARTESIAN_POINT('Ctrl Pts',(-17.5696671737039,-20.720055027991,
13.2352951669395));
#165711=CARTESIAN_POINT('Ctrl Pts',(-17.5690694103019,-20.7196612326977,
13.2352489809311));
#165712=CARTESIAN_POINT('Ctrl Pts',(-17.5587868246404,-20.7128797773917,
13.2344544155637));
#165713=CARTESIAN_POINT('Ctrl Pts',(-17.5491543110213,-20.7064128077944,
13.2337087918134));
#165714=CARTESIAN_POINT('Ctrl Pts',(-17.5066659675864,-20.677377915073,
13.2304157061503));
#165715=CARTESIAN_POINT('Ctrl Pts',(-17.4743958289856,-20.6539622734204,
13.2279032706524));
#165716=CARTESIAN_POINT('Ctrl Pts',(-17.437001712929,-20.6251820137652,
13.224996323079));
#165717=CARTESIAN_POINT('Ctrl Pts',(-17.4312226030626,-20.6206862094026,
13.2245471982384));
#165718=CARTESIAN_POINT('Ctrl Pts',(-17.4218767838708,-20.6133375703858,
13.2238212619225));
#165719=CARTESIAN_POINT('Ctrl Pts',(-17.4182958338883,-20.610503061577,
13.2235432022183));
#165720=CARTESIAN_POINT('Ctrl Pts',(-17.4119316343928,-20.605431881023,
13.2230492288381));
#165721=CARTESIAN_POINT('Ctrl Pts',(-17.4091448500313,-20.6031997398166,
13.2228329982393));
#165722=CARTESIAN_POINT('Ctrl Pts',(-17.4031550703202,-20.5983771566403,
13.2223684072554));
#165723=CARTESIAN_POINT('Ctrl Pts',(-17.3999539940804,-20.5957844212415,
13.2221202158317));
#165724=CARTESIAN_POINT('Ctrl Pts',(-17.3911140037175,-20.5885815746871,
13.2214350222382));
#165725=CARTESIAN_POINT('Ctrl Pts',(-17.3854912203313,-20.5839516304959,
13.2209994273968));
#165726=CARTESIAN_POINT('Ctrl Pts',(-17.3544049236562,-20.5580840084478,
13.2185917577018));
#165727=CARTESIAN_POINT('Ctrl Pts',(-17.3294176643107,-20.5362781180799,
13.2166586028926));
#165728=CARTESIAN_POINT('Ctrl Pts',(-17.1853104596759,-20.4044277265249,
13.2054514658538));
#165729=CARTESIAN_POINT('Ctrl Pts',(-17.0786307434889,-20.2815675355481,
13.1968792247434));
#165730=CARTESIAN_POINT('Ctrl Pts',(-16.921125726353,-20.0514479771962,
13.1816121712838));
#165731=CARTESIAN_POINT('Ctrl Pts',(-16.8633120122126,-19.9499079089429,
13.1750989154366));
#165732=CARTESIAN_POINT('Ctrl Pts',(-16.8081376511542,-19.831174243951,
13.1674287470711));
#165733=CARTESIAN_POINT('Ctrl Pts',(-16.802248074315,-19.8181568106517,
13.1665873678139));
#165734=CARTESIAN_POINT('Ctrl Pts',(-16.7930841113754,-19.7973437079106,
13.1652409554129));
#165735=CARTESIAN_POINT('Ctrl Pts',(-16.7897238189322,-19.7895861745453,
13.1647388623103));
#165736=CARTESIAN_POINT('Ctrl Pts',(-16.7838792514817,-19.77586877322,13.1638504935854));
#165737=CARTESIAN_POINT('Ctrl Pts',(-16.781375594216,-19.7699172438577,
13.1634648837798));
#165738=CARTESIAN_POINT('Ctrl Pts',(-16.7762533946041,-19.7575835261254,
13.1626653570131));
#165739=CARTESIAN_POINT('Ctrl Pts',(-16.7736387460745,-19.7511998128499,
13.1622513135794));
#165740=CARTESIAN_POINT('Ctrl Pts',(-16.7670070396622,-19.7347800157372,
13.1611857103279));
#165741=CARTESIAN_POINT('Ctrl Pts',(-16.7630356045105,-19.7247258271732,
13.1605326204928));
#165742=CARTESIAN_POINT('Ctrl Pts',(-16.746778326634,-19.6826276564685,
13.1577952623269));
#165743=CARTESIAN_POINT('Ctrl Pts',(-16.7351961508515,-19.6503192017796,
13.155687634972));
#165744=CARTESIAN_POINT('Ctrl Pts',(-16.7070664582551,-19.565407863023,
13.1501275958416));
#165745=CARTESIAN_POINT('Ctrl Pts',(-16.6917805320225,-19.5124173547892,
13.146636702717));
#165746=CARTESIAN_POINT('Ctrl Pts',(-16.6523815365308,-19.352657269505,
13.1360598530945));
#165747=CARTESIAN_POINT('Ctrl Pts',(-16.63445980609,-19.2445562920821,13.1288255301577));
#165748=CARTESIAN_POINT('Ctrl Pts',(-16.6206147033067,-19.0854858000645,
13.1182781000465));
#165749=CARTESIAN_POINT('Ctrl Pts',(-16.6180409145904,-19.0352663908553,
13.1149644091803));
#165750=CARTESIAN_POINT('Ctrl Pts',(-16.6170038677021,-18.9687499791338,
13.1106283038235));
#165751=CARTESIAN_POINT('Ctrl Pts',(-16.6169376580062,-18.9524954718793,
13.1095729175856));
#165752=CARTESIAN_POINT('Ctrl Pts',(-16.6174524777382,-18.8833362866789,
13.1051043759661));
#165753=CARTESIAN_POINT('Ctrl Pts',(-16.6198294737511,-18.8304593906509,
13.1017420235317));
#165754=CARTESIAN_POINT('Ctrl Pts',(-16.6249015871051,-18.7690559942071,
13.0979414686477));
#165755=CARTESIAN_POINT('Ctrl Pts',(-16.6256708945493,-18.7603935972077,
13.0974077384139));
#165756=CARTESIAN_POINT('Ctrl Pts',(-16.6269171871686,-18.7472780600256,
13.0966035606025));
#165757=CARTESIAN_POINT('Ctrl Pts',(-16.6273549489344,-18.7428214100118,
13.0963309899779));
#165758=CARTESIAN_POINT('Ctrl Pts',(-16.6281664661989,-18.7348207491394,
13.0958429437904));
#165759=CARTESIAN_POINT('Ctrl Pts',(-16.628535030248,-18.7312762794508,
13.0956271818577));
#165760=CARTESIAN_POINT('Ctrl Pts',(-16.6293557594768,-18.7235724965384,
13.0951592205105));
#165761=CARTESIAN_POINT('Ctrl Pts',(-16.6298113032941,-18.7194136013102,
13.0949072135247));
#165762=CARTESIAN_POINT('Ctrl Pts',(-16.6311266820552,-18.7077250677574,
13.0942006324703));
#165763=CARTESIAN_POINT('Ctrl Pts',(-16.6320146344134,-18.700198569024,
13.0937476134451));
#165764=CARTESIAN_POINT('Ctrl Pts',(-16.6375907064606,-18.6550207813029,
13.091039301309));
#165765=CARTESIAN_POINT('Ctrl Pts',(-16.6432502380772,-18.6174937694873,
13.0888352640505));
#165766=CARTESIAN_POINT('Ctrl Pts',(-16.6652823853798,-18.4940160236923,
13.0816749290102));
#165767=CARTESIAN_POINT('Ctrl Pts',(-16.6859735679076,-18.4089235330235,
13.0768864920537));
#165768=CARTESIAN_POINT('Ctrl Pts',(-16.7636144995826,-18.1583852342082,
13.0626164653763));
#165769=CARTESIAN_POINT('Ctrl Pts',(-16.8358276435823,-17.9984915360148,
13.053215739867));
#165770=CARTESIAN_POINT('Ctrl Pts',(-16.9388697291359,-17.8296242492804,
13.0417211504581));
#165771=CARTESIAN_POINT('Ctrl Pts',(-16.9511927996561,-17.8101513058842,
13.040371165572));
#165772=CARTESIAN_POINT('Ctrl Pts',(-16.9690714890971,-17.7828945104076,
13.0384448027332));
#165773=CARTESIAN_POINT('Ctrl Pts',(-16.9743660006824,-17.7749407498816,
13.0378781628341));
#165774=CARTESIAN_POINT('Ctrl Pts',(-16.9830548956979,-17.7620773706609,
13.0369542723203));
#165775=CARTESIAN_POINT('Ctrl Pts',(-16.9864165559753,-17.7571457297477,
13.0365982607901));
#165776=CARTESIAN_POINT('Ctrl Pts',(-16.9934959565628,-17.7468538561292,
13.0358514763955));
#165777=CARTESIAN_POINT('Ctrl Pts',(-16.9972177026315,-17.7414964670118,
13.0354605534526));
#165778=CARTESIAN_POINT('Ctrl Pts',(-17.0061287643284,-17.7287948417341,
13.034528464351));
#165779=CARTESIAN_POINT('Ctrl Pts',(-17.0113401998539,-17.721466345308,
13.0339864533244));
#165780=CARTESIAN_POINT('Ctrl Pts',(-17.0290463674991,-17.6969002584541,
13.0321551378376));
#165781=CARTESIAN_POINT('Ctrl Pts',(-17.0417540763313,-17.6798184358838,
13.0308576149445));
#165782=CARTESIAN_POINT('Ctrl Pts',(-17.1542173679943,-17.5333113050345,
13.0195137930639));
#165783=CARTESIAN_POINT('Ctrl Pts',(-17.2683722589163,-17.4156710659591,
13.0088618498842));
#165784=CARTESIAN_POINT('Ctrl Pts',(-17.4936222563106,-17.2317084714849,
12.9896460475969));
#165785=CARTESIAN_POINT('Ctrl Pts',(-17.5994478191215,-17.1601470007842,
12.9811957255661));
#165786=CARTESIAN_POINT('Ctrl Pts',(-17.7249440939048,-17.0908858119816,
12.9722520373462));
#165787=CARTESIAN_POINT('Ctrl Pts',(-17.7388963996446,-17.0833885633414,
12.9712719706824));
#165788=CARTESIAN_POINT('Ctrl Pts',(-17.7580828795255,-17.0733545938883,
12.9699449732795));
#165789=CARTESIAN_POINT('Ctrl Pts',(-17.763244904769,-17.0706820218648,
12.9695899827382));
#165790=CARTESIAN_POINT('Ctrl Pts',(-17.7714574672326,-17.0664728752481,
12.9690285051526));
#165791=CARTESIAN_POINT('Ctrl Pts',(-17.7745007832631,-17.0649223865919,
12.9688211548248));
#165792=CARTESIAN_POINT('Ctrl Pts',(-17.7807873482084,-17.0617386883837,
12.9683943275292));
#165793=CARTESIAN_POINT('Ctrl Pts',(-17.7840310478825,-17.0601064575698,
12.9681749175843));
#165794=CARTESIAN_POINT('Ctrl Pts',(-17.7917594566072,-17.0562424069358,
12.9676540732174));
#165795=CARTESIAN_POINT('Ctrl Pts',(-17.7962479525459,-17.0540181265502,
12.9673531098901));
#165796=CARTESIAN_POINT('Ctrl Pts',(-17.8113633772672,-17.0465943669352,
12.9663445888951));
#165797=CARTESIAN_POINT('Ctrl Pts',(-17.8220262065822,-17.041467933101,
12.9656414333361));
#165798=CARTESIAN_POINT('Ctrl Pts',(-17.9386649062282,-16.9865898466395,
12.9580336275535));
#165799=CARTESIAN_POINT('Ctrl Pts',(-18.0485655675198,-16.9456146416675,
12.9516101226785));
#165800=CARTESIAN_POINT('Ctrl Pts',(-18.3314767668379,-16.8661166397597,
12.935617175957));
#165801=CARTESIAN_POINT('Ctrl Pts',(-18.5069470991307,-16.8398033500741,
12.9261202882692));
#165802=CARTESIAN_POINT('Ctrl Pts',(-18.7065322400053,-16.8350543726336,
12.9145183136905));
#165803=CARTESIAN_POINT('Ctrl Pts',(-18.7294292767849,-16.8348811286629,
12.9131768029348));
#165804=CARTESIAN_POINT('Ctrl Pts',(-18.7618542938823,-16.8351617983587,
12.911260466604));
#165805=CARTESIAN_POINT('Ctrl Pts',(-18.7713838171537,-16.8353086480746,
12.9106952398952));
#165806=CARTESIAN_POINT('Ctrl Pts',(-18.7868744931945,-16.8356519998194,
12.9097730246598));
#165807=CARTESIAN_POINT('Ctrl Pts',(-18.7928364464923,-16.8358093560971,
12.9094172661618));
#165808=CARTESIAN_POINT('Ctrl Pts',(-18.8053216659356,-16.8361916856188,
12.908670499235));
#165809=CARTESIAN_POINT('Ctrl Pts',(-18.8118447067726,-16.8364216385625,
12.9082793384586));
#165810=CARTESIAN_POINT('Ctrl Pts',(-18.8273729830282,-16.8370409622449,
12.9073457331012));
#165811=CARTESIAN_POINT('Ctrl Pts',(-18.8363769452405,-16.8374576848649,
12.9068024363641));
#165812=CARTESIAN_POINT('Ctrl Pts',(-18.8667623768187,-16.8390585152533,
12.9049622477118));
#165813=CARTESIAN_POINT('Ctrl Pts',(-18.8881279175692,-16.8405095077609,
12.9036570286089));
#165814=CARTESIAN_POINT('Ctrl Pts',(-19.0047246468849,-16.8502069749094,
12.896470124863));
#165815=CARTESIAN_POINT('Ctrl Pts',(-19.0993233771937,-16.8645708848525,
12.8903979602762));
#165816=CARTESIAN_POINT('Ctrl Pts',(-19.3360518302462,-16.9171022305903,
12.874638198799));
#165817=CARTESIAN_POINT('Ctrl Pts',(-19.4757732903475,-16.9637734856989,
12.8647832448296));
#165818=CARTESIAN_POINT('Ctrl Pts',(-19.6204764948854,-17.0295034727646,
12.8544806231758));
#165819=CARTESIAN_POINT('Ctrl Pts',(-19.6313777229855,-17.0345676793184,
12.8537040930464));
#165820=CARTESIAN_POINT('Ctrl Pts',(-19.684638271346,-17.0598637811747,
12.8499101749084));
#165821=CARTESIAN_POINT('Ctrl Pts',(-19.7263632494966,-17.0814095823461,
12.8469377756625));
#165822=CARTESIAN_POINT('Ctrl Pts',(-19.774046542734,-17.1080772179113,
12.8435694545154));
#165823=CARTESIAN_POINT('Ctrl Pts',(-19.7807322571231,-17.1118642377903,
12.8430978536911));
#165824=CARTESIAN_POINT('Ctrl Pts',(-19.7914096780088,-17.1179893212938,
12.8423459502067));
#165825=CARTESIAN_POINT('Ctrl Pts',(-19.7954145253247,-17.1203041728711,
12.8420642165011));
#165826=CARTESIAN_POINT('Ctrl Pts',(-19.8024192482373,-17.1243836774142,
12.8415719957842));
#165827=CARTESIAN_POINT('Ctrl Pts',(-19.8054223979412,-17.1261426237375,
12.8413611439265));
#165828=CARTESIAN_POINT('Ctrl Pts',(-19.8117894489859,-17.1298929273187,
12.8409145053455));
#165829=CARTESIAN_POINT('Ctrl Pts',(-19.8151521698983,-17.1318861940101,
12.8406788454525));
#165830=CARTESIAN_POINT('Ctrl Pts',(-19.8220669391853,-17.1360108768627,
12.8401946904941));
#165831=CARTESIAN_POINT('Ctrl Pts',(-19.8256182943725,-17.1381434291685,
12.8399462698408));
#165832=CARTESIAN_POINT('Ctrl Pts',(-19.834471178125,-17.1434949120654,
12.8393275346212));
#165833=CARTESIAN_POINT('Ctrl Pts',(-19.8397649023677,-17.1467267658967,
12.8389580306695));
#165834=CARTESIAN_POINT('Ctrl Pts',(-19.8546646105452,-17.1559132648846,
12.8379191561724));
#165835=CARTESIAN_POINT('Ctrl Pts',(-19.8642373729619,-17.1619217274205,
12.8372530340652));
#165836=CARTESIAN_POINT('Ctrl Pts',(-19.8958505070486,-17.1821187998788,
12.8350560879775));
#165837=CARTESIAN_POINT('Ctrl Pts',(-19.9176762387845,-17.1966405643333,
12.833543963229));
#165838=CARTESIAN_POINT('Ctrl Pts',(-20.0759912279187,-17.3062715160992,
12.8225666700204));
#165839=CARTESIAN_POINT('Ctrl Pts',(-20.2011268501028,-17.4167761044752,
12.8137995936649));
#165840=CARTESIAN_POINT('Ctrl Pts',(-20.3826574391679,-17.6197688116501,
12.7988309613231));
#165841=CARTESIAN_POINT('Ctrl Pts',(-20.4472387654969,-17.7039134655659,
12.7928852697093));
#165842=CARTESIAN_POINT('Ctrl Pts',(-20.5129698561578,-17.8043266901874,
12.7858526703796));
#165843=CARTESIAN_POINT('Ctrl Pts',(-20.5205734975174,-17.8161994458466,
12.7850222646513));
#165844=CARTESIAN_POINT('Ctrl Pts',(-20.5325167209505,-17.8352649595421,
12.7836901381852));
#165845=CARTESIAN_POINT('Ctrl Pts',(-20.5369331453072,-17.8424092571693,
12.7831912595305));
#165846=CARTESIAN_POINT('Ctrl Pts',(-20.5446645848333,-17.8550841709679,
12.7823066273727));
#165847=CARTESIAN_POINT('Ctrl Pts',(-20.5479970846075,-17.8606040359401,
12.7819215216945));
#165848=CARTESIAN_POINT('Ctrl Pts',(-20.5548543643726,-17.8720804254847,
12.781121109729));
#165849=CARTESIAN_POINT('Ctrl Pts',(-20.5583752498665,-17.8780391768874,
12.7807056674335));
#165850=CARTESIAN_POINT('Ctrl Pts',(-20.5673726615341,-17.8934383358134,
12.7796323620631));
#165851=CARTESIAN_POINT('Ctrl Pts',(-20.5728054680181,-17.9029039334995,
12.7789729260842));
#165852=CARTESIAN_POINT('Ctrl Pts',(-20.595466542383,-17.9431032372606,
12.7761733581244));
#165853=CARTESIAN_POINT('Ctrl Pts',(-20.6119985375035,-17.9742210754947,
12.7740085190291));
#165854=CARTESIAN_POINT('Ctrl Pts',(-20.6533011646073,-18.0568794363104,
12.7682604816316));
#165855=CARTESIAN_POINT('Ctrl Pts',(-20.6767724033018,-18.1090336525876,
12.7646354791735));
#165856=CARTESIAN_POINT('Ctrl Pts',(-20.7066095078179,-18.1832214467718,
12.7594872233636));
#165857=CARTESIAN_POINT('Ctrl Pts',(-20.7147694497581,-18.2044974724095,
12.7580118269229));
#165858=CARTESIAN_POINT('Ctrl Pts',(-20.7225806094134,-18.2258897054408,
12.7565302021861));
#165859=CARTESIAN_POINT('Ctrl Pts',(-20.722580563326,-18.2258895792221,
12.5316746529861));
#165860=CARTESIAN_POINT('Ctrl Pts',(-20.6726392059308,-18.0891164249191,
12.5406280852242));
#165861=CARTESIAN_POINT('Ctrl Pts',(-20.6087205282652,-17.9578600560501,
12.5500631308234));
#165862=CARTESIAN_POINT('Ctrl Pts',(-20.495841044321,-17.7763075846016,
12.5641660621724));
#165863=CARTESIAN_POINT('Ctrl Pts',(-20.4570694493765,-17.7201849444968,
12.5686851501023));
#165864=CARTESIAN_POINT('Ctrl Pts',(-20.3695045829104,-17.605676700547,
12.578143339528));
#165865=CARTESIAN_POINT('Ctrl Pts',(-20.3201312863114,-17.5478449190529,
12.5830647942381));
#165866=CARTESIAN_POINT('Ctrl Pts',(-20.2570977371216,-17.4815915061845,
12.5887668295566));
#165867=CARTESIAN_POINT('Ctrl Pts',(-20.2463222522533,-17.4705111229829,
12.5897226874635));
#165868=CARTESIAN_POINT('Ctrl Pts',(-20.2323958720953,-17.4565009912937,
12.5909329936785));
#165869=CARTESIAN_POINT('Ctrl Pts',(-20.2293564012324,-17.4534618094339,
12.5911956468222));
#165870=CARTESIAN_POINT('Ctrl Pts',(-20.2234100628535,-17.4475521432674,
12.5917065391721));
#165871=CARTESIAN_POINT('Ctrl Pts',(-20.2205041026672,-17.4446807762249,
12.5919548464706));
#165872=CARTESIAN_POINT('Ctrl Pts',(-20.2150390814796,-17.4393119870393,
12.5924192353049));
#165873=CARTESIAN_POINT('Ctrl Pts',(-20.212482034711,-17.4368126654862,
12.5926354631504));
#165874=CARTESIAN_POINT('Ctrl Pts',(-20.2066071015656,-17.4310993913483,
12.593129859582));
#165875=CARTESIAN_POINT('Ctrl Pts',(-20.2032850258389,-17.4278898167287,
12.5934076862689));
#165876=CARTESIAN_POINT('Ctrl Pts',(-20.1929591289752,-17.417978741294,
12.5942659796904));
#165877=CARTESIAN_POINT('Ctrl Pts',(-20.1859196523087,-17.4113143430632,
12.5948436439327));
#165878=CARTESIAN_POINT('Ctrl Pts',(-20.1054372952489,-17.3361617773434,
12.6013673230243));
#165879=CARTESIAN_POINT('Ctrl Pts',(-20.0272461273801,-17.2729248900113,
12.6069500345036));
#165880=CARTESIAN_POINT('Ctrl Pts',(-19.8042374851132,-17.1174247970663,
12.6218252333107));
#165881=CARTESIAN_POINT('Ctrl Pts',(-19.6522468258273,-17.0368250357533,
12.630946333039));
#165882=CARTESIAN_POINT('Ctrl Pts',(-19.4517969301906,-16.9599333941322,
12.6432059230767));
#165883=CARTESIAN_POINT('Ctrl Pts',(-19.4109284029551,-16.9456776559222,
12.6457126382673));
#165884=CARTESIAN_POINT('Ctrl Pts',(-19.3584067042708,-16.9291445189173,
12.6489553371321));
#165885=CARTESIAN_POINT('Ctrl Pts',(-19.347130490564,-16.92569819061,12.6496527369484));
#165886=CARTESIAN_POINT('Ctrl Pts',(-19.3290044598153,-16.9203235195635,
12.6507759350379));
#165887=CARTESIAN_POINT('Ctrl Pts',(-19.3221725854135,-16.9183351711187,
12.6511997675783));
#165888=CARTESIAN_POINT('Ctrl Pts',(-19.3091831757126,-16.9146256625293,
12.652006577342));
#165889=CARTESIAN_POINT('Ctrl Pts',(-19.3030276024188,-16.9128978782556,
12.6523893334982));
#165890=CARTESIAN_POINT('Ctrl Pts',(-19.2890146527816,-16.9090330301002,
12.6532616502313));
#165891=CARTESIAN_POINT('Ctrl Pts',(-19.281152618338,-16.9069133724319,
12.653751770285));
#165892=CARTESIAN_POINT('Ctrl Pts',(-19.2607687325976,-16.9015436946763,
12.6550244059983));
#165893=CARTESIAN_POINT('Ctrl Pts',(-19.2482291098275,-16.8983630387472,
12.6558091509902));
#165894=CARTESIAN_POINT('Ctrl Pts',(-19.1667510125427,-16.8784892784045,
12.6609208404189));
#165895=CARTESIAN_POINT('Ctrl Pts',(-19.0970467100535,-16.8651565967857,
12.6653548976161));
#165896=CARTESIAN_POINT('Ctrl Pts',(-18.8701727638295,-16.8334722147435,
12.6799848545074));
#165897=CARTESIAN_POINT('Ctrl Pts',(-18.7115859575977,-16.8292210263562,
12.6905565333373));
#165898=CARTESIAN_POINT('Ctrl Pts',(-18.4973786524464,-16.8474971371102,
12.7046479156449));
#165899=CARTESIAN_POINT('Ctrl Pts',(-18.4409389667881,-16.8546116037792,
12.708336625622));
#165900=CARTESIAN_POINT('Ctrl Pts',(-18.3562334524621,-16.8687757483064,
12.7137752707624));
#165901=CARTESIAN_POINT('Ctrl Pts',(-18.3277158816484,-16.8741491253369,
12.7155892595651));
#165902=CARTESIAN_POINT('Ctrl Pts',(-18.2924798337307,-16.8815416604107,
12.7178019737823));
#165903=CARTESIAN_POINT('Ctrl Pts',(-18.2856504865096,-16.8830097849215,
12.7182294911942));
#165904=CARTESIAN_POINT('Ctrl Pts',(-18.2748697114186,-16.8853832457192,
12.7189021051901));
#165905=CARTESIAN_POINT('Ctrl Pts',(-18.2709134735501,-16.8862661592971,
12.7191484526767));
#165906=CARTESIAN_POINT('Ctrl Pts',(-18.2634665270089,-16.8879505631521,
12.7196112182471));
#165907=CARTESIAN_POINT('Ctrl Pts',(-18.2599753590175,-16.8887495384992,
12.7198277706465));
#165908=CARTESIAN_POINT('Ctrl Pts',(-18.2520106280811,-16.8905935991507,
12.720320931456));
#165909=CARTESIAN_POINT('Ctrl Pts',(-18.2475384343836,-16.8916443874431,
12.7205972089796));
#165910=CARTESIAN_POINT('Ctrl Pts',(-18.2357003146112,-16.8944665696313,
12.7213269389696));
#165911=CARTESIAN_POINT('Ctrl Pts',(-18.2283403396184,-16.8962629775936,
12.7217789915407));
#165912=CARTESIAN_POINT('Ctrl Pts',(-18.1775975456844,-16.9089371800601,
12.7248853376864));
#165913=CARTESIAN_POINT('Ctrl Pts',(-18.1345559281537,-16.9211487468151,
12.7274682464988));
#165914=CARTESIAN_POINT('Ctrl Pts',(-18.0851982777751,-16.9368585070135,
12.730403568002));
#165915=CARTESIAN_POINT('Ctrl Pts',(-18.0784769436947,-16.9390349143519,
12.7308027081704));
#165916=CARTESIAN_POINT('Ctrl Pts',(-18.0582336162471,-16.9457019662079,
12.7320034277663));
#165917=CARTESIAN_POINT('Ctrl Pts',(-18.044745778945,-16.9502955667868,
12.732801544856));
#165918=CARTESIAN_POINT('Ctrl Pts',(-17.8963569628164,-17.0025105735688,
12.741571219026));
#165919=CARTESIAN_POINT('Ctrl Pts',(-17.7665654491932,-17.0635537767595,
12.7491664376287));
#165920=CARTESIAN_POINT('Ctrl Pts',(-17.5642074657739,-17.18510422496,12.7621664916823));
#165921=CARTESIAN_POINT('Ctrl Pts',(-17.4877464683954,-17.2381783955783,
12.7673870748311));
#165922=CARTESIAN_POINT('Ctrl Pts',(-17.3985203725416,-17.3092497222161,
12.7740314606903));
#165923=CARTESIAN_POINT('Ctrl Pts',(-17.3822122522186,-17.322643026209,
12.7752699388119));
#165924=CARTESIAN_POINT('Ctrl Pts',(-17.3592685380076,-17.3420674851909,
12.7770483658151));
#165925=CARTESIAN_POINT('Ctrl Pts',(-17.3524664955446,-17.3479007302732,
12.7775802248401));
#165926=CARTESIAN_POINT('Ctrl Pts',(-17.3407813674926,-17.3580510295367,
12.7785020151554));
#165927=CARTESIAN_POINT('Ctrl Pts',(-17.335880771936,-17.3623478050028,
12.7788911022166));
#165928=CARTESIAN_POINT('Ctrl Pts',(-17.3265255808415,-17.3706270325755,
12.7796387159734));
#165929=CARTESIAN_POINT('Ctrl Pts',(-17.3220678450335,-17.3746058541631,
12.7799970884047));
#165930=CARTESIAN_POINT('Ctrl Pts',(-17.310498153287,-17.3850209008851,
12.7809328367908));
#165931=CARTESIAN_POINT('Ctrl Pts',(-17.3034130491469,-17.391486630634,
12.7815114574431));
#165932=CARTESIAN_POINT('Ctrl Pts',(-17.2792917200865,-17.4138016224707,
12.7835007981486));
#165933=CARTESIAN_POINT('Ctrl Pts',(-17.2624734614609,-17.4298830508599,
12.7849214292075));
#165934=CARTESIAN_POINT('Ctrl Pts',(-17.1239740107427,-17.5667557258532,
12.7969100999642));
#165935=CARTESIAN_POINT('Ctrl Pts',(-17.0171381398251,-17.7016205294686,
12.808145850001));
#165936=CARTESIAN_POINT('Ctrl Pts',(-16.8808749508392,-17.9245307106968,
12.8254101114445));
#165937=CARTESIAN_POINT('Ctrl Pts',(-16.8389294945554,-18.0041206017896,
12.8313402273036));
#165938=CARTESIAN_POINT('Ctrl Pts',(-16.786406127767,-18.1213061860514,
12.8395441228623));
#165939=CARTESIAN_POINT('Ctrl Pts',(-16.7716063354074,-18.1568989744915,
12.8419693529101));
#165940=CARTESIAN_POINT('Ctrl Pts',(-16.7550560170609,-18.1999842716596,
12.8448097528164));
#165941=CARTESIAN_POINT('Ctrl Pts',(-16.7523647584373,-18.2071048954922,
12.845276104228));
#165942=CARTESIAN_POINT('Ctrl Pts',(-16.7482513868724,-18.2181682686859,
12.845995745625));
#165943=CARTESIAN_POINT('Ctrl Pts',(-16.7468025082173,-18.2221009016467,
12.8462505900325));
#165944=CARTESIAN_POINT('Ctrl Pts',(-16.744143471165,-18.2293848259473,
12.8467207932211));
#165945=CARTESIAN_POINT('Ctrl Pts',(-16.7429301048028,-18.232734841755,
12.8469363373227));
#165946=CARTESIAN_POINT('Ctrl Pts',(-16.7402139764452,-18.2402934160427,
12.8474210746951));
#165947=CARTESIAN_POINT('Ctrl Pts',(-16.7387160833303,-18.2445036663757,
12.8476899767559));
#165948=CARTESIAN_POINT('Ctrl Pts',(-16.7343569286602,-18.2568802535473,
12.8484772970125));
#165949=CARTESIAN_POINT('Ctrl Pts',(-16.7315323510617,-18.2650595401201,
12.8489935902348));
#165950=CARTESIAN_POINT('Ctrl Pts',(-16.712149994112,-18.3223216616033,
12.8525815620223));
#165951=CARTESIAN_POINT('Ctrl Pts',(-16.6973469989159,-18.3719846977454,
12.8555577082946));
#165952=CARTESIAN_POINT('Ctrl Pts',(-16.6790029587518,-18.4429443200486,
12.8596848998645));
#165953=CARTESIAN_POINT('Ctrl Pts',(-16.6739428246946,-18.4638248237836,
12.8608842794552));
#165954=CARTESIAN_POINT('Ctrl Pts',(-16.6387823784657,-18.6192101247272,
12.8697214450266));
#165955=CARTESIAN_POINT('Ctrl Pts',(-16.621563652906,-18.7562927236294,
12.8770519057551));
#165956=CARTESIAN_POINT('Ctrl Pts',(-16.6153091136145,-18.9848146283761,
12.8896555702125));
#165957=CARTESIAN_POINT('Ctrl Pts',(-16.618663875674,-19.0756050852872,
12.8947579560401));
#165958=CARTESIAN_POINT('Ctrl Pts',(-16.6299380784356,-19.1866197428317,
12.9012593381151));
#165959=CARTESIAN_POINT('Ctrl Pts',(-16.6323486772578,-19.2073128775864,
12.9024822090889));
#165960=CARTESIAN_POINT('Ctrl Pts',(-16.6362262795873,-19.2368049976816,
12.9042420904617));
#165961=CARTESIAN_POINT('Ctrl Pts',(-16.6374441552643,-19.2456359224618,
12.9047712433211));
#165962=CARTESIAN_POINT('Ctrl Pts',(-16.6396477488413,-19.2609013094936,
12.9056898380959));
#165963=CARTESIAN_POINT('Ctrl Pts',(-16.6406074421037,-19.2673394488882,
12.9060784517288));
#165964=CARTESIAN_POINT('Ctrl Pts',(-16.6425065337519,-19.2796887304405,
12.9068262102084));
#165965=CARTESIAN_POINT('Ctrl Pts',(-16.6434413394955,-19.2856005234742,
12.9071852058547));
#165966=CARTESIAN_POINT('Ctrl Pts',(-16.6459483195019,-19.3010304365752,
12.9081249274343));
#165967=CARTESIAN_POINT('Ctrl Pts',(-16.6475604935405,-19.3105418345919,
12.9087069188967));
#165968=CARTESIAN_POINT('Ctrl Pts',(-16.6533404996115,-19.3432825195913,
12.9107198583121));
#165969=CARTESIAN_POINT('Ctrl Pts',(-16.6578316029644,-19.3664522688008,
12.9121610358039));
#165970=CARTESIAN_POINT('Ctrl Pts',(-16.6968555617556,-19.5511890244566,
12.9237897721436));
#165971=CARTESIAN_POINT('Ctrl Pts',(-16.7498014422358,-19.7082547965098,
12.9345918435711));
#165972=CARTESIAN_POINT('Ctrl Pts',(-16.8749489375303,-19.9727123861095,
12.9539263690238));
#165973=CARTESIAN_POINT('Ctrl Pts',(-16.9397446874142,-20.0827427822681,
12.9623537958568));
#165974=CARTESIAN_POINT('Ctrl Pts',(-17.0210404623721,-20.1960266799001,
12.9710016065529));
#165975=CARTESIAN_POINT('Ctrl Pts',(-17.0281138164715,-20.2057085394788,
12.9717403102875));
#165976=CARTESIAN_POINT('Ctrl Pts',(-17.0382747871505,-20.2193714407553,
12.9727815941784));
#165977=CARTESIAN_POINT('Ctrl Pts',(-17.0412947915898,-20.2234021570532,
12.9730886394964));
#165978=CARTESIAN_POINT('Ctrl Pts',(-17.0465196850856,-20.2303240615779,
12.9736156177129));
#165979=CARTESIAN_POINT('Ctrl Pts',(-17.0487176812485,-20.2332204051271,
12.9738360281671));
#165980=CARTESIAN_POINT('Ctrl Pts',(-17.0529903612111,-20.2388205814184,
12.9742619969251));
#165981=CARTESIAN_POINT('Ctrl Pts',(-17.0550641121286,-20.2415250673253,
12.974467620431));
#165982=CARTESIAN_POINT('Ctrl Pts',(-17.0606692276946,-20.2487985472894,
12.9750204221127));
#165983=CARTESIAN_POINT('Ctrl Pts',(-17.0642128007345,-20.2533581585189,
12.9753667446415));
#165984=CARTESIAN_POINT('Ctrl Pts',(-17.0773899300473,-20.2701710896825,
12.9766431860674));
#165985=CARTESIAN_POINT('Ctrl Pts',(-17.0871403354192,-20.2823327488407,
12.9775653668179));
#165986=CARTESIAN_POINT('Ctrl Pts',(-17.1836989037092,-20.4000813033934,
12.9864949800968));
#165987=CARTESIAN_POINT('Ctrl Pts',(-17.2804189429874,-20.4971490008717,
12.9938783338125));
#165988=CARTESIAN_POINT('Ctrl Pts',(-17.5049775028981,-20.6826273943054,
13.009694925083));
#165989=CARTESIAN_POINT('Ctrl Pts',(-17.6345178232724,-20.7676814038846,
13.0181143961081));
#165990=CARTESIAN_POINT('Ctrl Pts',(-17.7911005499161,-20.8475426771301,
13.0283508932813));
#165991=CARTESIAN_POINT('Ctrl Pts',(-17.8101924719464,-20.8569202125973,
13.0295990641214));
#165992=CARTESIAN_POINT('Ctrl Pts',(-17.8375492462544,-20.8698492778496,
13.0313889988085));
#165993=CARTESIAN_POINT('Ctrl Pts',(-17.8457008244117,-20.87363846165,13.031922526823));
#165994=CARTESIAN_POINT('Ctrl Pts',(-17.8598084670379,-20.8800873188591,
13.032846291248));
#165995=CARTESIAN_POINT('Ctrl Pts',(-17.8657531893988,-20.8827716125581,
13.0332356735642));
#165996=CARTESIAN_POINT('Ctrl Pts',(-17.8771616926128,-20.8878596915624,
13.0339832119924));
#165997=CARTESIAN_POINT('Ctrl Pts',(-17.8826234286354,-20.8902679285949,
13.0343412107489));
#165998=CARTESIAN_POINT('Ctrl Pts',(-17.8968576482662,-20.8964724350867,
13.0352745664545));
#165999=CARTESIAN_POINT('Ctrl Pts',(-17.9056457156943,-20.9002324150017,
13.0358511555999));
#166000=CARTESIAN_POINT('Ctrl Pts',(-17.9357273945377,-20.9128625503068,
13.0378261756929));
#166001=CARTESIAN_POINT('Ctrl Pts',(-17.9571397905482,-20.9214438917476,
13.0392343262504));
#166002=CARTESIAN_POINT('Ctrl Pts',(-18.1416936390911,-20.9919286503674,
13.051395127585));
#166003=CARTESIAN_POINT('Ctrl Pts',(-18.311742252086,-21.0337807434095,
13.0628424359433));
#166004=CARTESIAN_POINT('Ctrl Pts',(-18.5720581558695,-21.0646185849479,
13.0801628309152));
#166005=CARTESIAN_POINT('Ctrl Pts',(-18.65972413674,-21.0695144574044,13.085945321539));
#166006=CARTESIAN_POINT('Ctrl Pts',(-18.7854445783979,-21.0687159538271,
13.0939733905083));
#166007=CARTESIAN_POINT('Ctrl Pts',(-18.8234329046947,-21.0674515226767,
13.0963639509826));
#166008=CARTESIAN_POINT('Ctrl Pts',(-18.8689372444367,-21.0647087882098,
13.0991692345239));
#166009=CARTESIAN_POINT('Ctrl Pts',(-18.8765029382357,-21.0642119686014,
13.0996337111039));
#166010=CARTESIAN_POINT('Ctrl Pts',(-18.8882398367112,-21.0633778871278,
13.1003510876822));
#166011=CARTESIAN_POINT('Ctrl Pts',(-18.8924128967652,-21.0630688914194,
13.1006055268134));
#166012=CARTESIAN_POINT('Ctrl Pts',(-18.9001380748592,-21.0624738422768,
13.1010753540193));
#166013=CARTESIAN_POINT('Ctrl Pts',(-18.9036903563048,-21.0621911956339,
13.1012909250337));
#166014=CARTESIAN_POINT('Ctrl Pts',(-18.9117040925988,-21.061533194822,
13.1017761907375));
#166015=CARTESIAN_POINT('Ctrl Pts',(-18.9161650676059,-21.0611526577214,
13.1020455913726));
#166016=CARTESIAN_POINT('Ctrl Pts',(-18.9292829714867,-21.0599917246666,
13.1028357275256));
#166017=CARTESIAN_POINT('Ctrl Pts',(-18.9379364610194,-21.0591721514735,
13.1033543152021));
#166018=CARTESIAN_POINT('Ctrl Pts',(-18.9990565437284,-21.0530034165173,
13.1069999924302));
#166019=CARTESIAN_POINT('Ctrl Pts',(-19.0513168291057,-21.0457481572747,
13.1100280163762));
#166020=CARTESIAN_POINT('Ctrl Pts',(-19.1188001538871,-21.033794189404,
13.1138841966698));
#166021=CARTESIAN_POINT('Ctrl Pts',(-19.1343133969745,-21.0308668565553,
13.1147669153121));
#166022=CARTESIAN_POINT('Ctrl Pts',(-19.1996437267442,-21.0177806647656,
13.1184736760663));
#166023=CARTESIAN_POINT('Ctrl Pts',(-19.2491205902866,-21.0060021812644,
13.1212551280918));
#166024=CARTESIAN_POINT('Ctrl Pts',(-19.4035796404331,-20.9632986832349,
13.1299803013965));
#166025=CARTESIAN_POINT('Ctrl Pts',(-19.5066126262187,-20.9260132069043,
13.1358712809829));
#166026=CARTESIAN_POINT('Ctrl Pts',(-19.6565774838452,-20.8581964114394,
13.1450223352114));
#166027=CARTESIAN_POINT('Ctrl Pts',(-19.7059453743396,-20.8335035249732,
13.1481337027462));
#166028=CARTESIAN_POINT('Ctrl Pts',(-19.784378474871,-20.7903615760218,
13.15328351995));
#166029=CARTESIAN_POINT('Ctrl Pts',(-19.8140584783427,-20.7730825656447,
13.1552824652543));
#166030=CARTESIAN_POINT('Ctrl Pts',(-19.8525132550122,-20.749424271264,
13.157945208757));
#166031=CARTESIAN_POINT('Ctrl Pts',(-19.8616788915706,-20.7436880932539,
13.158585431278));
#166032=CARTESIAN_POINT('Ctrl Pts',(-19.8766199786655,-20.7341773706232,
13.1596384030966));
#166033=CARTESIAN_POINT('Ctrl Pts',(-19.8824217027545,-20.7304443165073,
13.1600496095859));
#166034=CARTESIAN_POINT('Ctrl Pts',(-19.8936175178687,-20.7231628662304,
13.160847705117));
#166035=CARTESIAN_POINT('Ctrl Pts',(-19.8990138328306,-20.7196180170903,
13.1612344584391));
#166036=CARTESIAN_POINT('Ctrl Pts',(-19.9114372707823,-20.7113754352052,
13.1621296962606));
#166037=CARTESIAN_POINT('Ctrl Pts',(-19.9184526074928,-20.7066602138298,
13.1626388362401));
#166038=CARTESIAN_POINT('Ctrl Pts',(-19.937245773135,-20.6938646950458,
13.1640126083004));
#166039=CARTESIAN_POINT('Ctrl Pts',(-19.9489702189492,-20.685707114188,
13.1648801648937));
#166040=CARTESIAN_POINT('Ctrl Pts',(-20.0755780798838,-20.5957014666802,
13.1743651431348));
#166041=CARTESIAN_POINT('Ctrl Pts',(-20.1820673884184,-20.5027010496833,
13.1834322607992));
#166042=CARTESIAN_POINT('Ctrl Pts',(-20.3445945972032,-20.3293207961588,
13.1990666404115));
#166043=CARTESIAN_POINT('Ctrl Pts',(-20.4057792723084,-20.2543754434638,
13.2054948121062));
#166044=CARTESIAN_POINT('Ctrl Pts',(-20.4993339321267,-20.1222738997033,
13.2160579507907));
#166045=CARTESIAN_POINT('Ctrl Pts',(-20.5345603034473,-20.0673157048691,
13.2202520750685));
#166046=CARTESIAN_POINT('Ctrl Pts',(-20.5737749635816,-19.9994207242408,
13.2251235166052));
#166047=CARTESIAN_POINT('Ctrl Pts',(-20.5802489458008,-19.9879666695039,
13.2259351052215));
#166048=CARTESIAN_POINT('Ctrl Pts',(-20.5891459492004,-19.9718773660392,
13.2270601035786));
#166049=CARTESIAN_POINT('Ctrl Pts',(-20.5916590623751,-19.9672926395438,
13.2273789882407));
#166050=CARTESIAN_POINT('Ctrl Pts',(-20.5959079053943,-19.959472793484,
13.2279199561409));
#166051=CARTESIAN_POINT('Ctrl Pts',(-20.597652242804,-19.9562423992223,
13.2281425834928));
#166052=CARTESIAN_POINT('Ctrl Pts',(-20.6009776731424,-19.9500454237942,
13.2285680129199));
#166053=CARTESIAN_POINT('Ctrl Pts',(-20.6025601087368,-19.9470796050424,
13.2287709030964));
#166054=CARTESIAN_POINT('Ctrl Pts',(-20.6067291654819,-19.9392208989337,
13.2293066524614));
#166055=CARTESIAN_POINT('Ctrl Pts',(-20.6093036956872,-19.9343215772095,
13.2296387490427));
#166056=CARTESIAN_POINT('Ctrl Pts',(-20.6183487932644,-19.9169436287297,
13.2308101746344));
#166057=CARTESIAN_POINT('Ctrl Pts',(-20.624714422573,-19.9044104037931,
13.2316431587626));
#166058=CARTESIAN_POINT('Ctrl Pts',(-20.7038354065135,-19.7447097740224,
13.2421192210842));
#166059=CARTESIAN_POINT('Ctrl Pts',(-20.7593686541722,-19.5896039360084,
13.2508474239028));
#166060=CARTESIAN_POINT('Ctrl Pts',(-20.8270296741189,-19.2974350214183,
13.2671777061719));
#166061=CARTESIAN_POINT('Ctrl Pts',(-20.8448588559151,-19.1626336171357,
13.2746744187749));
#166062=CARTESIAN_POINT('Ctrl Pts',(-20.8502665616344,-19.0102153568468,
13.2835989852316));
#166063=CARTESIAN_POINT('Ctrl Pts',(-20.8506630232661,-18.9933619287538,
13.2845914868813));
#166064=CARTESIAN_POINT('Ctrl Pts',(-20.8509528941037,-18.9683224475064,
13.2860751767025));
#166065=CARTESIAN_POINT('Ctrl Pts',(-20.8510001744628,-18.9601385869792,
13.2865615472164));
#166066=CARTESIAN_POINT('Ctrl Pts',(-20.8509998627402,-18.9455564775112,
13.287430820218));
#166067=CARTESIAN_POINT('Ctrl Pts',(-20.8509707194824,-18.9391582988112,
13.2878131398688));
#166068=CARTESIAN_POINT('Ctrl Pts',(-20.8508481156793,-18.9256683307239,
13.2886211834744));
#166069=CARTESIAN_POINT('Ctrl Pts',(-20.8507480205214,-18.918576694131,
13.2890471107737));
#166070=CARTESIAN_POINT('Ctrl Pts',(-20.8503886243578,-18.8998005217454,
13.2901779006967));
#166071=CARTESIAN_POINT('Ctrl Pts',(-20.8500681972661,-18.8881175237119,
13.2908846698275));
#166072=CARTESIAN_POINT('Ctrl Pts',(-20.8481220039088,-18.8336263276935,
13.2941963139784));
#166073=CARTESIAN_POINT('Ctrl Pts',(-20.8452939285612,-18.7908736457192,
13.2968385575518));
#166074=CARTESIAN_POINT('Ctrl Pts',(-20.8339020495849,-18.6730661298717,
13.3042463415294));
#166075=CARTESIAN_POINT('Ctrl Pts',(-20.8226163019958,-18.5983437869904,
13.3090901552408));
#166076=CARTESIAN_POINT('Ctrl Pts',(-20.7864357517189,-18.422914129632,
13.32076528655));
#166077=CARTESIAN_POINT('Ctrl Pts',(-20.7580935482861,-18.3231480981609,
13.3276519677475));
#166078=CARTESIAN_POINT('Ctrl Pts',(-20.7225805383928,-18.2258895109384,
13.3344632701429));
#166079=CARTESIAN_POINT('Origin',(-18.734,-18.952,0.));
#166080=CARTESIAN_POINT('',(-20.7249097977618,-18.2250590878524,14.355439975907));
#166081=CARTESIAN_POINT('',(-20.7225805482453,-18.2258895379212,14.1348940720942));
#166082=CARTESIAN_POINT('',(-20.7225805737622,-18.2258896078036,0.));
#166083=CARTESIAN_POINT('',(-20.8478582366632,-18.9515402791097,14.3110888556867));
#166084=CARTESIAN_POINT('Ctrl Pts',(-20.8476070208165,-18.9515314190756,
14.3109441065097));
#166085=CARTESIAN_POINT('Ctrl Pts',(-20.8480883129925,-18.7039932788114,
14.3257760629755));
#166086=CARTESIAN_POINT('Ctrl Pts',(-20.8073980168978,-18.4566058676403,
14.3406080194413));
#166087=CARTESIAN_POINT('Ctrl Pts',(-20.7249097977618,-18.2250590878524,
14.355439975907));
#166088=CARTESIAN_POINT('Ctrl Pts',(-20.8509999712464,-18.9516510837263,
14.3128991057222));
#166089=CARTESIAN_POINT('Ctrl Pts',(-20.8510014360955,-18.9605388474593,
14.312378540246));
#166090=CARTESIAN_POINT('Ctrl Pts',(-20.8509469309215,-18.9694264524988,
14.3118562864048));
#166091=CARTESIAN_POINT('Ctrl Pts',(-20.8507292584146,-18.9869375893009,
14.3108238157218));
#166092=CARTESIAN_POINT('Ctrl Pts',(-20.8505693532511,-18.9955609702645,
14.3103137106949));
#166093=CARTESIAN_POINT('Ctrl Pts',(-20.8502036146175,-19.0103940167029,
14.3094333214644));
#166094=CARTESIAN_POINT('Ctrl Pts',(-20.850023130942,-19.016604239536,14.3090638320091));
#166095=CARTESIAN_POINT('Ctrl Pts',(-20.8496088606317,-19.0289820929612,
14.3083255693495));
#166096=CARTESIAN_POINT('Ctrl Pts',(-20.8493754333867,-19.0351496746715,
14.3079568109861));
#166097=CARTESIAN_POINT('Ctrl Pts',(-20.8488557235166,-19.0474570436085,
14.3072191250324));
#166098=CARTESIAN_POINT('Ctrl Pts',(-20.8485696657882,-19.0535967802356,
14.3068502080422));
#166099=CARTESIAN_POINT('Ctrl Pts',(-20.8477228783011,-19.0702146299458,
14.3058491893612));
#166100=CARTESIAN_POINT('Ctrl Pts',(-20.8471109811983,-19.0806898594257,
14.3052154881987));
#166101=CARTESIAN_POINT('Ctrl Pts',(-20.8445147262455,-19.1201005063434,
14.3028209232233));
#166102=CARTESIAN_POINT('Ctrl Pts',(-20.8420137567466,-19.1489976149218,
14.3010439561728));
#166103=CARTESIAN_POINT('Ctrl Pts',(-20.815907258728,-19.3923281087132,
14.2858946196423));
#166104=CARTESIAN_POINT('Ctrl Pts',(-20.7602432250021,-19.6020196557498,
14.2714263286646));
#166105=CARTESIAN_POINT('Ctrl Pts',(-20.6467520636624,-19.8617627039859,
14.2529056809952));
#166106=CARTESIAN_POINT('Ctrl Pts',(-20.6166241201534,-19.9225755266126,
14.2485387040674));
#166107=CARTESIAN_POINT('Ctrl Pts',(-20.5770943855693,-19.9935720493767,
14.2434879589216));
#166108=CARTESIAN_POINT('Ctrl Pts',(-20.5704516718481,-20.0052400136454,
14.2426595268361));
#166109=CARTESIAN_POINT('Ctrl Pts',(-20.5610470376768,-20.0213997863401,
14.2415153069965));
#166110=CARTESIAN_POINT('Ctrl Pts',(-20.558378825691,-20.0259453815967,
14.2411937972707));
#166111=CARTESIAN_POINT('Ctrl Pts',(-20.5538191683491,-20.0336472313171,
14.2406497024673));
#166112=CARTESIAN_POINT('Ctrl Pts',(-20.5519364303086,-20.0368085889079,
14.2404265583759));
#166113=CARTESIAN_POINT('Ctrl Pts',(-20.5483224687521,-20.04284106053,14.2400011420792));
#166114=CARTESIAN_POINT('Ctrl Pts',(-20.5465926605702,-20.0457129820781,
14.2397987769742));
#166115=CARTESIAN_POINT('Ctrl Pts',(-20.5420136668464,-20.053274575647,
14.2392663669325));
#166116=CARTESIAN_POINT('Ctrl Pts',(-20.5391530354266,-20.0579573367416,
14.2389370667533));
#166117=CARTESIAN_POINT('Ctrl Pts',(-20.5290469898277,-20.0743569314511,
14.2377850743866));
#166118=CARTESIAN_POINT('Ctrl Pts',(-20.5217052701548,-20.0860144031987,
14.2369684545243));
#166119=CARTESIAN_POINT('Ctrl Pts',(-20.4236098853709,-20.2384536124661,
14.2263084073253));
#166120=CARTESIAN_POINT('Ctrl Pts',(-20.3165592300704,-20.3680749711931,
14.2174199495125));
#166121=CARTESIAN_POINT('Ctrl Pts',(-20.1071165397495,-20.5678912026601,
14.201648127221));
#166122=CARTESIAN_POINT('Ctrl Pts',(-20.0118088457996,-20.6442626566637,
14.1949126375874));
#166123=CARTESIAN_POINT('Ctrl Pts',(-19.8967870552831,-20.7211483787345,
14.1868799981298));
#166124=CARTESIAN_POINT('Ctrl Pts',(-19.8830022008332,-20.7301320654897,
14.1859191076192));
#166125=CARTESIAN_POINT('Ctrl Pts',(-19.860972871489,-20.7441256026124,
14.184385580337));
#166126=CARTESIAN_POINT('Ctrl Pts',(-19.8527962948688,-20.7492414625177,
14.1838168278146));
#166127=CARTESIAN_POINT('Ctrl Pts',(-19.8372243392276,-20.75883696328,14.1827343413239));
#166128=CARTESIAN_POINT('Ctrl Pts',(-19.8298359015976,-20.7633275319303,
14.1822210199465));
#166129=CARTESIAN_POINT('Ctrl Pts',(-19.8169494055923,-20.7710520248803,
14.1813261175671));
#166130=CARTESIAN_POINT('Ctrl Pts',(-19.8114638196377,-20.7743066153345,
14.1809452973286));
#166131=CARTESIAN_POINT('Ctrl Pts',(-19.800801872806,-20.7805673614268,
14.1802053303951));
#166132=CARTESIAN_POINT('Ctrl Pts',(-19.7956273000035,-20.7835764537254,
14.1798462951409));
#166133=CARTESIAN_POINT('Ctrl Pts',(-19.7820770209202,-20.7913794311546,
14.1789063217241));
#166134=CARTESIAN_POINT('Ctrl Pts',(-19.773681243935,-20.7961380207893,
14.178324116709));
#166135=CARTESIAN_POINT('Ctrl Pts',(-19.7446895773684,-20.812309116856,
14.1763142087727));
#166136=CARTESIAN_POINT('Ctrl Pts',(-19.7239365761549,-20.8234349940621,
14.1748763337507));
#166137=CARTESIAN_POINT('Ctrl Pts',(-19.555430641894,-20.9101854463847,
14.1632041284054));
#166138=CARTESIAN_POINT('Ctrl Pts',(-19.3994619530342,-20.9685264577361,
14.152348894216));
#166139=CARTESIAN_POINT('Ctrl Pts',(-19.1152559846428,-21.0382378526541,
14.1330105284854));
#166140=CARTESIAN_POINT('Ctrl Pts',(-18.9897188576312,-21.057316856051,
14.1246326210804));
#166141=CARTESIAN_POINT('Ctrl Pts',(-18.8512577411353,-21.0657840985883,
14.1160292893991));
#166142=CARTESIAN_POINT('Ctrl Pts',(-18.8392907274131,-21.066413978212,
14.1152910141762));
#166143=CARTESIAN_POINT('Ctrl Pts',(-18.8222882584098,-21.0671641870112,
14.1142502251586));
#166144=CARTESIAN_POINT('Ctrl Pts',(-18.8172569832257,-21.0673682021185,
14.1139432518533));
#166145=CARTESIAN_POINT('Ctrl Pts',(-18.8085917741356,-21.067688607849,
14.1134163580798));
#166146=CARTESIAN_POINT('Ctrl Pts',(-18.8049581960322,-21.0678135913507,
14.1131959604581));
#166147=CARTESIAN_POINT('Ctrl Pts',(-18.7979176584284,-21.0680376058945,
14.1127699857626));
#166148=CARTESIAN_POINT('Ctrl Pts',(-18.7945107816376,-21.0681377701615,
14.112564343633));
#166149=CARTESIAN_POINT('Ctrl Pts',(-18.785329555893,-21.0683855133529,
14.1120114270799));
#166150=CARTESIAN_POINT('Ctrl Pts',(-18.7795547712931,-21.068517689279,
14.1116650089419));
#166151=CARTESIAN_POINT('Ctrl Pts',(-18.7581848562079,-21.0689193111002,
14.1103878415527));
#166152=CARTESIAN_POINT('Ctrl Pts',(-18.7425869945597,-21.0690400498063,
14.1094650421133));
#166153=CARTESIAN_POINT('Ctrl Pts',(-18.5906053038285,-21.0685366994878,
14.1005528397399));
#166154=CARTESIAN_POINT('Ctrl Pts',(-18.4545648530217,-21.05490654891,14.0931846465046));
#166155=CARTESIAN_POINT('Ctrl Pts',(-18.1689284329872,-20.9980575117669,
14.0773689311472));
#166156=CARTESIAN_POINT('Ctrl Pts',(-18.0208832086587,-20.9512784175718,
14.0689349670101));
#166157=CARTESIAN_POINT('Ctrl Pts',(-17.8598079324731,-20.8801933712459,
14.0586815360964));
#166158=CARTESIAN_POINT('Ctrl Pts',(-17.8404789674107,-20.8713127842066,
14.057433318977));
#166159=CARTESIAN_POINT('Ctrl Pts',(-17.8131765986745,-20.8582670517137,
14.0556433293685));
#166160=CARTESIAN_POINT('Ctrl Pts',(-17.8050904620997,-20.8543398422678,
14.0551097934122));
#166161=CARTESIAN_POINT('Ctrl Pts',(-17.791180615331,-20.8474743874975,
14.054186019593));
#166162=CARTESIAN_POINT('Ctrl Pts',(-17.7853449785908,-20.8445604863923,
14.0537966358714));
#166163=CARTESIAN_POINT('Ctrl Pts',(-17.7741949792,-20.8389284438281,14.0530490977907));
#166164=CARTESIAN_POINT('Ctrl Pts',(-17.7688784561684,-20.8362146997035,
14.052691100802));
#166165=CARTESIAN_POINT('Ctrl Pts',(-17.7550784322163,-20.8290969418229,
14.0517577564098));
#166166=CARTESIAN_POINT('Ctrl Pts',(-17.7466132250411,-20.824657928406,
14.0511811768692));
#166167=CARTESIAN_POINT('Ctrl Pts',(-17.71782353978,-20.8093116193805,14.0492062246067));
#166168=CARTESIAN_POINT('Ctrl Pts',(-17.6976479570919,-20.7981298510406,
14.047798133178));
#166169=CARTESIAN_POINT('Ctrl Pts',(-17.5264449751161,-20.6995543916272,
14.035637443227));
#166170=CARTESIAN_POINT('Ctrl Pts',(-17.3866017638648,-20.5941420245203,
14.024190190605));
#166171=CARTESIAN_POINT('Ctrl Pts',(-17.1982886047833,-20.4117853370239,
14.006869735388));
#166172=CARTESIAN_POINT('Ctrl Pts',(-17.1391261069682,-20.3469057028291,
14.0010871382322));
#166173=CARTESIAN_POINT('Ctrl Pts',(-17.0603452764371,-20.248924388656,
13.9930589421129));
#166174=CARTESIAN_POINT('Ctrl Pts',(-17.0373338866468,-20.2186718275902,
13.990668356381));
#166175=CARTESIAN_POINT('Ctrl Pts',(-17.0107219488226,-20.1816581811141,
13.9878630472437));
#166176=CARTESIAN_POINT('Ctrl Pts',(-17.0063290290687,-20.1754784445367,
13.9873985692915));
#166177=CARTESIAN_POINT('Ctrl Pts',(-16.9995632764417,-20.1658516225195,
13.9866811910579));
#166178=CARTESIAN_POINT('Ctrl Pts',(-16.9971673558746,-20.1624209501328,
13.9864267516327));
#166179=CARTESIAN_POINT('Ctrl Pts',(-16.992749885307,-20.1560555373117,
13.9859569241591));
#166180=CARTESIAN_POINT('Ctrl Pts',(-16.9907255906737,-20.1531228217541,
13.9857413531691));
#166181=CARTESIAN_POINT('Ctrl Pts',(-16.9861746963316,-20.1464939314966,
13.9852560878668));
#166182=CARTESIAN_POINT('Ctrl Pts',(-16.9836524181472,-20.1427948555794,
13.9849866876068));
#166183=CARTESIAN_POINT('Ctrl Pts',(-16.9762679474938,-20.1318909192387,
13.9841965535607));
#166184=CARTESIAN_POINT('Ctrl Pts',(-16.9714383023856,-20.1246639832771,
13.9836779675989));
#166185=CARTESIAN_POINT('Ctrl Pts',(-16.9376215326702,-20.073380662921,
13.9800323698311));
#166186=CARTESIAN_POINT('Ctrl Pts',(-16.9102424847078,-20.0282804945466,
13.9770044185946));
#166187=CARTESIAN_POINT('Ctrl Pts',(-16.8769283941964,-19.9684747513366,
13.973152481501));
#166188=CARTESIAN_POINT('Ctrl Pts',(-16.8694353012686,-19.9546636379199,
13.972273883515));
#166189=CARTESIAN_POINT('Ctrl Pts',(-16.7917531791569,-19.8075986866824,
13.963020402823));
#166190=CARTESIAN_POINT('Ctrl Pts',(-16.7358199237623,-19.6672985567803,
13.9550418741927));
#166191=CARTESIAN_POINT('Ctrl Pts',(-16.6786700562493,-19.4629751067554,
13.943302459916));
#166192=CARTESIAN_POINT('Ctrl Pts',(-16.6646856642338,-19.4030144864149,
13.9398482784423));
#166193=CARTESIAN_POINT('Ctrl Pts',(-16.6464811915163,-19.306025395074,
13.9341845511461));
#166194=CARTESIAN_POINT('Ctrl Pts',(-16.6405912302544,-19.2693456024298,
13.932025680234));
#166195=CARTESIAN_POINT('Ctrl Pts',(-16.6341955207937,-19.2215067079759,
13.9291805581188));
#166196=CARTESIAN_POINT('Ctrl Pts',(-16.6328085296784,-19.2104707226106,
13.9285222036378));
#166197=CARTESIAN_POINT('Ctrl Pts',(-16.6306942844003,-19.1925049069366,
13.9274469857476));
#166198=CARTESIAN_POINT('Ctrl Pts',(-16.6299141509969,-19.1855814242963,
13.9270317949479));
#166199=CARTESIAN_POINT('Ctrl Pts',(-16.6284796090807,-19.1722595076541,
13.9262312461332));
#166200=CARTESIAN_POINT('Ctrl Pts',(-16.6278201536842,-19.1658616862521,
13.9258460519744));
#166201=CARTESIAN_POINT('Ctrl Pts',(-16.6263769640699,-19.1512057928275,
13.9249619450536));
#166202=CARTESIAN_POINT('Ctrl Pts',(-16.625612595598,-19.1429459593165,
13.9244624281989));
#166203=CARTESIAN_POINT('Ctrl Pts',(-16.6237108599387,-19.1209900023121,
13.9231312261583));
#166204=CARTESIAN_POINT('Ctrl Pts',(-16.6226582994084,-19.107287104761,
13.9222968918674));
#166205=CARTESIAN_POINT('Ctrl Pts',(-16.6156492014754,-19.0027133894429,
13.9159018783798));
#166206=CARTESIAN_POINT('Ctrl Pts',(-16.6154289765755,-18.9115654345479,
13.9101616903506));
#166207=CARTESIAN_POINT('Ctrl Pts',(-16.6298062740627,-18.6802080758641,
13.8951896727587));
#166208=CARTESIAN_POINT('Ctrl Pts',(-16.652526716625,-18.540945083973,13.8857808166372));
#166209=CARTESIAN_POINT('Ctrl Pts',(-16.7027934891498,-18.3530150138238,
13.8730499831034));
#166210=CARTESIAN_POINT('Ctrl Pts',(-16.7186705068227,-18.3015918780689,
13.8695669561803));
#166211=CARTESIAN_POINT('Ctrl Pts',(-16.7457537754623,-18.224436830547,
13.8643941405357));
#166212=CARTESIAN_POINT('Ctrl Pts',(-16.7555396984852,-18.1982319813948,
13.8626469172767));
#166213=CARTESIAN_POINT('Ctrl Pts',(-16.7683850010594,-18.165810252608,
13.8605040155152));
#166214=CARTESIAN_POINT('Ctrl Pts',(-16.7709588260316,-18.1594055290996,
13.8600816261532));
#166215=CARTESIAN_POINT('Ctrl Pts',(-16.7750868929788,-18.1492766843221,
13.8594152380421));
#166216=CARTESIAN_POINT('Ctrl Pts',(-16.7766205105752,-18.1455442867704,
13.859170026412));
#166217=CARTESIAN_POINT('Ctrl Pts',(-16.7795369287051,-18.138503867484,
13.8587081715774));
#166218=CARTESIAN_POINT('Ctrl Pts',(-16.780917443828,-18.1351950149378,
13.8584914010853));
#166219=CARTESIAN_POINT('Ctrl Pts',(-16.7840980326324,-18.1276258694268,
13.8579961761178));
#166220=CARTESIAN_POINT('Ctrl Pts',(-16.7859036636946,-18.1233679616951,
13.8577180627045));
#166221=CARTESIAN_POINT('Ctrl Pts',(-16.790745127673,-18.1120544674999,
13.8569802592059));
#166222=CARTESIAN_POINT('Ctrl Pts',(-16.7938054622387,-18.105009353016,
13.8565220189608));
#166223=CARTESIAN_POINT('Ctrl Pts',(-16.8158172413755,-18.0550819824384,
13.8532820550441));
#166224=CARTESIAN_POINT('Ctrl Pts',(-16.8361517793974,-18.0128195729012,
13.8505788338361));
#166225=CARTESIAN_POINT('Ctrl Pts',(-16.8622548894907,-17.9628849218245,
13.8473921435814));
#166226=CARTESIAN_POINT('Ctrl Pts',(-16.8666912053126,-17.9545350802392,
13.8468595336313));
#166227=CARTESIAN_POINT('Ctrl Pts',(-16.9495543953602,-17.8010639600214,
13.8370697901186));
#166228=CARTESIAN_POINT('Ctrl Pts',(-17.0446244900916,-17.6655641278161,
13.8283772994982));
#166229=CARTESIAN_POINT('Ctrl Pts',(-17.1946818535298,-17.497408547478,
13.8158966267372));
#166230=CARTESIAN_POINT('Ctrl Pts',(-17.2368015447831,-17.4540905822883,
13.8125041463953));
#166231=CARTESIAN_POINT('Ctrl Pts',(-17.3073622529474,-17.387475507713,
13.8069324970062));
#166232=CARTESIAN_POINT('Ctrl Pts',(-17.3346589072069,-17.3630140289342,
13.804801877169));
#166233=CARTESIAN_POINT('Ctrl Pts',(-17.3710083433145,-17.3321033119606,
13.8019889058576));
#166234=CARTESIAN_POINT('Ctrl Pts',(-17.3794971322821,-17.3249986138849,
13.8013336602531));
#166235=CARTESIAN_POINT('Ctrl Pts',(-17.3934098967941,-17.3135386622874,
13.8002622589076));
#166236=CARTESIAN_POINT('Ctrl Pts',(-17.3988003747197,-17.309142934133,
13.7998477532396));
#166237=CARTESIAN_POINT('Ctrl Pts',(-17.4092198962982,-17.3007313682633,
13.7990476487931));
#166238=CARTESIAN_POINT('Ctrl Pts',(-17.4142457882592,-17.296711736133,
13.7986622091267));
#166239=CARTESIAN_POINT('Ctrl Pts',(-17.4258116925875,-17.2875476609736,
13.797776295505));
#166240=CARTESIAN_POINT('Ctrl Pts',(-17.432363832322,-17.2824187589559,
13.7972752091056));
#166241=CARTESIAN_POINT('Ctrl Pts',(-17.4498869072675,-17.2688678438976,
13.7959370948986));
#166242=CARTESIAN_POINT('Ctrl Pts',(-17.4609102893831,-17.2605145982584,
13.7950973741676));
#166243=CARTESIAN_POINT('Ctrl Pts',(-17.5478113223775,-17.1959938516101,
13.788492543134));
#166244=CARTESIAN_POINT('Ctrl Pts',(-17.6272770229325,-17.1448582822446,
13.7825340005772));
#166245=CARTESIAN_POINT('Ctrl Pts',(-17.8649989507245,-17.0134594411235,
13.7649613241975));
#166246=CARTESIAN_POINT('Ctrl Pts',(-18.030255929927,-16.9475448290306,
13.7529883196793));
#166247=CARTESIAN_POINT('Ctrl Pts',(-18.2409377359212,-16.892821776179,
13.73906029975));
#166248=CARTESIAN_POINT('Ctrl Pts',(-18.2803769179404,-16.8837756536014,
13.7365113679217));
#166249=CARTESIAN_POINT('Ctrl Pts',(-18.327620672732,-16.8743560521237,
13.733546088942));
#166250=CARTESIAN_POINT('Ctrl Pts',(-18.3351957454265,-16.8728887229116,
13.7330733130385));
#166251=CARTESIAN_POINT('Ctrl Pts',(-18.3469196367595,-16.8706841793789,
13.7323459155056));
#166252=CARTESIAN_POINT('Ctrl Pts',(-18.3510628270251,-16.8699178990631,
13.7320896865725));
#166253=CARTESIAN_POINT('Ctrl Pts',(-18.3587123022363,-16.8685267393389,
13.7316181854028));
#166254=CARTESIAN_POINT('Ctrl Pts',(-18.3622178500195,-16.8678983428661,
13.7314027197448));
#166255=CARTESIAN_POINT('Ctrl Pts',(-18.3700981299812,-16.8665062575944,
13.7309197259417));
#166256=CARTESIAN_POINT('Ctrl Pts',(-18.3744736751895,-16.8657474881474,
13.7306524795444));
#166257=CARTESIAN_POINT('Ctrl Pts',(-18.3856620565777,-16.8638435397812,
13.7299714429248));
#166258=CARTESIAN_POINT('Ctrl Pts',(-18.3924782298691,-16.862717920271,
13.729558737507));
#166259=CARTESIAN_POINT('Ctrl Pts',(-18.4320757636264,-16.8563777646128,
13.7271732821514));
#166260=CARTESIAN_POINT('Ctrl Pts',(-18.4649725959688,-16.8519011144175,
13.7252395420557));
#166261=CARTESIAN_POINT('Ctrl Pts',(-18.5165060387728,-16.8461192945068,
13.722266216998));
#166262=CARTESIAN_POINT('Ctrl Pts',(-18.5350761803347,-16.8442840513349,
13.7212060535681));
#166263=CARTESIAN_POINT('Ctrl Pts',(-18.5848200668732,-16.8400312853727,
13.718390684282));
#166264=CARTESIAN_POINT('Ctrl Pts',(-18.616027717275,-16.838058379965,13.7166500582021));
#166265=CARTESIAN_POINT('Ctrl Pts',(-18.68572842501,-16.835200410613,13.712798128199));
#166266=CARTESIAN_POINT('Ctrl Pts',(-18.7242249885063,-16.8346726223255,
13.710694808877));
#166267=CARTESIAN_POINT('Ctrl Pts',(-18.8719904178439,-16.8366771173393,
13.7026494073521));
#166268=CARTESIAN_POINT('Ctrl Pts',(-18.9809856286892,-16.8466189272732,
13.6967644777885));
#166269=CARTESIAN_POINT('Ctrl Pts',(-19.1429758994154,-16.874151050549,
13.6876274890093));
#166270=CARTESIAN_POINT('Ctrl Pts',(-19.1968465613857,-16.8854836171478,
13.6845241836493));
#166271=CARTESIAN_POINT('Ctrl Pts',(-19.2834498582769,-16.9072583411936,
13.6793865221568));
#166272=CARTESIAN_POINT('Ctrl Pts',(-19.3164784167342,-16.9164208941806,
13.6773914262923));
#166273=CARTESIAN_POINT('Ctrl Pts',(-19.3596071847738,-16.9295209777438,
13.6747330844915));
#166274=CARTESIAN_POINT('Ctrl Pts',(-19.369921314309,-16.9327402790717,
13.6740933148737));
#166275=CARTESIAN_POINT('Ctrl Pts',(-19.3867783029255,-16.9381437340827,
13.6730408982627));
#166276=CARTESIAN_POINT('Ctrl Pts',(-19.3933360114689,-16.9402811839638,
13.6726297908862));
#166277=CARTESIAN_POINT('Ctrl Pts',(-19.4060125483478,-16.9444816737608,
13.6718317521141));
#166278=CARTESIAN_POINT('Ctrl Pts',(-19.4121326201157,-16.9465407400236,
13.6714449557201));
#166279=CARTESIAN_POINT('Ctrl Pts',(-19.4262461222219,-16.9513611456157,
13.6705494206052));
#166280=CARTESIAN_POINT('Ctrl Pts',(-19.4342325775575,-16.9541424341338,
13.670040025033));
#166281=CARTESIAN_POINT('Ctrl Pts',(-19.4556758312295,-16.9617544338049,
13.6686651159863));
#166282=CARTESIAN_POINT('Ctrl Pts',(-19.4691005306975,-16.9666736758996,
13.6677966704614));
#166283=CARTESIAN_POINT('Ctrl Pts',(-19.592328958455,-17.0132497568144,
13.6597527510237));
#166284=CARTESIAN_POINT('Ctrl Pts',(-19.6985201378396,-17.0638331403191,
13.6522722846333));
#166285=CARTESIAN_POINT('Ctrl Pts',(-19.9414515472103,-17.2054117586762,
13.6339020390175));
#166286=CARTESIAN_POINT('Ctrl Pts',(-20.072896412781,-17.3040113998141,
13.6228710079268));
#166287=CARTESIAN_POINT('Ctrl Pts',(-20.2141769117082,-17.4381541448046,
13.6105089692731));
#166288=CARTESIAN_POINT('Ctrl Pts',(-20.2362207830319,-17.4600261670342,
13.6085650322808));
#166289=CARTESIAN_POINT('Ctrl Pts',(-20.2627314468167,-17.4875137068112,
13.6062172177954));
#166290=CARTESIAN_POINT('Ctrl Pts',(-20.2676601593797,-17.4926760269561,
13.6057802891099));
#166291=CARTESIAN_POINT('Ctrl Pts',(-20.2753701286764,-17.5008336308648,
13.6050962575892));
#166292=CARTESIAN_POINT('Ctrl Pts',(-20.2781689266112,-17.5038121560977,
13.6048478328276));
#166293=CARTESIAN_POINT('Ctrl Pts',(-20.2833998779188,-17.5094114233512,
13.6043833447437));
#166294=CARTESIAN_POINT('Ctrl Pts',(-20.2858339899481,-17.5120301909328,
13.6041671343974));
#166295=CARTESIAN_POINT('Ctrl Pts',(-20.2913956841174,-17.5180442851251,
13.6036729353168));
#166296=CARTESIAN_POINT('Ctrl Pts',(-20.2945187977089,-17.5214436774273,
13.6033952874689));
#166297=CARTESIAN_POINT('Ctrl Pts',(-20.304155013997,-17.5320014459726,
13.6025380966028));
#166298=CARTESIAN_POINT('Ctrl Pts',(-20.3106302734806,-17.5391944046701,
13.6019613457059));
#166299=CARTESIAN_POINT('Ctrl Pts',(-20.3791745620288,-17.6163941059099,
13.5958449039933));
#166300=CARTESIAN_POINT('Ctrl Pts',(-20.4365950923684,-17.6904070118395,
13.5906201463139));
#166301=CARTESIAN_POINT('Ctrl Pts',(-20.5627799908811,-17.877437094088,
13.5782429302421));
#166302=CARTESIAN_POINT('Ctrl Pts',(-20.6262222119337,-17.993554852825,
13.5711935662999));
#166303=CARTESIAN_POINT('Ctrl Pts',(-20.6941947372831,-18.1514291345996,
13.5616457581666));
#166304=CARTESIAN_POINT('Ctrl Pts',(-20.708915345871,-18.1884649857798,
13.5594101580691));
#166305=CARTESIAN_POINT('Ctrl Pts',(-20.7225805759573,-18.2258896138153,
13.5571445817067));
#166306=CARTESIAN_POINT('',(-20.8509992001584,-18.9500893141201,14.0892704168218));
#166307=CARTESIAN_POINT('Ctrl Pts',(-20.7225805383928,-18.2258895109384,
13.3344632701429));
#166308=CARTESIAN_POINT('Ctrl Pts',(-20.7140997256968,-18.2026633224573,
13.3360898678322));
#166309=CARTESIAN_POINT('Ctrl Pts',(-20.7052099499586,-18.1795801024561,
13.3377116603475));
#166310=CARTESIAN_POINT('Ctrl Pts',(-20.6896738686132,-18.1412567374251,
13.3404079591312));
#166311=CARTESIAN_POINT('Ctrl Pts',(-20.683252173486,-18.1259365018981,
13.3414868503263));
#166312=CARTESIAN_POINT('Ctrl Pts',(-20.6554928164708,-18.0618377305783,
13.3460009999898));
#166313=CARTESIAN_POINT('Ctrl Pts',(-20.632497437654,-18.0137931890523,
13.3493852384935));
#166314=CARTESIAN_POINT('Ctrl Pts',(-20.6036571232171,-17.9589505700114,
13.3532075704532));
#166315=CARTESIAN_POINT('Ctrl Pts',(-20.5995537513667,-17.9512632036568,
13.3537423864081));
#166316=CARTESIAN_POINT('Ctrl Pts',(-20.5932681151595,-17.9396605497492,
13.3545478723295));
#166317=CARTESIAN_POINT('Ctrl Pts',(-20.5911207479857,-17.9357266042847,
13.3548206754776));
#166318=CARTESIAN_POINT('Ctrl Pts',(-20.5872434452906,-17.9286767698784,
13.3553089697548));
#166319=CARTESIAN_POINT('Ctrl Pts',(-20.58551812815,-17.9255584173787,13.3555247485522));
#166320=CARTESIAN_POINT('Ctrl Pts',(-20.5817516591871,-17.9187912673803,
13.3559925534721));
#166321=CARTESIAN_POINT('Ctrl Pts',(-20.5797075772965,-17.9151441667258,
13.3562443882116));
#166322=CARTESIAN_POINT('Ctrl Pts',(-20.5739344574349,-17.9049147964847,
13.356949999503));
#166323=CARTESIAN_POINT('Ctrl Pts',(-20.5701808785337,-17.8983463489839,
13.3574022278542));
#166324=CARTESIAN_POINT('Ctrl Pts',(-20.5475081236854,-17.8591600627494,
13.3600958701374));
#166325=CARTESIAN_POINT('Ctrl Pts',(-20.527754170794,-17.8270301275868,
13.3622866718655));
#166326=CARTESIAN_POINT('Ctrl Pts',(-20.4598647486886,-17.7229468928424,
13.3693824410159));
#166327=CARTESIAN_POINT('Ctrl Pts',(-20.4081729372359,-17.6534130691412,
13.3741229837252));
#166328=CARTESIAN_POINT('Ctrl Pts',(-20.2388248844504,-17.4525968152739,
13.388417610194));
#166329=CARTESIAN_POINT('Ctrl Pts',(-20.1089424673344,-17.3326685377626,
13.3978831132822));
#166330=CARTESIAN_POINT('Ctrl Pts',(-19.9470527295094,-17.2168577587889,
13.409450069178));
#166331=CARTESIAN_POINT('Ctrl Pts',(-19.9281750522112,-17.2038119649424,
13.4107944175979));
#166332=CARTESIAN_POINT('Ctrl Pts',(-19.9011552309914,-17.1857812551975,
13.4127141111369));
#166333=CARTESIAN_POINT('Ctrl Pts',(-19.8931852908434,-17.1805403067843,
13.4132798108868));
#166334=CARTESIAN_POINT('Ctrl Pts',(-19.8801738731756,-17.1721095427535,
13.4142025867968));
#166335=CARTESIAN_POINT('Ctrl Pts',(-19.875153795802,-17.1688868234034,
13.4145584298995));
#166336=CARTESIAN_POINT('Ctrl Pts',(-19.8646137410571,-17.1621832063159,
13.4153052021165));
#166337=CARTESIAN_POINT('Ctrl Pts',(-19.8590911632111,-17.1587065328271,
13.4156962828169));
#166338=CARTESIAN_POINT('Ctrl Pts',(-19.8459085946077,-17.150492466,13.4166293783693));
#166339=CARTESIAN_POINT('Ctrl Pts',(-19.8382343195216,-17.1457783409854,
13.4171722429262));
#166340=CARTESIAN_POINT('Ctrl Pts',(-19.8122484043422,-17.1300433176869,
13.4190094454509));
#166341=CARTESIAN_POINT('Ctrl Pts',(-19.7938004833726,-17.1192510655922,
13.4203120739224));
#166342=CARTESIAN_POINT('Ctrl Pts',(-19.6922725130606,-17.0619014722255,
13.4274744994076));
#166343=CARTESIAN_POINT('Ctrl Pts',(-19.6062972601117,-17.0207175467903,
13.4335233267607));
#166344=CARTESIAN_POINT('Ctrl Pts',(-19.3593949823414,-16.9223034938732,
13.4507948383493));
#166345=CARTESIAN_POINT('Ctrl Pts',(-19.1938957496031,-16.8785295908205,
13.4623043893491));
#166346=CARTESIAN_POINT('Ctrl Pts',(-18.9884991558451,-16.85003118873,13.4755393953443));
#166347=CARTESIAN_POINT('Ctrl Pts',(-18.9519273095244,-16.8459252698673,
13.4778537801019));
#166348=CARTESIAN_POINT('Ctrl Pts',(-18.9081486791395,-16.842162980718,
13.48055961979));
#166349=CARTESIAN_POINT('Ctrl Pts',(-18.9010295875812,-16.8415874501487,
13.4809975956011));
#166350=CARTESIAN_POINT('Ctrl Pts',(-18.8894080893929,-16.8407071052158,
13.4817090940777));
#166351=CARTESIAN_POINT('Ctrl Pts',(-18.8849074472827,-16.8403806439035,
13.4819837863723));
#166352=CARTESIAN_POINT('Ctrl Pts',(-18.8768483173873,-16.8398219595999,
13.4824741064647));
#166353=CARTESIAN_POINT('Ctrl Pts',(-18.8732902681027,-16.8395843358969,
13.482690032465));
#166354=CARTESIAN_POINT('Ctrl Pts',(-18.8655823031331,-16.8390891204712,
13.483156612986));
#166355=CARTESIAN_POINT('Ctrl Pts',(-18.861432237046,-16.8388347643941,
13.4834070844442));
#166356=CARTESIAN_POINT('Ctrl Pts',(-18.8498346670885,-16.8381582432594,
13.4841050351879));
#166357=CARTESIAN_POINT('Ctrl Pts',(-18.8423855569119,-16.8377632068639,
13.4845510198406));
#166358=CARTESIAN_POINT('Ctrl Pts',(-18.7990585884251,-16.8356951104398,
13.4871324249199));
#166359=CARTESIAN_POINT('Ctrl Pts',(-18.7631425826237,-16.8348958313183,
13.4892220156317));
#166360=CARTESIAN_POINT('Ctrl Pts',(-18.6474945266842,-16.8352661414381,
13.4958379844384));
#166361=CARTESIAN_POINT('Ctrl Pts',(-18.5678392824195,-16.8400250888151,
13.5002243290217));
#166362=CARTESIAN_POINT('Ctrl Pts',(-18.3036786030416,-16.8708493772849,
13.5147244717422));
#166363=CARTESIAN_POINT('Ctrl Pts',(-18.1223976098282,-16.9167356492839,
13.5246809892134));
#166364=CARTESIAN_POINT('Ctrl Pts',(-17.9289806596003,-16.9939093609115,
13.536793282158));
#166365=CARTESIAN_POINT('Ctrl Pts',(-17.9086325759213,-17.00239910476,13.5380857651937));
#166366=CARTESIAN_POINT('Ctrl Pts',(-17.8806750307968,-17.014579835793,
13.5398884657194));
#166367=CARTESIAN_POINT('Ctrl Pts',(-17.872949080915,-17.0180011097885,
13.540389504952));
#166368=CARTESIAN_POINT('Ctrl Pts',(-17.8597034874644,-17.0239617429605,
13.5412535359755));
#166369=CARTESIAN_POINT('Ctrl Pts',(-17.8541738747296,-17.0264787976894,
13.5416157596264));
#166370=CARTESIAN_POINT('Ctrl Pts',(-17.8427959661267,-17.0317172140661,
13.5423642541021));
#166371=CARTESIAN_POINT('Ctrl Pts',(-17.8369491255737,-17.0344415692843,
13.5427506253296));
#166372=CARTESIAN_POINT('Ctrl Pts',(-17.8233709213203,-17.0408440714321,
13.543651996248));
#166373=CARTESIAN_POINT('Ctrl Pts',(-17.8156492787915,-17.0445424639774,
13.5441676942268));
#166374=CARTESIAN_POINT('Ctrl Pts',(-17.7910017922441,-17.0565320876256,
13.545823899905));
#166375=CARTESIAN_POINT('Ctrl Pts',(-17.7741645187312,-17.0650023742698,
13.5469706326529));
#166376=CARTESIAN_POINT('Ctrl Pts',(-17.6906014235813,-17.1084480205814,
13.552740523411));
#166377=CARTESIAN_POINT('Ctrl Pts',(-17.6256697793026,-17.1467392315843,
13.557480085036));
#166378=CARTESIAN_POINT('Ctrl Pts',(-17.4719788015028,-17.2487944783576,
13.5693359018199));
#166379=CARTESIAN_POINT('Ctrl Pts',(-17.3858489648803,-17.3161235165715,
13.5765519881518));
#166380=CARTESIAN_POINT('Ctrl Pts',(-17.2943894784147,-17.3997663762781,
13.5847394763276));
#166381=CARTESIAN_POINT('Ctrl Pts',(-17.2835818943926,-17.4098602531417,
13.5857158257668));
#166382=CARTESIAN_POINT('Ctrl Pts',(-17.1976226427082,-17.491845998022,
13.5935486530659));
#166383=CARTESIAN_POINT('Ctrl Pts',(-17.1277466129228,-17.5690826875177,
13.6003416506233));
#166384=CARTESIAN_POINT('Ctrl Pts',(-17.057872973444,-17.6587942808735,
13.6073672271781));
#166385=CARTESIAN_POINT('Ctrl Pts',(-17.051972828847,-17.666477754054,13.6079624323683));
#166386=CARTESIAN_POINT('Ctrl Pts',(-17.0433381408901,-17.6778835202656,
13.608836086388));
#166387=CARTESIAN_POINT('Ctrl Pts',(-17.0405627996145,-17.681574569263,
13.6091172961327));
#166388=CARTESIAN_POINT('Ctrl Pts',(-17.0356600964017,-17.6881395029313,
13.6096147313358));
#166389=CARTESIAN_POINT('Ctrl Pts',(-17.0335279172941,-17.6910097221541,
13.6098312911786));
#166390=CARTESIAN_POINT('Ctrl Pts',(-17.0289747128538,-17.6971715394593,
13.610294224304));
#166391=CARTESIAN_POINT('Ctrl Pts',(-17.0265559489038,-17.7004647395233,
13.6105404410541));
#166392=CARTESIAN_POINT('Ctrl Pts',(-17.0199414904071,-17.7095253356414,
13.6112146353298));
#166393=CARTESIAN_POINT('Ctrl Pts',(-17.0157653378792,-17.7153070247375,
13.6116412789131));
#166394=CARTESIAN_POINT('Ctrl Pts',(-16.9936078185478,-17.7463119862559,
13.6139108475841));
#166395=CARTESIAN_POINT('Ctrl Pts',(-16.9761514530323,-17.7719079502791,
13.6157199200887));
#166396=CARTESIAN_POINT('Ctrl Pts',(-16.8701129766784,-17.9349675839643,
13.6269072190229));
#166397=CARTESIAN_POINT('Ctrl Pts',(-16.7971380216548,-18.0819380516337,
13.6355501683147));
#166398=CARTESIAN_POINT('Ctrl Pts',(-16.7019803899064,-18.3466517233322,
13.6509452032218));
#166399=CARTESIAN_POINT('Ctrl Pts',(-16.6714699089154,-18.4605587446626,
13.6575148200393));
#166400=CARTESIAN_POINT('Ctrl Pts',(-16.6480483140075,-18.5904767082956,
13.6652484282959));
#166401=CARTESIAN_POINT('Ctrl Pts',(-16.6456537143955,-18.6045761908023,
13.6660905974197));
#166402=CARTESIAN_POINT('Ctrl Pts',(-16.6420705639612,-18.6270511232341,
13.6674380376078));
#166403=CARTESIAN_POINT('Ctrl Pts',(-16.6407890146802,-18.6354114568612,
13.6679403615201));
#166404=CARTESIAN_POINT('Ctrl Pts',(-16.6386174640658,-18.6501677191829,
13.6688289991286));
#166405=CARTESIAN_POINT('Ctrl Pts',(-16.6377065577357,-18.6565604966579,
13.669214645714));
#166406=CARTESIAN_POINT('Ctrl Pts',(-16.6358832671285,-18.6697895436354,
13.6700141118039));
#166407=CARTESIAN_POINT('Ctrl Pts',(-16.6349750148609,-18.6766262967393,
13.670428057106));
#166408=CARTESIAN_POINT('Ctrl Pts',(-16.6327298982582,-18.6941828921962,
13.6714931194885));
#166409=CARTESIAN_POINT('Ctrl Pts',(-16.6314416628657,-18.7049086530796,
13.67214576359));
#166410=CARTESIAN_POINT('Ctrl Pts',(-16.6264111340294,-18.7496844652818,
13.6748788036134));
#166411=CARTESIAN_POINT('Ctrl Pts',(-16.6234136393663,-18.7838114079327,
13.6769824664931));
#166412=CARTESIAN_POINT('Ctrl Pts',(-16.6177643956782,-18.8728784215353,
13.6825295580915));
#166413=CARTESIAN_POINT('Ctrl Pts',(-16.6164234538964,-18.9278729967481,
13.6860112451016));
#166414=CARTESIAN_POINT('Ctrl Pts',(-16.6188178731786,-19.0921455464016,
13.6965704085244));
#166415=CARTESIAN_POINT('Ctrl Pts',(-16.6288727173682,-19.2011422472975,
13.7037963099291));
#166416=CARTESIAN_POINT('Ctrl Pts',(-16.6537814520219,-19.3467913599842,
13.7135573676062));
#166417=CARTESIAN_POINT('Ctrl Pts',(-16.661300308591,-19.3845338322806,
13.7160951787984));
#166418=CARTESIAN_POINT('Ctrl Pts',(-16.6768194325393,-19.4526836670681,
13.7206740430664));
#166419=CARTESIAN_POINT('Ctrl Pts',(-16.684476396842,-19.4831583106033,
13.7227202264793));
#166420=CARTESIAN_POINT('Ctrl Pts',(-16.7060867296695,-19.5617238918079,
13.7279748925652));
#166421=CARTESIAN_POINT('Ctrl Pts',(-16.7210737955619,-19.6095138226699,
13.7311511391529));
#166422=CARTESIAN_POINT('Ctrl Pts',(-16.7403469552473,-19.6641079525071,
13.7347216404907));
#166423=CARTESIAN_POINT('Ctrl Pts',(-16.7429920707199,-19.6714703807263,
13.7352019041542));
#166424=CARTESIAN_POINT('Ctrl Pts',(-16.7472801112778,-19.6832009710555,
13.7359649258532));
#166425=CARTESIAN_POINT('Ctrl Pts',(-16.7488967439463,-19.687578575057,
13.7362491812701));
#166426=CARTESIAN_POINT('Ctrl Pts',(-16.751782949525,-19.6953151813461,
13.7367506401667));
#166427=CARTESIAN_POINT('Ctrl Pts',(-16.7530466100361,-19.6986763432342,
13.7369681921469));
#166428=CARTESIAN_POINT('Ctrl Pts',(-16.7557401372558,-19.7057857844427,
13.7374276888843));
#166429=CARTESIAN_POINT('Ctrl Pts',(-16.7571721049696,-19.7095332120891,
13.7376695057031));
#166430=CARTESIAN_POINT('Ctrl Pts',(-16.7610588300651,-19.7196186129533,
13.7383193191846));
#166431=CARTESIAN_POINT('Ctrl Pts',(-16.763533495767,-19.725948934708,13.7387261384488));
#166432=CARTESIAN_POINT('Ctrl Pts',(-16.7758761031225,-19.7570790019163,
13.7407220475595));
#166433=CARTESIAN_POINT('Ctrl Pts',(-16.786182434969,-19.7817037289964,
13.7422862252088));
#166434=CARTESIAN_POINT('Ctrl Pts',(-16.8171977959429,-19.8520423900543,
13.7467298369642));
#166435=CARTESIAN_POINT('Ctrl Pts',(-16.8390708079562,-19.8972253809776,
13.7495542946331));
#166436=CARTESIAN_POINT('Ctrl Pts',(-16.9239141563581,-20.0576772663545,
13.75962114507));
#166437=CARTESIAN_POINT('Ctrl Pts',(-16.9959669729675,-20.1678028703928,
13.7666181239493));
#166438=CARTESIAN_POINT('Ctrl Pts',(-17.1431422403223,-20.3526712097384,
13.7796117497776));
#166439=CARTESIAN_POINT('Ctrl Pts',(-17.2145324694088,-20.4298100472926,
13.7855061735589));
#166440=CARTESIAN_POINT('Ctrl Pts',(-17.3016464824971,-20.5109261136325,
13.7924814135577));
#166441=CARTESIAN_POINT('Ctrl Pts',(-17.3120457229041,-20.5204174337361,
13.7933106888672));
#166442=CARTESIAN_POINT('Ctrl Pts',(-17.3287943748239,-20.535400329009,
13.7946413429502));
#166443=CARTESIAN_POINT('Ctrl Pts',(-17.3350832267281,-20.5409591905696,
13.7951398896436));
#166444=CARTESIAN_POINT('Ctrl Pts',(-17.3462606078872,-20.5507213461684,
13.7960241368025));
#166445=CARTESIAN_POINT('Ctrl Pts',(-17.3511356189083,-20.5549400067391,
13.7964091912981));
#166446=CARTESIAN_POINT('Ctrl Pts',(-17.3612859311094,-20.5636429574033,
13.7972096990382));
#166447=CARTESIAN_POINT('Ctrl Pts',(-17.3665641072611,-20.5681237621406,
13.7976252892904));
#166448=CARTESIAN_POINT('Ctrl Pts',(-17.3802271697713,-20.5796079000919,
13.7986994085144));
#166449=CARTESIAN_POINT('Ctrl Pts',(-17.3886443803018,-20.5865722993634,
13.7993595149462));
#166450=CARTESIAN_POINT('Ctrl Pts',(-17.4245097909862,-20.6157826391659,
13.8021657360717));
#166451=CARTESIAN_POINT('Ctrl Pts',(-17.4524574314345,-20.6374037162345,
13.8043367044642));
#166452=CARTESIAN_POINT('Ctrl Pts',(-17.5271912972352,-20.6922861205314,
13.8101050116233));
#166453=CARTESIAN_POINT('Ctrl Pts',(-17.5748096560177,-20.7243599670701,
13.8137445222459));
#166454=CARTESIAN_POINT('Ctrl Pts',(-17.7245790189376,-20.8166193140851,
13.8250717711392));
#166455=CARTESIAN_POINT('Ctrl Pts',(-17.8305251155659,-20.8701931868951,
13.8329351818468));
#166456=CARTESIAN_POINT('Ctrl Pts',(-18.0381718596145,-20.9541582639182,
13.8477080786132));
#166457=CARTESIAN_POINT('Ctrl Pts',(-18.1387881851723,-20.9863408508938,
13.854602481805));
#166458=CARTESIAN_POINT('Ctrl Pts',(-18.2508144784688,-21.0131439931278,
13.8617192156344));
#166459=CARTESIAN_POINT('Ctrl Pts',(-18.260249668403,-21.0153330899585,
13.8623143164452));
#166460=CARTESIAN_POINT('Ctrl Pts',(-18.2742049855909,-21.0184701467707,
13.8631878470701));
#166461=CARTESIAN_POINT('Ctrl Pts',(-18.2787135688655,-21.0194681592053,
13.8634690366977));
#166462=CARTESIAN_POINT('Ctrl Pts',(-18.2867189020335,-21.021212749662,
13.8639664496666));
#166463=CARTESIAN_POINT('Ctrl Pts',(-18.2902143102526,-21.0219652282625,
13.864183007281));
#166464=CARTESIAN_POINT('Ctrl Pts',(-18.2977085174992,-21.0235586979776,
13.864645950415));
#166465=CARTESIAN_POINT('Ctrl Pts',(-18.3017078387464,-21.0243969660365,
13.8648921793249));
#166466=CARTESIAN_POINT('Ctrl Pts',(-18.3126950647206,-21.0266667276134,
13.8655664412073));
#166467=CARTESIAN_POINT('Ctrl Pts',(-18.3196878905484,-21.028074506952,
13.8659931397916));
#166468=CARTESIAN_POINT('Ctrl Pts',(-18.357098027051,-21.0354092813369,
13.8682635270551));
#166469=CARTESIAN_POINT('Ctrl Pts',(-18.3876373215015,-21.0407035342838,
13.8700733342172));
#166470=CARTESIAN_POINT('Ctrl Pts',(-18.5800207910995,-21.0697189021429,
13.8812635286908));
#166471=CARTESIAN_POINT('Ctrl Pts',(-18.7440573512384,-21.0752885214934,
13.8899084050625));
#166472=CARTESIAN_POINT('Ctrl Pts',(-19.0243994562741,-21.052287063675,
13.9053029776013));
#166473=CARTESIAN_POINT('Ctrl Pts',(-19.1406631071423,-21.0329030176184,
13.911869773093));
#166474=CARTESIAN_POINT('Ctrl Pts',(-19.2685672101117,-21.0004460955248,
13.9196002060546));
#166475=CARTESIAN_POINT('Ctrl Pts',(-19.2823922637549,-20.9967883554316,
13.9204423379327));
#166476=CARTESIAN_POINT('Ctrl Pts',(-19.3043331006423,-20.9907448808141,
13.921789729658));
#166477=CARTESIAN_POINT('Ctrl Pts',(-19.3124736254387,-20.9884500475678,
13.9222920426886));
#166478=CARTESIAN_POINT('Ctrl Pts',(-19.3268045873397,-20.9843172534022,
13.923180667619));
#166479=CARTESIAN_POINT('Ctrl Pts',(-19.3330008107649,-20.9824996243596,
13.9235663124689));
#166480=CARTESIAN_POINT('Ctrl Pts',(-19.3457976655777,-20.9786820628479,
13.9243657814118));
#166481=CARTESIAN_POINT('Ctrl Pts',(-19.3523970261013,-20.9766781679649,
13.9247797313342));
#166482=CARTESIAN_POINT('Ctrl Pts',(-19.369308094027,-20.9714527314666,
13.9258448191825));
#166483=CARTESIAN_POINT('Ctrl Pts',(-19.3796050536432,-20.9681844699579,
13.9264974842708));
#166484=CARTESIAN_POINT('Ctrl Pts',(-19.421801582802,-20.9544348719619,
13.9291894395693));
#166485=CARTESIAN_POINT('Ctrl Pts',(-19.4534732108165,-20.9432745992925,
13.9312509841543));
#166486=CARTESIAN_POINT('Ctrl Pts',(-19.5351606113183,-20.9122868117059,
13.9366788028705));
#166487=CARTESIAN_POINT('Ctrl Pts',(-19.5847073637069,-20.8912985648005,
13.940081644078));
#166488=CARTESIAN_POINT('Ctrl Pts',(-19.7590211255306,-20.8094922872943,
13.9524453325196));
#166489=CARTESIAN_POINT('Ctrl Pts',(-19.8785357599393,-20.7383307517078,
13.9616908974154));
#166490=CARTESIAN_POINT('Ctrl Pts',(-20.0633780619625,-20.6020621379154,
13.9767881809416));
#166491=CARTESIAN_POINT('Ctrl Pts',(-20.1330007581972,-20.5434621715121,
13.9826868325319));
#166492=CARTESIAN_POINT('Ctrl Pts',(-20.2056220821844,-20.4738773840299,
13.9889006167982));
#166493=CARTESIAN_POINT('Ctrl Pts',(-20.2125516650544,-20.4671459687698,
13.9894941620132));
#166494=CARTESIAN_POINT('Ctrl Pts',(-20.2227217037495,-20.4571305480552,
13.9903658533879));
#166495=CARTESIAN_POINT('Ctrl Pts',(-20.2259977809915,-20.4538831180721,
13.9906467429663));
#166496=CARTESIAN_POINT('Ctrl Pts',(-20.2317939704682,-20.448099930615,
13.9911438244957));
#166497=CARTESIAN_POINT('Ctrl Pts',(-20.2343182970572,-20.4455684746767,
13.9913603490581));
#166498=CARTESIAN_POINT('Ctrl Pts',(-20.2397163708351,-20.4401276600474,
13.9918234423276));
#166499=CARTESIAN_POINT('Ctrl Pts',(-20.24258809648,-20.4372163740709,13.99206985327));
#166500=CARTESIAN_POINT('Ctrl Pts',(-20.2484649752047,-20.431223905618,
13.9925742727638));
#166501=CARTESIAN_POINT('Ctrl Pts',(-20.2514692059129,-20.4281418407161,
13.9928322099775));
#166502=CARTESIAN_POINT('Ctrl Pts',(-20.2652664701271,-20.4139004805739,
13.9940173096999));
#166503=CARTESIAN_POINT('Ctrl Pts',(-20.2759462702773,-20.4026315000053,
13.9949360391927));
#166504=CARTESIAN_POINT('Ctrl Pts',(-20.3410495727756,-20.3324051484403,
14.0005529595109));
#166505=CARTESIAN_POINT('Ctrl Pts',(-20.3922144945842,-20.2705045048262,
14.0050403501236));
#166506=CARTESIAN_POINT('Ctrl Pts',(-20.4809416628919,-20.1497987291867,
14.0132760841966));
#166507=CARTESIAN_POINT('Ctrl Pts',(-20.5193512764045,-20.0917579492557,
14.0170382609235));
#166508=CARTESIAN_POINT('Ctrl Pts',(-20.6313102103813,-19.9029877845586,
14.0289663785397));
#166509=CARTESIAN_POINT('Ctrl Pts',(-20.6938625764002,-19.7663059930405,
14.0371981153533));
#166510=CARTESIAN_POINT('Ctrl Pts',(-20.745951996354,-19.6107403493133,
14.0468105577194));
#166511=CARTESIAN_POINT('Ctrl Pts',(-20.7503149306902,-19.5972625583361,
14.0476448853232));
#166512=CARTESIAN_POINT('Ctrl Pts',(-20.7570544852589,-19.5757070035014,
14.0489821190155));
#166513=CARTESIAN_POINT('Ctrl Pts',(-20.7595187964723,-19.5676569487601,
14.0494821481899));
#166514=CARTESIAN_POINT('Ctrl Pts',(-20.7637864757215,-19.5534129017074,
14.0503681159981));
#166515=CARTESIAN_POINT('Ctrl Pts',(-20.7656096812489,-19.5472249297501,
14.0507534003742));
#166516=CARTESIAN_POINT('Ctrl Pts',(-20.7693280076272,-19.5343887795456,
14.0515534868461));
#166517=CARTESIAN_POINT('Ctrl Pts',(-20.7712189019553,-19.5277394661866,
14.0519684215081));
#166518=CARTESIAN_POINT('Ctrl Pts',(-20.7760008784298,-19.5106051428325,
14.0530389334059));
#166519=CARTESIAN_POINT('Ctrl Pts',(-20.7788437611398,-19.5001069956869,
14.0536960679433));
#166520=CARTESIAN_POINT('Ctrl Pts',(-20.7848190503623,-19.4773478463147,
14.0551235064335));
#166521=CARTESIAN_POINT('Ctrl Pts',(-20.7879226529658,-19.4650797810014,
14.0558947147319));
#166522=CARTESIAN_POINT('Ctrl Pts',(-20.7966336980483,-19.4293001665496,
14.0581493044168));
#166523=CARTESIAN_POINT('Ctrl Pts',(-20.8019485533546,-19.4057200974013,
14.0596419062654));
#166524=CARTESIAN_POINT('Ctrl Pts',(-20.8363441713581,-19.2399337326738,
14.0701853145707));
#166525=CARTESIAN_POINT('Ctrl Pts',(-20.8511300498368,-19.0951834122695,
14.0796830572144));
#166526=CARTESIAN_POINT('Ctrl Pts',(-20.8509991383111,-18.9500899240172,
14.0892704847094));
#166527=CARTESIAN_POINT('Ctrl Pts',(-20.8509991377672,-18.9500893212942,
14.0892705245358));
#166528=CARTESIAN_POINT('Ctrl Pts',(-20.8508884780097,-18.8274802136491,
14.0973722384938));
#166529=CARTESIAN_POINT('Ctrl Pts',(-20.8401264223167,-18.7050980350981,
14.1054939319305));
#166530=CARTESIAN_POINT('Ctrl Pts',(-20.8166444854234,-18.5719488868771,
14.1139585516479));
#166531=CARTESIAN_POINT('Ctrl Pts',(-20.8143518751223,-18.5595933316814,
14.1147402926256));
#166532=CARTESIAN_POINT('Ctrl Pts',(-20.8106712434454,-18.5406969048476,
14.115929398801));
#166533=CARTESIAN_POINT('Ctrl Pts',(-20.8093620674484,-18.5341411947832,
14.1163407347543));
#166534=CARTESIAN_POINT('Ctrl Pts',(-20.8071513237826,-18.5233376109753,
14.1170164988066));
#166535=CARTESIAN_POINT('Ctrl Pts',(-20.8062677119474,-18.5190861681048,
14.1172818880159));
#166536=CARTESIAN_POINT('Ctrl Pts',(-20.8045210241027,-18.5108099824553,
14.1177974250332));
#166537=CARTESIAN_POINT('Ctrl Pts',(-20.8036592788867,-18.5067849813663,
14.1180476457386));
#166538=CARTESIAN_POINT('Ctrl Pts',(-20.8020280137088,-18.4992728345161,
14.1185136771087));
#166539=CARTESIAN_POINT('Ctrl Pts',(-20.8012614184,-18.4957851601687,14.1187296456484));
#166540=CARTESIAN_POINT('Ctrl Pts',(-20.7994932703445,-18.4878368284238,
14.119220944986));
#166541=CARTESIAN_POINT('Ctrl Pts',(-20.7984860931811,-18.483377474242,
14.1194959498741));
#166542=CARTESIAN_POINT('Ctrl Pts',(-20.7953527021747,-18.4697103149334,
14.1203369411167));
#166543=CARTESIAN_POINT('Ctrl Pts',(-20.7931792404185,-18.4605133100409,
14.1209002854826));
#166544=CARTESIAN_POINT('Ctrl Pts',(-20.7723521633478,-18.3749475295864,
14.1261199678598));
#166545=CARTESIAN_POINT('Ctrl Pts',(-20.7495260400938,-18.299684482012,
14.1305523345105));
#166546=CARTESIAN_POINT('Ctrl Pts',(-20.7225805482453,-18.2258895379212,
14.1348940720942));
#166547=CARTESIAN_POINT('Origin',(-18.734,-18.952,0.));
#166548=CARTESIAN_POINT('',(-20.7225805737622,-18.2258896078036,15.1555945473776));
#166549=CARTESIAN_POINT('',(-20.7225805503655,-18.2258895437275,14.9318514930297));
#166550=CARTESIAN_POINT('',(-20.7225805737622,-18.2258896078036,0.));
#166551=CARTESIAN_POINT('',(-20.8523539179813,-18.9502594238256,15.1109429533473));
#166552=CARTESIAN_POINT('Ctrl Pts',(-20.8509992748742,-18.9502478064743,
15.1109437209775));
#166553=CARTESIAN_POINT('Ctrl Pts',(-20.8509006165464,-18.8310488678702,
15.1181312937192));
#166554=CARTESIAN_POINT('Ctrl Pts',(-20.8407310772906,-18.7122546433193,
15.1253188664609));
#166555=CARTESIAN_POINT('Ctrl Pts',(-20.8207141748805,-18.5951905938,15.1325064392026));
#166556=CARTESIAN_POINT('Ctrl Pts',(-20.8084963315187,-18.5237374692842,
15.1368935634494));
#166557=CARTESIAN_POINT('Ctrl Pts',(-20.7925803619145,-18.4527731734038,
15.1412806876962));
#166558=CARTESIAN_POINT('Ctrl Pts',(-20.7730188005911,-18.3827098008609,
15.1456678119431));
#166559=CARTESIAN_POINT('Ctrl Pts',(-20.7582648347418,-18.3298657262649,
15.1489767237546));
#166560=CARTESIAN_POINT('Ctrl Pts',(-20.7414380855554,-18.277534208989,
15.1522856355661));
#166561=CARTESIAN_POINT('Ctrl Pts',(-20.7225805737622,-18.2258896078036,
15.1555945473776));
#166562=CARTESIAN_POINT('Ctrl Pts',(-20.7249097977618,-18.2250590878524,
14.355439975907));
#166563=CARTESIAN_POINT('Ctrl Pts',(-20.6989344912625,-18.1521456629184,
14.360110516976));
#166564=CARTESIAN_POINT('Ctrl Pts',(-20.3954318177898,-17.4332648257454,
14.4071729936054));
#166565=CARTESIAN_POINT('Ctrl Pts',(-19.0148744663066,-16.4645435790994,
14.4966274057954));
#166566=CARTESIAN_POINT('Ctrl Pts',(-16.7944748199427,-17.3694160408942,
14.6238032124768));
#166567=CARTESIAN_POINT('Ctrl Pts',(-16.3534691457724,-19.7262110589277,
14.7509790191583));
#166568=CARTESIAN_POINT('Ctrl Pts',(-18.0964527779473,-21.3727154833541,
14.8781548258396));
#166569=CARTESIAN_POINT('Ctrl Pts',(-20.2927765759232,-20.8308253929522,
14.9981428039027));
#166570=CARTESIAN_POINT('Ctrl Pts',(-20.8471439650915,-19.534463852321,
15.0757388464053));
#166571=CARTESIAN_POINT('Ctrl Pts',(-20.8523539179813,-18.9502594238256,
15.1109429533473));
#166572=CARTESIAN_POINT('Ctrl Pts',(-20.7225805482453,-18.2258895379212,
14.1348940720942));
#166573=CARTESIAN_POINT('Ctrl Pts',(-20.707502733624,-18.1845963044093,
14.1373235662296));
#166574=CARTESIAN_POINT('Ctrl Pts',(-20.6911350897703,-18.1437627423971,
14.1397244927296));
#166575=CARTESIAN_POINT('Ctrl Pts',(-20.6449227773403,-18.0381371044714,
14.1459967299859));
#166576=CARTESIAN_POINT('Ctrl Pts',(-20.6130671130522,-17.9743099162901,
14.1498507562372));
#166577=CARTESIAN_POINT('Ctrl Pts',(-20.5342706048791,-17.8345651178331,
14.1586406107144));
#166578=CARTESIAN_POINT('Ctrl Pts',(-20.4856320614129,-17.7597677103411,
14.1635989258829));
#166579=CARTESIAN_POINT('Ctrl Pts',(-20.4120582786952,-17.6608866196624,
14.1706898593858));
#166580=CARTESIAN_POINT('Ctrl Pts',(-20.3910309374818,-17.6340084877275,
14.1726761120272));
#166581=CARTESIAN_POINT('Ctrl Pts',(-20.3624525439932,-17.5992436398234,
14.1753299557445));
#166582=CARTESIAN_POINT('Ctrl Pts',(-20.3554763928526,-17.5908895126539,
14.1759743426739));
#166583=CARTESIAN_POINT('Ctrl Pts',(-20.3439634012343,-17.5773165241001,
14.1770324207133));
#166584=CARTESIAN_POINT('Ctrl Pts',(-20.3394648061884,-17.5720653759787,
14.1774445395521));
#166585=CARTESIAN_POINT('Ctrl Pts',(-20.3307201063842,-17.561958450634,
14.1782431677588));
#166586=CARTESIAN_POINT('Ctrl Pts',(-20.3264773709349,-17.5570998499078,
14.1786295348415));
#166587=CARTESIAN_POINT('Ctrl Pts',(-20.316648725643,-17.5459477887591,
14.1795220849354));
#166588=CARTESIAN_POINT('Ctrl Pts',(-20.3110473916266,-17.5396681229666,
14.1800289110287));
#166589=CARTESIAN_POINT('Ctrl Pts',(-20.2959253366837,-17.5229168888778,
14.1813924050948));
#166590=CARTESIAN_POINT('Ctrl Pts',(-20.2863369245266,-17.512507258319,
14.1822519298717));
#166591=CARTESIAN_POINT('Ctrl Pts',(-20.2021839445793,-17.4229654550481,
14.1897536291562));
#166592=CARTESIAN_POINT('Ctrl Pts',(-20.1217415373617,-17.3496024822226,
14.1966553495631));
#166593=CARTESIAN_POINT('Ctrl Pts',(-19.9590042495324,-17.2226657405498,
14.2100939977286));
#166594=CARTESIAN_POINT('Ctrl Pts',(-19.8779113499631,-17.1679882900035,
14.2165787219792));
#166595=CARTESIAN_POINT('Ctrl Pts',(-19.7310865022736,-17.0831294331119,
14.2277562426462));
#166596=CARTESIAN_POINT('Ctrl Pts',(-19.66703816724,-17.0503428538897,14.2324611436209));
#166597=CARTESIAN_POINT('Ctrl Pts',(-19.570731222272,-17.0070827054999,
14.2391772890039));
#166598=CARTESIAN_POINT('Ctrl Pts',(-19.5396941270583,-16.9940215296004,
14.241289168206));
#166599=CARTESIAN_POINT('Ctrl Pts',(-19.5015759896546,-16.9790405019908,
14.243808284867));
#166600=CARTESIAN_POINT('Ctrl Pts',(-19.4947814012484,-16.9764105325894,
14.244254473837));
#166601=CARTESIAN_POINT('Ctrl Pts',(-19.4840930400149,-16.9723367269592,
14.2449517481225));
#166602=CARTESIAN_POINT('Ctrl Pts',(-19.4802084401077,-16.9708692097942,
14.2452042145345));
#166603=CARTESIAN_POINT('Ctrl Pts',(-19.472979405025,-16.9681625169269,
14.2456722388445));
#166604=CARTESIAN_POINT('Ctrl Pts',(-19.4696361888589,-16.9669203748444,
14.2458879680286));
#166605=CARTESIAN_POINT('Ctrl Pts',(-19.4620491211678,-16.9641232672844,
14.2463759290164));
#166606=CARTESIAN_POINT('Ctrl Pts',(-19.4578034301438,-16.9625734437562,
14.2466478524034));
#166607=CARTESIAN_POINT('Ctrl Pts',(-19.4451918054621,-16.958015483434,
14.2474523079116));
#166608=CARTESIAN_POINT('Ctrl Pts',(-19.4368117305669,-16.9550463916004,
14.2479825740317));
#166609=CARTESIAN_POINT('Ctrl Pts',(-19.3737813934032,-16.9331604238273,
14.2519407069241));
#166610=CARTESIAN_POINT('Ctrl Pts',(-19.3183900465949,-16.9164354574461,
14.2552492223628));
#166611=CARTESIAN_POINT('Ctrl Pts',(-19.1043468997635,-16.8612668298124,
14.2676350961639));
#166612=CARTESIAN_POINT('Ctrl Pts',(-18.9421302667622,-16.8389429270101,
14.276240860935));
#166613=CARTESIAN_POINT('Ctrl Pts',(-18.7188998916316,-16.8342019031165,
14.2886086156895));
#166614=CARTESIAN_POINT('Ctrl Pts',(-18.658825349921,-16.835482869544,14.291983310044));
#166615=CARTESIAN_POINT('Ctrl Pts',(-18.5747475981794,-16.8408598127308,
14.2968212630423));
#166616=CARTESIAN_POINT('Ctrl Pts',(-18.550634613922,-16.8428173892078,
14.2982219233524));
#166617=CARTESIAN_POINT('Ctrl Pts',(-18.5085797231295,-16.8469581560757,
14.3006907659365));
#166618=CARTESIAN_POINT('Ctrl Pts',(-18.4906221402878,-16.8489587133596,
14.3017532747122));
#166619=CARTESIAN_POINT('Ctrl Pts',(-18.4642216584597,-16.8522425101154,
14.3033284126285));
#166620=CARTESIAN_POINT('Ctrl Pts',(-18.4557570975741,-16.8533473956169,
14.303835420355));
#166621=CARTESIAN_POINT('Ctrl Pts',(-18.4409124051437,-16.8553764716857,
14.3047281587992));
#166622=CARTESIAN_POINT('Ctrl Pts',(-18.4345293426919,-16.8562786726924,
14.3051131896441));
#166623=CARTESIAN_POINT('Ctrl Pts',(-18.4221313181258,-16.8580888440937,
14.305863346691));
#166624=CARTESIAN_POINT('Ctrl Pts',(-18.4161159470959,-16.8589936141352,
14.3062283679213));
#166625=CARTESIAN_POINT('Ctrl Pts',(-18.4017264520659,-16.8612213973453,
14.3071041035565));
#166626=CARTESIAN_POINT('Ctrl Pts',(-18.3933562611894,-16.8625688056523,
14.3076155877192));
#166627=CARTESIAN_POINT('Ctrl Pts',(-18.3630693681826,-16.8676311250196,
14.3094740220012));
#166628=CARTESIAN_POINT('Ctrl Pts',(-18.3412040226162,-16.8716407998544,
14.310830291111));
#166629=CARTESIAN_POINT('Ctrl Pts',(-18.1386086613959,-16.9121005653244,
14.3235370765305));
#166630=CARTESIAN_POINT('Ctrl Pts',(-17.9633343551751,-16.9716646897236,
14.3356748925132));
#166631=CARTESIAN_POINT('Ctrl Pts',(-17.7254086641247,-17.0889412809956,
14.3531899125361));
#166632=CARTESIAN_POINT('Ctrl Pts',(-17.6548952835398,-17.1288765738331,
14.3585115566974));
#166633=CARTESIAN_POINT('Ctrl Pts',(-17.5563731920112,-17.1923983100319,
14.3659856297798));
#166634=CARTESIAN_POINT('Ctrl Pts',(-17.5264146902734,-17.2128217198054,
14.3682634042163));
#166635=CARTESIAN_POINT('Ctrl Pts',(-17.4909237354192,-17.2383762537897,
14.3709540780363));
#166636=CARTESIAN_POINT('Ctrl Pts',(-17.4848770368072,-17.2427788996733,
14.3714122151689));
#166637=CARTESIAN_POINT('Ctrl Pts',(-17.4755019515319,-17.2496812913505,
14.3721219291204));
#166638=CARTESIAN_POINT('Ctrl Pts',(-17.4721574585316,-17.2521589118258,
14.3723749938538));
#166639=CARTESIAN_POINT('Ctrl Pts',(-17.4659614929848,-17.2567772836794,
14.3728435600627));
#166640=CARTESIAN_POINT('Ctrl Pts',(-17.463108148362,-17.2589153550628,
14.373059236371));
#166641=CARTESIAN_POINT('Ctrl Pts',(-17.4566606449759,-17.2637720887509,
14.3735463575713));
#166642=CARTESIAN_POINT('Ctrl Pts',(-17.4530697665441,-17.2664950174813,
14.3738174984965));
#166643=CARTESIAN_POINT('Ctrl Pts',(-17.4422365027572,-17.2747643930803,
14.3746351159321));
#166644=CARTESIAN_POINT('Ctrl Pts',(-17.4350211370524,-17.2803462875632,
14.3751791596857));
#166645=CARTESIAN_POINT('Ctrl Pts',(-17.3795390550491,-17.3238440493634,
14.3793604568176));
#166646=CARTESIAN_POINT('Ctrl Pts',(-17.3329010200042,-17.363799953952,
14.3828631914692));
#166647=CARTESIAN_POINT('Ctrl Pts',(-17.1808057771431,-17.5060263520505,
14.3945000839994));
#166648=CARTESIAN_POINT('Ctrl Pts',(-17.0842725629316,-17.6172131127653,
14.4022866534614));
#166649=CARTESIAN_POINT('Ctrl Pts',(-16.9468074857225,-17.8134764928882,
14.4154841570817));
#166650=CARTESIAN_POINT('Ctrl Pts',(-16.8986502333391,-17.8928582654723,
14.420692585604));
#166651=CARTESIAN_POINT('Ctrl Pts',(-16.8461311090808,-17.9938328974515,
14.4273222610451));
#166652=CARTESIAN_POINT('Ctrl Pts',(-16.8366864196515,-18.0126734985682,
14.4285591422182));
#166653=CARTESIAN_POINT('Ctrl Pts',(-16.8236312642079,-18.0397168730359,
14.4303356725141));
#166654=CARTESIAN_POINT('Ctrl Pts',(-16.8197889710002,-18.0478067998837,
14.4308672557061));
#166655=CARTESIAN_POINT('Ctrl Pts',(-16.8132397964634,-18.061824900431,
14.4317887200009));
#166656=CARTESIAN_POINT('Ctrl Pts',(-16.8105087221281,-18.0677416837436,
14.4321777585026));
#166657=CARTESIAN_POINT('Ctrl Pts',(-16.8053255545808,-18.0791084841885,
14.4329253857192));
#166658=CARTESIAN_POINT('Ctrl Pts',(-16.8028691315946,-18.0845564671159,
14.433283820683));
#166659=CARTESIAN_POINT('Ctrl Pts',(-16.7965280034257,-18.0987805829214,
14.434219968693));
#166660=CARTESIAN_POINT('Ctrl Pts',(-16.7926798845747,-18.1075727882821,
14.4347989285279));
#166661=CARTESIAN_POINT('Ctrl Pts',(-16.7796940626519,-18.1378008277755,
14.4367906526954));
#166662=CARTESIAN_POINT('Ctrl Pts',(-16.7708508182644,-18.1593606047104,
14.4382133600276));
#166663=CARTESIAN_POINT('Ctrl Pts',(-16.7001127360201,-18.3402694669195,
14.4501732455666));
#166664=CARTESIAN_POINT('Ctrl Pts',(-16.6573841189443,-18.5064033231155,
14.4613736928985));
#166665=CARTESIAN_POINT('Ctrl Pts',(-16.6233203227714,-18.7652862150299,
14.4786285618332));
#166666=CARTESIAN_POINT('Ctrl Pts',(-16.617279953992,-18.85541336513,14.4845834405331));
#166667=CARTESIAN_POINT('Ctrl Pts',(-16.6168937485584,-18.9842815274449,
14.4928167545805));
#166668=CARTESIAN_POINT('Ctrl Pts',(-16.6178351419536,-19.0229063125209,
14.4952477332147));
#166669=CARTESIAN_POINT('Ctrl Pts',(-16.6202270208638,-19.0690931745979,
14.4980939507509));
#166670=CARTESIAN_POINT('Ctrl Pts',(-16.6206620134154,-19.0766979445322,
14.4985606097976));
#166671=CARTESIAN_POINT('Ctrl Pts',(-16.6214000296449,-19.0884842067556,
14.4992806227628));
#166672=CARTESIAN_POINT('Ctrl Pts',(-16.6216744391971,-19.0926673356527,
14.499535533618));
#166673=CARTESIAN_POINT('Ctrl Pts',(-16.6222050590464,-19.10040425159,14.5000057986263));
#166674=CARTESIAN_POINT('Ctrl Pts',(-16.6224578130785,-19.1039581774259,
14.5002213384898));
#166675=CARTESIAN_POINT('Ctrl Pts',(-16.6230477081639,-19.1119668051106,
14.5007059900314));
#166676=CARTESIAN_POINT('Ctrl Pts',(-16.6233899772391,-19.1164210747067,
14.5009748109626));
#166677=CARTESIAN_POINT('Ctrl Pts',(-16.6244360979845,-19.1294934040059,
14.5017616734413));
#166678=CARTESIAN_POINT('Ctrl Pts',(-16.6251786617099,-19.1381083934463,
14.5022775937213));
#166679=CARTESIAN_POINT('Ctrl Pts',(-16.6307248635287,-19.1981515951569,
14.5058564298033));
#166680=CARTESIAN_POINT('Ctrl Pts',(-16.6373568970773,-19.2493979500217,
14.5088243661345));
#166681=CARTESIAN_POINT('Ctrl Pts',(-16.6494414417739,-19.321836351759,
14.512960364339));
#166682=CARTESIAN_POINT('Ctrl Pts',(-16.653356506915,-19.3432620728162,
14.5141762324835));
#166683=CARTESIAN_POINT('Ctrl Pts',(-16.6665993301805,-19.4099023400314,
14.5179447529216));
#166684=CARTESIAN_POINT('Ctrl Pts',(-16.6770759599669,-19.4548755528155,
14.5204691381087));
#166685=CARTESIAN_POINT('Ctrl Pts',(-16.7172948679962,-19.6051063544682,
14.5289363881225));
#166686=CARTESIAN_POINT('Ctrl Pts',(-16.7537170859711,-19.7083902412168,
14.5348247302892));
#166687=CARTESIAN_POINT('Ctrl Pts',(-16.8202493131744,-19.8587993779259,
14.543969652374));
#166688=CARTESIAN_POINT('Ctrl Pts',(-16.8445041725424,-19.9083114950661,
14.5470775046067));
#166689=CARTESIAN_POINT('Ctrl Pts',(-16.8869471269055,-19.987017821485,
14.5522220220363));
#166690=CARTESIAN_POINT('Ctrl Pts',(-16.9039633466278,-20.0168154100458,
14.5542192894047));
#166691=CARTESIAN_POINT('Ctrl Pts',(-16.9272822665565,-20.055438657677,
14.5568801143203));
#166692=CARTESIAN_POINT('Ctrl Pts',(-16.9329397995333,-20.0646490854403,
14.5575201395267));
#166693=CARTESIAN_POINT('Ctrl Pts',(-16.9423229784206,-20.0796657466327,
14.5585728694591));
#166694=CARTESIAN_POINT('Ctrl Pts',(-16.9460069531642,-20.0854978820092,
14.5589840327675));
#166695=CARTESIAN_POINT('Ctrl Pts',(-16.9531942099514,-20.0967538724314,
14.5597821035472));
#166696=CARTESIAN_POINT('Ctrl Pts',(-16.9566939348884,-20.1021799162748,
14.5601688756115));
#166697=CARTESIAN_POINT('Ctrl Pts',(-16.9648334161859,-20.1146736765535,
14.5610642428417));
#166698=CARTESIAN_POINT('Ctrl Pts',(-16.9694907751497,-20.1217297429807,
14.5615734940843));
#166699=CARTESIAN_POINT('Ctrl Pts',(-16.9821331246805,-20.1406360406638,
14.5629477610436));
#166700=CARTESIAN_POINT('Ctrl Pts',(-16.9901959298311,-20.152433478021,
14.5638157045524));
#166701=CARTESIAN_POINT('Ctrl Pts',(-17.0652574980544,-20.2599108955587,
14.5718202909221));
#166702=CARTESIAN_POINT('Ctrl Pts',(-17.1399371257419,-20.3499585840822,
14.5792584768438));
#166703=CARTESIAN_POINT('Ctrl Pts',(-17.3354199611098,-20.5495286040024,
14.597505795565));
#166704=CARTESIAN_POINT('Ctrl Pts',(-17.4621895115106,-20.6521829016177,
14.6084546437164));
#166705=CARTESIAN_POINT('Ctrl Pts',(-17.627039443414,-20.7568253765623,
14.620863629073));
#166706=CARTESIAN_POINT('Ctrl Pts',(-17.655024909666,-20.7736940853253,
14.6229114564933));
#166707=CARTESIAN_POINT('Ctrl Pts',(-17.6896861172972,-20.7935075580639,
14.625366588211));
#166708=CARTESIAN_POINT('Ctrl Pts',(-17.6959994465687,-20.7970735558757,
14.6258105453715));
#166709=CARTESIAN_POINT('Ctrl Pts',(-17.7059218432776,-20.8026110377434,
14.6265030956947));
#166710=CARTESIAN_POINT('Ctrl Pts',(-17.7095184764235,-20.8046045227902,
14.6267530648796));
#166711=CARTESIAN_POINT('Ctrl Pts',(-17.7162497605517,-20.8083098356687,
14.6272188772913));
#166712=CARTESIAN_POINT('Ctrl Pts',(-17.7193829006355,-20.8100241919327,
14.6274348768802));
#166713=CARTESIAN_POINT('Ctrl Pts',(-17.7265418205627,-20.8139178209395,
14.627926569461));
#166714=CARTESIAN_POINT('Ctrl Pts',(-17.7305703318085,-20.8160919658492,
14.6282019345012));
#166715=CARTESIAN_POINT('Ctrl Pts',(-17.7429638509639,-20.822728798854,
14.6290451229149));
#166716=CARTESIAN_POINT('Ctrl Pts',(-17.7513519434513,-20.827148445346,
14.6296102841839));
#166717=CARTESIAN_POINT('Ctrl Pts',(-17.8671859292204,-20.8871900981783,
14.6373429986399));
#166718=CARTESIAN_POINT('Ctrl Pts',(-17.9791944290598,-20.9335661655134,
14.6439805057908));
#166719=CARTESIAN_POINT('Ctrl Pts',(-18.2651924255875,-21.0241835095277,
14.6603064593958));
#166720=CARTESIAN_POINT('Ctrl Pts',(-18.4419637514492,-21.0563841948392,
14.6699251402767));
#166721=CARTESIAN_POINT('Ctrl Pts',(-18.642123633161,-21.0671144549188,
14.6815960955469));
#166722=CARTESIAN_POINT('Ctrl Pts',(-18.6635892682765,-21.0679377833667,
14.6828564502759));
#166723=CARTESIAN_POINT('Ctrl Pts',(-18.6940855940363,-21.068642928833,
14.6846608395756));
#166724=CARTESIAN_POINT('Ctrl Pts',(-18.7031091692341,-21.0687938493666,
14.685196452973));
#166725=CARTESIAN_POINT('Ctrl Pts',(-18.7186621460312,-21.068954505945,
14.6861226874363));
#166726=CARTESIAN_POINT('Ctrl Pts',(-18.7251911832734,-21.0689917414294,
14.6865124420484));
#166727=CARTESIAN_POINT('Ctrl Pts',(-18.7376819738936,-21.0690051925942,
14.6872599007969));
#166728=CARTESIAN_POINT('Ctrl Pts',(-18.7436436678334,-21.0689864290881,
14.6876174437478));
#166729=CARTESIAN_POINT('Ctrl Pts',(-18.7591228075927,-21.0688723237722,
14.6885478696725));
#166730=CARTESIAN_POINT('Ctrl Pts',(-18.768639753568,-21.0687379794059,
14.6891219695787));
#166731=CARTESIAN_POINT('Ctrl Pts',(-18.8009696859958,-21.0680635107694,
14.691079382418));
#166732=CARTESIAN_POINT('Ctrl Pts',(-18.8237740980564,-21.0672187281264,
14.6924721817665));
#166733=CARTESIAN_POINT('Ctrl Pts',(-19.0240757280663,-21.0565537154634,
14.7048164834835));
#166734=CARTESIAN_POINT('Ctrl Pts',(-19.1996626289566,-21.0247817669645,
14.7164925311726));
#166735=CARTESIAN_POINT('Ctrl Pts',(-19.4506665101214,-20.9458344943402,
14.7338754759693));
#166736=CARTESIAN_POINT('Ctrl Pts',(-19.5305375663184,-20.9152923006605,
14.7395017807799));
#166737=CARTESIAN_POINT('Ctrl Pts',(-19.6424270586408,-20.864550511978,
14.7473429782496));
#166738=CARTESIAN_POINT('Ctrl Pts',(-19.6760922432131,-20.848194026208,
14.7496961010084));
#166739=CARTESIAN_POINT('Ctrl Pts',(-19.7160080828495,-20.8274749012922,
14.7524634050521));
#166740=CARTESIAN_POINT('Ctrl Pts',(-19.7226892732827,-20.8239614058514,
14.7529258188324));
#166741=CARTESIAN_POINT('Ctrl Pts',(-19.7330383414801,-20.8184481887533,
14.7536407028168));
#166742=CARTESIAN_POINT('Ctrl Pts',(-19.7367192564565,-20.8164732613998,
14.7538946954068));
#166743=CARTESIAN_POINT('Ctrl Pts',(-19.7435300021399,-20.8127930776969,
14.7543641105007));
#166744=CARTESIAN_POINT('Ctrl Pts',(-19.7466613443232,-20.8110908275909,
14.7545797133162));
#166745=CARTESIAN_POINT('Ctrl Pts',(-19.7537247501403,-20.8072279004783,
14.7550655709126));
#166746=CARTESIAN_POINT('Ctrl Pts',(-19.7576542420374,-20.8050626331488,
14.7553355284645));
#166747=CARTESIAN_POINT('Ctrl Pts',(-19.7692143287784,-20.7986446879429,
14.7561288154487));
#166748=CARTESIAN_POINT('Ctrl Pts',(-19.7768256261236,-20.7943571937778,
14.7566499713084));
#166749=CARTESIAN_POINT('Ctrl Pts',(-19.8310962478148,-20.7633421127041,
14.7603592573306));
#166750=CARTESIAN_POINT('Ctrl Pts',(-19.8767530185861,-20.7348900713738,
14.7634443584259));
#166751=CARTESIAN_POINT('Ctrl Pts',(-20.0608279562891,-20.6101995162181,
14.7759434364569));
#166752=CARTESIAN_POINT('Ctrl Pts',(-20.1885934080942,-20.499340890524,
14.7848133067536));
#166753=CARTESIAN_POINT('Ctrl Pts',(-20.3564534647442,-20.3143266674313,
14.7986576872988));
#166754=CARTESIAN_POINT('Ctrl Pts',(-20.4075288571257,-20.2510720812714,
14.8032487951523));
#166755=CARTESIAN_POINT('Ctrl Pts',(-20.4662740102747,-20.1690871364965,
14.8091326478384));
#166756=CARTESIAN_POINT('Ctrl Pts',(-20.4774847986288,-20.1529725488644,
14.810285933835));
#166757=CARTESIAN_POINT('Ctrl Pts',(-20.4933402542996,-20.129491665318,
14.8119628819907));
#166758=CARTESIAN_POINT('Ctrl Pts',(-20.4981663215216,-20.1222486653921,
14.812479681482));
#166759=CARTESIAN_POINT('Ctrl Pts',(-20.5065035600957,-20.1095672900544,
14.8133837821075));
#166760=CARTESIAN_POINT('Ctrl Pts',(-20.5100347292345,-20.1041421529798,
14.813770327022));
#166761=CARTESIAN_POINT('Ctrl Pts',(-20.5168105239017,-20.093626940683,
14.8145191342108));
#166762=CARTESIAN_POINT('Ctrl Pts',(-20.5200583734894,-20.0885390099521,
14.8148812712892));
#166763=CARTESIAN_POINT('Ctrl Pts',(-20.5277198381499,-20.0764229703323,
14.8157432390812));
#166764=CARTESIAN_POINT('Ctrl Pts',(-20.5321139486244,-20.0693827001873,
14.8162437856645));
#166765=CARTESIAN_POINT('Ctrl Pts',(-20.5475456049671,-20.0443312533415,
14.818023883128));
#166766=CARTESIAN_POINT('Ctrl Pts',(-20.5583545593534,-20.0261813717135,
14.8193117641296));
#166767=CARTESIAN_POINT('Ctrl Pts',(-20.6657650088142,-19.839524182704,
14.8325424137311));
#166768=CARTESIAN_POINT('Ctrl Pts',(-20.7389930443321,-19.6586728277574,
14.8453728959637));
#166769=CARTESIAN_POINT('Ctrl Pts',(-20.8048202355923,-19.398055353222,
14.8631017541084));
#166770=CARTESIAN_POINT('Ctrl Pts',(-20.8192617767641,-19.3247555236717,
14.8679935204894));
#166771=CARTESIAN_POINT('Ctrl Pts',(-20.8346727919646,-19.2166767560843,
14.8749433752754));
#166772=CARTESIAN_POINT('Ctrl Pts',(-20.8387085640078,-19.1823956212695,
14.8771093266513));
#166773=CARTESIAN_POINT('Ctrl Pts',(-20.8425871759834,-19.1406888050124,
14.8796857842226));
#166774=CARTESIAN_POINT('Ctrl Pts',(-20.843231456135,-19.1333450081682,
14.880137248492));
#166775=CARTESIAN_POINT('Ctrl Pts',(-20.844177533657,-19.121873202885,14.880838889526));
#166776=CARTESIAN_POINT('Ctrl Pts',(-20.8445056015823,-19.1177475036803,
14.8810905010912));
#166777=CARTESIAN_POINT('Ctrl Pts',(-20.8450939760934,-19.1100631376055,
14.8815577589508));
#166778=CARTESIAN_POINT('Ctrl Pts',(-20.8453573821213,-19.1065048108827,
14.8817735714453));
#166779=CARTESIAN_POINT('Ctrl Pts',(-20.8459354331482,-19.0984183338005,
14.8822627676358));
#166780=CARTESIAN_POINT('Ctrl Pts',(-20.8462445116755,-19.0938898376823,
14.8825358364075));
#166781=CARTESIAN_POINT('Ctrl Pts',(-20.8470081048128,-19.0821461249705,
14.8832417692837));
#166782=CARTESIAN_POINT('Ctrl Pts',(-20.8474402334159,-19.0749294432504,
14.8836734093755));
#166783=CARTESIAN_POINT('Ctrl Pts',(-20.8499256633027,-19.0295248659026,
14.8863762934984));
#166784=CARTESIAN_POINT('Ctrl Pts',(-20.8509809805955,-18.9912868194502,
14.8885955342883));
#166785=CARTESIAN_POINT('Ctrl Pts',(-20.8510792902781,-18.7909008209396,
14.9000236869547));
#166786=CARTESIAN_POINT('Ctrl Pts',(-20.832532273869,-18.6292767121341,
14.9085853292683));
#166787=CARTESIAN_POINT('Ctrl Pts',(-20.7763041393555,-18.3880942468308,
14.9221736104699));
#166788=CARTESIAN_POINT('Ctrl Pts',(-20.7518790836572,-18.3061287042505,
14.9269355922798));
#166789=CARTESIAN_POINT('Ctrl Pts',(-20.7225805503655,-18.2258895437275,
14.9318514930297));
#166790=CARTESIAN_POINT('Origin',(-18.734,-18.952,0.));
#166791=CARTESIAN_POINT('',(-20.7225805738037,-18.2258896079172,15.9575279467182));
#166792=CARTESIAN_POINT('',(-20.7225805680845,-18.2258895922541,15.7328935628168));
#166793=CARTESIAN_POINT('',(-20.7225805737622,-18.2258896078036,0.));
#166794=CARTESIAN_POINT('',(-20.8509995343428,-18.9534041339616,15.9109437209775));
#166795=CARTESIAN_POINT('Ctrl Pts',(-20.7225805738037,-18.2258896079172,
15.9575279467182));
#166796=CARTESIAN_POINT('Ctrl Pts',(-20.7279981079307,-18.2407264746532,
15.9565690253348));
#166797=CARTESIAN_POINT('Ctrl Pts',(-20.7332493642926,-18.2556233409562,
15.9556045828014));
#166798=CARTESIAN_POINT('Ctrl Pts',(-20.768347076402,-18.3588595979594,
15.9489085458843));
#166799=CARTESIAN_POINT('Ctrl Pts',(-20.7924915060708,-18.4490166027167,
15.9429916617944));
#166800=CARTESIAN_POINT('Ctrl Pts',(-20.8375614450588,-18.676438452644,
15.927941103698));
#166801=CARTESIAN_POINT('Ctrl Pts',(-20.8510859073874,-18.8147188131726,
15.918664814329));
#166802=CARTESIAN_POINT('Ctrl Pts',(-20.8509995894475,-18.9533184382234,
15.9096292174278));
#166803=CARTESIAN_POINT('Ctrl Pts',(-20.7225805737622,-18.2258896078036,
15.1555945473776));
#166804=CARTESIAN_POINT('Ctrl Pts',(-20.6976334619431,-18.1575675696285,
15.1599719962089));
#166805=CARTESIAN_POINT('Ctrl Pts',(-20.6691305109114,-18.090448506577,
15.1643494450402));
#166806=CARTESIAN_POINT('Ctrl Pts',(-20.6372132212172,-18.0249247956158,
15.1687268938715));
#166807=CARTESIAN_POINT('Ctrl Pts',(-20.6053187551123,-17.9594479397066,
15.1731012124529));
#166808=CARTESIAN_POINT('Ctrl Pts',(-20.5700150048519,-17.8955646048789,
15.1774755310343));
#166809=CARTESIAN_POINT('Ctrl Pts',(-20.5314915042865,-17.8336470628564,
15.1818498496157));
#166810=CARTESIAN_POINT('Ctrl Pts',(-20.4929828430108,-17.7717533715308,
15.1862224832053));
#166811=CARTESIAN_POINT('Ctrl Pts',(-20.4512571477743,-17.7118243791939,
15.1905951167949));
#166812=CARTESIAN_POINT('Ctrl Pts',(-20.4065489800678,-17.6542061376034,
15.1949677503846));
#166813=CARTESIAN_POINT('Ctrl Pts',(-20.3618432858589,-17.5965910837656,
15.1993401420565));
#166814=CARTESIAN_POINT('Ctrl Pts',(-20.3141557437213,-17.5412869069951,
15.2037125337283));
#166815=CARTESIAN_POINT('Ctrl Pts',(-20.2637621434272,-17.4886077817151,
15.2080849254002));
#166816=CARTESIAN_POINT('Ctrl Pts',(-20.2133188587134,-17.4358767186541,
15.2124616279319));
#166817=CARTESIAN_POINT('Ctrl Pts',(-20.1601645203762,-17.3857762266896,
15.2168383304635));
#166818=CARTESIAN_POINT('Ctrl Pts',(-20.104612302126,-17.3385840842298,
15.2212150329952));
#166819=CARTESIAN_POINT('Ctrl Pts',(-20.0490337746074,-17.2913695917939,
15.2255938083125));
#166820=CARTESIAN_POINT('Ctrl Pts',(-19.991055488614,-17.2470664862988,
15.2299725836298));
#166821=CARTESIAN_POINT('Ctrl Pts',(-19.9310221067214,-17.2059109197924,
15.2343513589471));
#166822=CARTESIAN_POINT('Ctrl Pts',(-19.8708775583487,-17.1646791436952,
15.2387382426372));
#166823=CARTESIAN_POINT('Ctrl Pts',(-19.8086707226497,-17.1266068052155,
15.2431251263273));
#166824=CARTESIAN_POINT('Ctrl Pts',(-19.7447731738505,-17.0918853285283,
15.2475120100174));
#166825=CARTESIAN_POINT('Ctrl Pts',(-19.6856842856162,-17.0597768440269,
15.2515687553062));
#166826=CARTESIAN_POINT('Ctrl Pts',(-19.6251501220134,-17.0305334662485,
15.2556255005951));
#166827=CARTESIAN_POINT('Ctrl Pts',(-19.5634785608967,-17.0042694444527,
15.2596822458839));
#166828=CARTESIAN_POINT('Ctrl Pts',(-19.4967680143858,-16.9758594737003,
15.2640704548148));
#166829=CARTESIAN_POINT('Ctrl Pts',(-19.4284659821152,-16.9508253061037,
15.2684586637457));
#166830=CARTESIAN_POINT('Ctrl Pts',(-19.3589476876738,-16.9293459545263,
15.2728468726766));
#166831=CARTESIAN_POINT('Ctrl Pts',(-19.2895325699075,-16.9078984818679,
15.2772285687779));
#166832=CARTESIAN_POINT('Ctrl Pts',(-19.2189052304797,-16.8899954929979,
15.2816102648792));
#166833=CARTESIAN_POINT('Ctrl Pts',(-19.1474611885818,-16.8757681137367,
15.2859919609804));
#166834=CARTESIAN_POINT('Ctrl Pts',(-19.0761010991188,-16.8615574527783,
15.2903685082401));
#166835=CARTESIAN_POINT('Ctrl Pts',(-19.0039266843571,-16.8510139151847,
15.2947450554997));
#166836=CARTESIAN_POINT('Ctrl Pts',(-18.9313473123121,-16.84421845574,15.2991216027594));
#166837=CARTESIAN_POINT('Ctrl Pts',(-18.85881396905,-16.8374273058769,15.3034953744764));
#166838=CARTESIAN_POINT('Ctrl Pts',(-18.7858766571603,-16.8343795627893,
15.3078691461934));
#166839=CARTESIAN_POINT('Ctrl Pts',(-18.7129521899217,-16.8351046342129,
15.3122429179103));
#166840=CARTESIAN_POINT('Ctrl Pts',(-18.6400499138434,-16.8358294849948,
15.3166153586739));
#166841=CARTESIAN_POINT('Ctrl Pts',(-18.5671609567202,-16.840324866202,
15.3209877994375));
#166842=CARTESIAN_POINT('Ctrl Pts',(-18.4947027860634,-16.8485680796845,
15.325360240201));
#166843=CARTESIAN_POINT('Ctrl Pts',(-18.4222427626431,-16.8568115039469,
15.3297327927684));
#166844=CARTESIAN_POINT('Ctrl Pts',(-18.3502140266188,-16.8688028942382,
15.3341053453357));
#166845=CARTESIAN_POINT('Ctrl Pts',(-18.2790278943149,-16.8844678036247,
15.3384778979031));
#166846=CARTESIAN_POINT('Ctrl Pts',(-18.2077678823577,-16.9001489706451,
15.3428549884704));
#166847=CARTESIAN_POINT('Ctrl Pts',(-18.1373526922048,-16.9195111648158,
15.3472320790378));
#166848=CARTESIAN_POINT('Ctrl Pts',(-18.068181604065,-16.9424291842201,
15.3516091696051));
#166849=CARTESIAN_POINT('Ctrl Pts',(-17.9989727390266,-16.9653597200053,
15.355988650664));
#166850=CARTESIAN_POINT('Ctrl Pts',(-17.9310097785358,-16.9918497721616,
15.360368131723));
#166851=CARTESIAN_POINT('Ctrl Pts',(-17.8646724802095,-17.0217257543719,
15.3647476127819));
#166852=CARTESIAN_POINT('Ctrl Pts',(-17.7982175994673,-17.0516546915603,
15.3691348564417));
#166853=CARTESIAN_POINT('Ctrl Pts',(-17.7333945644586,-17.0849813228793,
15.3735221001014));
#166854=CARTESIAN_POINT('Ctrl Pts',(-17.67055844431,-17.1214861219779,15.3779093437611));
#166855=CARTESIAN_POINT('Ctrl Pts',(-17.627835937484,-17.1463058677703,
15.3808922466959));
#166856=CARTESIAN_POINT('Ctrl Pts',(-17.5860313573343,-17.1725938434286,
15.3838751496307));
#166857=CARTESIAN_POINT('Ctrl Pts',(-17.5452478505357,-17.2002701900282,
15.3868580525654));
#166858=CARTESIAN_POINT('Ctrl Pts',(-17.4852504075478,-17.2409854241403,
15.3912462614963));
#166859=CARTESIAN_POINT('Ctrl Pts',(-17.4272300397247,-17.2848661041391,
15.3956344704272));
#166860=CARTESIAN_POINT('Ctrl Pts',(-17.3715403699669,-17.3316936226349,
15.4000226793581));
#166861=CARTESIAN_POINT('Ctrl Pts',(-17.3159333529126,-17.378451641329,
15.4044043754593));
#166862=CARTESIAN_POINT('Ctrl Pts',(-17.2626505332037,-17.4281475084506,
15.4087860715606));
#166863=CARTESIAN_POINT('Ctrl Pts',(-17.2120162539407,-17.4805196308712,
15.4131677676619));
#166864=CARTESIAN_POINT('Ctrl Pts',(-17.1614414739856,-17.5328302118801,
15.4175443149215));
#166865=CARTESIAN_POINT('Ctrl Pts',(-17.1135093856061,-17.5878104559202,
15.4219208621811));
#166866=CARTESIAN_POINT('Ctrl Pts',(-17.0685096421066,-17.6451599685638,
15.4262974094408));
#166867=CARTESIAN_POINT('Ctrl Pts',(-17.0235384367905,-17.70247311098,15.4306711811577));
#166868=CARTESIAN_POINT('Ctrl Pts',(-16.9814961836094,-17.7621521621708,
15.4350449528747));
#166869=CARTESIAN_POINT('Ctrl Pts',(-16.9426332229373,-17.8238625659805,
15.4394187245917));
#166870=CARTESIAN_POINT('Ctrl Pts',(-16.9037820883947,-17.8855541911071,
15.4437911653552));
#166871=CARTESIAN_POINT('Ctrl Pts',(-16.8681085825381,-17.9492755337056,
15.4481636061187));
#166872=CARTESIAN_POINT('Ctrl Pts',(-16.8358195870614,-18.0146632835868,
15.4525360468823));
#166873=CARTESIAN_POINT('Ctrl Pts',(-16.8035297659516,-18.0800527054399,
15.4569085994496));
#166874=CARTESIAN_POINT('Ctrl Pts',(-16.774624838831,-18.1471081857714,
15.461281152017));
#166875=CARTESIAN_POINT('Ctrl Pts',(-16.7492648453349,-18.2154435759314,
15.4656537045843));
#166876=CARTESIAN_POINT('Ctrl Pts',(-16.7238785322811,-18.2838498871369,
15.4700307951516));
#166877=CARTESIAN_POINT('Ctrl Pts',(-16.7020446665449,-18.3535383070813,
15.4744078857189));
#166878=CARTESIAN_POINT('Ctrl Pts',(-16.6838740959319,-18.4241053348735,
15.4787849762862));
#166879=CARTESIAN_POINT('Ctrl Pts',(-16.665693601696,-18.4947109019386,
15.4831644573452));
#166880=CARTESIAN_POINT('Ctrl Pts',(-16.6511804819233,-18.566195559148,
15.4875439384041));
#166881=CARTESIAN_POINT('Ctrl Pts',(-16.6403943335878,-18.6381460314626,
15.491923419463));
#166882=CARTESIAN_POINT('Ctrl Pts',(-16.6295890668767,-18.7102240355065,
15.4963106631227));
#166883=CARTESIAN_POINT('Ctrl Pts',(-16.6225240103779,-18.7827690229242,
15.5006979067824));
#166884=CARTESIAN_POINT('Ctrl Pts',(-16.6192067693547,-18.855363611321,
15.5050851504422));
#166885=CARTESIAN_POINT('Ctrl Pts',(-16.6169513651075,-18.9047209362344,
15.5080680533771));
#166886=CARTESIAN_POINT('Ctrl Pts',(-16.6164273661252,-18.9541011550573,
15.511050956312));
#166887=CARTESIAN_POINT('Ctrl Pts',(-16.6176234550289,-19.0033743116383,
15.5140338592469));
#166888=CARTESIAN_POINT('Ctrl Pts',(-16.6193830456439,-19.0758610503895,
15.5184220681778));
#166889=CARTESIAN_POINT('Ctrl Pts',(-16.6248744285954,-19.1483987776271,
15.5228102771086));
#166890=CARTESIAN_POINT('Ctrl Pts',(-16.6341051990331,-19.2205718244199,
15.5271984860395));
#166891=CARTESIAN_POINT('Ctrl Pts',(-16.643322269477,-19.2926377544447,
15.5315801821408));
#166892=CARTESIAN_POINT('Ctrl Pts',(-16.6562676494649,-19.3643396039473,
15.5359618782421));
#166893=CARTESIAN_POINT('Ctrl Pts',(-16.6728969413427,-19.4352630563096,
15.5403435743433));
#166894=CARTESIAN_POINT('Ctrl Pts',(-16.6895066924792,-19.506103167971,
15.544720121603));
#166895=CARTESIAN_POINT('Ctrl Pts',(-16.7097916465688,-19.576166232197,
15.5490966688626));
#166896=CARTESIAN_POINT('Ctrl Pts',(-16.7336560032764,-19.6450460985908,
15.5534732161223));
#166897=CARTESIAN_POINT('Ctrl Pts',(-16.7575052255558,-19.7138822823745,
15.5578469878392));
#166898=CARTESIAN_POINT('Ctrl Pts',(-16.7849291889403,-19.7815363024759,
15.5622207595562));
#166899=CARTESIAN_POINT('Ctrl Pts',(-16.8157820891438,-19.8476165733563,
15.5665945312732));
#166900=CARTESIAN_POINT('Ctrl Pts',(-16.8466256007062,-19.9136767357882,
15.5709669720367));
#166901=CARTESIAN_POINT('Ctrl Pts',(-16.8808957735919,-19.9781636629368,
15.5753394128003));
#166902=CARTESIAN_POINT('Ctrl Pts',(-16.9183991025641,-20.0407067471224,
15.5797118535638));
#166903=CARTESIAN_POINT('Ctrl Pts',(-16.9559033905005,-20.1032514305415,
15.5840844061312));
#166904=CARTESIAN_POINT('Ctrl Pts',(-16.9966407488745,-20.1638517596418,
15.5884569586985));
#166905=CARTESIAN_POINT('Ctrl Pts',(-17.0403731142002,-20.2221641514765,
15.5928295112658));
#166906=CARTESIAN_POINT('Ctrl Pts',(-17.0841508666242,-20.280537062111,
15.5972066018332));
#166907=CARTESIAN_POINT('Ctrl Pts',(-17.1309295419551,-20.3366169078816,
15.6015836924005));
#166908=CARTESIAN_POINT('Ctrl Pts',(-17.1804298596136,-20.3900920759463,
15.6059607829678));
#166909=CARTESIAN_POINT('Ctrl Pts',(-17.2299572112327,-20.4435964487851,
15.6103402640268));
#166910=CARTESIAN_POINT('Ctrl Pts',(-17.2822088187839,-20.4944929748966,
15.6147197450857));
#166911=CARTESIAN_POINT('Ctrl Pts',(-17.3368694420731,-20.5425078447171,
15.6190992261446));
#166912=CARTESIAN_POINT('Ctrl Pts',(-17.3916269509501,-20.5906078205721,
15.6234864698044));
#166913=CARTESIAN_POINT('Ctrl Pts',(-17.4488016237921,-20.6358156407829,
15.6278737134641));
#166914=CARTESIAN_POINT('Ctrl Pts',(-17.5080466246419,-20.6778989893525,
15.6322609571238));
#166915=CARTESIAN_POINT('Ctrl Pts',(-17.5483275163853,-20.7065116112382,
15.6352438600586));
#166916=CARTESIAN_POINT('Ctrl Pts',(-17.5895648351146,-20.7336807873359,
15.6382267629935));
#166917=CARTESIAN_POINT('Ctrl Pts',(-17.6316431823902,-20.7593456909704,
15.6412096659283));
#166918=CARTESIAN_POINT('Ctrl Pts',(-17.6935454914315,-20.7971018505908,
15.6455978748592));
#166919=CARTESIAN_POINT('Ctrl Pts',(-17.7575106221337,-20.8317477625257,
15.6499860837901));
#166920=CARTESIAN_POINT('Ctrl Pts',(-17.8231931738168,-20.8630520467476,
15.654374292721));
#166921=CARTESIAN_POINT('Ctrl Pts',(-17.8887782417028,-20.8943098702212,
15.6587559888223));
#166922=CARTESIAN_POINT('Ctrl Pts',(-17.9560752387298,-20.9222357055048,
15.6631376849236));
#166923=CARTESIAN_POINT('Ctrl Pts',(-18.0247117585808,-20.9466426222721,
15.6675193810248));
#166924=CARTESIAN_POINT('Ctrl Pts',(-18.0932676250588,-20.9710208589698,
15.6718959282845));
#166925=CARTESIAN_POINT('Ctrl Pts',(-18.1631594352668,-20.9918882305584,
15.6762724755441));
#166926=CARTESIAN_POINT('Ctrl Pts',(-18.2339938260915,-21.0091054484526,
15.6806490228038));
#166927=CARTESIAN_POINT('Ctrl Pts',(-18.304783294775,-21.0263117474375,
15.6850227945208));
#166928=CARTESIAN_POINT('Ctrl Pts',(-18.376513690443,-21.0398723720884,
15.6893965662377));
#166929=CARTESIAN_POINT('Ctrl Pts',(-18.4487768305325,-21.0496979629105,
15.6937703379547));
#166930=CARTESIAN_POINT('Ctrl Pts',(-18.5210179807058,-21.0595205637724,
15.6981427787183));
#166931=CARTESIAN_POINT('Ctrl Pts',(-18.5937910757581,-21.0656103223221,
15.7025152194818));
#166932=CARTESIAN_POINT('Ctrl Pts',(-18.6666797525664,-21.0679293429331,
15.7068876602454));
#166933=CARTESIAN_POINT('Ctrl Pts',(-18.7395702931462,-21.0702484228418,
15.7112602128128));
#166934=CARTESIAN_POINT('Ctrl Pts',(-18.8125759391524,-21.0687965600418,
15.7156327653801));
#166935=CARTESIAN_POINT('Ctrl Pts',(-18.8852789324503,-21.0635879533178,
15.7200053179475));
#166936=CARTESIAN_POINT('Ctrl Pts',(-18.958057379657,-21.0583739409052,
15.7243824085148));
#166937=CARTESIAN_POINT('Ctrl Pts',(-19.030532064851,-21.0493954347149,
15.7287594990821));
#166938=CARTESIAN_POINT('Ctrl Pts',(-19.1022898016655,-21.0367185953958,
15.7331365896495));
#166939=CARTESIAN_POINT('Ctrl Pts',(-19.1740867280434,-21.0240348327843,
15.7375160707084));
#166940=CARTESIAN_POINT('Ctrl Pts',(-19.2451654560907,-21.007648824085,
15.7418955517674));
#166941=CARTESIAN_POINT('Ctrl Pts',(-19.3151251217576,-20.9876774284896,
15.7462750328263));
#166942=CARTESIAN_POINT('Ctrl Pts',(-19.3852087904624,-20.9676706337297,
15.750662276486));
#166943=CARTESIAN_POINT('Ctrl Pts',(-19.4541689789729,-20.9440659176035,
15.7550495201458));
#166944=CARTESIAN_POINT('Ctrl Pts',(-19.5216226105755,-20.9170291660203,
15.7594367638055));
#166945=CARTESIAN_POINT('Ctrl Pts',(-19.5674845802478,-20.8986467801992,
15.7624196667403));
#166946=CARTESIAN_POINT('Ctrl Pts',(-19.6126505362301,-20.8786788808129,
15.765402569675));
#166947=CARTESIAN_POINT('Ctrl Pts',(-19.6570068699279,-20.8571895753615,
15.7683854726098));
#166948=CARTESIAN_POINT('Ctrl Pts',(-19.7222603709407,-20.8255762228108,
15.7727736815407));
#166949=CARTESIAN_POINT('Ctrl Pts',(-19.7860152120979,-20.7905448456105,
15.7771618904716));
#166950=CARTESIAN_POINT('Ctrl Pts',(-19.8478898805759,-20.7522606294508,
15.7815500994025));
#166951=CARTESIAN_POINT('Ctrl Pts',(-19.9096727167869,-20.7140332334156,
15.7859317955037));
#166952=CARTESIAN_POINT('Ctrl Pts',(-19.9695805130032,-20.6725628338803,
15.790313491605));
#166953=CARTESIAN_POINT('Ctrl Pts',(-20.027254513927,-20.6280613837827,
15.7946951877063));
#166954=CARTESIAN_POINT('Ctrl Pts',(-20.0848607433098,-20.5836122264305,
15.7990717349659));
#166955=CARTESIAN_POINT('Ctrl Pts',(-20.1402380117451,-20.5361393871243,
15.8034482822255));
#166956=CARTESIAN_POINT('Ctrl Pts',(-20.1930562795832,-20.485898227722,
15.8078248294852));
#166957=CARTESIAN_POINT('Ctrl Pts',(-20.2458410508435,-20.4356889305328,
15.8121986012022));
#166958=CARTESIAN_POINT('Ctrl Pts',(-20.2960696928601,-20.3827151282833,
15.8165723729191));
#166959=CARTESIAN_POINT('Ctrl Pts',(-20.3434461269596,-20.3272716693129,
15.8209461446361));
#166960=CARTESIAN_POINT('Ctrl Pts',(-20.3908081442512,-20.2718450819733,
15.8253185853997));
#166961=CARTESIAN_POINT('Ctrl Pts',(-20.4353193635672,-20.2139506964278,
15.8296910261632));
#166962=CARTESIAN_POINT('Ctrl Pts',(-20.4767225512214,-20.1539180959884,
15.8340634669268));
#166963=CARTESIAN_POINT('Ctrl Pts',(-20.5181267975597,-20.0938839605087,
15.8384360194941));
#166964=CARTESIAN_POINT('Ctrl Pts',(-20.5564225822287,-20.0317118998147,
15.8428085720614));
#166965=CARTESIAN_POINT('Ctrl Pts',(-20.5913957196045,-19.9677608679186,
15.8471811246288));
#166966=CARTESIAN_POINT('Ctrl Pts',(-20.6264051534215,-19.9037434652295,
15.8515582151961));
#166967=CARTESIAN_POINT('Ctrl Pts',(-20.6580848230993,-19.8379438292391,
15.8559353057634));
#166968=CARTESIAN_POINT('Ctrl Pts',(-20.6862667093298,-19.7707451957981,
15.8603123963308));
#166969=CARTESIAN_POINT('Ctrl Pts',(-20.7144639867344,-19.7035098626893,
15.8646918773897));
#166970=CARTESIAN_POINT('Ctrl Pts',(-20.7391595139378,-19.6348744651304,
15.8690713584487));
#166971=CARTESIAN_POINT('Ctrl Pts',(-20.7602345709195,-19.5652393200134,
15.8734508395076));
#166972=CARTESIAN_POINT('Ctrl Pts',(-20.7813469832984,-19.4954807470691,
15.8778380831673));
#166973=CARTESIAN_POINT('Ctrl Pts',(-20.798825994671,-19.424719356578,15.882225326827));
#166974=CARTESIAN_POINT('Ctrl Pts',(-20.8126037366754,-19.3533670463295,
15.8866125704868));
#166975=CARTESIAN_POINT('Ctrl Pts',(-20.8219712736182,-19.3048543508528,
15.8895954734216));
#166976=CARTESIAN_POINT('Ctrl Pts',(-20.8296289055562,-19.2560686843217,
15.8925783763564));
#166977=CARTESIAN_POINT('Ctrl Pts',(-20.8355690425742,-19.207140273759,
15.8955612792912));
#166978=CARTESIAN_POINT('Ctrl Pts',(-20.8457798800575,-19.1230344615427,
15.9006887598533));
#166979=CARTESIAN_POINT('Ctrl Pts',(-20.850943223371,-19.0383036553196,
15.9058162404154));
#166980=CARTESIAN_POINT('Ctrl Pts',(-20.8509995343428,-18.9534041339616,
15.9109437209775));
#166981=CARTESIAN_POINT('',(-20.8509995791063,-18.9533349395905,15.6876313735509));
#166982=CARTESIAN_POINT('Ctrl Pts',(-20.7225805503655,-18.2258895437275,
14.9318514930297));
#166983=CARTESIAN_POINT('Ctrl Pts',(-20.7140100821148,-18.2024178166321,
14.9332895026011));
#166984=CARTESIAN_POINT('Ctrl Pts',(-20.7050225797307,-18.179093798098,
14.9347403257965));
#166985=CARTESIAN_POINT('Ctrl Pts',(-20.6902873303515,-18.1427842636067,
14.9370362637722));
#166986=CARTESIAN_POINT('Ctrl Pts',(-20.6848211899767,-18.1296941584371,
14.9378717048454));
#166987=CARTESIAN_POINT('Ctrl Pts',(-20.6758998533147,-18.1089193810253,
14.9392103882356));
#166988=CARTESIAN_POINT('Ctrl Pts',(-20.6725295621615,-18.1011985520166,
14.9397107437133));
#166989=CARTESIAN_POINT('Ctrl Pts',(-20.6664968922938,-18.0876005621048,
14.9405970906885));
#166990=CARTESIAN_POINT('Ctrl Pts',(-20.6638535463659,-18.0817150379815,
14.9409824261025));
#166991=CARTESIAN_POINT('Ctrl Pts',(-20.6583232649041,-18.069550721461,
14.9417824220348));
#166992=CARTESIAN_POINT('Ctrl Pts',(-20.6554324098596,-18.0632738050306,
14.9421972141488));
#166993=CARTESIAN_POINT('Ctrl Pts',(-20.6479172888172,-18.0471642829473,
14.9432669413107));
#166994=CARTESIAN_POINT('Ctrl Pts',(-20.6432480047396,-18.0373530119265,
14.9439234292868));
#166995=CARTESIAN_POINT('Ctrl Pts',(-20.623305154258,-17.9962665399389,
14.9466939274273));
#166996=CARTESIAN_POINT('Ctrl Pts',(-20.60733773314,-17.9653359617657,14.9488320096977));
#166997=CARTESIAN_POINT('Ctrl Pts',(-20.563605069465,-17.8855130100752,
14.9544918546439));
#166998=CARTESIAN_POINT('Ctrl Pts',(-20.5346433137451,-17.8373108063542,
14.9580538430729));
#166999=CARTESIAN_POINT('Ctrl Pts',(-20.4347647586242,-17.6851473573637,
14.969763671701));
#167000=CARTESIAN_POINT('Ctrl Pts',(-20.3564957391982,-17.5863429069977,
14.9781231163307));
#167001=CARTESIAN_POINT('Ctrl Pts',(-20.2011023779936,-17.4225225399811,
14.9930006084852));
#167002=CARTESIAN_POINT('Ctrl Pts',(-20.1272128098503,-17.3549234499617,
14.9995201870726));
#167003=CARTESIAN_POINT('Ctrl Pts',(-20.0412146212309,-17.2867754181238,
15.0062995681532));
#167004=CARTESIAN_POINT('Ctrl Pts',(-20.0335754769467,-17.2808068448063,
15.0068951999125));
#167005=CARTESIAN_POINT('Ctrl Pts',(-20.0222359690359,-17.2720718985144,
15.0077693581891));
#167006=CARTESIAN_POINT('Ctrl Pts',(-20.018567242737,-17.2692649234357,
15.0080506501258));
#167007=CARTESIAN_POINT('Ctrl Pts',(-20.0120424365972,-17.2643065102165,
15.0085481761867));
#167008=CARTESIAN_POINT('Ctrl Pts',(-20.0091900671863,-17.2621502793356,
15.0087647451505));
#167009=CARTESIAN_POINT('Ctrl Pts',(-20.0030671640945,-17.2575460403536,
15.0092276374586));
#167010=CARTESIAN_POINT('Ctrl Pts',(-19.9997950128624,-17.2551002756775,
15.0094738045857));
#167011=CARTESIAN_POINT('Ctrl Pts',(-19.9907938693459,-17.2484129075098,
15.0101477229807));
#167012=CARTESIAN_POINT('Ctrl Pts',(-19.9850504408161,-17.2441906987168,
15.0105741421245));
#167013=CARTESIAN_POINT('Ctrl Pts',(-19.9542778887906,-17.2218071920604,
15.0128403741077));
#167014=CARTESIAN_POINT('Ctrl Pts',(-19.9288730082408,-17.2041659118355,
15.0146464521655));
#167015=CARTESIAN_POINT('Ctrl Pts',(-19.8508165898018,-17.1524608712662,
15.020031926796));
#167016=CARTESIAN_POINT('Ctrl Pts',(-19.7970274433944,-17.1201719036548,
15.023524573912));
#167017=CARTESIAN_POINT('Ctrl Pts',(-19.6236648901271,-17.0263166627344,
15.0343589449834));
#167018=CARTESIAN_POINT('Ctrl Pts',(-19.4996237033979,-16.9737227247783,
15.0415276930897));
#167019=CARTESIAN_POINT('Ctrl Pts',(-19.3325235182404,-16.9209600284138,
15.0512527370378));
#167020=CARTESIAN_POINT('Ctrl Pts',(-19.2932700150733,-16.9098025137702,
15.0535399696008));
#167021=CARTESIAN_POINT('Ctrl Pts',(-19.2066105138334,-16.8878561237639,
15.0586207112253));
#167022=CARTESIAN_POINT('Ctrl Pts',(-19.1591071714363,-16.8775521217728,
15.0614260183341));
#167023=CARTESIAN_POINT('Ctrl Pts',(-19.0988926664441,-16.8666460307821,
15.0650250366351));
#167024=CARTESIAN_POINT('Ctrl Pts',(-19.086471857336,-16.8645107390911,
15.0657696811737));
#167025=CARTESIAN_POINT('Ctrl Pts',(-19.0667599296158,-16.861302956798,
15.066955287616));
#167026=CARTESIAN_POINT('Ctrl Pts',(-19.059480879897,-16.8601573931273,
15.0673939267733));
#167027=CARTESIAN_POINT('Ctrl Pts',(-19.0459068961037,-16.8580937088595,
15.0682135031394));
#167028=CARTESIAN_POINT('Ctrl Pts',(-19.0396135007279,-16.8571659123645,
15.0685941287033));
#167029=CARTESIAN_POINT('Ctrl Pts',(-19.0256263806054,-16.8551682490841,
15.0694415329751));
#167030=CARTESIAN_POINT('Ctrl Pts',(-19.0179307843542,-16.8541123374447,
15.0699087479767));
#167031=CARTESIAN_POINT('Ctrl Pts',(-18.9955533550318,-16.8511673159892,
15.0712702582554));
#167032=CARTESIAN_POINT('Ctrl Pts',(-18.9808575273109,-16.84938984415,15.0721680618509));
#167033=CARTESIAN_POINT('Ctrl Pts',(-18.8639365135023,-16.8364908104568,
15.0793414308601));
#167034=CARTESIAN_POINT('Ctrl Pts',(-18.7610580396062,-16.8326781614781,
15.0858478166534));
#167035=CARTESIAN_POINT('Ctrl Pts',(-18.5026305788978,-16.8419222680883,
15.1026339664158));
#167036=CARTESIAN_POINT('Ctrl Pts',(-18.3480409092547,-16.8646591784076,
15.1131042240962));
#167037=CARTESIAN_POINT('Ctrl Pts',(-18.1465341195476,-16.9174650569955,
15.1265601184731));
#167038=CARTESIAN_POINT('Ctrl Pts',(-18.0962266236068,-16.9326697371415,
15.1298979314946));
#167039=CARTESIAN_POINT('Ctrl Pts',(-18.0383148603353,-16.9525534059556,
15.1336748472197));
#167040=CARTESIAN_POINT('Ctrl Pts',(-18.0301141996943,-16.9554256131912,
15.134208118171));
#167041=CARTESIAN_POINT('Ctrl Pts',(-18.0177156732353,-16.9598539707664,
15.1350117425559));
#167042=CARTESIAN_POINT('Ctrl Pts',(-18.0135047923686,-16.9613730396702,
15.1352842147549));
#167043=CARTESIAN_POINT('Ctrl Pts',(-18.0059505398211,-16.964125335466,
15.1357721560182));
#167044=CARTESIAN_POINT('Ctrl Pts',(-18.0026054509707,-16.9653536518565,
15.1359879109025));
#167045=CARTESIAN_POINT('Ctrl Pts',(-17.9953385778605,-16.9680428892514,
15.1364559388706));
#167046=CARTESIAN_POINT('Ctrl Pts',(-17.9914180318467,-16.9695069898947,
15.1367080190812));
#167047=CARTESIAN_POINT('Ctrl Pts',(-17.980404769588,-16.9736570699484,
15.1374150125109));
#167048=CARTESIAN_POINT('Ctrl Pts',(-17.9733220257991,-16.9763695832229,
15.1378683677725));
#167049=CARTESIAN_POINT('Ctrl Pts',(-17.9308016113123,-16.992916400669,
15.1405829504437));
#167050=CARTESIAN_POINT('Ctrl Pts',(-17.8957251244416,-17.0076667364892,
15.1427926455673));
#167051=CARTESIAN_POINT('Ctrl Pts',(-17.7810024653374,-17.059592150679,
15.1499807157809));
#167052=CARTESIAN_POINT('Ctrl Pts',(-17.7032694218125,-17.1007818357106,
15.1547897428524));
#167053=CARTESIAN_POINT('Ctrl Pts',(-17.4797369312111,-17.2376867240354,
15.1690494204472));
#167054=CARTESIAN_POINT('Ctrl Pts',(-17.3429765256505,-17.3466673888159,
15.1784224143218));
#167055=CARTESIAN_POINT('Ctrl Pts',(-17.204968133178,-17.4876628048802,
15.1898859848335));
#167056=CARTESIAN_POINT('Ctrl Pts',(-17.1890923572652,-17.5044219590816,
15.1912382901944));
#167057=CARTESIAN_POINT('Ctrl Pts',(-17.1670331084522,-17.5284849204347,
15.1931673993233));
#167058=CARTESIAN_POINT('Ctrl Pts',(-17.160619875148,-17.5355765466786,
15.1937344267605));
#167059=CARTESIAN_POINT('Ctrl Pts',(-17.1502809956308,-17.5471659344809,
15.1946587768455));
#167060=CARTESIAN_POINT('Ctrl Pts',(-17.1463259017311,-17.5516373351859,
15.1950148579219));
#167061=CARTESIAN_POINT('Ctrl Pts',(-17.1380892620196,-17.5610289520697,
15.1957616480098));
#167062=CARTESIAN_POINT('Ctrl Pts',(-17.1338114421202,-17.5659523393713,
15.1961525064804));
#167063=CARTESIAN_POINT('Ctrl Pts',(-17.1236935747793,-17.5777063704543,
15.1970841833849));
#167064=CARTESIAN_POINT('Ctrl Pts',(-17.1178741720236,-17.5845545467654,
15.1976258447062));
#167065=CARTESIAN_POINT('Ctrl Pts',(-17.0984378080704,-17.6077243104415,
15.1994547520618));
#167066=CARTESIAN_POINT('Ctrl Pts',(-17.0850234453315,-17.6242134645767,
15.200750187143));
#167067=CARTESIAN_POINT('Ctrl Pts',(-17.0134816870639,-17.7149102380274,
15.207844884841));
#167068=CARTESIAN_POINT('Ctrl Pts',(-16.9601191872357,-17.7927256160896,
15.213829198846));
#167069=CARTESIAN_POINT('Ctrl Pts',(-16.8276093320395,-18.016638557212,
15.2307280904052));
#167070=CARTESIAN_POINT('Ctrl Pts',(-16.7601847899077,-18.1688803243164,
15.2419108154703));
#167071=CARTESIAN_POINT('Ctrl Pts',(-16.6988392690935,-18.3675569577416,
15.2552397293083));
#167072=CARTESIAN_POINT('Ctrl Pts',(-16.687644510726,-18.4080490597497,
15.2578906944697));
#167073=CARTESIAN_POINT('Ctrl Pts',(-16.675893492263,-18.4560746848134,
15.2609373419138));
#167074=CARTESIAN_POINT('Ctrl Pts',(-16.6741638822505,-18.4633083925592,
15.2613936515972));
#167075=CARTESIAN_POINT('Ctrl Pts',(-16.6714258402955,-18.4750324822145,
15.2621288768928));
#167076=CARTESIAN_POINT('Ctrl Pts',(-16.6703938825172,-18.4795172277065,
15.2624090925418));
#167077=CARTESIAN_POINT('Ctrl Pts',(-16.6685864919216,-18.4874907825841,
15.2629054309221));
#167078=CARTESIAN_POINT('Ctrl Pts',(-16.6678052627434,-18.4909782208841,
15.2631218825314));
#167079=CARTESIAN_POINT('Ctrl Pts',(-16.666147560555,-18.498467125969,15.2635853189283));
#167080=CARTESIAN_POINT('Ctrl Pts',(-16.6652738711421,-18.5024691516922,
15.2638321433353));
#167081=CARTESIAN_POINT('Ctrl Pts',(-16.6629010519147,-18.513491529012,
15.2645097179222));
#167082=CARTESIAN_POINT('Ctrl Pts',(-16.6614259895895,-18.5205170842103,
15.2649391117915));
#167083=CARTESIAN_POINT('Ctrl Pts',(-16.6536452675477,-18.5585364641904,
15.2672500552113));
#167084=CARTESIAN_POINT('Ctrl Pts',(-16.6479986932256,-18.5896629236122,
15.269096273308));
#167085=CARTESIAN_POINT('Ctrl Pts',(-16.6174873072952,-18.7823506489699,
15.2803088500755));
#167086=CARTESIAN_POINT('Ctrl Pts',(-16.6107040317,-18.9462297264881,15.2889470397337));
#167087=CARTESIAN_POINT('Ctrl Pts',(-16.6315477623825,-19.2260281016585,
15.3043057725485));
#167088=CARTESIAN_POINT('Ctrl Pts',(-16.6499147915423,-19.3418465995857,
15.31084104163));
#167089=CARTESIAN_POINT('Ctrl Pts',(-16.6811576404712,-19.4694278135802,
15.3185359899385));
#167090=CARTESIAN_POINT('Ctrl Pts',(-16.6846978343963,-19.4832757424116,
15.3193776890723));
#167091=CARTESIAN_POINT('Ctrl Pts',(-16.6905550894349,-19.5052570792134,
15.320724517713));
#167092=CARTESIAN_POINT('Ctrl Pts',(-16.6927811664494,-19.5134144356961,
15.3212267042999));
#167093=CARTESIAN_POINT('Ctrl Pts',(-16.6967932181768,-19.5277770582127,
15.3221151819242));
#167094=CARTESIAN_POINT('Ctrl Pts',(-16.6985588351089,-19.5339879341633,
15.3225008066207));
#167095=CARTESIAN_POINT('Ctrl Pts',(-16.7022693173298,-19.5468167891505,
15.3233003087764));
#167096=CARTESIAN_POINT('Ctrl Pts',(-16.704218166859,-19.5534335272145,
15.3237143124345));
#167097=CARTESIAN_POINT('Ctrl Pts',(-16.7093033188198,-19.5703923870958,
15.3247796964519));
#167098=CARTESIAN_POINT('Ctrl Pts',(-16.7124865131509,-19.5807201371872,
15.3254326056138));
#167099=CARTESIAN_POINT('Ctrl Pts',(-16.7260999466082,-19.6237159837186,
15.3281682126281));
#167100=CARTESIAN_POINT('Ctrl Pts',(-16.7372436280267,-19.6561510932417,
15.3302742321447));
#167101=CARTESIAN_POINT('Ctrl Pts',(-16.7683257596659,-19.7399386426837,
15.3358290190082));
#167102=CARTESIAN_POINT('Ctrl Pts',(-16.7894883421232,-19.7908063640503,
15.3393161771292));
#167103=CARTESIAN_POINT('Ctrl Pts',(-16.8585268381152,-19.9400545332637,
15.3498858524371));
#167104=CARTESIAN_POINT('Ctrl Pts',(-16.9120657081409,-20.0356066220399,
15.3571167600105));
#167105=CARTESIAN_POINT('Ctrl Pts',(-16.9983226644594,-20.1649464433047,
15.3673863357202));
#167106=CARTESIAN_POINT('Ctrl Pts',(-17.0251516246502,-20.2024608410114,
15.3704263820036));
#167107=CARTESIAN_POINT('Ctrl Pts',(-17.0664519509549,-20.2563959180539,
15.3748627775964));
#167108=CARTESIAN_POINT('Ctrl Pts',(-17.0799865766435,-20.2735161172016,
15.3762811610953));
#167109=CARTESIAN_POINT('Ctrl Pts',(-17.1264767746259,-20.3304890602427,
15.3810284957954));
#167110=CARTESIAN_POINT('Ctrl Pts',(-17.1606297870683,-20.3693461598136,
15.3843124864419));
#167111=CARTESIAN_POINT('Ctrl Pts',(-17.2021187940727,-20.4131994318693,
15.388036017511));
#167112=CARTESIAN_POINT('Ctrl Pts',(-17.2081015600556,-20.4194460009142,
15.3885668262704));
#167113=CARTESIAN_POINT('Ctrl Pts',(-17.2172326797203,-20.428863520488,
15.3893674830195));
#167114=CARTESIAN_POINT('Ctrl Pts',(-17.2203529815626,-20.4320613725245,
15.3896394268918));
#167115=CARTESIAN_POINT('Ctrl Pts',(-17.2259797502575,-20.4377915805903,
15.3901268058044));
#167116=CARTESIAN_POINT('Ctrl Pts',(-17.2284824944755,-20.4403274961236,
15.3903425237122));
#167117=CARTESIAN_POINT('Ctrl Pts',(-17.2339435712008,-20.4458330831323,
15.3908109132161));
#167118=CARTESIAN_POINT('Ctrl Pts',(-17.2369043153148,-20.4488002810791,
15.3910633895394));
#167119=CARTESIAN_POINT('Ctrl Pts',(-17.2452686446277,-20.4571331968504,
15.3917726151543));
#167120=CARTESIAN_POINT('Ctrl Pts',(-17.2506924595149,-20.4624786436958,
15.3922277906716));
#167121=CARTESIAN_POINT('Ctrl Pts',(-17.2837764024432,-20.4947345053903,
15.3949766597113));
#167122=CARTESIAN_POINT('Ctrl Pts',(-17.3121411588994,-20.520915579421,
15.3972172955542));
#167123=CARTESIAN_POINT('Ctrl Pts',(-17.409050835543,-20.6055761451323,
15.4045584980955));
#167124=CARTESIAN_POINT('Ctrl Pts',(-17.4806134175529,-20.6604580795296,
15.4094813850064));
#167125=CARTESIAN_POINT('Ctrl Pts',(-17.6976245072979,-20.8058884037477,
15.4236863702818));
#167126=CARTESIAN_POINT('Ctrl Pts',(-17.8507979070175,-20.8835598809046,
15.4329073799991));
#167127=CARTESIAN_POINT('Ctrl Pts',(-18.0335321837806,-20.9498929075246,
15.4442004469876));
#167128=CARTESIAN_POINT('Ctrl Pts',(-18.0555494686134,-20.9574765131314,
15.4455643951208));
#167129=CARTESIAN_POINT('Ctrl Pts',(-18.0868087785433,-20.9676697602659,
15.4475072914679));
#167130=CARTESIAN_POINT('Ctrl Pts',(-18.0959508118928,-20.9705822471554,
15.448076270261));
#167131=CARTESIAN_POINT('Ctrl Pts',(-18.1108181498144,-20.9752076241768,
15.4490029353864));
#167132=CARTESIAN_POINT('Ctrl Pts',(-18.1165315292812,-20.9769586157422,
15.4493593675996));
#167133=CARTESIAN_POINT('Ctrl Pts',(-18.1284912799885,-20.9805686241052,
15.4501061920079));
#167134=CARTESIAN_POINT('Ctrl Pts',(-18.1347389670044,-20.9824230311866,
15.4504967305619));
#167135=CARTESIAN_POINT('Ctrl Pts',(-18.149594736269,-20.9867579067292,
15.4514263548101));
#167136=CARTESIAN_POINT('Ctrl Pts',(-18.158210144992,-20.9892126276577,
15.4519662735384));
#167137=CARTESIAN_POINT('Ctrl Pts',(-18.1871580384758,-20.9972622274732,
15.4537832151529));
#167138=CARTESIAN_POINT('Ctrl Pts',(-18.2075579831668,-21.0026078275547,
15.4550682818953));
#167139=CARTESIAN_POINT('Ctrl Pts',(-18.3182122525613,-21.0298436811777,
15.4620659767638));
#167140=CARTESIAN_POINT('Ctrl Pts',(-18.4097416493751,-21.04607888967,15.4679580387461));
#167141=CARTESIAN_POINT('Ctrl Pts',(-18.6541252393588,-21.0730192659131,
15.4839156481026));
#167142=CARTESIAN_POINT('Ctrl Pts',(-18.8075774858957,-21.0732461727291,
15.4941917929603));
#167143=CARTESIAN_POINT('Ctrl Pts',(-18.9633199080035,-21.0565461675966,
15.5043285933707));
#167144=CARTESIAN_POINT('Ctrl Pts',(-18.9669302640211,-21.056149634434,
15.5045633939949));
#167145=CARTESIAN_POINT('Ctrl Pts',(-19.0222532155453,-21.0499292626121,
15.508158318721));
#167146=CARTESIAN_POINT('Ctrl Pts',(-19.0737396946946,-21.0422093238847,
15.5114638371581));
#167147=CARTESIAN_POINT('Ctrl Pts',(-19.1334072596646,-21.0309992503506,
15.5152085724859));
#167148=CARTESIAN_POINT('Ctrl Pts',(-19.141911257241,-21.0293474562839,
15.5157402182174));
#167149=CARTESIAN_POINT('Ctrl Pts',(-19.154788500525,-21.0267640892072,
15.5165418838924));
#167150=CARTESIAN_POINT('Ctrl Pts',(-19.1591692098003,-21.0258708088799,
15.5168140074847));
#167151=CARTESIAN_POINT('Ctrl Pts',(-19.1670361088122,-21.0242406772178,
15.5173015775243));
#167152=CARTESIAN_POINT('Ctrl Pts',(-19.170523280348,-21.0235088998456,
15.5175173078435));
#167153=CARTESIAN_POINT('Ctrl Pts',(-19.1781065376194,-21.0218975660512,
15.5179855736042));
#167154=CARTESIAN_POINT('Ctrl Pts',(-19.18220185192,-21.0210146571097,15.5182379145921));
#167155=CARTESIAN_POINT('Ctrl Pts',(-19.1937234716516,-21.0184948966738,
15.5189463773023));
#167156=CARTESIAN_POINT('Ctrl Pts',(-19.2011437039711,-21.0168301606141,
15.5194009306643));
#167157=CARTESIAN_POINT('Ctrl Pts',(-19.2459797007189,-21.006517097298,
15.522138015781));
#167158=CARTESIAN_POINT('Ctrl Pts',(-19.2831659926924,-20.9968914020362,
15.5243680167707));
#167159=CARTESIAN_POINT('Ctrl Pts',(-19.4059031199549,-20.961530689677,
15.5316563038228));
#167160=CARTESIAN_POINT('Ctrl Pts',(-19.4900899996355,-20.9313933011439,
15.5365398122478));
#167161=CARTESIAN_POINT('Ctrl Pts',(-19.730183897947,-20.8278817239532,
15.5507589194619));
#167162=CARTESIAN_POINT('Ctrl Pts',(-19.8793220881741,-20.7407272276739,
15.5600279547936));
#167163=CARTESIAN_POINT('Ctrl Pts',(-20.0347835024601,-20.6223871118364,
15.5713778662168));
#167164=CARTESIAN_POINT('Ctrl Pts',(-20.0530706137417,-20.6079841413669,
15.5727413092634));
#167165=CARTESIAN_POINT('Ctrl Pts',(-20.078553579852,-20.5872237469678,
15.5746836071848));
#167166=CARTESIAN_POINT('Ctrl Pts',(-20.0859497883209,-20.5811141141724,
15.5752525010511));
#167167=CARTESIAN_POINT('Ctrl Pts',(-20.0978850644286,-20.5711177340743,
15.5761790653872));
#167168=CARTESIAN_POINT('Ctrl Pts',(-20.1024497033832,-20.5672616239942,
15.5765354822846));
#167169=CARTESIAN_POINT('Ctrl Pts',(-20.1116089907752,-20.559457360816,
15.5772548405965));
#167170=CARTESIAN_POINT('Ctrl Pts',(-20.1162031386547,-20.5555087092422,
15.5776178006941));
#167171=CARTESIAN_POINT('Ctrl Pts',(-20.1271967570972,-20.545977388516,
15.5784915500211));
#167172=CARTESIAN_POINT('Ctrl Pts',(-20.1335796693684,-20.5403758575646,
15.5790031209341));
#167173=CARTESIAN_POINT('Ctrl Pts',(-20.153834463005,-20.5223837275505,
15.5806402947629));
#167174=CARTESIAN_POINT('Ctrl Pts',(-20.1675765342527,-20.509848914329,
15.5817719442139));
#167175=CARTESIAN_POINT('Ctrl Pts',(-20.1993790457063,-20.4800631366377,
15.5844410650096));
#167176=CARTESIAN_POINT('Ctrl Pts',(-20.21730261354,-20.4626707023589,15.5859844865919));
#167177=CARTESIAN_POINT('Ctrl Pts',(-20.2792768851416,-20.4003665062822,
15.5914623361029));
#167178=CARTESIAN_POINT('Ctrl Pts',(-20.3216264213745,-20.3538157325635,
15.595465872288));
#167179=CARTESIAN_POINT('Ctrl Pts',(-20.4170842132422,-20.2390057522114,
15.605120123752));
#167180=CARTESIAN_POINT('Ctrl Pts',(-20.4682073322372,-20.1692426219444,
15.6108203699025));
#167181=CARTESIAN_POINT('Ctrl Pts',(-20.5798191126562,-19.9955753179193,
15.6244629060589));
#167182=CARTESIAN_POINT('Ctrl Pts',(-20.6360168547679,-19.8892486639399,
15.6323956032691));
#167183=CARTESIAN_POINT('Ctrl Pts',(-20.6891096196537,-19.7640887067501,
15.6408791931028));
#167184=CARTESIAN_POINT('Ctrl Pts',(-20.6951525735272,-19.749384669021,
15.6418629227137));
#167185=CARTESIAN_POINT('Ctrl Pts',(-20.7031816721666,-19.7292042417736,
15.643194069304));
#167186=CARTESIAN_POINT('Ctrl Pts',(-20.7053115240518,-19.7237860897997,
15.6435496095536));
#167187=CARTESIAN_POINT('Ctrl Pts',(-20.7086560753642,-19.7151736771791,
15.6441117420015));
#167188=CARTESIAN_POINT('Ctrl Pts',(-20.7098854190927,-19.7119851896667,
15.6443192009855));
#167189=CARTESIAN_POINT('Ctrl Pts',(-20.7124047678474,-19.7054034460699,
15.6447460743496));
#167190=CARTESIAN_POINT('Ctrl Pts',(-20.713693765801,-19.7020098477928,
15.6449654224589));
#167191=CARTESIAN_POINT('Ctrl Pts',(-20.716738503589,-19.693931302329,15.645485833969));
#167192=CARTESIAN_POINT('Ctrl Pts',(-20.7184863900503,-19.6892433789904,
15.6457864284112));
#167193=CARTESIAN_POINT('Ctrl Pts',(-20.7242988977446,-19.6734834755288,
15.6467924261389));
#167194=CARTESIAN_POINT('Ctrl Pts',(-20.728287691953,-19.6623835047555,
15.6474934572906));
#167195=CARTESIAN_POINT('Ctrl Pts',(-20.7681644656086,-19.5484313285155,
15.6546191733456));
#167196=CARTESIAN_POINT('Ctrl Pts',(-20.7961606459488,-19.4429737431072,
15.6606275804652));
#167197=CARTESIAN_POINT('Ctrl Pts',(-20.8391772197475,-19.2096417403651,
15.6735634057899));
#167198=CARTESIAN_POINT('Ctrl Pts',(-20.8509186831227,-19.0816229643116,
15.6804481091254));
#167199=CARTESIAN_POINT('Ctrl Pts',(-20.8509995791063,-18.9533349395905,
15.6876313735509));
#167200=CARTESIAN_POINT('Ctrl Pts',(-20.8509995807916,-18.9533322642405,
15.6876315233525));
#167201=CARTESIAN_POINT('Ctrl Pts',(-20.8510434832008,-18.8835702913221,
15.6915377254668));
#167202=CARTESIAN_POINT('Ctrl Pts',(-20.8476390986516,-18.813853334251,
15.6955212716884));
#167203=CARTESIAN_POINT('Ctrl Pts',(-20.8397874096428,-18.7341582859695,
15.7002202785958));
#167204=CARTESIAN_POINT('Ctrl Pts',(-20.8386998140563,-18.7238896888305,
15.7008284797941));
#167205=CARTESIAN_POINT('Ctrl Pts',(-20.8367367290434,-18.7065661363465,
15.7018593465851));
#167206=CARTESIAN_POINT('Ctrl Pts',(-20.8359007413786,-18.6995068226344,
15.7022807726844));
#167207=CARTESIAN_POINT('Ctrl Pts',(-20.8342952123103,-18.6865101421559,
15.703059191235));
#167208=CARTESIAN_POINT('Ctrl Pts',(-20.8335360061598,-18.6805715542189,
15.7034158550995));
#167209=CARTESIAN_POINT('Ctrl Pts',(-20.8319166972447,-18.6683185904104,
15.7041538110236));
#167210=CARTESIAN_POINT('Ctrl Pts',(-20.8310532538255,-18.6620047242297,
15.7045352051574));
#167211=CARTESIAN_POINT('Ctrl Pts',(-20.829051087632,-18.6478407310378,
15.70539337289));
#167212=CARTESIAN_POINT('Ctrl Pts',(-20.8278967296628,-18.6399929431577,
15.7058706368674));
#167213=CARTESIAN_POINT('Ctrl Pts',(-20.8248477064104,-18.6200438297961,
15.7070884616442));
#167214=CARTESIAN_POINT('Ctrl Pts',(-20.8228920894939,-18.6079522432944,
15.7078309441352));
#167215=CARTESIAN_POINT('Ctrl Pts',(-20.8108471705794,-18.5373703808585,
15.712190926308));
#167216=CARTESIAN_POINT('Ctrl Pts',(-20.7984074056688,-18.4793131503511,
15.7158825925014));
#167217=CARTESIAN_POINT('Ctrl Pts',(-20.7682273476263,-18.3626357677033,
15.7235218213669));
#167218=CARTESIAN_POINT('Ctrl Pts',(-20.7503497420336,-18.3041081380381,
15.7274702344468));
#167219=CARTESIAN_POINT('Ctrl Pts',(-20.7275382064969,-18.2395763771033,
15.731940929413));
#167220=CARTESIAN_POINT('Ctrl Pts',(-20.7250768450579,-18.2327260841001,
15.7324169989626));
#167221=CARTESIAN_POINT('Ctrl Pts',(-20.7225805680845,-18.2258895922541,
15.7328935628168));
#167222=CARTESIAN_POINT('Origin',(-18.734,-18.952,0.));
#167223=CARTESIAN_POINT('',(-20.7225806455427,-18.225889804387,16.7554729693871));
#167224=CARTESIAN_POINT('',(-20.7225805737622,-18.2258896078036,16.5356516434534));
#167225=CARTESIAN_POINT('',(-20.7225805737622,-18.2258896078036,0.));
#167226=CARTESIAN_POINT('Ctrl Pts',(-20.7225806455427,-18.225889804387,
16.7554729693871));
#167227=CARTESIAN_POINT('Ctrl Pts',(-20.7433304007774,-18.2827166633251,
16.7521870153233));
#167228=CARTESIAN_POINT('Ctrl Pts',(-20.7616464121081,-18.3404387186907,
16.7488940864294));
#167229=CARTESIAN_POINT('Ctrl Pts',(-20.8031161861311,-18.4936521079305,
16.7401351474939));
#167230=CARTESIAN_POINT('Ctrl Pts',(-20.8221382618788,-18.5900612993263,
16.7345999458387));
#167231=CARTESIAN_POINT('Ctrl Pts',(-20.8362368161789,-18.7019907840574,
16.727981337334));
#167232=CARTESIAN_POINT('Ctrl Pts',(-20.8379188844333,-18.7165651876537,
16.7271160006981));
#167233=CARTESIAN_POINT('Ctrl Pts',(-20.8402567486994,-18.7388535287691,
16.7257868384695));
#167234=CARTESIAN_POINT('Ctrl Pts',(-20.841021963568,-18.7465557198488,
16.7253264607647));
#167235=CARTESIAN_POINT('Ctrl Pts',(-20.842281502877,-18.759981493603,16.7245220637299));
#167236=CARTESIAN_POINT('Ctrl Pts',(-20.8427948029376,-18.7657032467542,
16.7241786455911));
#167237=CARTESIAN_POINT('Ctrl Pts',(-20.8438966146525,-18.7785735783429,
16.7234047859348));
#167238=CARTESIAN_POINT('Ctrl Pts',(-20.8444720950107,-18.7857231752158,
16.7229739387381));
#167239=CARTESIAN_POINT('Ctrl Pts',(-20.8459169689109,-18.8048914669959,
16.7218161867558));
#167240=CARTESIAN_POINT('Ctrl Pts',(-20.8467200883861,-18.8169147573708,
16.7210872104599));
#167241=CARTESIAN_POINT('Ctrl Pts',(-20.8498276623859,-18.870285691608,
16.7178385757437));
#167242=CARTESIAN_POINT('Ctrl Pts',(-20.8510211084486,-18.9116865688087,
16.7152844039434));
#167243=CARTESIAN_POINT('Ctrl Pts',(-20.850912165469,-19.1225723337198,
16.7020917815533));
#167244=CARTESIAN_POINT('Ctrl Pts',(-20.8304727788428,-19.2914051854431,
16.6908606080341));
#167245=CARTESIAN_POINT('Ctrl Pts',(-20.7654397479167,-19.5567378280083,
16.6728476439127));
#167246=CARTESIAN_POINT('Ctrl Pts',(-20.7333602044736,-19.6555759962661,
16.6660710908063));
#167247=CARTESIAN_POINT('Ctrl Pts',(-20.6904971169902,-19.7606419972116,
16.6590603002077));
#167248=CARTESIAN_POINT('Ctrl Pts',(-20.6867761538587,-19.769586784111,
16.6584650715421));
#167249=CARTESIAN_POINT('Ctrl Pts',(-20.6811908866164,-19.7827574721508,
16.6575913897736));
#167250=CARTESIAN_POINT('Ctrl Pts',(-20.6793740068196,-19.7870031742334,
16.6573101755078));
#167251=CARTESIAN_POINT('Ctrl Pts',(-20.6761257889957,-19.7945254915889,
16.6568127353112));
#167252=CARTESIAN_POINT('Ctrl Pts',(-20.6747000299203,-19.7978044566008,
16.6565961749707));
#167253=CARTESIAN_POINT('Ctrl Pts',(-20.6716271662102,-19.8048227597676,
16.6561332441046));
#167254=CARTESIAN_POINT('Ctrl Pts',(-20.6699775459862,-19.808560935894,
16.6558870300943));
#167255=CARTESIAN_POINT('Ctrl Pts',(-20.6654189081288,-19.8188107430203,
16.6552128510389));
#167256=CARTESIAN_POINT('Ctrl Pts',(-20.6624877614455,-19.8253125558148,
16.6547862198358));
#167257=CARTESIAN_POINT('Ctrl Pts',(-20.6466515931049,-19.8599714948498,
16.6525168352999));
#167258=CARTESIAN_POINT('Ctrl Pts',(-20.6331619290125,-19.8878592562669,
16.6507079280444));
#167259=CARTESIAN_POINT('Ctrl Pts',(-20.5446480453333,-20.0610448453689,
16.6395212795386));
#167260=CARTESIAN_POINT('Ctrl Pts',(-20.4536052813395,-20.1975508157827,
16.6308787629752));
#167261=CARTESIAN_POINT('Ctrl Pts',(-20.2715339080947,-20.4119803264541,
16.6154836238592));
#167262=CARTESIAN_POINT('Ctrl Pts',(-20.1879784152798,-20.4952091533928,
16.6089133731584));
#167263=CARTESIAN_POINT('Ctrl Pts',(-20.0870076676277,-20.5802701809529,
16.6011790515034));
#167264=CARTESIAN_POINT('Ctrl Pts',(-20.0759772262385,-20.5893730913118,
16.6003368740551));
#167265=CARTESIAN_POINT('Ctrl Pts',(-20.0582778839451,-20.6036805455875,
16.5989894230401));
#167266=CARTESIAN_POINT('Ctrl Pts',(-20.0516684376678,-20.6089581840788,
16.5984870967004));
#167267=CARTESIAN_POINT('Ctrl Pts',(-20.0399575021892,-20.6181949766471,
16.597598456269));
#167268=CARTESIAN_POINT('Ctrl Pts',(-20.0348691637174,-20.6221706844486,
16.597212809302));
#167269=CARTESIAN_POINT('Ctrl Pts',(-20.0243087507026,-20.6303443907801,
16.5964133438653));
#167270=CARTESIAN_POINT('Ctrl Pts',(-20.0188341977554,-20.6345390482035,
16.5959993996052));
#167271=CARTESIAN_POINT('Ctrl Pts',(-20.0047322523664,-20.6452351409896,
16.5949343429442));
#167272=CARTESIAN_POINT('Ctrl Pts',(-19.9960754940778,-20.6516973672864,
16.5942817035537));
#167273=CARTESIAN_POINT('Ctrl Pts',(-19.959764187597,-20.6783732256257,
16.5915487090691));
#167274=CARTESIAN_POINT('Ctrl Pts',(-19.9316718087257,-20.6979794904271,
16.5894450879867));
#167275=CARTESIAN_POINT('Ctrl Pts',(-19.8572712434404,-20.7472645789596,
16.5838981328216));
#167276=CARTESIAN_POINT('Ctrl Pts',(-19.8102625768518,-20.7758342151229,
16.5804165427932));
#167277=CARTESIAN_POINT('Ctrl Pts',(-19.6666536112232,-20.8556263228075,
16.5698575657444));
#167278=CARTESIAN_POINT('Ctrl Pts',(-19.5671477253852,-20.9012299337775,
16.5626317531228));
#167279=CARTESIAN_POINT('Ctrl Pts',(-19.4286088059413,-20.9521690157592,
16.552881044773));
#167280=CARTESIAN_POINT('Ctrl Pts',(-19.392289113875,-20.9644147255279,
16.5503534706963));
#167281=CARTESIAN_POINT('Ctrl Pts',(-19.3246456648601,-20.9851943145759,
16.5457174296647));
#167282=CARTESIAN_POINT('Ctrl Pts',(-19.2934188655449,-20.9940068800373,
16.5436047819984));
#167283=CARTESIAN_POINT('Ctrl Pts',(-19.25610976587,-21.0036158021435,16.5411216843684));
#167284=CARTESIAN_POINT('Ctrl Pts',(-19.2502120930008,-21.0051076648632,
16.5407303765171));
#167285=CARTESIAN_POINT('Ctrl Pts',(-19.201934124693,-21.0170987799747,
16.5375374567557));
#167286=CARTESIAN_POINT('Ctrl Pts',(-19.1592412847681,-21.0263109145861,
16.5347785708004));
#167287=CARTESIAN_POINT('Ctrl Pts',(-19.1088916453316,-21.0355550985196,
16.5316235776351));
#167288=CARTESIAN_POINT('Ctrl Pts',(-19.1014850874102,-21.0368741709515,
16.5311619582455));
#167289=CARTESIAN_POINT('Ctrl Pts',(-19.0895113834967,-21.0389408402356,
16.5304198760706));
#167290=CARTESIAN_POINT('Ctrl Pts',(-19.0849486182727,-21.039712979006,
16.5301380743789));
#167291=CARTESIAN_POINT('Ctrl Pts',(-19.0768549940912,-21.0410553473933,
16.5296399842439));
#167292=CARTESIAN_POINT('Ctrl Pts',(-19.0733251879188,-21.0416315964721,
16.5294233581386));
#167293=CARTESIAN_POINT('Ctrl Pts',(-19.0657655361668,-21.0428460668367,
16.5289607163303));
#167294=CARTESIAN_POINT('Ctrl Pts',(-19.0617353120279,-21.0434815830151,
16.5287148548996));
#167295=CARTESIAN_POINT('Ctrl Pts',(-19.0506819368636,-21.0451918282216,
16.52804263549));
#167296=CARTESIAN_POINT('Ctrl Pts',(-19.0436550991242,-21.0462428707567,
16.5276175984607));
#167297=CARTESIAN_POINT('Ctrl Pts',(-19.0063349687547,-21.051633102683,
16.5253717842882));
#167298=CARTESIAN_POINT('Ctrl Pts',(-18.9759538526256,-21.0553506732712,
16.5235840258274));
#167299=CARTESIAN_POINT('Ctrl Pts',(-18.8841163528689,-21.0645719285763,
16.5182730500866));
#167300=CARTESIAN_POINT('Ctrl Pts',(-18.8224868914983,-21.0680496800947,
16.5148337853914));
#167301=CARTESIAN_POINT('Ctrl Pts',(-18.6143119207719,-21.0706842330412,
16.5033847511416));
#167302=CARTESIAN_POINT('Ctrl Pts',(-18.4680405289909,-21.057330010441,
16.4955930882093));
#167303=CARTESIAN_POINT('Ctrl Pts',(-18.2502318366963,-21.0143674859086,
16.483203073728));
#167304=CARTESIAN_POINT('Ctrl Pts',(-18.1769878617819,-20.9958020841793,
16.4789020525457));
#167305=CARTESIAN_POINT('Ctrl Pts',(-18.092339907895,-20.9694573804946,
16.4737005392247));
#167306=CARTESIAN_POINT('Ctrl Pts',(-18.0798196479728,-20.9654323955079,
16.4729252095672));
#167307=CARTESIAN_POINT('Ctrl Pts',(-18.0595477196723,-20.9587063784519,
16.4716597749045));
#167308=CARTESIAN_POINT('Ctrl Pts',(-18.0517727126453,-20.9560764190143,
16.4711720123531));
#167309=CARTESIAN_POINT('Ctrl Pts',(-18.0379616925817,-20.9513150449416,
16.4703011813339));
#167310=CARTESIAN_POINT('Ctrl Pts',(-18.0319196520133,-20.9492013313395,
16.469918703543));
#167311=CARTESIAN_POINT('Ctrl Pts',(-18.0192156464425,-20.9446922609549,
16.4691112863063));
#167312=CARTESIAN_POINT('Ctrl Pts',(-18.0125559357631,-20.9422908278044,
16.4686861483788));
#167313=CARTESIAN_POINT('Ctrl Pts',(-17.9949886405581,-20.9358564589759,
16.4675596810414));
#167314=CARTESIAN_POINT('Ctrl Pts',(-17.9841021399848,-20.9317670141442,
16.4668564710611));
#167315=CARTESIAN_POINT('Ctrl Pts',(-17.9338560790471,-20.9124185035176,
16.4635865962899));
#167316=CARTESIAN_POINT('Ctrl Pts',(-17.8949270703928,-20.8960749010727,
16.4609837014544));
#167317=CARTESIAN_POINT('Ctrl Pts',(-17.7022848815273,-20.80833354588,16.4477412616152));
#167318=CARTESIAN_POINT('Ctrl Pts',(-17.5570685797906,-20.7198305109251,
16.4365104661703));
#167319=CARTESIAN_POINT('Ctrl Pts',(-17.3424662776604,-20.550777992831,
16.4184972078534));
#167320=CARTESIAN_POINT('Ctrl Pts',(-17.2657722325295,-20.4806495720731,
16.4117200331262));
#167321=CARTESIAN_POINT('Ctrl Pts',(-17.1878748806363,-20.3981258463336,
16.4047086835717));
#167322=CARTESIAN_POINT('Ctrl Pts',(-17.1812733680155,-20.3910353931278,
16.404113455817));
#167323=CARTESIAN_POINT('Ctrl Pts',(-17.1715970514039,-20.3804982858402,
16.4032397751254));
#167324=CARTESIAN_POINT('Ctrl Pts',(-17.1684845883978,-20.3770866020698,
16.4029585610351));
#167325=CARTESIAN_POINT('Ctrl Pts',(-17.1629821591379,-20.3710154079326,
16.4024611210324));
#167326=CARTESIAN_POINT('Ctrl Pts',(-17.1605877441662,-20.3683600030105,
16.4022445607113));
#167327=CARTESIAN_POINT('Ctrl Pts',(-17.1554714956469,-20.3626571007061,
16.401781629758));
#167328=CARTESIAN_POINT('Ctrl Pts',(-17.1527517613888,-20.3596077945813,
16.4015354156416));
#167329=CARTESIAN_POINT('Ctrl Pts',(-17.1453091422223,-20.3512145015766,
16.4008612359966));
#167330=CARTESIAN_POINT('Ctrl Pts',(-17.1406043566029,-20.3458544364128,
16.4004346043137));
#167331=CARTESIAN_POINT('Ctrl Pts',(-17.1156121589638,-20.3170894311429,
16.3981652126395));
#167332=CARTESIAN_POINT('Ctrl Pts',(-17.0958120028952,-20.2932638343221,
16.3963562989776));
#167333=CARTESIAN_POINT('Ctrl Pts',(-16.9748146182204,-20.1409885282248,
16.3851696252664));
#167334=CARTESIAN_POINT('Ctrl Pts',(-16.8882525121577,-20.0015977725196,
16.376527091936));
#167335=CARTESIAN_POINT('Ctrl Pts',(-16.7684483562408,-19.7470847110939,
16.3611319568612));
#167336=CARTESIAN_POINT('Ctrl Pts',(-16.7272828594526,-19.6365684268349,
16.3545617307249));
#167337=CARTESIAN_POINT('Ctrl Pts',(-16.6916599373497,-19.5094411172259,
16.346827436716));
#167338=CARTESIAN_POINT('Ctrl Pts',(-16.6879408231711,-19.4956316405894,
16.3459852595905));
#167339=CARTESIAN_POINT('Ctrl Pts',(-16.6822453265477,-19.47359687357,16.3446378089953));
#167340=CARTESIAN_POINT('Ctrl Pts',(-16.6801777928989,-19.4653954392108,
16.3441354827498));
#167341=CARTESIAN_POINT('Ctrl Pts',(-16.6766185543211,-19.4509110989956,
16.3432468424284));
#167342=CARTESIAN_POINT('Ctrl Pts',(-16.6751063363659,-19.4446333100251,
16.3428611954765));
#167343=CARTESIAN_POINT('Ctrl Pts',(-16.6720384352565,-19.4316363953371,
16.3420617300151));
#167344=CARTESIAN_POINT('Ctrl Pts',(-16.670486819531,-19.4249163969364,
16.3416477857149));
#167345=CARTESIAN_POINT('Ctrl Pts',(-16.6665891812606,-19.4076514089845,
16.3405827288332));
#167346=CARTESIAN_POINT('Ctrl Pts',(-16.6642910076633,-19.3970959224894,
16.3399300892607));
#167347=CARTESIAN_POINT('Ctrl Pts',(-16.655042903979,-19.3529984444207,
16.3371970930156));
#167348=CARTESIAN_POINT('Ctrl Pts',(-16.6488271141355,-19.3193093794526,
16.335093470317));
#167349=CARTESIAN_POINT('Ctrl Pts',(-16.6347687364804,-19.2311796972352,
16.3295465098757));
#167350=CARTESIAN_POINT('Ctrl Pts',(-16.628225824255,-19.1765606947516,
16.3260649160965));
#167351=CARTESIAN_POINT('Ctrl Pts',(-16.6150523778384,-19.0128023052817,
16.31550593184));
#167352=CARTESIAN_POINT('Ctrl Pts',(-16.6147394887864,-18.9033444449292,
16.3082801157851));
#167353=CARTESIAN_POINT('Ctrl Pts',(-16.6317147686931,-18.6760083004113,
16.2932208042183));
#167354=CARTESIAN_POINT('Ctrl Pts',(-16.6504903797373,-18.5585933039911,
16.2854153491064));
#167355=CARTESIAN_POINT('Ctrl Pts',(-16.681299499744,-18.4341194351724,
16.2774951671424));
#167356=CARTESIAN_POINT('Ctrl Pts',(-16.6836490795375,-18.4248940012532,
16.2769103820135));
#167357=CARTESIAN_POINT('Ctrl Pts',(-16.6872224857877,-18.4112488259812,
16.2760490572723));
#167358=CARTESIAN_POINT('Ctrl Pts',(-16.6883985325368,-18.4068168545214,
16.2757698657304));
#167359=CARTESIAN_POINT('Ctrl Pts',(-16.6905163956354,-18.3989389550257,
16.2752746531635));
#167360=CARTESIAN_POINT('Ctrl Pts',(-16.6914525416327,-18.3954915618333,
16.2750583089369));
#167361=CARTESIAN_POINT('Ctrl Pts',(-16.693483760298,-18.3880856949776,
16.2745943351165));
#167362=CARTESIAN_POINT('Ctrl Pts',(-16.6945816242233,-18.3841280451547,
16.274346869938));
#167363=CARTESIAN_POINT('Ctrl Pts',(-16.6976433006485,-18.3732145190731,
16.2736657266126));
#167364=CARTESIAN_POINT('Ctrl Pts',(-16.6996312499662,-18.3662653909507,
16.273233428569));
#167365=CARTESIAN_POINT('Ctrl Pts',(-16.7107070706989,-18.3282851370081,
16.2708777924707));
#167366=CARTESIAN_POINT('Ctrl Pts',(-16.7204699065066,-18.2974533415275,
16.268991421104));
#167367=CARTESIAN_POINT('Ctrl Pts',(-16.7836410857761,-18.1127683304777,
16.2577818114249));
#167368=CARTESIAN_POINT('Ctrl Pts',(-16.8539552330603,-17.9652612904372,
16.2491744108014));
#167369=CARTESIAN_POINT('Ctrl Pts',(-17.0025994125749,-17.728233323449,
16.2338581171959));
#167370=CARTESIAN_POINT('Ctrl Pts',(-17.0727897122348,-17.6345297020076,
16.227332724695));
#167371=CARTESIAN_POINT('Ctrl Pts',(-17.1598314465528,-17.5364129871619,
16.2196488940311));
#167372=CARTESIAN_POINT('Ctrl Pts',(-17.1694229890076,-17.5258190902483,
16.2188073366481));
#167373=CARTESIAN_POINT('Ctrl Pts',(-17.1848587356927,-17.509113369155,
16.217460692462));
#167374=CARTESIAN_POINT('Ctrl Pts',(-17.1906336750816,-17.5029379343191,
16.2169585473031));
#167375=CARTESIAN_POINT('Ctrl Pts',(-17.2008837715803,-17.4921077706464,
16.2160701179424));
#167376=CARTESIAN_POINT('Ctrl Pts',(-17.2053435465578,-17.4874385854138,
16.2156844998494));
#167377=CARTESIAN_POINT('Ctrl Pts',(-17.2146118821266,-17.4778235075864,
16.2148849868044));
#167378=CARTESIAN_POINT('Ctrl Pts',(-17.2194233902501,-17.4728805744747,
16.2144709655322));
#167379=CARTESIAN_POINT('Ctrl Pts',(-17.2318357897996,-17.4602532020903,
16.2134054844155));
#167380=CARTESIAN_POINT('Ctrl Pts',(-17.2394714603043,-17.4526033677739,
16.2127524952305));
#167381=CARTESIAN_POINT('Ctrl Pts',(-17.2715846280124,-17.4209196467429,
16.2100161127028));
#167382=CARTESIAN_POINT('Ctrl Pts',(-17.2965847734587,-17.3974251325252,
16.2079093811543));
#167383=CARTESIAN_POINT('Ctrl Pts',(-17.3632024511578,-17.3378007008676,
16.2023522685208));
#167384=CARTESIAN_POINT('Ctrl Pts',(-17.4056773673499,-17.3026718155528,
16.1988634565686));
#167385=CARTESIAN_POINT('Ctrl Pts',(-17.5364258213347,-17.2028653557094,
16.1882906043449));
#167386=CARTESIAN_POINT('Ctrl Pts',(-17.6283885083299,-17.1433331758317,
16.1810581842581));
#167387=CARTESIAN_POINT('Ctrl Pts',(-17.8286028055045,-17.0347197674754,
16.1660118140119));
#167388=CARTESIAN_POINT('Ctrl Pts',(-17.9372409669876,-16.9870854624434,
16.1582259124908));
#167389=CARTESIAN_POINT('Ctrl Pts',(-18.0583234426079,-16.9456996596702,
16.1503222336106));
#167390=CARTESIAN_POINT('Ctrl Pts',(-18.0673643776012,-16.9426775220053,
16.1497366565087));
#167391=CARTESIAN_POINT('Ctrl Pts',(-18.0807864631423,-16.9382914503205,
16.1488743939089));
#167392=CARTESIAN_POINT('Ctrl Pts',(-18.0851519853102,-16.9368805736297,
16.1485950482683));
#167393=CARTESIAN_POINT('Ctrl Pts',(-18.0929250020887,-16.9343963200008,
16.1480996665727));
#167394=CARTESIAN_POINT('Ctrl Pts',(-18.0963306550094,-16.9333173677835,
16.1478833064619));
#167395=CARTESIAN_POINT('Ctrl Pts',(-18.1036559237867,-16.9310170213546,
16.147419414766));
#167396=CARTESIAN_POINT('Ctrl Pts',(-18.1075763546096,-16.9297984097658,
16.1471720469845));
#167397=CARTESIAN_POINT('Ctrl Pts',(-18.1184013853841,-16.9264681000771,
16.1464914463911));
#167398=CARTESIAN_POINT('Ctrl Pts',(-18.1253133564909,-16.9243802858148,
16.1460595900522));
#167399=CARTESIAN_POINT('Ctrl Pts',(-18.1631324759223,-16.9131675463646,
16.1437108193451));
#167400=CARTESIAN_POINT('Ctrl Pts',(-18.1942360177133,-16.9047133560511,
16.1418306179178));
#167401=CARTESIAN_POINT('Ctrl Pts',(-18.3836962095876,-16.8578350236903,
16.1306206037636));
#167402=CARTESIAN_POINT('Ctrl Pts',(-18.5458760788671,-16.8370860438932,
16.1220085093624));
#167403=CARTESIAN_POINT('Ctrl Pts',(-18.8257588912867,-16.833760147858,
16.1066857054097));
#167404=CARTESIAN_POINT('Ctrl Pts',(-18.9425712162399,-16.8420586397392,
16.1001587624404));
#167405=CARTESIAN_POINT('Ctrl Pts',(-19.072215412372,-16.8621426911253,
16.0924731864519));
#167406=CARTESIAN_POINT('Ctrl Pts',(-19.0863153060788,-16.8644734380583,
16.0916316066258));
#167407=CARTESIAN_POINT('Ctrl Pts',(-19.1087177432724,-16.8684100448933,
16.090284933236));
#167408=CARTESIAN_POINT('Ctrl Pts',(-19.1170362825691,-16.8699232263875,
16.0897827815184));
#167409=CARTESIAN_POINT('Ctrl Pts',(-19.1316910479962,-16.8726797933575,
16.088894344518));
#167410=CARTESIAN_POINT('Ctrl Pts',(-19.1380311038229,-16.8739024187671,
16.0885087253806));
#167411=CARTESIAN_POINT('Ctrl Pts',(-19.1511326109341,-16.8764911544907,
16.087709214063));
#167412=CARTESIAN_POINT('Ctrl Pts',(-19.157893169326,-16.8778613445242,
16.0872951955818));
#167413=CARTESIAN_POINT('Ctrl Pts',(-19.1752291412896,-16.8814631942712,
16.0862297298473));
#167414=CARTESIAN_POINT('Ctrl Pts',(-19.1857942834094,-16.883742826026,
16.0855767533386));
#167415=CARTESIAN_POINT('Ctrl Pts',(-19.2298155706251,-16.8935946549533,
16.0828404936628));
#167416=CARTESIAN_POINT('Ctrl Pts',(-19.2631011082522,-16.90189818653,16.0807338749108));
#167417=CARTESIAN_POINT('Ctrl Pts',(-19.3492891962965,-16.9256377266945,
16.075177130733));
#167418=CARTESIAN_POINT('Ctrl Pts',(-19.4018141917393,-16.9423362862348,
16.0716885807934));
#167419=CARTESIAN_POINT('Ctrl Pts',(-19.6495378507836,-17.0318760899302,
16.0547574511729));
#167420=CARTESIAN_POINT('Ctrl Pts',(-19.8338998364072,-17.1312054412726,
16.0405669763651));
#167421=CARTESIAN_POINT('Ctrl Pts',(-20.0044080120687,-17.2585499789393,
16.0271505076349));
#167422=CARTESIAN_POINT('Ctrl Pts',(-20.0080261722787,-17.2612703338487,
16.0268657280972));
#167423=CARTESIAN_POINT('Ctrl Pts',(-20.0280040217407,-17.2763914514997,
16.025292962427));
#167424=CARTESIAN_POINT('Ctrl Pts',(-20.0441920761446,-17.2890185773859,
16.0240172720375));
#167425=CARTESIAN_POINT('Ctrl Pts',(-20.0652189659571,-17.3059177980897,
16.0223613761366));
#167426=CARTESIAN_POINT('Ctrl Pts',(-20.0702249728066,-17.3099788748926,
16.0219672316426));
#167427=CARTESIAN_POINT('Ctrl Pts',(-20.0782557868953,-17.3165548460233,
16.0213351779903));
#167428=CARTESIAN_POINT('Ctrl Pts',(-20.0812922245914,-17.3190553792589,
16.0210962568669));
#167429=CARTESIAN_POINT('Ctrl Pts',(-20.0869640811617,-17.323752793223,
16.0206501052632));
#167430=CARTESIAN_POINT('Ctrl Pts',(-20.0896011292765,-17.3259476177834,
16.0204427323188));
#167431=CARTESIAN_POINT('Ctrl Pts',(-20.0958375106931,-17.331163895237,
16.0199524288521));
#167432=CARTESIAN_POINT('Ctrl Pts',(-20.0994321632624,-17.334190959187,
16.0196699071926));
#167433=CARTESIAN_POINT('Ctrl Pts',(-20.1106650807128,-17.3437143291432,
16.0187872291092));
#167434=CARTESIAN_POINT('Ctrl Pts',(-20.1182674188441,-17.3502530582034,
16.0181900923124));
#167435=CARTESIAN_POINT('Ctrl Pts',(-20.1360932561222,-17.3658066717296,
16.0167897424049));
#167436=CARTESIAN_POINT('Ctrl Pts',(-20.1462768332242,-17.3748668604227,
16.0159895953197));
#167437=CARTESIAN_POINT('Ctrl Pts',(-20.1816926502187,-17.4069939564975,
16.0132034065174));
#167438=CARTESIAN_POINT('Ctrl Pts',(-20.2064541365772,-17.4305741061277,
16.0112490691357));
#167439=CARTESIAN_POINT('Ctrl Pts',(-20.284326716011,-17.50841442696,16.0050399557774));
#167440=CARTESIAN_POINT('Ctrl Pts',(-20.3350960491686,-17.5649365441214,
16.0008919511948));
#167441=CARTESIAN_POINT('Ctrl Pts',(-20.4906343550071,-17.7580482000638,
15.9874071572346));
#167442=CARTESIAN_POINT('Ctrl Pts',(-20.5818013803714,-17.9046660609108,
15.9781419429746));
#167443=CARTESIAN_POINT('Ctrl Pts',(-20.6640048012645,-18.0817643148415,
15.9667991612902));
#167444=CARTESIAN_POINT('Ctrl Pts',(-20.6734378070351,-18.1029949290666,
15.965438375539));
#167445=CARTESIAN_POINT('Ctrl Pts',(-20.6862667106885,-18.1331986957681,
15.9634992255069));
#167446=CARTESIAN_POINT('Ctrl Pts',(-20.6899541444026,-18.1420467508086,
15.9629307780299));
#167447=CARTESIAN_POINT('Ctrl Pts',(-20.6958419130385,-18.1564492490118,
15.9620047434131));
#167448=CARTESIAN_POINT('Ctrl Pts',(-20.6980790762592,-18.1619885632303,
15.961648406972));
#167449=CARTESIAN_POINT('Ctrl Pts',(-20.7027082004979,-18.1735916803545,
15.9609015928601));
#167450=CARTESIAN_POINT('Ctrl Pts',(-20.7050956576965,-18.1796572020561,
15.9605109679891));
#167451=CARTESIAN_POINT('Ctrl Pts',(-20.7107003736708,-18.1940916794411,
15.9595807886435));
#167452=CARTESIAN_POINT('Ctrl Pts',(-20.7138925340841,-18.2024701878809,
15.9590403984714));
#167453=CARTESIAN_POINT('Ctrl Pts',(-20.7189000460753,-18.2158686938571,
15.9581754212387));
#167454=CARTESIAN_POINT('Ctrl Pts',(-20.7207498043567,-18.2208757249084,
15.95785199894));
#167455=CARTESIAN_POINT('Ctrl Pts',(-20.7225805738037,-18.2258896079172,
15.9575279467182));
#167456=CARTESIAN_POINT('Ctrl Pts',(-20.7225805680844,-18.2258895922541,
15.7328935628168));
#167457=CARTESIAN_POINT('Ctrl Pts',(-20.6693404889608,-18.0800823077706,
15.7430576181593));
#167458=CARTESIAN_POINT('Ctrl Pts',(-20.600219906329,-17.9405553341241,
15.7534914468738));
#167459=CARTESIAN_POINT('Ctrl Pts',(-20.4987970870316,-17.7822775194804,
15.7654387928763));
#167460=CARTESIAN_POINT('Ctrl Pts',(-20.4805077342581,-17.7551414254491,
15.7674896854294));
#167461=CARTESIAN_POINT('Ctrl Pts',(-20.4574030229023,-17.7225189551059,
15.7699479745011));
#167462=CARTESIAN_POINT('Ctrl Pts',(-20.4531800205688,-17.71662083574,15.7703921327795));
#167463=CARTESIAN_POINT('Ctrl Pts',(-20.4465152606251,-17.7074127602526,
15.7710849267591));
#167464=CARTESIAN_POINT('Ctrl Pts',(-20.444094078235,-17.7040880802449,
15.7713349400436));
#167465=CARTESIAN_POINT('Ctrl Pts',(-20.4395523386009,-17.6978895680709,
15.771800790781));
#167466=CARTESIAN_POINT('Ctrl Pts',(-20.4374342212101,-17.6950140774759,
15.7720167848616));
#167467=CARTESIAN_POINT('Ctrl Pts',(-20.4325851774586,-17.6884659322428,
15.7725084082));
#167468=CARTESIAN_POINT('Ctrl Pts',(-20.4298496174517,-17.6847967718805,
15.7727837098655));
#167469=CARTESIAN_POINT('Ctrl Pts',(-20.4214139000893,-17.6735583258191,
15.7736265114171));
#167470=CARTESIAN_POINT('Ctrl Pts',(-20.4156747152556,-17.6660182955739,
15.7741913527461));
#167471=CARTESIAN_POINT('Ctrl Pts',(-20.3358231113844,-17.5625595777808,
15.7819371900118));
#167472=CARTESIAN_POINT('Ctrl Pts',(-20.2536450104188,-17.4731255568374,
15.7885861201467));
#167473=CARTESIAN_POINT('Ctrl Pts',(-20.0843244631099,-17.3179664642329,
15.8010832541351));
#167474=CARTESIAN_POINT('Ctrl Pts',(-19.9988904749386,-17.2509730015323,
15.8069253952696));
#167475=CARTESIAN_POINT('Ctrl Pts',(-19.8637962840653,-17.1608653170644,
15.8159630588426));
#167476=CARTESIAN_POINT('Ctrl Pts',(-19.817760545941,-17.1326414419455,
15.8190095450046));
#167477=CARTESIAN_POINT('Ctrl Pts',(-19.7511164034378,-17.095210388649,
15.8234090042272));
#167478=CARTESIAN_POINT('Ctrl Pts',(-19.7313607677121,-17.084524462379,
15.8247117570074));
#167479=CARTESIAN_POINT('Ctrl Pts',(-19.6962617628501,-17.0662550354213,
15.82702619618));
#167480=CARTESIAN_POINT('Ctrl Pts',(-19.6809892769589,-17.0585393969076,
15.8280332281916));
#167481=CARTESIAN_POINT('Ctrl Pts',(-19.6582661738927,-17.0474034015377,
15.8295321841298));
#167482=CARTESIAN_POINT('Ctrl Pts',(-19.6508862813413,-17.0438397060831,
15.8300191058044));
#167483=CARTESIAN_POINT('Ctrl Pts',(-19.6379544133566,-17.0376873447261,
15.8308725939925));
#167484=CARTESIAN_POINT('Ctrl Pts',(-19.6324115153633,-17.0350797430739,
15.8312384983682));
#167485=CARTESIAN_POINT('Ctrl Pts',(-19.6213453955741,-17.0299323359772,
15.8319692000979));
#167486=CARTESIAN_POINT('Ctrl Pts',(-19.6158223956264,-17.02739219125,15.8323339813512));
#167487=CARTESIAN_POINT('Ctrl Pts',(-19.6025844323973,-17.021372715966,
15.8332085796982));
#167488=CARTESIAN_POINT('Ctrl Pts',(-19.5948594403423,-17.0179158118689,
15.8337191620677));
#167489=CARTESIAN_POINT('Ctrl Pts',(-19.5668565065813,-17.0055856124753,
15.8355709046529));
#167490=CARTESIAN_POINT('Ctrl Pts',(-19.5464609881557,-16.9969843957482,
15.8369212966272));
#167491=CARTESIAN_POINT('Ctrl Pts',(-19.3540550539053,-16.9193735591264,
15.8496805843615));
#167492=CARTESIAN_POINT('Ctrl Pts',(-19.1738451659808,-16.8729263471608,
15.8618862752345));
#167493=CARTESIAN_POINT('Ctrl Pts',(-18.9102072121805,-16.8408174010051,
15.8794212657179));
#167494=CARTESIAN_POINT('Ctrl Pts',(-18.8299787501099,-16.8356515527881,
15.8846992286326));
#167495=CARTESIAN_POINT('Ctrl Pts',(-18.7135698354324,-16.8347911808613,
15.8921203730578));
#167496=CARTESIAN_POINT('Ctrl Pts',(-18.6774899759871,-16.8354467754887,
15.8943870852074));
#167497=CARTESIAN_POINT('Ctrl Pts',(-18.633980135916,-16.8373509002736,
15.8970664865295));
#167498=CARTESIAN_POINT('Ctrl Pts',(-18.6265197812475,-16.8377169549504,
15.8975239812815));
#167499=CARTESIAN_POINT('Ctrl Pts',(-18.6149075998526,-16.8383483481803,
15.8982329183928));
#167500=CARTESIAN_POINT('Ctrl Pts',(-18.6107544394904,-16.8385864490083,
15.8984858435178));
#167501=CARTESIAN_POINT('Ctrl Pts',(-18.6030426460603,-16.8390513763321,
15.8989542828912));
#167502=CARTESIAN_POINT('Ctrl Pts',(-18.5994839178959,-16.8392749495632,
15.8991699711456));
#167503=CARTESIAN_POINT('Ctrl Pts',(-18.5914257708345,-16.8398016369341,
15.8996572865141));
#167504=CARTESIAN_POINT('Ctrl Pts',(-18.586926757062,-16.8401101359595,
15.8999286086305));
#167505=CARTESIAN_POINT('Ctrl Pts',(-18.575314335671,-16.8409436920978,
15.9006270478957));
#167506=CARTESIAN_POINT('Ctrl Pts',(-18.5682024680538,-16.8414903324418,
15.9010529837413));
#167507=CARTESIAN_POINT('Ctrl Pts',(-18.5245759179977,-16.8450654887221,
15.9036554211107));
#167508=CARTESIAN_POINT('Ctrl Pts',(-18.4881397919416,-16.8490058007657,
15.905784243566));
#167509=CARTESIAN_POINT('Ctrl Pts',(-18.2827363879426,-16.8766308252548,
15.9176236651224));
#167510=CARTESIAN_POINT('Ctrl Pts',(-18.1170048105963,-16.9197290810761,
15.9266000128124));
#167511=CARTESIAN_POINT('Ctrl Pts',(-17.8695282265188,-17.0171960535051,
15.941231328725));
#167512=CARTESIAN_POINT('Ctrl Pts',(-17.783295613102,-17.0580792365382,
15.9465768614697));
#167513=CARTESIAN_POINT('Ctrl Pts',(-17.6814560607314,-17.1150738845568,
15.9533725383239));
#167514=CARTESIAN_POINT('Ctrl Pts',(-17.6629550070717,-17.125799334274,
15.9546273284147));
#167515=CARTESIAN_POINT('Ctrl Pts',(-17.6368957528842,-17.1414386433616,
15.9564251174629));
#167516=CARTESIAN_POINT('Ctrl Pts',(-17.6292011797927,-17.1461235595312,
15.9569597801513));
#167517=CARTESIAN_POINT('Ctrl Pts',(-17.6159843405472,-17.1542868480853,
15.9578848880821));
#167518=CARTESIAN_POINT('Ctrl Pts',(-17.6104477852283,-17.1577419331212,
15.9582744725098));
#167519=CARTESIAN_POINT('Ctrl Pts',(-17.5998814575152,-17.1644039287878,
15.9590219656223));
#167520=CARTESIAN_POINT('Ctrl Pts',(-17.5948490827513,-17.1676066104076,
15.9593797148631));
#167521=CARTESIAN_POINT('Ctrl Pts',(-17.5818067783103,-17.1759845939957,
15.9603114683245));
#167522=CARTESIAN_POINT('Ctrl Pts',(-17.5738182287436,-17.181192784219,
15.9608866963878));
#167523=CARTESIAN_POINT('Ctrl Pts',(-17.546740597358,-17.1991081118468,
15.9628520900761));
#167524=CARTESIAN_POINT('Ctrl Pts',(-17.5278234312205,-17.2120710127303,
15.9642518475003));
#167525=CARTESIAN_POINT('Ctrl Pts',(-17.3653109714664,-17.327355942597,
15.9765153748533));
#167526=CARTESIAN_POINT('Ctrl Pts',(-17.2348351460839,-17.4469222779745,
15.9880903961454));
#167527=CARTESIAN_POINT('Ctrl Pts',(-17.0647462974219,-17.647104803255,
16.0054455463183));
#167528=CARTESIAN_POINT('Ctrl Pts',(-17.0128643256578,-17.7163409489386,
16.0111404585931));
#167529=CARTESIAN_POINT('Ctrl Pts',(-16.9446526771664,-17.8200350665684,
16.0190638518097));
#167530=CARTESIAN_POINT('Ctrl Pts',(-16.9247896830059,-17.8520605076755,
16.021433516982));
#167531=CARTESIAN_POINT('Ctrl Pts',(-16.9019773457206,-17.8911328085888,
16.0242176105003));
#167532=CARTESIAN_POINT('Ctrl Pts',(-16.8981988637378,-17.8976848688987,
16.0246809407275));
#167533=CARTESIAN_POINT('Ctrl Pts',(-16.892386545359,-17.9078896803595,
16.0253969321961));
#167534=CARTESIAN_POINT('Ctrl Pts',(-16.8903283219204,-17.911528366538,
16.0256511232538));
#167535=CARTESIAN_POINT('Ctrl Pts',(-16.886535415185,-17.918280352754,16.0261207212314));
#167536=CARTESIAN_POINT('Ctrl Pts',(-16.8847978302417,-17.9213919091592,
16.0263363096318));
#167537=CARTESIAN_POINT('Ctrl Pts',(-16.880892563893,-17.9284268851611,
16.0268219028805));
#167538=CARTESIAN_POINT('Ctrl Pts',(-16.8787294867131,-17.9323527989771,
16.0270916119162));
#167539=CARTESIAN_POINT('Ctrl Pts',(-16.8723969817171,-17.9439329523265,
16.0278834921752));
#167540=CARTESIAN_POINT('Ctrl Pts',(-16.868262278401,-17.9516062123351,
16.0284035013328));
#167541=CARTESIAN_POINT('Ctrl Pts',(-16.8391906225886,-18.0063651315831,
16.0320826491193));
#167542=CARTESIAN_POINT('Ctrl Pts',(-16.8159894888871,-18.0543560969524,
16.0351406523154));
#167543=CARTESIAN_POINT('Ctrl Pts',(-16.7878975794551,-18.1185399500332,
16.039081030343));
#167544=CARTESIAN_POINT('Ctrl Pts',(-16.7813556003007,-18.1339840128234,
16.0400180910657));
#167545=CARTESIAN_POINT('Ctrl Pts',(-16.7185790792292,-18.2872301580459,
16.0492220961055));
#167546=CARTESIAN_POINT('Ctrl Pts',(-16.6768402139197,-18.4305236918782,
16.0571116269683));
#167547=CARTESIAN_POINT('Ctrl Pts',(-16.6395590291366,-18.6376689096515,
16.0687567174571));
#167548=CARTESIAN_POINT('Ctrl Pts',(-16.631297263296,-18.6987661894777,
16.0722153770887));
#167549=CARTESIAN_POINT('Ctrl Pts',(-16.6223427137143,-18.7971616116903,
16.0778857802934));
#167550=CARTESIAN_POINT('Ctrl Pts',(-16.6199491887369,-18.8342700529912,
16.0800466926872));
#167551=CARTESIAN_POINT('Ctrl Pts',(-16.6181105876072,-18.8825392484015,
16.0828941370441));
#167552=CARTESIAN_POINT('Ctrl Pts',(-16.6177747445232,-18.8936607985675,
16.0835527146772));
#167553=CARTESIAN_POINT('Ctrl Pts',(-16.6173711819886,-18.9117507508806,
16.0846282065509));
#167554=CARTESIAN_POINT('Ctrl Pts',(-16.6172501679848,-18.9187178400606,
16.0850434465598));
#167555=CARTESIAN_POINT('Ctrl Pts',(-16.6170836099393,-18.9321163066294,
16.0858440276361));
#167556=CARTESIAN_POINT('Ctrl Pts',(-16.6170329728605,-18.9385475519692,
16.086229204508));
#167557=CARTESIAN_POINT('Ctrl Pts',(-16.6169841377923,-18.9532721511588,
16.0871131832957));
#167558=CARTESIAN_POINT('Ctrl Pts',(-16.6170053663742,-18.9615654247404,
16.0876125887117));
#167559=CARTESIAN_POINT('Ctrl Pts',(-16.6171912048053,-18.9835947699358,
16.0889433004205));
#167560=CARTESIAN_POINT('Ctrl Pts',(-16.6174407822385,-18.9973295560186,
16.0897772527229));
#167561=CARTESIAN_POINT('Ctrl Pts',(-16.6203578225619,-19.1018486626708,
16.0961570487287));
#167562=CARTESIAN_POINT('Ctrl Pts',(-16.6287309930167,-19.1923674174292,
16.1018814117833));
#167563=CARTESIAN_POINT('Ctrl Pts',(-16.6648011226226,-19.4208919264391,
16.1168225464823));
#167564=CARTESIAN_POINT('Ctrl Pts',(-16.700485727514,-19.5571928642288,
16.1262165228961));
#167565=CARTESIAN_POINT('Ctrl Pts',(-16.7682471058372,-19.739676349936,
16.1389575964096));
#167566=CARTESIAN_POINT('Ctrl Pts',(-16.7890284005296,-19.7896781894948,
16.1424627236111));
#167567=CARTESIAN_POINT('Ctrl Pts',(-16.8234687220353,-19.8643309967244,
16.1476642188366));
#167568=CARTESIAN_POINT('Ctrl Pts',(-16.8357395311062,-19.889595318648,
16.1494187191127));
#167569=CARTESIAN_POINT('Ctrl Pts',(-16.8516528118022,-19.9207651072571,
16.1515692437521));
#167570=CARTESIAN_POINT('Ctrl Pts',(-16.8548257160725,-19.9269055254869,
16.1519922022534));
#167571=CARTESIAN_POINT('Ctrl Pts',(-16.8598995416166,-19.9366079274268,
16.1526592814996));
#167572=CARTESIAN_POINT('Ctrl Pts',(-16.8617806452694,-19.9401801390771,
16.1529046193221));
#167573=CARTESIAN_POINT('Ctrl Pts',(-16.8653513822066,-19.9469141644755,
16.1533665741894));
#167574=CARTESIAN_POINT('Ctrl Pts',(-16.8670388066997,-19.9500770282594,
16.1535833193056));
#167575=CARTESIAN_POINT('Ctrl Pts',(-16.8709199733089,-19.9573075008329,
16.1540783098381));
#167576=CARTESIAN_POINT('Ctrl Pts',(-16.8731190036609,-19.9613722184989,
16.1543562153446));
#167577=CARTESIAN_POINT('Ctrl Pts',(-16.879002574489,-19.972162910879,16.155093103112));
#167578=CARTESIAN_POINT('Ctrl Pts',(-16.8827104212753,-19.9788761917194,
16.1555506412396));
#167579=CARTESIAN_POINT('Ctrl Pts',(-16.909226066583,-20.0262739380936,
16.1587756194034));
#167580=CARTESIAN_POINT('Ctrl Pts',(-16.9333382691052,-20.0662183091007,
16.1614653709725));
#167581=CARTESIAN_POINT('Ctrl Pts',(-16.9612209659845,-20.1091361318867,
16.164360546137));
#167582=CARTESIAN_POINT('Ctrl Pts',(-16.9637017233245,-20.1129278802964,
16.1646163768893));
#167583=CARTESIAN_POINT('Ctrl Pts',(-16.9790315977765,-20.1361956426712,
16.1661867222183));
#167584=CARTESIAN_POINT('Ctrl Pts',(-16.9921901196731,-20.1554665800866,
16.1674893203714));
#167585=CARTESIAN_POINT('Ctrl Pts',(-17.0319413225092,-20.2116649217534,
16.1713057961291));
#167586=CARTESIAN_POINT('Ctrl Pts',(-17.0594094141591,-20.2479575840421,
16.1737938546244));
#167587=CARTESIAN_POINT('Ctrl Pts',(-17.1567932397521,-20.3683561853195,
16.182224685891));
#167588=CARTESIAN_POINT('Ctrl Pts',(-17.232043158185,-20.447918035758,16.1881126943056));
#167589=CARTESIAN_POINT('Ctrl Pts',(-17.353949655852,-20.5582960325788,
16.197256840454));
#167590=CARTESIAN_POINT('Ctrl Pts',(-17.3962267946189,-20.5936723492566,
16.20036424792));
#167591=CARTESIAN_POINT('Ctrl Pts',(-17.4669834775263,-20.6483298863517,
16.2055080947614));
#167592=CARTESIAN_POINT('Ctrl Pts',(-17.4946377878849,-20.6686383026581,
16.2075051497761));
#167593=CARTESIAN_POINT('Ctrl Pts',(-17.5316371049999,-20.6944492242487,
16.2101657318742));
#167594=CARTESIAN_POINT('Ctrl Pts',(-17.5405490926554,-20.7005653420898,
16.2108057320983));
#167595=CARTESIAN_POINT('Ctrl Pts',(-17.5552247318944,-20.7104724768369,
16.2118584314054));
#167596=CARTESIAN_POINT('Ctrl Pts',(-17.5609608381677,-20.7143040905492,
16.2122695892469));
#167597=CARTESIAN_POINT('Ctrl Pts',(-17.5721021383834,-20.7216677795498,
16.2130676568961));
#167598=CARTESIAN_POINT('Ctrl Pts',(-17.5775049724133,-20.7252032992696,
16.2134544313362));
#167599=CARTESIAN_POINT('Ctrl Pts',(-17.5900196128839,-20.7333111343143,
16.2143498149645));
#167600=CARTESIAN_POINT('Ctrl Pts',(-17.5971427696027,-20.7378656494239,
16.214859080305));
#167601=CARTESIAN_POINT('Ctrl Pts',(-17.616378334742,-20.7500030651019,
16.2162334099759));
#167602=CARTESIAN_POINT('Ctrl Pts',(-17.6285403941042,-20.757506093256,
16.2171014025143));
#167603=CARTESIAN_POINT('Ctrl Pts',(-17.7408543730624,-20.8252347014787,
16.2251097131299));
#167604=CARTESIAN_POINT('Ctrl Pts',(-17.8457401892452,-20.8771839345009,
16.2325518997681));
#167605=CARTESIAN_POINT('Ctrl Pts',(-18.105691032488,-20.9801545905997,
16.2508154736347));
#167606=CARTESIAN_POINT('Ctrl Pts',(-18.2634255268701,-21.0224451085997,
16.2617770366288));
#167607=CARTESIAN_POINT('Ctrl Pts',(-18.4565507487976,-21.0509912109393,
16.2741813302676));
#167608=CARTESIAN_POINT('Ctrl Pts',(-18.4887618004647,-21.0549980226765,
16.2762152558618));
#167609=CARTESIAN_POINT('Ctrl Pts',(-18.5282533591424,-21.0589906685718,
16.2786560612136));
#167610=CARTESIAN_POINT('Ctrl Pts',(-18.5354563245833,-21.0596816102314,
16.2790991018273));
#167611=CARTESIAN_POINT('Ctrl Pts',(-18.5467548382939,-21.0607069810728,
16.2797905416686));
#167612=CARTESIAN_POINT('Ctrl Pts',(-18.5508479795884,-21.0610664334463,
16.2800403098128));
#167613=CARTESIAN_POINT('Ctrl Pts',(-18.5585013851382,-21.0617160935517,
16.2805059478559));
#167614=CARTESIAN_POINT('Ctrl Pts',(-18.5620612980682,-21.0620092042967,
16.2807219729064));
#167615=CARTESIAN_POINT('Ctrl Pts',(-18.5701900823374,-21.0626577910543,
16.2812139827468));
#167616=CARTESIAN_POINT('Ctrl Pts',(-18.5747593678951,-21.0630074424445,
16.2814896379402));
#167617=CARTESIAN_POINT('Ctrl Pts',(-18.5888102154943,-21.0640367627134,
16.2823345988338));
#167618=CARTESIAN_POINT('Ctrl Pts',(-18.5982953992801,-21.0646674204766,
16.2829012261454));
#167619=CARTESIAN_POINT('Ctrl Pts',(-18.6836895437452,-21.0697676819452,
16.2879711442723));
#167620=CARTESIAN_POINT('Ctrl Pts',(-18.759792488342,-21.070208786245,16.2922672311556));
#167621=CARTESIAN_POINT('Ctrl Pts',(-18.8781838246555,-21.0645112577357,
16.2988268320853));
#167622=CARTESIAN_POINT('Ctrl Pts',(-18.9205358367219,-21.0611935314556,
16.3011484604701));
#167623=CARTESIAN_POINT('Ctrl Pts',(-19.0714391604339,-21.0447910662302,
16.3094125077734));
#167624=CARTESIAN_POINT('Ctrl Pts',(-19.1790386628083,-21.0245779443096,
16.3152990895486));
#167625=CARTESIAN_POINT('Ctrl Pts',(-19.3377693422375,-20.9818237867634,
16.3244399190603));
#167626=CARTESIAN_POINT('Ctrl Pts',(-19.3903645828794,-20.9654316263566,
16.3275454255471));
#167627=CARTESIAN_POINT('Ctrl Pts',(-19.4745732360926,-20.9355362720992,
16.3326864061115));
#167628=CARTESIAN_POINT('Ctrl Pts',(-19.506603093924,-20.9232810869314,
16.3346825533624));
#167629=CARTESIAN_POINT('Ctrl Pts',(-19.5483165348401,-20.9061479913124,
16.3373420974504));
#167630=CARTESIAN_POINT('Ctrl Pts',(-19.5582814103397,-20.901965625563,
16.3379819908532));
#167631=CARTESIAN_POINT('Ctrl Pts',(-19.5745533211271,-20.8949891130161,
16.3390345592115));
#167632=CARTESIAN_POINT('Ctrl Pts',(-19.5808795728355,-20.8922400795622,
16.3394456936781));
#167633=CARTESIAN_POINT('Ctrl Pts',(-19.5931016139735,-20.8868579042829,
16.3402437479494));
#167634=CARTESIAN_POINT('Ctrl Pts',(-19.5989990200743,-20.8842286062305,
16.3406305325559));
#167635=CARTESIAN_POINT('Ctrl Pts',(-19.6125913968172,-20.8780938859456,
16.3415259863345));
#167636=CARTESIAN_POINT('Ctrl Pts',(-19.620277539638,-20.8745692756129,
16.3420353119828));
#167637=CARTESIAN_POINT('Ctrl Pts',(-19.6408989794062,-20.8649630282152,
16.3434099099331));
#167638=CARTESIAN_POINT('Ctrl Pts',(-19.6537939665719,-20.8587963576363,
16.3442781122221));
#167639=CARTESIAN_POINT('Ctrl Pts',(-19.7717737012449,-20.8009005932817,
16.3523026300373));
#167640=CARTESIAN_POINT('Ctrl Pts',(-19.8724412996336,-20.7406730294043,
16.3597622333303));
#167641=CARTESIAN_POINT('Ctrl Pts',(-20.1005658692126,-20.5771018974074,
16.3780997130634));
#167642=CARTESIAN_POINT('Ctrl Pts',(-20.222027613262,-20.4666724019441,
16.3891199844154));
#167643=CARTESIAN_POINT('Ctrl Pts',(-20.3502424320361,-20.3196401927744,
16.4015038056873));
#167644=CARTESIAN_POINT('Ctrl Pts',(-20.3703947119184,-20.2954626485046,
16.403474702757));
#167645=CARTESIAN_POINT('Ctrl Pts',(-20.3944666551621,-20.2652367863771,
16.4058504237192));
#167646=CARTESIAN_POINT('Ctrl Pts',(-20.3989032864566,-20.2596075176184,
16.4062892167495));
#167647=CARTESIAN_POINT('Ctrl Pts',(-20.4058289727061,-20.2507277023311,
16.4069755086302));
#167648=CARTESIAN_POINT('Ctrl Pts',(-20.4083372859219,-20.2474923436321,
16.407224343668));
#167649=CARTESIAN_POINT('Ctrl Pts',(-20.4130180216304,-20.2414185738344,
16.407689180096));
#167650=CARTESIAN_POINT('Ctrl Pts',(-20.4151926158865,-20.2385819694111,
16.4079053309998));
#167651=CARTESIAN_POINT('Ctrl Pts',(-20.4201529718949,-20.2320774852705,
16.4083988484328));
#167652=CARTESIAN_POINT('Ctrl Pts',(-20.4229339498758,-20.2284060195732,
16.4086758775802));
#167653=CARTESIAN_POINT('Ctrl Pts',(-20.4301820138803,-20.2187719141843,
16.4093988859359));
#167654=CARTESIAN_POINT('Ctrl Pts',(-20.4346296891585,-20.2127946584717,
16.4098435411797));
#167655=CARTESIAN_POINT('Ctrl Pts',(-20.4640847617239,-20.172770360006,
16.412795880125));
#167656=CARTESIAN_POINT('Ctrl Pts',(-20.4881016525195,-20.1380023128013,
16.4152399558393));
#167657=CARTESIAN_POINT('Ctrl Pts',(-20.5515193138918,-20.0400504068208,
16.4218683294491));
#167658=CARTESIAN_POINT('Ctrl Pts',(-20.5886539074199,-19.9754698403651,
16.4259560558961));
#167659=CARTESIAN_POINT('Ctrl Pts',(-20.6728522487848,-19.8093443013035,
16.4361043156865));
#167660=CARTESIAN_POINT('Ctrl Pts',(-20.7154134942979,-19.7057818601762,
16.4421169431856));
#167661=CARTESIAN_POINT('Ctrl Pts',(-20.7754133653133,-19.5189637878021,
16.4530200566841));
#167662=CARTESIAN_POINT('Ctrl Pts',(-20.7963949740725,-19.4371195748214,
16.4578124645552));
#167663=CARTESIAN_POINT('Ctrl Pts',(-20.8151326638564,-19.3403009459394,
16.46360140908));
#167664=CARTESIAN_POINT('Ctrl Pts',(-20.8176912864146,-19.326327927584,
16.4644396207964));
#167665=CARTESIAN_POINT('Ctrl Pts',(-20.8214097413267,-19.3048001825602,
16.4657356371529));
#167666=CARTESIAN_POINT('Ctrl Pts',(-20.8226696398739,-19.2972629869016,
16.4661902581937));
#167667=CARTESIAN_POINT('Ctrl Pts',(-20.8248931361382,-19.2835034506971,
16.4670218343697));
#167668=CARTESIAN_POINT('Ctrl Pts',(-20.8258698386487,-19.2772832940697,
16.467398368603));
#167669=CARTESIAN_POINT('Ctrl Pts',(-20.8279419770617,-19.2636914154738,
16.4682225180916));
#167670=CARTESIAN_POINT('Ctrl Pts',(-20.8290262606143,-19.2563181015063,
16.4686704816853));
#167671=CARTESIAN_POINT('Ctrl Pts',(-20.8318905540241,-19.2360992748401,
16.4699013512523));
#167672=CARTESIAN_POINT('Ctrl Pts',(-20.8335914772361,-19.2232430489611,
16.4706867456919));
#167673=CARTESIAN_POINT('Ctrl Pts',(-20.8416314801174,-19.1578589077599,
16.4746955887798));
#167674=CARTESIAN_POINT('Ctrl Pts',(-20.846117415472,-19.1051260510563,
16.4779768670436));
#167675=CARTESIAN_POINT('Ctrl Pts',(-20.8502336389003,-19.018329912382,
16.4834601303997));
#167676=CARTESIAN_POINT('Ctrl Pts',(-20.8510257893228,-18.9843434163513,
16.4856276880682));
#167677=CARTESIAN_POINT('Ctrl Pts',(-20.8508977919258,-18.8197312346676,
16.4962189028986));
#167678=CARTESIAN_POINT('Ctrl Pts',(-20.8387067143781,-18.6894054886347,
16.5049104438664));
#167679=CARTESIAN_POINT('Ctrl Pts',(-20.7970384719494,-18.4676530630201,
16.5197603527283));
#167680=CARTESIAN_POINT('Ctrl Pts',(-20.7732180773672,-18.3755335280661,
16.525940140316));
#167681=CARTESIAN_POINT('Ctrl Pts',(-20.7402342466764,-18.2761250472743,
16.5324112063177));
#167682=CARTESIAN_POINT('Ctrl Pts',(-20.7371210647758,-18.2669534232681,
16.5330062931116));
#167683=CARTESIAN_POINT('Ctrl Pts',(-20.7324307947245,-18.2534409967208,
16.5338798071661));
#167684=CARTESIAN_POINT('Ctrl Pts',(-20.7309023230061,-18.2490836211387,
16.534160994092));
#167685=CARTESIAN_POINT('Ctrl Pts',(-20.728165063312,-18.2413612139805,
16.534658404075));
#167686=CARTESIAN_POINT('Ctrl Pts',(-20.7269619965586,-18.2379942122916,
16.5348749613903));
#167687=CARTESIAN_POINT('Ctrl Pts',(-20.7247001831083,-18.2317143719838,
16.5352782673501));
#167688=CARTESIAN_POINT('Ctrl Pts',(-20.7236435792586,-18.2288008346675,
16.5354651435967));
#167689=CARTESIAN_POINT('Ctrl Pts',(-20.7225805737622,-18.2258896078036,
16.5356516434534));
#167690=CARTESIAN_POINT('Origin',(-18.734,-18.952,0.));
#167691=CARTESIAN_POINT('',(-20.7225805855593,-18.2258896401121,17.5536949999931));
#167692=CARTESIAN_POINT('',(-20.7225805737355,-18.2258896077305,17.3329786086887));
#167693=CARTESIAN_POINT('',(-20.7225805737622,-18.2258896078036,0.));
#167694=CARTESIAN_POINT('',(-20.850999020182,-18.9502127631604,17.5117109399533));
#167695=CARTESIAN_POINT('Ctrl Pts',(-20.7225805855593,-18.2258896401121,
17.553694999993));
#167696=CARTESIAN_POINT('Ctrl Pts',(-20.7266285790002,-18.2369757801973,
17.552950415919));
#167697=CARTESIAN_POINT('Ctrl Pts',(-20.7305846696713,-18.2480979710921,
17.5522097264263));
#167698=CARTESIAN_POINT('Ctrl Pts',(-20.7395043458259,-18.2738554344083,
17.5505098677726));
#167699=CARTESIAN_POINT('Ctrl Pts',(-20.7444005421372,-18.2885111719396,
17.5495541086848));
#167700=CARTESIAN_POINT('Ctrl Pts',(-20.750899367023,-18.3086967657258,
17.5482546361465));
#167701=CARTESIAN_POINT('Ctrl Pts',(-20.7526404209504,-18.3141810910543,
17.5479032786566));
#167702=CARTESIAN_POINT('Ctrl Pts',(-20.7553758462965,-18.3229210900391,
17.5473461274144));
#167703=CARTESIAN_POINT('Ctrl Pts',(-20.7563847482496,-18.3261721343886,
17.5471394933976));
#167704=CARTESIAN_POINT('Ctrl Pts',(-20.7584558538732,-18.33290329118,17.5467129504672));
#167705=CARTESIAN_POINT('Ctrl Pts',(-20.7595169279054,-18.3363837119768,
17.5464931136084));
#167706=CARTESIAN_POINT('Ctrl Pts',(-20.7620296890385,-18.3447026276586,
17.5459693240063));
#167707=CARTESIAN_POINT('Ctrl Pts',(-20.7634730525617,-18.3495436545245,
17.5456658569024));
#167708=CARTESIAN_POINT('Ctrl Pts',(-20.7683087921699,-18.365977276532,
17.544640090409));
#167709=CARTESIAN_POINT('Ctrl Pts',(-20.7716193511503,-18.3775939681374,
17.5439224008817));
#167710=CARTESIAN_POINT('Ctrl Pts',(-20.7793503161945,-18.405629988541,
17.5422066981606));
#167711=CARTESIAN_POINT('Ctrl Pts',(-20.7836727516699,-18.422075709297,
17.5412137329758));
#167712=CARTESIAN_POINT('Ctrl Pts',(-20.7992282069319,-18.4843001268574,
17.537501174438));
#167713=CARTESIAN_POINT('Ctrl Pts',(-20.8091300683324,-18.5304000817769,
17.5348408066407));
#167714=CARTESIAN_POINT('Ctrl Pts',(-20.839677969429,-18.700030258527,17.5252552166219));
#167715=CARTESIAN_POINT('Ctrl Pts',(-20.8508934167311,-18.824991233221,
17.5185706624773));
#167716=CARTESIAN_POINT('Ctrl Pts',(-20.850999243967,-18.9502108540428,
17.5117114353352));
#167717=CARTESIAN_POINT('Ctrl Pts',(-20.8509992455974,-18.9502127843178,
17.5117113295994));
#167718=CARTESIAN_POINT('Ctrl Pts',(-20.8510695262169,-19.0334618402732,
17.5071511472245));
#167719=CARTESIAN_POINT('Ctrl Pts',(-20.8462293176907,-19.1166379126245,
17.5025270519463));
#167720=CARTESIAN_POINT('Ctrl Pts',(-20.8325132046076,-19.2332451195831,
17.4958024131623));
#167721=CARTESIAN_POINT('Ctrl Pts',(-20.8277008026706,-19.2670765721156,
17.4938228650143));
#167722=CARTESIAN_POINT('Ctrl Pts',(-20.8203841631101,-19.310880315912,
17.4912165050731));
#167723=CARTESIAN_POINT('Ctrl Pts',(-20.8186230170447,-19.3209726663742,
17.4906130039197));
#167724=CARTESIAN_POINT('Ctrl Pts',(-20.8155218560417,-19.3380127245543,
17.4895887993749));
#167725=CARTESIAN_POINT('Ctrl Pts',(-20.8142201261234,-19.3449672832719,
17.4891693092348));
#167726=CARTESIAN_POINT('Ctrl Pts',(-20.8115753898661,-19.3587154474302,
17.4883370439448));
#167727=CARTESIAN_POINT('Ctrl Pts',(-20.8102338631363,-19.3655092496791,
17.4879243205081));
#167728=CARTESIAN_POINT('Ctrl Pts',(-20.8075792012131,-19.3786144078015,
17.4871253293806));
#167729=CARTESIAN_POINT('Ctrl Pts',(-20.8062705223735,-19.3849265957684,
17.4867392082836));
#167730=CARTESIAN_POINT('Ctrl Pts',(-20.8031922253141,-19.3994404235502,
17.4858483918317));
#167731=CARTESIAN_POINT('Ctrl Pts',(-20.8014026463276,-19.4076376770188,
17.4853430613936));
#167732=CARTESIAN_POINT('Ctrl Pts',(-20.7964820731091,-19.4295506466621,
17.483986196528));
#167733=CARTESIAN_POINT('Ctrl Pts',(-20.7932630478049,-19.4432459740009,
17.4831318485563));
#167734=CARTESIAN_POINT('Ctrl Pts',(-20.7649958663005,-19.5583456074873,
17.4758971160508));
#167735=CARTESIAN_POINT('Ctrl Pts',(-20.7326147078825,-19.6577852284586,
17.4692780254053));
#167736=CARTESIAN_POINT('Ctrl Pts',(-20.6610715696034,-19.8324515836869,
17.4570100463674));
#167737=CARTESIAN_POINT('Ctrl Pts',(-20.6244765246981,-19.9085025570576,
17.451433154835));
#167738=CARTESIAN_POINT('Ctrl Pts',(-20.5381977865182,-20.063398031067,
17.4397198098766));
#167739=CARTESIAN_POINT('Ctrl Pts',(-20.4876434191509,-20.1415682249568,
17.4335968453404));
#167740=CARTESIAN_POINT('Ctrl Pts',(-20.4137245280448,-20.2408608798846,
17.4257440962747));
#167741=CARTESIAN_POINT('Ctrl Pts',(-20.3948022331264,-20.2651538488293,
17.4238168235806));
#167742=CARTESIAN_POINT('Ctrl Pts',(-20.3708599262467,-20.2945458102632,
17.4214862789034));
#167743=CARTESIAN_POINT('Ctrl Pts',(-20.3663363358639,-20.3000421954618,
17.421050517244));
#167744=CARTESIAN_POINT('Ctrl Pts',(-20.3591745750054,-20.3086551777334,
17.4203679008892));
#167745=CARTESIAN_POINT('Ctrl Pts',(-20.356555013109,-20.3117870791417,
17.4201197331622));
#167746=CARTESIAN_POINT('Ctrl Pts',(-20.351624142597,-20.317647802847,17.4196554619898));
#167747=CARTESIAN_POINT('Ctrl Pts',(-20.3493150076173,-20.3203783155646,
17.4194392130833));
#167748=CARTESIAN_POINT('Ctrl Pts',(-20.3440048979135,-20.3266252576383,
17.4189445809203));
#167749=CARTESIAN_POINT('Ctrl Pts',(-20.3409993215095,-20.3301377114932,
17.4186665407722));
#167750=CARTESIAN_POINT('Ctrl Pts',(-20.3330828580916,-20.3393281399851,
17.4179391539201));
#167751=CARTESIAN_POINT('Ctrl Pts',(-20.3281531834687,-20.3449899448515,
17.4174911574037));
#167752=CARTESIAN_POINT('Ctrl Pts',(-20.2945560036734,-20.3831648649959,
17.4144703435428));
#167753=CARTESIAN_POINT('Ctrl Pts',(-20.2649237166947,-20.4148195594296,
17.4119645343398));
#167754=CARTESIAN_POINT('Ctrl Pts',(-20.1835998145477,-20.4965133857353,
17.4054236572952));
#167755=CARTESIAN_POINT('Ctrl Pts',(-20.1302937814578,-20.5448672994004,
17.4014724000781));
#167756=CARTESIAN_POINT('Ctrl Pts',(-20.0058451160796,-20.6466968397585,
17.392707799697));
#167757=CARTESIAN_POINT('Ctrl Pts',(-19.933588696755,-20.6985892974522,
17.3879174280155));
#167758=CARTESIAN_POINT('Ctrl Pts',(-19.7972997306427,-20.7840106376653,
17.3790773092358));
#167759=CARTESIAN_POINT('Ctrl Pts',(-19.7344089441507,-20.8190966793269,
17.3750666298382));
#167760=CARTESIAN_POINT('Ctrl Pts',(-19.6453082205645,-20.8630089863234,
17.3693856194332));
#167761=CARTESIAN_POINT('Ctrl Pts',(-19.6205279724454,-20.8746299896293,
17.3678060415376));
#167762=CARTESIAN_POINT('Ctrl Pts',(-19.5772513509196,-20.8939105519997,
17.3650437045443));
#167763=CARTESIAN_POINT('Ctrl Pts',(-19.5588584719605,-20.9017943208189,
17.3638685595109));
#167764=CARTESIAN_POINT('Ctrl Pts',(-19.5322720645011,-20.9127465850986,
17.3621671675772));
#167765=CARTESIAN_POINT('Ctrl Pts',(-19.5241666156303,-20.9160270303605,
17.3616480997127));
#167766=CARTESIAN_POINT('Ctrl Pts',(-19.5099910500453,-20.9216622245086,
17.3607395802514));
#167767=CARTESIAN_POINT('Ctrl Pts',(-19.5039299225899,-20.9240393761907,
17.360350889664));
#167768=CARTESIAN_POINT('Ctrl Pts',(-19.4922774704833,-20.9285475155234,
17.3596031568151));
#167769=CARTESIAN_POINT('Ctrl Pts',(-19.4866878799951,-20.9306828339909,
17.3592442645864));
#167770=CARTESIAN_POINT('Ctrl Pts',(-19.4720715059446,-20.9361956410871,
17.3583052008593));
#167771=CARTESIAN_POINT('Ctrl Pts',(-19.4630306532431,-20.9395352051783,
17.3577237672871));
#167772=CARTESIAN_POINT('Ctrl Pts',(-19.4318254212238,-20.9508204198185,
17.3557147217561));
#167773=CARTESIAN_POINT('Ctrl Pts',(-19.4095521047387,-20.958457742573,
17.3542769330927));
#167774=CARTESIAN_POINT('Ctrl Pts',(-19.227864233617,-21.0173887515002,
17.3425137850433));
#167775=CARTESIAN_POINT('Ctrl Pts',(-19.0630323608603,-21.0499632506091,
17.331555211189));
#167776=CARTESIAN_POINT('Ctrl Pts',(-18.7712099510454,-21.0723772608182,
17.312213430873));
#167777=CARTESIAN_POINT('Ctrl Pts',(-18.6456783000796,-21.0708653071399,
17.3039353141196));
#167778=CARTESIAN_POINT('Ctrl Pts',(-18.5090983611205,-21.057053803406,
17.2954216778607));
#167779=CARTESIAN_POINT('Ctrl Pts',(-18.4971999757858,-21.0557485653287,
17.2946842650551));
#167780=CARTESIAN_POINT('Ctrl Pts',(-18.4803148521982,-21.053751216658,
17.2936444721052));
#167781=CARTESIAN_POINT('Ctrl Pts',(-18.4753187790598,-21.0531421556078,
17.2933376438129));
#167782=CARTESIAN_POINT('Ctrl Pts',(-18.4667179063014,-21.0520624984887,
17.2928109200508));
#167783=CARTESIAN_POINT('Ctrl Pts',(-18.4631120750835,-21.0516004258151,
17.292590548237));
#167784=CARTESIAN_POINT('Ctrl Pts',(-18.4561272117378,-21.050687050161,
17.2921645614603));
#167785=CARTESIAN_POINT('Ctrl Pts',(-18.4527480794268,-21.0502368737881,
17.2919588817362));
#167786=CARTESIAN_POINT('Ctrl Pts',(-18.4436430440941,-21.0490014878938,
17.2914057333722));
#167787=CARTESIAN_POINT('Ctrl Pts',(-18.4379191961337,-21.0482009830732,
17.2910591223061));
#167788=CARTESIAN_POINT('Ctrl Pts',(-18.416739362049,-21.0451504088812,
17.2897804897764));
#167789=CARTESIAN_POINT('Ctrl Pts',(-18.4013047068568,-21.0427526923624,
17.2888564416926));
#167790=CARTESIAN_POINT('Ctrl Pts',(-18.2517875119768,-21.0178280199976,
17.2799681064258));
#167791=CARTESIAN_POINT('Ctrl Pts',(-18.120123620421,-20.9826009742182,
17.2726210040869));
#167792=CARTESIAN_POINT('Ctrl Pts',(-17.8473499671938,-20.8806345077521,
17.2568069650021));
#167793=CARTESIAN_POINT('Ctrl Pts',(-17.708401958035,-20.8104726312299,
17.2483533301633));
#167794=CARTESIAN_POINT('Ctrl Pts',(-17.5605536548037,-20.7141478848008,
17.2380769063227));
#167795=CARTESIAN_POINT('Ctrl Pts',(-17.5429072246168,-20.7022683922302,
17.2368286278881));
#167796=CARTESIAN_POINT('Ctrl Pts',(-17.5180625448446,-20.684993340224,
17.2350385655076));
#167797=CARTESIAN_POINT('Ctrl Pts',(-17.510714681298,-20.6798144684435,
17.234505019022));
#167798=CARTESIAN_POINT('Ctrl Pts',(-17.4980925964965,-20.6707973807744,
17.2335812327407));
#167799=CARTESIAN_POINT('Ctrl Pts',(-17.4928026809292,-20.6669812709924,
17.2331918471486));
#167800=CARTESIAN_POINT('Ctrl Pts',(-17.4827058285511,-20.6596262840938,
17.2324443095098));
#167801=CARTESIAN_POINT('Ctrl Pts',(-17.4778960507041,-20.656091399268,
17.2320863148529));
#167802=CARTESIAN_POINT('Ctrl Pts',(-17.4654233759976,-20.6468432700202,
17.2311529854179));
#167803=CARTESIAN_POINT('Ctrl Pts',(-17.457784171652,-20.6410984327993,
17.2305764185805));
#167804=CARTESIAN_POINT('Ctrl Pts',(-17.4318444734706,-20.6213148223869,
17.2286015560826));
#167805=CARTESIAN_POINT('Ctrl Pts',(-17.4137351301006,-20.6070291836654,
17.2271935429105));
#167806=CARTESIAN_POINT('Ctrl Pts',(-17.2606449930511,-20.4821516166951,
17.215032336043));
#167807=CARTESIAN_POINT('Ctrl Pts',(-17.1396071314855,-20.3555765989584,
17.2035843977549));
#167808=CARTESIAN_POINT('Ctrl Pts',(-16.9831369067,-20.1452560628161,17.1862637157592));
#167809=CARTESIAN_POINT('Ctrl Pts',(-16.9352051229845,-20.0716966232254,
17.1804815539708));
#167810=CARTESIAN_POINT('Ctrl Pts',(-16.8732450303252,-19.9623087769314,
17.1724538775296));
#167811=CARTESIAN_POINT('Ctrl Pts',(-16.8554095330915,-19.928745184233,
17.170063395062));
#167812=CARTESIAN_POINT('Ctrl Pts',(-16.8351098744618,-19.8879288294555,
17.1672581905981));
#167813=CARTESIAN_POINT('Ctrl Pts',(-16.8317701006238,-19.8811221106966,
17.1667937182804));
#167814=CARTESIAN_POINT('Ctrl Pts',(-16.8266439153093,-19.8705310422349,
17.1660763468545));
#167815=CARTESIAN_POINT('Ctrl Pts',(-16.8248320740249,-19.8667591707565,
17.1658219086481));
#167816=CARTESIAN_POINT('Ctrl Pts',(-16.8214979542809,-19.8597651810801,
17.1653520823024));
#167817=CARTESIAN_POINT('Ctrl Pts',(-16.8199726409069,-19.8565446190239,
17.1651365112287));
#167818=CARTESIAN_POINT('Ctrl Pts',(-16.8165492740957,-19.8492690557924,
17.1646512443249));
#167819=CARTESIAN_POINT('Ctrl Pts',(-16.814655953314,-19.8452118875449,
17.1643818425557));
#167820=CARTESIAN_POINT('Ctrl Pts',(-16.8091248003533,-19.833260470886,
17.1635916999788));
#167821=CARTESIAN_POINT('Ctrl Pts',(-16.8055226483594,-19.8253496790139,
17.1630731070649));
#167822=CARTESIAN_POINT('Ctrl Pts',(-16.7804085174573,-19.7692827357452,
17.1594271870966));
#167823=CARTESIAN_POINT('Ctrl Pts',(-16.7606521474861,-19.7203553816621,
17.156398941036));
#167824=CARTESIAN_POINT('Ctrl Pts',(-16.7373630223412,-19.6558329690251,
17.1525392329145));
#167825=CARTESIAN_POINT('Ctrl Pts',(-16.7321508787293,-19.6408687700225,
17.1516532436768));
#167826=CARTESIAN_POINT('Ctrl Pts',(-16.7109435884538,-19.5777079244072,
17.147946742212));
#167827=CARTESIAN_POINT('Ctrl Pts',(-16.6965167799816,-19.5290009753863,
17.145168636274));
#167828=CARTESIAN_POINT('Ctrl Pts',(-16.6565769513346,-19.373867983843,
17.1364468229742));
#167829=CARTESIAN_POINT('Ctrl Pts',(-16.6375537615508,-19.265960843546,
17.1305558812288));
#167830=CARTESIAN_POINT('Ctrl Pts',(-16.6216106654859,-19.1021504885194,
17.1214049149708));
#167831=CARTESIAN_POINT('Ctrl Pts',(-16.6184150535142,-19.0470450235747,
17.1182935978638));
#167832=CARTESIAN_POINT('Ctrl Pts',(-16.6167287782852,-18.9575470175329,
17.1131438566884));
#167833=CARTESIAN_POINT('Ctrl Pts',(-16.6169173792691,-18.9232045909833,
17.1111449354558));
#167834=CARTESIAN_POINT('Ctrl Pts',(-16.6182634646052,-18.8780755499623,
17.1084822194833));
#167835=CARTESIAN_POINT('Ctrl Pts',(-16.6186686240855,-18.8672705775777,
17.107841999799));
#167836=CARTESIAN_POINT('Ctrl Pts',(-16.6194678522679,-18.8495773849862,
17.1067890314628));
#167837=CARTESIAN_POINT('Ctrl Pts',(-16.6198128568608,-18.8426870642994,
17.1063778255992));
#167838=CARTESIAN_POINT('Ctrl Pts',(-16.6205459278243,-18.829351839316,
17.1055797304374));
#167839=CARTESIAN_POINT('Ctrl Pts',(-16.6209298108531,-18.8229067746896,
17.1051929768543));
#167840=CARTESIAN_POINT('Ctrl Pts',(-16.6218843373953,-18.8080282081486,
17.1042977371976));
#167841=CARTESIAN_POINT('Ctrl Pts',(-16.6224760171326,-18.7995962086847,
17.1037885956355));
#167842=CARTESIAN_POINT('Ctrl Pts',(-16.6242032878061,-18.7769261807373,
17.1024148165201));
#167843=CARTESIAN_POINT('Ctrl Pts',(-16.6254324868048,-18.762695917692,
17.1015472544075));
#167844=CARTESIAN_POINT('Ctrl Pts',(-16.6403656975414,-18.6080816605446,
17.0920626676959));
#167845=CARTESIAN_POINT('Ctrl Pts',(-16.6679204806769,-18.4694168577996,
17.0829959915786));
#167846=CARTESIAN_POINT('Ctrl Pts',(-16.7372284608753,-18.242120645508,
17.0673628311088));
#167847=CARTESIAN_POINT('Ctrl Pts',(-16.7717048783854,-18.1517354615935,
17.0609354431817));
#167848=CARTESIAN_POINT('Ctrl Pts',(-16.8327736612588,-18.0195703079126,
17.0514347346944));
#167849=CARTESIAN_POINT('Ctrl Pts',(-16.8548502235409,-17.9758424958889,
17.0482747682353));
#167850=CARTESIAN_POINT('Ctrl Pts',(-16.8910617351461,-17.9099075468264,
17.0435245514821));
#167851=CARTESIAN_POINT('Ctrl Pts',(-16.904126168122,-17.8871337947401,
17.0418866803956));
#167852=CARTESIAN_POINT('Ctrl Pts',(-16.9210832996784,-17.8588084691842,
17.0398587510873));
#167853=CARTESIAN_POINT('Ctrl Pts',(-16.9245829012481,-17.8530257278042,
17.039445232032));
#167854=CARTESIAN_POINT('Ctrl Pts',(-16.9301992783735,-17.8438447838953,
17.0387896199361));
#167855=CARTESIAN_POINT('Ctrl Pts',(-16.9322980664955,-17.8404357104777,
17.0385463786577));
#167856=CARTESIAN_POINT('Ctrl Pts',(-16.9362988798129,-17.8339782684281,
17.0380860458462));
#167857=CARTESIAN_POINT('Ctrl Pts',(-16.9381989711154,-17.830928827148,
17.0378688393651));
#167858=CARTESIAN_POINT('Ctrl Pts',(-16.9425929354552,-17.8239168250786,
17.0373697765376));
#167859=CARTESIAN_POINT('Ctrl Pts',(-16.9450921957221,-17.8199576910739,
17.0370882800091));
#167860=CARTESIAN_POINT('Ctrl Pts',(-16.951830798566,-17.8093609643162,
17.0363355230918));
#167861=CARTESIAN_POINT('Ctrl Pts',(-16.9560941277454,-17.8027386101618,
17.0358658072725));
#167862=CARTESIAN_POINT('Ctrl Pts',(-16.9884370261509,-17.7531101513779,
17.0323498909384));
#167863=CARTESIAN_POINT('Ctrl Pts',(-17.0180388274937,-17.7111111495177,
17.0293980441262));
#167864=CARTESIAN_POINT('Ctrl Pts',(-17.0626704741397,-17.6524439651622,
17.0252455293426));
#167865=CARTESIAN_POINT('Ctrl Pts',(-17.076480291065,-17.6348755810427,
17.0239980918122));
#167866=CARTESIAN_POINT('Ctrl Pts',(-17.1195097664553,-17.5818837300231,
17.0202124901868));
#167867=CARTESIAN_POINT('Ctrl Pts',(-17.149606423822,-17.5471887870443,
17.0177016909427));
#167868=CARTESIAN_POINT('Ctrl Pts',(-17.2551132129274,-17.4332700014714,
17.0092480620041));
#167869=CARTESIAN_POINT('Ctrl Pts',(-17.335522033852,-17.3589195148344,
17.0033598456689));
#167870=CARTESIAN_POINT('Ctrl Pts',(-17.4645496538013,-17.2569418063313,
16.9942152161125));
#167871=CARTESIAN_POINT('Ctrl Pts',(-17.5091038410045,-17.2244713560694,
16.9911075315518));
#167872=CARTESIAN_POINT('Ctrl Pts',(-17.5833664007015,-17.1746681709009,
16.9859632669315));
#167873=CARTESIAN_POINT('Ctrl Pts',(-17.6123199771704,-17.1562550737006,
16.9839660796235));
#167874=CARTESIAN_POINT('Ctrl Pts',(-17.6509662038036,-17.1329772864511,
16.9813053462602));
#167875=CARTESIAN_POINT('Ctrl Pts',(-17.6602678219077,-17.1274712829664,
16.9806653304793));
#167876=CARTESIAN_POINT('Ctrl Pts',(-17.675573974019,-17.1185685360993,
16.9796126121064));
#167877=CARTESIAN_POINT('Ctrl Pts',(-17.6815537401217,-17.1151294401533,
16.9792014508654));
#167878=CARTESIAN_POINT('Ctrl Pts',(-17.6931629814044,-17.1085280063909,
16.97840338128));
#167879=CARTESIAN_POINT('Ctrl Pts',(-17.6987903321349,-17.1053620732191,
16.9780166083275));
#167880=CARTESIAN_POINT('Ctrl Pts',(-17.7118194671034,-17.0981101869123,
16.977121234935));
#167881=CARTESIAN_POINT('Ctrl Pts',(-17.7192313839569,-17.0940427524946,
16.9766119783896));
#167882=CARTESIAN_POINT('Ctrl Pts',(-17.739235676222,-17.0832204156952,
16.9752376878263));
#167883=CARTESIAN_POINT('Ctrl Pts',(-17.7518722409626,-17.0765485226784,
16.9743697258596));
#167884=CARTESIAN_POINT('Ctrl Pts',(-17.8684340106715,-17.016506977069,
16.9663637394059));
#167885=CARTESIAN_POINT('Ctrl Pts',(-17.976525859467,-16.97170637349,16.9589240495139));
#167886=CARTESIAN_POINT('Ctrl Pts',(-18.2426368976508,-16.8863988150121,
16.9406706497531));
#167887=CARTESIAN_POINT('Ctrl Pts',(-18.4027307136964,-16.8547621316976,
16.9297170534721));
#167888=CARTESIAN_POINT('Ctrl Pts',(-18.5973513535805,-16.8391634787584,
16.917309831331));
#167889=CARTESIAN_POINT('Ctrl Pts',(-18.6298937159241,-16.8373101480052,
16.915267206154));
#167890=CARTESIAN_POINT('Ctrl Pts',(-18.6697088681062,-16.8359640498544,
16.9128174343481));
#167891=CARTESIAN_POINT('Ctrl Pts',(-18.6769511939428,-16.8357564107192,
16.9123738193341));
#167892=CARTESIAN_POINT('Ctrl Pts',(-18.6883043083638,-16.8354892385981,
16.9116816835412));
#167893=CARTESIAN_POINT('Ctrl Pts',(-18.6924143676602,-16.8354044941909,
16.9114317893946));
#167894=CARTESIAN_POINT('Ctrl Pts',(-18.7000958400244,-16.8352684948106,
16.9109660421379));
#167895=CARTESIAN_POINT('Ctrl Pts',(-18.7036670967368,-16.8352143064694,
16.9107500331173));
#167896=CARTESIAN_POINT('Ctrl Pts',(-18.7118177015949,-16.835111264717,
16.9102582224434));
#167897=CARTESIAN_POINT('Ctrl Pts',(-18.7163970728415,-16.8350682321364,
16.9099827493544));
#167898=CARTESIAN_POINT('Ctrl Pts',(-18.7304665956651,-16.8349816773258,
16.9091389011255));
#167899=CARTESIAN_POINT('Ctrl Pts',(-18.7399570796502,-16.8349871081469,
16.9085731941461));
#167900=CARTESIAN_POINT('Ctrl Pts',(-18.8248564970574,-16.8356066218915,
16.9035413315385));
#167901=CARTESIAN_POINT('Ctrl Pts',(-18.9001911933304,-16.8401858786632,
16.8992789492573));
#167902=CARTESIAN_POINT('Ctrl Pts',(-19.0179552061379,-16.8536871815412,
16.892716497893));
#167903=CARTESIAN_POINT('Ctrl Pts',(-19.0606231991676,-16.859904227562,
16.8903599415697));
#167904=CARTESIAN_POINT('Ctrl Pts',(-19.2107231899026,-16.8864792634062,
16.88206090032));
#167905=CARTESIAN_POINT('Ctrl Pts',(-19.3167346056707,-16.9138487774787,
16.8761740322291));
#167906=CARTESIAN_POINT('Ctrl Pts',(-19.472260511082,-16.9671337025608,
16.8670325370955));
#167907=CARTESIAN_POINT('Ctrl Pts',(-19.5236473528516,-16.9870116502655,
16.8639266491064));
#167908=CARTESIAN_POINT('Ctrl Pts',(-19.6056756524519,-17.0224802057107,
16.8587850933084));
#167909=CARTESIAN_POINT('Ctrl Pts',(-19.6368163005452,-17.0368531098807,
16.8567887638693));
#167910=CARTESIAN_POINT('Ctrl Pts',(-19.6772925704882,-17.0567414621613,
16.8541290114569));
#167911=CARTESIAN_POINT('Ctrl Pts',(-19.6869554753732,-17.0615816192734,
16.8534890966186));
#167912=CARTESIAN_POINT('Ctrl Pts',(-19.7027243104024,-17.0696318663711,
16.8524365019883));
#167913=CARTESIAN_POINT('Ctrl Pts',(-19.7088524357667,-17.072798226157,
16.852025362836));
#167914=CARTESIAN_POINT('Ctrl Pts',(-19.7206868460627,-17.0789864495197,
16.8512273058944));
#167915=CARTESIAN_POINT('Ctrl Pts',(-19.7263950018332,-17.0820045851982,
16.8508405233371));
#167916=CARTESIAN_POINT('Ctrl Pts',(-19.7395460561159,-17.0890352591336,
16.8499450836638));
#167917=CARTESIAN_POINT('Ctrl Pts',(-19.7469788632167,-17.0930663497269,
16.8494357701368));
#167918=CARTESIAN_POINT('Ctrl Pts',(-19.7669102787446,-17.1040309410979,
16.848061226093));
#167919=CARTESIAN_POINT('Ctrl Pts',(-19.7793629816096,-17.1110465764857,
16.8471930659468));
#167920=CARTESIAN_POINT('Ctrl Pts',(-19.8931562728313,-17.1766825769026,
16.8391718406982));
#167921=CARTESIAN_POINT('Ctrl Pts',(-19.9895254231834,-17.2434792130333,
16.8317157764982));
#167922=CARTESIAN_POINT('Ctrl Pts',(-20.2060245923141,-17.4217896389405,
16.8133937656602));
#167923=CARTESIAN_POINT('Ctrl Pts',(-20.3197212627132,-17.5399488641614,
16.8023859059752));
#167924=CARTESIAN_POINT('Ctrl Pts',(-20.4378742552593,-17.6952164848327,
16.7899979178305));
#167925=CARTESIAN_POINT('Ctrl Pts',(-20.4564885302219,-17.7208518388757,
16.7880138528937));
#167926=CARTESIAN_POINT('Ctrl Pts',(-20.4786098198552,-17.7528014530596,
16.7856245165779));
#167927=CARTESIAN_POINT('Ctrl Pts',(-20.4826680678981,-17.7587269506774,
16.7851848234535));
#167928=CARTESIAN_POINT('Ctrl Pts',(-20.4889939386435,-17.7680650100906,
16.784497440466));
#167929=CARTESIAN_POINT('Ctrl Pts',(-20.4912818993623,-17.7714636338349,
16.7842484075076));
#167930=CARTESIAN_POINT('Ctrl Pts',(-20.4955471583454,-17.7778392866195,
16.78378340213));
#167931=CARTESIAN_POINT('Ctrl Pts',(-20.4975267620635,-17.7808146467676,
16.7835672789989));
#167932=CARTESIAN_POINT('Ctrl Pts',(-20.5020376687181,-17.7876319443204,
16.7830740862629));
#167933=CARTESIAN_POINT('Ctrl Pts',(-20.504563983472,-17.791477122827,16.7827973523673));
#167934=CARTESIAN_POINT('Ctrl Pts',(-20.5111393634606,-17.8015566317732,
16.78207562117));
#167935=CARTESIAN_POINT('Ctrl Pts',(-20.5151682022345,-17.8078041689976,
16.7816319402299));
#167936=CARTESIAN_POINT('Ctrl Pts',(-20.5417014523473,-17.8494291606566,
16.7786992181592));
#167937=CARTESIAN_POINT('Ctrl Pts',(-20.5631851567631,-17.8854498668355,
16.7762728279761));
#167938=CARTESIAN_POINT('Ctrl Pts',(-20.5941595696157,-17.9410758066855,
16.7726551234392));
#167939=CARTESIAN_POINT('Ctrl Pts',(-20.6044401401784,-17.9602262946154,
16.771432146629));
#167940=CARTESIAN_POINT('Ctrl Pts',(-20.6222691366742,-17.9947015518818,
16.7692644778012));
#167941=CARTESIAN_POINT('Ctrl Pts',(-20.6299303041583,-18.009965524945,
16.7683163897668));
#167942=CARTESIAN_POINT('Ctrl Pts',(-20.6692391383491,-18.0907061637996,
16.7633540808339));
#167943=CARTESIAN_POINT('Ctrl Pts',(-20.6976645159724,-18.1576525955934,
16.7594187150736));
#167944=CARTESIAN_POINT('Ctrl Pts',(-20.7225806455427,-18.225889804387,
16.7554729693871));
#167945=CARTESIAN_POINT('',(-20.8509999221897,-18.9514260237555,17.2909082342155));
#167946=CARTESIAN_POINT('Ctrl Pts',(-20.7225805737622,-18.2258896078036,
16.5356516434534));
#167947=CARTESIAN_POINT('Ctrl Pts',(-20.7222420301486,-18.2249624467816,
16.5357110395108));
#167948=CARTESIAN_POINT('Ctrl Pts',(-20.7219028372283,-18.2240355201043,
16.5357703973916));
#167949=CARTESIAN_POINT('Ctrl Pts',(-20.7191070459373,-18.2164118699226,
16.5362584073765));
#167950=CARTESIAN_POINT('Ctrl Pts',(-20.7166172251023,-18.2097272583708,
16.5366851133493));
#167951=CARTESIAN_POINT('Ctrl Pts',(-20.703129761205,-18.1740684980674,
16.5389556106031));
#167952=CARTESIAN_POINT('Ctrl Pts',(-20.6915300510584,-18.1453242498908,
16.5407655164785));
#167953=CARTESIAN_POINT('Ctrl Pts',(-20.6147736079762,-17.9665379995588,
16.5519561005528));
#167954=CARTESIAN_POINT('Ctrl Pts',(-20.5330352496231,-17.8242015957943,
16.560601236315));
#167955=CARTESIAN_POINT('Ctrl Pts',(-20.3657124080848,-17.5980980420755,
16.5759957468391));
#167956=CARTESIAN_POINT('Ctrl Pts',(-20.2879589757414,-17.5095222517557,
16.5825621627779));
#167957=CARTESIAN_POINT('Ctrl Pts',(-20.1929613260748,-17.4179448005569,
16.590292168564));
#167958=CARTESIAN_POINT('Ctrl Pts',(-20.1825655592422,-17.4081245802994,
16.5911342954128));
#167959=CARTESIAN_POINT('Ctrl Pts',(-20.1658644146375,-17.3926652596687,
16.5924816805941));
#167960=CARTESIAN_POINT('Ctrl Pts',(-20.1596232408126,-17.386957218988,
16.5929839921552));
#167961=CARTESIAN_POINT('Ctrl Pts',(-20.1485570617236,-17.3769574557105,
16.5938726153736));
#167962=CARTESIAN_POINT('Ctrl Pts',(-20.1437462839575,-17.3726500987316,
16.5942582599892));
#167963=CARTESIAN_POINT('Ctrl Pts',(-20.133756625154,-17.3637878107906,
16.5950577293174));
#167964=CARTESIAN_POINT('Ctrl Pts',(-20.1285750467172,-17.3592360485814,
16.5954716798637));
#167965=CARTESIAN_POINT('Ctrl Pts',(-20.1152202516283,-17.3476196440815,
16.5965367711511));
#167966=CARTESIAN_POINT('Ctrl Pts',(-20.1070151064927,-17.3405921619488,
16.5971894390735));
#167967=CARTESIAN_POINT('Ctrl Pts',(-20.0725673342631,-17.3115427079128,
16.5999227096948));
#167968=CARTESIAN_POINT('Ctrl Pts',(-20.0458470835339,-17.2900975812277,
16.6020265842632));
#167969=CARTESIAN_POINT('Ctrl Pts',(-19.9749016345451,-17.2359355160258,
16.6075743669528));
#167970=CARTESIAN_POINT('Ctrl Pts',(-19.9299029955634,-17.204278801301,
16.6110565452528));
#167971=CARTESIAN_POINT('Ctrl Pts',(-19.8068133545947,-17.1246656791153,
16.6204783095656));
#167972=CARTESIAN_POINT('Ctrl Pts',(-19.7267585893265,-17.0799670518381,
16.6265050649784));
#167973=CARTESIAN_POINT('Ctrl Pts',(-19.5956094518915,-17.0175236832881,
16.6361027564918));
#167974=CARTESIAN_POINT('Ctrl Pts',(-19.546291174055,-16.9963025073906,
16.6396526882863));
#167975=CARTESIAN_POINT('Ctrl Pts',(-19.4618465339254,-16.9637128297234,
16.645587671196));
#167976=CARTESIAN_POINT('Ctrl Pts',(-19.4271320951876,-16.951346467928,
16.6479878622863));
#167977=CARTESIAN_POINT('Ctrl Pts',(-19.3471239569802,-16.9251777609809,
16.6534058788003));
#167978=CARTESIAN_POINT('Ctrl Pts',(-19.3016518031468,-16.9119751084276,
16.6564037279012));
#167979=CARTESIAN_POINT('Ctrl Pts',(-19.2483051863362,-16.8984083830984,
16.6597975247556));
#167980=CARTESIAN_POINT('Ctrl Pts',(-19.240828275168,-16.8965503028953,
16.6602704030422));
#167981=CARTESIAN_POINT('Ctrl Pts',(-19.228840242613,-16.8936405593376,
16.6610239471918));
#167982=CARTESIAN_POINT('Ctrl Pts',(-19.2243356045278,-16.8925628320957,
16.6613060537998));
#167983=CARTESIAN_POINT('Ctrl Pts',(-19.2163369550479,-16.8906769000415,
16.6618050762793));
#167984=CARTESIAN_POINT('Ctrl Pts',(-19.2128443851018,-16.8898627794906,
16.6620223290233));
#167985=CARTESIAN_POINT('Ctrl Pts',(-19.2054214227456,-16.8881523571832,
16.6624826911082));
#167986=CARTESIAN_POINT('Ctrl Pts',(-19.2014905428926,-16.887258407569,
16.6627256648546));
#167987=CARTESIAN_POINT('Ctrl Pts',(-19.1908395447488,-16.8848681637446,
16.6633818753885));
#167988=CARTESIAN_POINT('Ctrl Pts',(-19.18411457444,-16.8833933986964,16.6637938945099));
#167989=CARTESIAN_POINT('Ctrl Pts',(-19.1502487982697,-16.8761397089737,
16.6658576989648));
#167990=CARTESIAN_POINT('Ctrl Pts',(-19.1230020420402,-16.8708617084941,
16.6674824896379));
#167991=CARTESIAN_POINT('Ctrl Pts',(-19.0432741923606,-16.857038180993,
16.6721539673701));
#167992=CARTESIAN_POINT('Ctrl Pts',(-18.9905631766393,-16.8499315761761,
16.6751387029452));
#167993=CARTESIAN_POINT('Ctrl Pts',(-18.7975121391367,-16.8312752159257,
16.685869490249));
#167994=CARTESIAN_POINT('Ctrl Pts',(-18.6563848057086,-16.8317439972712,
16.6933531304301));
#167995=CARTESIAN_POINT('Ctrl Pts',(-18.4249527490239,-16.855664962178,
16.7062229336917));
#167996=CARTESIAN_POINT('Ctrl Pts',(-18.334282573879,-16.8710497892409,
16.711414877912));
#167997=CARTESIAN_POINT('Ctrl Pts',(-18.231513257621,-16.8954530102101,
16.7176071698761));
#167998=CARTESIAN_POINT('Ctrl Pts',(-18.218153209067,-16.8987634032048,
16.7184181235569));
#167999=CARTESIAN_POINT('Ctrl Pts',(-18.1967888854907,-16.9042787959941,
16.71972489411));
#168000=CARTESIAN_POINT('Ctrl Pts',(-18.188763512746,-16.9064010459382,
16.7202180387283));
#168001=CARTESIAN_POINT('Ctrl Pts',(-18.1745418052073,-16.910251507313,
16.721096045105));
#168002=CARTESIAN_POINT('Ctrl Pts',(-18.1683404427557,-16.9119608721893,
16.7214802909954));
#168003=CARTESIAN_POINT('Ctrl Pts',(-18.155441417578,-16.9155797410592,
16.722282477645));
#168004=CARTESIAN_POINT('Ctrl Pts',(-18.1487452032223,-16.9174940832321,
16.7227005720818));
#168005=CARTESIAN_POINT('Ctrl Pts',(-18.131391715772,-16.9225479337874,
16.7237884479509));
#168006=CARTESIAN_POINT('Ctrl Pts',(-18.1207495961006,-16.9257383268636,
16.7244598845654));
#168007=CARTESIAN_POINT('Ctrl Pts',(-18.0747517122328,-16.9399235593037,
16.7273809648823));
#168008=CARTESIAN_POINT('Ctrl Pts',(-18.0396644231717,-16.9517605784893,
16.7296580666283));
#168009=CARTESIAN_POINT('Ctrl Pts',(-17.9473873520448,-16.9856116068852,
16.735781408014));
#168010=CARTESIAN_POINT('Ctrl Pts',(-17.8908153141529,-17.0091975774585,
16.7396765619259));
#168011=CARTESIAN_POINT('Ctrl Pts',(-17.6944560693447,-17.1012564693211,
16.7536824899201));
#168012=CARTESIAN_POINT('Ctrl Pts',(-17.5612889335845,-17.1826368251964,
16.7641254004742));
#168013=CARTESIAN_POINT('Ctrl Pts',(-17.4256691251995,-17.2876045165932,
16.775274728743));
#168014=CARTESIAN_POINT('Ctrl Pts',(-17.4132004202791,-17.297481794303,
16.7763045754062));
#168015=CARTESIAN_POINT('Ctrl Pts',(-17.3633098138706,-17.337926862869,
16.7804412366845));
#168016=CARTESIAN_POINT('Ctrl Pts',(-17.3268250501749,-17.3696336913954,
16.7835034127499));
#168017=CARTESIAN_POINT('Ctrl Pts',(-17.2857831522735,-17.4078442409456,
16.7869611033205));
#168018=CARTESIAN_POINT('Ctrl Pts',(-17.280140614872,-17.4131556483058,
16.7874367666734));
#168019=CARTESIAN_POINT('Ctrl Pts',(-17.2711626558328,-17.4217001995823,
16.7881938863815));
#168020=CARTESIAN_POINT('Ctrl Pts',(-17.2678085518274,-17.4249134887303,
16.7884768047266));
#168021=CARTESIAN_POINT('Ctrl Pts',(-17.2618823674125,-17.4306283988318,
16.7889767457891));
#168022=CARTESIAN_POINT('Ctrl Pts',(-17.2593060386514,-17.4331255502477,
16.7891941097726));
#168023=CARTESIAN_POINT('Ctrl Pts',(-17.2538539030307,-17.4384370770107,
16.7896541366006));
#168024=CARTESIAN_POINT('Ctrl Pts',(-17.2509797737923,-17.4412530987947,
16.7898966667735));
#168025=CARTESIAN_POINT('Ctrl Pts',(-17.2432338235334,-17.4488858520152,
16.7905504237056));
#168026=CARTESIAN_POINT('Ctrl Pts',(-17.238377277939,-17.4537181136533,
16.7909604483107));
#168027=CARTESIAN_POINT('Ctrl Pts',(-17.2142587984533,-17.4779501217995,
16.7929979049127));
#168028=CARTESIAN_POINT('Ctrl Pts',(-17.1953494862934,-17.4976990957821,
16.7945991609618));
#168029=CARTESIAN_POINT('Ctrl Pts',(-17.1416026067507,-17.55605480778,16.799181551355));
#168030=CARTESIAN_POINT('Ctrl Pts',(-17.1077966336604,-17.5955871643184,
16.8021035150069));
#168031=CARTESIAN_POINT('Ctrl Pts',(-16.9891049431107,-17.7452084395329,
16.8126800653688));
#168032=CARTESIAN_POINT('Ctrl Pts',(-16.9136618791501,-17.8623320950039,
16.8200706137296));
#168033=CARTESIAN_POINT('Ctrl Pts',(-16.8068179112161,-18.070686153413,
16.8330021879265));
#168034=CARTESIAN_POINT('Ctrl Pts',(-16.7691588994095,-18.1581857384207,
16.8383711955845));
#168035=CARTESIAN_POINT('Ctrl Pts',(-16.7329083146597,-18.260976911818,
16.8447602569049));
#168036=CARTESIAN_POINT('Ctrl Pts',(-16.7284301515187,-18.274083773018,
16.8455762488259));
#168037=CARTESIAN_POINT('Ctrl Pts',(-16.7214663083016,-18.2951389236566,
16.8468895906961));
#168038=CARTESIAN_POINT('Ctrl Pts',(-16.7188983072456,-18.3030597110123,
16.8473842248714));
#168039=CARTESIAN_POINT('Ctrl Pts',(-16.7144282204306,-18.3171297329511,
16.8482639473344));
#168040=CARTESIAN_POINT('Ctrl Pts',(-16.7125073147607,-18.3232729122047,
16.8486484114684));
#168041=CARTESIAN_POINT('Ctrl Pts',(-16.7085697250381,-18.3360701788467,
16.8494501118859));
#168042=CARTESIAN_POINT('Ctrl Pts',(-16.706557750201,-18.3427256239972,
16.8498674971716));
#168043=CARTESIAN_POINT('Ctrl Pts',(-16.7014310274273,-18.3599910105879,
16.8509514804946));
#168044=CARTESIAN_POINT('Ctrl Pts',(-16.6983665859002,-18.3706155592522,
16.8516197115848));
#168045=CARTESIAN_POINT('Ctrl Pts',(-16.6855348777617,-18.4164491517749,
16.8545078236665));
#168046=CARTESIAN_POINT('Ctrl Pts',(-16.6765972941571,-18.4518821008629,
16.8567544008797));
#168047=CARTESIAN_POINT('Ctrl Pts',(-16.6553861857809,-18.5462036424157,
16.8627748393013));
#168048=CARTESIAN_POINT('Ctrl Pts',(-16.644698373882,-18.605411281478,16.8665956013806));
#168049=CARTESIAN_POINT('Ctrl Pts',(-16.6139710412325,-18.8299646187728,
16.8812208442814));
#168050=CARTESIAN_POINT('Ctrl Pts',(-16.6109402702495,-18.9970091067736,
16.8924272711971));
#168051=CARTESIAN_POINT('Ctrl Pts',(-16.6329449335284,-19.2170295548752,
16.9067297600396));
#168052=CARTESIAN_POINT('Ctrl Pts',(-16.6404834758119,-19.2711594023646,
16.9102050133028));
#168053=CARTESIAN_POINT('Ctrl Pts',(-16.6516534379398,-19.3335739784397,
16.9141167542428));
#168054=CARTESIAN_POINT('Ctrl Pts',(-16.6532519873198,-19.342196898224,
16.9146550410336));
#168055=CARTESIAN_POINT('Ctrl Pts',(-16.6557506714089,-19.3552231673058,
16.9154647071087));
#168056=CARTESIAN_POINT('Ctrl Pts',(-16.65661129703,-19.3596338701279,16.9157382521202));
#168057=CARTESIAN_POINT('Ctrl Pts',(-16.6581797704984,-19.3675383031256,
16.916227339784));
#168058=CARTESIAN_POINT('Ctrl Pts',(-16.6588824007356,-19.3710330015503,
16.9164431742448));
#168059=CARTESIAN_POINT('Ctrl Pts',(-16.6604264787284,-19.3786137064543,
16.9169104885663));
#168060=CARTESIAN_POINT('Ctrl Pts',(-16.6612711751822,-19.3826989924671,
16.9171617803487));
#168061=CARTESIAN_POINT('Ctrl Pts',(-16.6636729891647,-19.3941443917744,
16.9178643375515));
#168062=CARTESIAN_POINT('Ctrl Pts',(-16.6652572889207,-19.4014988255602,
16.918314076231));
#168063=CARTESIAN_POINT('Ctrl Pts',(-16.6748611173275,-19.4449539748703,
16.9209622094855));
#168064=CARTESIAN_POINT('Ctrl Pts',(-16.6837867874714,-19.480850373623,
16.923111961268));
#168065=CARTESIAN_POINT('Ctrl Pts',(-16.7159760238316,-19.5971970646749,
16.9300102235489));
#168066=CARTESIAN_POINT('Ctrl Pts',(-16.7430730715202,-19.6765082426188,
16.9346045941927));
#168067=CARTESIAN_POINT('Ctrl Pts',(-16.8430743112417,-19.9207972901339,
16.9489788794502));
#168068=CARTESIAN_POINT('Ctrl Pts',(-16.9323569716125,-20.0781634485424,
16.9586444012629));
#168069=CARTESIAN_POINT('Ctrl Pts',(-17.0540570765474,-20.240406813255,
16.9704341212555));
#168070=CARTESIAN_POINT('Ctrl Pts',(-17.0679146180673,-20.2582770703781,
16.9717592439999));
#168071=CARTESIAN_POINT('Ctrl Pts',(-17.0879863379307,-20.2833218872036,
16.9736561843642));
#168072=CARTESIAN_POINT('Ctrl Pts',(-17.0939668880918,-20.2906823112529,
16.9742186695119));
#168073=CARTESIAN_POINT('Ctrl Pts',(-17.1037832329451,-20.3025990380786,
16.9751376373646));
#168074=CARTESIAN_POINT('Ctrl Pts',(-17.1075891965159,-20.3071798280818,
16.9754929075487));
#168075=CARTESIAN_POINT('Ctrl Pts',(-17.1156116581692,-20.31675304647,16.9762396554278));
#168076=CARTESIAN_POINT('Ctrl Pts',(-17.1198320382819,-20.3217421263506,
16.9766312899186));
#168077=CARTESIAN_POINT('Ctrl Pts',(-17.1299555941359,-20.3335978218622,
16.9775678963823));
#168078=CARTESIAN_POINT('Ctrl Pts',(-17.1358798241044,-20.340446216737,
16.9781137349578));
#168079=CARTESIAN_POINT('Ctrl Pts',(-17.1561244258381,-20.3635476986631,
16.9799715573836));
#168080=CARTESIAN_POINT('Ctrl Pts',(-17.1706498834008,-20.3796185034324,
16.9812920867932));
#168081=CARTESIAN_POINT('Ctrl Pts',(-17.2520210338456,-20.4669153775368,
16.9886245994275));
#168082=CARTESIAN_POINT('Ctrl Pts',(-17.3234792587851,-20.5336627178883,
16.994835812582));
#168083=CARTESIAN_POINT('Ctrl Pts',(-17.5099162840561,-20.6850965982024,
17.0104620336871));
#168084=CARTESIAN_POINT('Ctrl Pts',(-17.6293375144373,-20.7635526363035,
17.0200145367689));
#168085=CARTESIAN_POINT('Ctrl Pts',(-17.8089521712131,-20.8571448643554,
17.0331578346631));
#168086=CARTESIAN_POINT('Ctrl Pts',(-17.8633330561953,-20.882603771998,
17.0369878252698));
#168087=CARTESIAN_POINT('Ctrl Pts',(-17.927002448383,-20.9091725407835,
17.0412456547012));
#168088=CARTESIAN_POINT('Ctrl Pts',(-17.9352996383769,-20.9125731665961,
17.0417961938796));
#168089=CARTESIAN_POINT('Ctrl Pts',(-17.9478263141324,-20.917614537629,
17.0426205966818));
#168090=CARTESIAN_POINT('Ctrl Pts',(-17.9520397545371,-20.9192945255579,
17.0428967426908));
#168091=CARTESIAN_POINT('Ctrl Pts',(-17.9595769344767,-20.9222717185525,
17.0433886335362));
#168092=CARTESIAN_POINT('Ctrl Pts',(-17.9628985741172,-20.9235740718949,
17.0436046846649));
#168093=CARTESIAN_POINT('Ctrl Pts',(-17.9700824553348,-20.9263698060981,
17.0440703771532));
#168094=CARTESIAN_POINT('Ctrl Pts',(-17.973945778666,-20.9278602500142,
17.0443198416477));
#168095=CARTESIAN_POINT('Ctrl Pts',(-17.9847081014494,-20.9319760449427,
17.0450121501837));
#168096=CARTESIAN_POINT('Ctrl Pts',(-17.9916165733289,-20.9345766918909,
17.0454535384972));
#168097=CARTESIAN_POINT('Ctrl Pts',(-18.0310433374864,-20.9491836439789,
17.0479561804461));
#168098=CARTESIAN_POINT('Ctrl Pts',(-18.0638410686655,-20.9604267218073,
17.0499748109498));
#168099=CARTESIAN_POINT('Ctrl Pts',(-18.1686092808636,-20.9934887469145,
17.0562680637444));
#168100=CARTESIAN_POINT('Ctrl Pts',(-18.2414768688217,-21.0122829120892,
17.0604179200224));
#168101=CARTESIAN_POINT('Ctrl Pts',(-18.5047006749382,-21.0654062408314,
17.0750830272929));
#168102=CARTESIAN_POINT('Ctrl Pts',(-18.6985300441149,-21.0775118966688,
17.0853827311156));
#168103=CARTESIAN_POINT('Ctrl Pts',(-18.9124866154572,-21.0615692744244,
17.0978722171974));
#168104=CARTESIAN_POINT('Ctrl Pts',(-18.9336390197124,-21.0596726997015,
17.0991178779777));
#168105=CARTESIAN_POINT('Ctrl Pts',(-18.9630312679992,-21.0565909020386,
17.1008653210772));
#168106=CARTESIAN_POINT('Ctrl Pts',(-18.9712984965738,-21.0556747864598,
17.1013586523916));
#168107=CARTESIAN_POINT('Ctrl Pts',(-18.9855603310346,-21.0540092517808,
17.1022129342335));
#168108=CARTESIAN_POINT('Ctrl Pts',(-18.9915575636832,-21.053282845061,
17.1025731563047));
#168109=CARTESIAN_POINT('Ctrl Pts',(-19.0039713265761,-21.0517253022865,
17.1033208687463));
#168110=CARTESIAN_POINT('Ctrl Pts',(-19.0103873130794,-21.0508904006551,
17.1037084744519));
#168111=CARTESIAN_POINT('Ctrl Pts',(-19.0254065747516,-21.0488659087179,
17.1046185750984));
#168112=CARTESIAN_POINT('Ctrl Pts',(-19.0340065094453,-21.0476527674522,
17.1051418098431));
#168113=CARTESIAN_POINT('Ctrl Pts',(-19.0619171734273,-21.0435402544047,
17.1068469531146));
#168114=CARTESIAN_POINT('Ctrl Pts',(-19.081194870727,-21.0404266781636,
17.1080356146905));
#168115=CARTESIAN_POINT('Ctrl Pts',(-19.1796641441247,-21.0231216836101,
17.1141650097136));
#168116=CARTESIAN_POINT('Ctrl Pts',(-19.2580346514347,-21.0046925297819,
17.1192390786239));
#168117=CARTESIAN_POINT('Ctrl Pts',(-19.4872281638598,-20.9368147407889,
17.1346478897531));
#168118=CARTESIAN_POINT('Ctrl Pts',(-19.6337378918041,-20.8748382907497,
17.1452934873961));
#168119=CARTESIAN_POINT('Ctrl Pts',(-19.8277912654149,-20.7656745182451,
17.1597745925));
#168120=CARTESIAN_POINT('Ctrl Pts',(-19.8821872105743,-20.731736607114,
17.1638734363951));
#168121=CARTESIAN_POINT('Ctrl Pts',(-19.9425484966151,-20.6901554424236,
17.1683981386437));
#168122=CARTESIAN_POINT('Ctrl Pts',(-19.95009845222,-20.6848815228588,17.1689636296993));
#168123=CARTESIAN_POINT('Ctrl Pts',(-19.9613055878804,-20.6769436105449,
17.1698020666634));
#168124=CARTESIAN_POINT('Ctrl Pts',(-19.9649889174969,-20.6743169718378,
17.1700774680032));
#168125=CARTESIAN_POINT('Ctrl Pts',(-19.9714780795977,-20.6696579999997,
17.1705623379281));
#168126=CARTESIAN_POINT('Ctrl Pts',(-19.9742873622996,-20.6676305726915,
17.1707721379487));
#168127=CARTESIAN_POINT('Ctrl Pts',(-19.9771026961052,-20.6655882490026,
17.170982276612));
#168128=CARTESIAN_POINT('Ctrl Pts',(-19.9771136738019,-20.6655802853063,
17.170983095994));
#168129=CARTESIAN_POINT('Ctrl Pts',(-19.9771354433339,-20.6655644924265,
17.1709847208818));
#168130=CARTESIAN_POINT('Ctrl Pts',(-19.9771462357018,-20.6655566628618,
17.1709855264275));
#168131=CARTESIAN_POINT('Ctrl Pts',(-19.9771676399043,-20.6655411343959,
17.1709871240405));
#168132=CARTESIAN_POINT('Ctrl Pts',(-19.9771782513505,-20.6655334357815,
17.170987916079));
#168133=CARTESIAN_POINT('Ctrl Pts',(-19.9771992967715,-20.6655181670099,
17.1709894869063));
#168134=CARTESIAN_POINT('Ctrl Pts',(-19.9772097309217,-20.6655105967305,
17.1709902657083));
#168135=CARTESIAN_POINT('Ctrl Pts',(-19.977229852374,-20.6654959977512,
17.1709917675649));
#168136=CARTESIAN_POINT('Ctrl Pts',(-19.9772395398793,-20.665488968924,
17.1709924906349));
#168137=CARTESIAN_POINT('Ctrl Pts',(-19.9772588793793,-20.665474936784,
17.1709939341217));
#168138=CARTESIAN_POINT('Ctrl Pts',(-19.9772685307359,-20.6654679339352,
17.1709946544909));
#168139=CARTESIAN_POINT('Ctrl Pts',(-19.9772877963939,-20.6654539548757,
17.1709960924611));
#168140=CARTESIAN_POINT('Ctrl Pts',(-19.9772974112058,-20.6654469782955,
17.1709968101001));
#168141=CARTESIAN_POINT('Ctrl Pts',(-19.9773166058526,-20.6654330502682,
17.1709982427649));
#168142=CARTESIAN_POINT('Ctrl Pts',(-19.9773261851852,-20.6654260991863,
17.1709989577532));
#168143=CARTESIAN_POINT('Ctrl Pts',(-19.9773453071036,-20.6654122234426,
17.1710003849846));
#168144=CARTESIAN_POINT('Ctrl Pts',(-19.9773548504042,-20.6654052982629,
17.171001097281));
#168145=CARTESIAN_POINT('Ctrl Pts',(-19.9806584190717,-20.6630079925801,
17.1712476698269));
#168146=CARTESIAN_POINT('Ctrl Pts',(-19.9839455755235,-20.6606080953178,
17.1714928669859));
#168147=CARTESIAN_POINT('Ctrl Pts',(-19.9907411636819,-20.655616644728,
17.1719995009706));
#168148=CARTESIAN_POINT('Ctrl Pts',(-19.9942485519808,-20.6530236955077,
17.1722608409171));
#168149=CARTESIAN_POINT('Ctrl Pts',(-20.0031488824285,-20.6464012023043,
17.1729237095971));
#168150=CARTESIAN_POINT('Ctrl Pts',(-20.0085307082385,-20.6423567069021,
17.1733242436459));
#168151=CARTESIAN_POINT('Ctrl Pts',(-20.0240018453476,-20.63061409789,17.1744751195144));
#168152=CARTESIAN_POINT('Ctrl Pts',(-20.034041526479,-20.6228507104135,
17.175221290356));
#168153=CARTESIAN_POINT('Ctrl Pts',(-20.0682671456734,-20.5958897895153,
17.177765036077));
#168154=CARTESIAN_POINT('Ctrl Pts',(-20.0921035374571,-20.5762528834093,
17.1795366818744));
#168155=CARTESIAN_POINT('Ctrl Pts',(-20.2111558238006,-20.4737212301426,
17.1884346582502));
#168156=CARTESIAN_POINT('Ctrl Pts',(-20.2992558521049,-20.3829451181268,
17.195197038758));
#168157=CARTESIAN_POINT('Ctrl Pts',(-20.4088523546216,-20.247702555824,
17.2046738914946));
#168158=CARTESIAN_POINT('Ctrl Pts',(-20.437690006796,-20.2095435068449,
17.207288535583));
#168159=CARTESIAN_POINT('Ctrl Pts',(-20.5177923269409,-20.0957309612451,
17.2149889304014));
#168160=CARTESIAN_POINT('Ctrl Pts',(-20.5654773367654,-20.0177032377189,
17.2201527915231));
#168161=CARTESIAN_POINT('Ctrl Pts',(-20.6143678990597,-19.9246739637255,
17.2263139475871));
#168162=CARTESIAN_POINT('Ctrl Pts',(-20.6206458751859,-19.9124402135795,
17.2271241155909));
#168163=CARTESIAN_POINT('Ctrl Pts',(-20.6305202472311,-19.8927278016584,
17.228429861149));
#168164=CARTESIAN_POINT('Ctrl Pts',(-20.6341926876479,-19.8852875182859,
17.2289227732065));
#168165=CARTESIAN_POINT('Ctrl Pts',(-20.6406341832621,-19.8720415548439,
17.2298005119924));
#168166=CARTESIAN_POINT('Ctrl Pts',(-20.6434207110624,-19.8662444520911,
17.2301847241456));
#168167=CARTESIAN_POINT('Ctrl Pts',(-20.6491701054274,-19.8541424483194,
17.2309869883666));
#168168=CARTESIAN_POINT('Ctrl Pts',(-20.6521283521303,-19.8478354495841,
17.2314051948477));
#168169=CARTESIAN_POINT('Ctrl Pts',(-20.6597270499608,-19.8314247814691,
17.2324936855358));
#168170=CARTESIAN_POINT('Ctrl Pts',(-20.6643190860116,-19.8212990486623,
17.2331656284302));
#168171=CARTESIAN_POINT('Ctrl Pts',(-20.6838886323732,-19.7772272266871,
17.2360919506323));
#168172=CARTESIAN_POINT('Ctrl Pts',(-20.6980512870115,-19.7429285195912,
17.2383739101748));
#168173=CARTESIAN_POINT('Ctrl Pts',(-20.7332564627841,-19.6508837265034,
17.2445136879773));
#168174=CARTESIAN_POINT('Ctrl Pts',(-20.7526971487398,-19.5925666060741,
17.2484207466186));
#168175=CARTESIAN_POINT('Ctrl Pts',(-20.8236534047749,-19.3441763308729,
17.2651063524798));
#168176=CARTESIAN_POINT('Ctrl Pts',(-20.8510532927738,-19.1482730593989,
17.2784800810824));
#168177=CARTESIAN_POINT('Ctrl Pts',(-20.8509999221897,-18.9514260237555,
17.2909082342155));
#168178=CARTESIAN_POINT('Ctrl Pts',(-20.8509999215524,-18.9514236778724,
17.2909083823253));
#168179=CARTESIAN_POINT('Ctrl Pts',(-20.8509956361684,-18.935682207655,
17.2919022365754));
#168180=CARTESIAN_POINT('Ctrl Pts',(-20.8508157763398,-18.919940709559,
17.2928889660196));
#168181=CARTESIAN_POINT('Ctrl Pts',(-20.850214855114,-18.8933322838161,
17.2945432125346));
#168182=CARTESIAN_POINT('Ctrl Pts',(-20.8498856304743,-18.882464226158,
17.2952150250629));
#168183=CARTESIAN_POINT('Ctrl Pts',(-20.849291499802,-18.8668317566442,
17.2961753415949));
#168184=CARTESIAN_POINT('Ctrl Pts',(-20.8490942019215,-18.8620651524252,
17.2964673539702));
#168185=CARTESIAN_POINT('Ctrl Pts',(-20.8487208814448,-18.8537280704049,
17.2969766461215));
#168186=CARTESIAN_POINT('Ctrl Pts',(-20.8485519258228,-18.8501573174116,
17.2971943076044));
#168187=CARTESIAN_POINT('Ctrl Pts',(-20.8482044718159,-18.8431880863994,
17.2976181945417));
#168188=CARTESIAN_POINT('Ctrl Pts',(-20.848026821273,-18.8397895692581,
17.2978244667218));
#168189=CARTESIAN_POINT('Ctrl Pts',(-20.8476550554098,-18.8329920284264,
17.298236155742));
#168190=CARTESIAN_POINT('Ctrl Pts',(-20.8474609359881,-18.8295930435458,
17.2984415725897));
#168191=CARTESIAN_POINT('Ctrl Pts',(-20.846973681577,-18.8214082289121,
17.298935190113));
#168192=CARTESIAN_POINT('Ctrl Pts',(-20.8466724838614,-18.8166228724245,
17.2992229416761));
#168193=CARTESIAN_POINT('Ctrl Pts',(-20.8455076197931,-18.7990673600145,
17.3002756055668));
#168194=CARTESIAN_POINT('Ctrl Pts',(-20.8445443857378,-18.786303787924,
17.3010351496069));
#168195=CARTESIAN_POINT('Ctrl Pts',(-20.8412948271697,-18.7478907425378,
17.3033057236318));
#168196=CARTESIAN_POINT('Ctrl Pts',(-20.838656156522,-18.7222726321763,
17.3047993762694));
#168197=CARTESIAN_POINT('Ctrl Pts',(-20.8160114727723,-18.5358628444971,
17.3155583767712));
#168198=CARTESIAN_POINT('Ctrl Pts',(-20.7780845405037,-18.3778969488394,
17.3241155065484));
#168199=CARTESIAN_POINT('Ctrl Pts',(-20.7225805737356,-18.2258896077308,
17.3329786086887));
#168200=CARTESIAN_POINT('Origin',(-18.734,-18.952,0.));
#168201=CARTESIAN_POINT('',(-20.7225805841812,-18.2258896363379,18.3568546368673));
#168202=CARTESIAN_POINT('',(-20.7225805578635,-18.2258895642624,18.13180632455));
#168203=CARTESIAN_POINT('',(-20.7225805737622,-18.2258896078036,0.));
#168204=CARTESIAN_POINT('Ctrl Pts',(-20.7225805841812,-18.2258896363379,
18.3568546368673));
#168205=CARTESIAN_POINT('Ctrl Pts',(-20.727923816343,-18.2405230147683,
18.3558520868808));
#168206=CARTESIAN_POINT('Ctrl Pts',(-20.7331061395786,-18.2552170561466,
18.3548454415314));
#168207=CARTESIAN_POINT('Ctrl Pts',(-20.7819943705009,-18.3988736054763,
18.3450068227108));
#168208=CARTESIAN_POINT('Ctrl Pts',(-20.8133221923182,-18.5317079699484,
18.3359031584784));
#168209=CARTESIAN_POINT('Ctrl Pts',(-20.8417531210889,-18.7406859733689,
18.3221216814772));
#168210=CARTESIAN_POINT('Ctrl Pts',(-20.8479010506242,-18.8152459538833,
18.3173148853575));
#168211=CARTESIAN_POINT('Ctrl Pts',(-20.8503509139878,-18.8988371843921,
18.3121558368701));
#168212=CARTESIAN_POINT('Ctrl Pts',(-20.8505548518705,-18.9076937766778,
18.3116121302995));
#168213=CARTESIAN_POINT('Ctrl Pts',(-20.8507777609052,-18.9210041598406,
18.3107996272138));
#168214=CARTESIAN_POINT('Ctrl Pts',(-20.8508382797461,-18.9254570271004,
18.310528588847));
#168215=CARTESIAN_POINT('Ctrl Pts',(-20.8509183444085,-18.9331296582656,
18.3100629466643));
#168216=CARTESIAN_POINT('Ctrl Pts',(-20.8509445960285,-18.9363492967765,
18.3098679704955));
#168217=CARTESIAN_POINT('Ctrl Pts',(-20.8509874023568,-18.9436391203129,
18.3094274664756));
#168218=CARTESIAN_POINT('Ctrl Pts',(-20.8509995645971,-18.9477092909051,
18.3091821873668));
#168219=CARTESIAN_POINT('Ctrl Pts',(-20.8510007238652,-18.9588398526186,
18.3085132019213));
#168220=CARTESIAN_POINT('Ctrl Pts',(-20.8509661391233,-18.9659002674402,
18.3080907953781));
#168221=CARTESIAN_POINT('Ctrl Pts',(-20.8505991936105,-19.0029597814589,
18.3058832357657));
#168222=CARTESIAN_POINT('Ctrl Pts',(-20.8496644747793,-19.0329511230616,
18.3041297816601));
#168223=CARTESIAN_POINT('Ctrl Pts',(-20.8449576280264,-19.1226665407886,
18.298956837913));
#168224=CARTESIAN_POINT('Ctrl Pts',(-20.8392906833233,-19.1822636369617,
18.2956162480313));
#168225=CARTESIAN_POINT('Ctrl Pts',(-20.8082534011065,-19.4070597635603,
18.2831217660778));
#168226=CARTESIAN_POINT('Ctrl Pts',(-20.7658883757387,-19.5692821115655,
18.2742744347359));
#168227=CARTESIAN_POINT('Ctrl Pts',(-20.6832637936845,-19.779991040733,
18.2615099001174));
#168228=CARTESIAN_POINT('Ctrl Pts',(-20.6593332571522,-19.8342071298561,
18.2581085315601));
#168229=CARTESIAN_POINT('Ctrl Pts',(-20.6277538903282,-19.8983271407323,
18.2539095578999));
#168230=CARTESIAN_POINT('Ctrl Pts',(-20.6222502135285,-19.9092617072119,
18.2531871747713));
#168231=CARTESIAN_POINT('Ctrl Pts',(-20.6130255255541,-19.927199958927,
18.251991363438));
#168232=CARTESIAN_POINT('Ctrl Pts',(-20.609359395494,-19.9342316532726,
18.2515198662545));
#168233=CARTESIAN_POINT('Ctrl Pts',(-20.6026761213407,-19.9468764556063,
18.2506669537519));
#168234=CARTESIAN_POINT('Ctrl Pts',(-20.5996729629049,-19.9524968778072,
18.2502860377094));
#168235=CARTESIAN_POINT('Ctrl Pts',(-20.5931997995598,-19.9644809339232,
18.2494699188435));
#168236=CARTESIAN_POINT('Ctrl Pts',(-20.5897224046173,-19.9708404640606,
18.249034455803));
#168237=CARTESIAN_POINT('Ctrl Pts',(-20.5802117969951,-19.9880234293588,
18.2478513438037));
#168238=CARTESIAN_POINT('Ctrl Pts',(-20.5741161729741,-19.998811828969,
18.247101462982));
#168239=CARTESIAN_POINT('Ctrl Pts',(-20.5423240491179,-20.0539436306089,
18.2432324027919));
#168240=CARTESIAN_POINT('Ctrl Pts',(-20.5151199527809,-20.0973936585241,
18.2400588250411));
#168241=CARTESIAN_POINT('Ctrl Pts',(-20.3905655885019,-20.2811476841275,
18.2260769719922));
#168242=CARTESIAN_POINT('Ctrl Pts',(-20.2780252262199,-20.410359560337,
18.2147052045248));
#168243=CARTESIAN_POINT('Ctrl Pts',(-20.0828499636757,-20.5862471663019,
18.197426879911));
#168244=CARTESIAN_POINT('Ctrl Pts',(-20.0105246495634,-20.6433452711746,
18.1914506510582));
#168245=CARTESIAN_POINT('Ctrl Pts',(-19.9267413830612,-20.7010427300654,
18.1851657057317));
#168246=CARTESIAN_POINT('Ctrl Pts',(-19.9187408297852,-20.7064719014111,
18.184571666022));
#168247=CARTESIAN_POINT('Ctrl Pts',(-19.9068673208059,-20.714411001995,
18.1836993899339));
#168248=CARTESIAN_POINT('Ctrl Pts',(-19.9030230341607,-20.7169632967005,
18.18341840493));
#168249=CARTESIAN_POINT('Ctrl Pts',(-19.896185488613,-20.7214707320428,
18.1829212180328));
#168250=CARTESIAN_POINT('Ctrl Pts',(-19.8931955948251,-20.7234308778818,
18.1827046830001));
#168251=CARTESIAN_POINT('Ctrl Pts',(-19.8867759877724,-20.7276162975148,
18.1822416376643));
#168252=CARTESIAN_POINT('Ctrl Pts',(-19.8833447995145,-20.7298392071457,
18.1819952847579));
#168253=CARTESIAN_POINT('Ctrl Pts',(-19.8739015190362,-20.7359183113465,
18.1813203333773));
#168254=CARTESIAN_POINT('Ctrl Pts',(-19.8678762534227,-20.7397540826111,
18.1808930738412));
#168255=CARTESIAN_POINT('Ctrl Pts',(-19.8354946863946,-20.7601390921028,
18.1786143173532));
#168256=CARTESIAN_POINT('Ctrl Pts',(-19.8087937969521,-20.7761370687922,
18.1767969984881));
#168257=CARTESIAN_POINT('Ctrl Pts',(-19.6393308138361,-20.8726581660643,
18.1655817890799));
#168258=CARTESIAN_POINT('Ctrl Pts',(-19.4879600380041,-20.936970608127,
18.1569210803046));
#168259=CARTESIAN_POINT('Ctrl Pts',(-19.21821219991,-21.016210652848,18.1415316974819));
#168260=CARTESIAN_POINT('Ctrl Pts',(-19.1032203146341,-21.0398453333557,
18.1349896364419));
#168261=CARTESIAN_POINT('Ctrl Pts',(-18.9726798992676,-21.0555506288579,
18.1272870429984));
#168262=CARTESIAN_POINT('Ctrl Pts',(-18.9584707408627,-21.0571142995226,
18.1264452480962));
#168263=CARTESIAN_POINT('Ctrl Pts',(-18.9358327566271,-21.0593737316021,
18.1250982948451));
#168264=CARTESIAN_POINT('Ctrl Pts',(-18.9274135615199,-21.0601631097593,
18.1245960802784));
#168265=CARTESIAN_POINT('Ctrl Pts',(-18.9125575902411,-21.0614662549206,
18.1237075700652));
#168266=CARTESIAN_POINT('Ctrl Pts',(-18.906122733441,-21.0620010561345,
18.1233219409166));
#168267=CARTESIAN_POINT('Ctrl Pts',(-18.8928091429336,-21.0630462413223,
18.1225224461373));
#168268=CARTESIAN_POINT('Ctrl Pts',(-18.8859301677541,-21.0635524618761,
18.1221084543894));
#168269=CARTESIAN_POINT('Ctrl Pts',(-18.8682680002355,-21.064765457926,
18.121043135992));
#168270=CARTESIAN_POINT('Ctrl Pts',(-18.8574817455996,-21.0654232959384,
18.1203902809032));
#168271=CARTESIAN_POINT('Ctrl Pts',(-18.8124547121445,-21.0678235554727,
18.1176551976899));
#168272=CARTESIAN_POINT('Ctrl Pts',(-18.7781807533269,-21.0688165496486,
18.1155496590693));
#168273=CARTESIAN_POINT('Ctrl Pts',(-18.688839464362,-21.0692343228054,
18.1099964427806));
#168274=CARTESIAN_POINT('Ctrl Pts',(-18.633794657651,-21.0673436415773,
18.1065104013983));
#168275=CARTESIAN_POINT('Ctrl Pts',(-18.4698251969851,-21.0552973934552,
18.0959428714677));
#168276=CARTESIAN_POINT('Ctrl Pts',(-18.3615529979198,-21.0388464283819,
18.0887129854226));
#168277=CARTESIAN_POINT('Ctrl Pts',(-18.2114912298976,-21.0039924234121,
18.0785363688311));
#168278=CARTESIAN_POINT('Ctrl Pts',(-18.1682672901211,-20.9924987130141,
18.0755880089385));
#168279=CARTESIAN_POINT('Ctrl Pts',(-18.1012772324308,-20.9723928515956,
18.0710175203661));
#168280=CARTESIAN_POINT('Ctrl Pts',(-18.0772463794659,-20.9647096482502,
18.0693778409696));
#168281=CARTESIAN_POINT('Ctrl Pts',(-18.0061316575159,-20.9405633327487,
18.0645353213173));
#168282=CARTESIAN_POINT('Ctrl Pts',(-17.9594824762451,-20.9228627359995,
18.0613715088615));
#168283=CARTESIAN_POINT('Ctrl Pts',(-17.9062943651239,-20.9005003091176,
18.0578132958856));
#168284=CARTESIAN_POINT('Ctrl Pts',(-17.899107000947,-20.8974315092235,
18.057333533971));
#168285=CARTESIAN_POINT('Ctrl Pts',(-17.8876573644764,-20.8924677007372,
18.0565711557512));
#168286=CARTESIAN_POINT('Ctrl Pts',(-17.8833841550521,-20.8905983182683,
18.0562870459428));
#168287=CARTESIAN_POINT('Ctrl Pts',(-17.8758323811237,-20.8872648990781,
18.0557857526248));
#168288=CARTESIAN_POINT('Ctrl Pts',(-17.8725513201089,-20.8858066253754,
18.0555682214023));
#168289=CARTESIAN_POINT('Ctrl Pts',(-17.8656110037712,-20.8827008196495,
18.0551086682571));
#168290=CARTESIAN_POINT('Ctrl Pts',(-17.8619527254979,-20.8810512319314,
18.0548667747834));
#168291=CARTESIAN_POINT('Ctrl Pts',(-17.8521058793528,-20.8765773650674,
18.0542165376706));
#168292=CARTESIAN_POINT('Ctrl Pts',(-17.8459261362952,-20.8737336156806,
18.053809374079));
#168293=CARTESIAN_POINT('Ctrl Pts',(-17.8155051845937,-20.8595566422519,
18.0518090478888));
#168294=CARTESIAN_POINT('Ctrl Pts',(-17.7914654681454,-20.847793732554,
18.0502409302592));
#168295=CARTESIAN_POINT('Ctrl Pts',(-17.7228371599742,-20.8125848346542,
18.0457826621028));
#168296=CARTESIAN_POINT('Ctrl Pts',(-17.6788521079625,-20.7879983166106,
18.0429479230668));
#168297=CARTESIAN_POINT('Ctrl Pts',(-17.5228299208417,-20.6933248420271,
18.0328274459526));
#168298=CARTESIAN_POINT('Ctrl Pts',(-17.4165383533822,-20.6143604956974,
18.0257891302147));
#168299=CARTESIAN_POINT('Ctrl Pts',(-17.2410217493351,-20.4564957652909,
18.0128026653224));
#168300=CARTESIAN_POINT('Ctrl Pts',(-17.1689780628106,-20.3814033227774,
18.0069635370779));
#168301=CARTESIAN_POINT('Ctrl Pts',(-17.0937841342084,-20.2904986119138,
18.0000501285924));
#168302=CARTESIAN_POINT('Ctrl Pts',(-17.0849323036247,-20.2795776207272,
17.9992221052818));
#168303=CARTESIAN_POINT('Ctrl Pts',(-17.0709740091984,-20.2620014883353,
17.997893082113));
#168304=CARTESIAN_POINT('Ctrl Pts',(-17.065797102752,-20.2554026377321,
17.9973949032759));
#168305=CARTESIAN_POINT('Ctrl Pts',(-17.0567111208458,-20.2436781975901,
17.9965110825607));
#168306=CARTESIAN_POINT('Ctrl Pts',(-17.0527859649435,-20.2385651624284,
17.9961260845979));
#168307=CARTESIAN_POINT('Ctrl Pts',(-17.0446916909445,-20.2279210050911,
17.9953254697914));
#168308=CARTESIAN_POINT('Ctrl Pts',(-17.0405262489611,-20.2223871957183,
17.9949097148293));
#168309=CARTESIAN_POINT('Ctrl Pts',(-17.0298535752569,-20.2080627301401,
17.9938346897126));
#168310=CARTESIAN_POINT('Ctrl Pts',(-17.0233872356521,-20.1992419903254,
17.9931738370211));
#168311=CARTESIAN_POINT('Ctrl Pts',(-16.9962582801869,-20.1616275171632,
17.9903601918649));
#168312=CARTESIAN_POINT('Ctrl Pts',(-16.9762530581476,-20.1323687835299,
17.9881823815818));
#168313=CARTESIAN_POINT('Ctrl Pts',(-16.9256642718921,-20.0542401112198,
17.9823914183201));
#168314=CARTESIAN_POINT('Ctrl Pts',(-16.896327505035,-20.0046016523789,
17.9787356803089));
#168315=CARTESIAN_POINT('Ctrl Pts',(-16.7931618785148,-19.8125550916975,
17.9646949379143));
#168316=CARTESIAN_POINT('Ctrl Pts',(-16.7335762438135,-19.6631294708399,
17.953928257806));
#168317=CARTESIAN_POINT('Ctrl Pts',(-16.6876722885981,-19.4946199940057,
17.942569155782));
#168318=CARTESIAN_POINT('Ctrl Pts',(-16.6840529924436,-19.4807824131925,
17.9416423151621));
#168319=CARTESIAN_POINT('Ctrl Pts',(-16.678091015169,-19.4570064089786,
17.9400610435645));
#168320=CARTESIAN_POINT('Ctrl Pts',(-16.6756795120582,-19.4470858530889,
17.9394045915666));
#168321=CARTESIAN_POINT('Ctrl Pts',(-16.6639027907777,-19.3970643846387,
17.9361125930817));
#168322=CARTESIAN_POINT('Ctrl Pts',(-16.655636573956,-19.3567106947001,
17.9335146964976));
#168323=CARTESIAN_POINT('Ctrl Pts',(-16.6472805078279,-19.3088549163633,
17.930521480672));
#168324=CARTESIAN_POINT('Ctrl Pts',(-16.6460468456,-19.3015644419097,17.9300678722536));
#168325=CARTESIAN_POINT('Ctrl Pts',(-16.6441094919014,-19.2897391315461,
17.9293361378908));
#168326=CARTESIAN_POINT('Ctrl Pts',(-16.6433823163802,-19.2852082812151,
17.929056731494));
#168327=CARTESIAN_POINT('Ctrl Pts',(-16.6421152128537,-19.2771458141817,
17.9285612830895));
#168328=CARTESIAN_POINT('Ctrl Pts',(-16.6415694877184,-19.273615166166,
17.928344916689));
#168329=CARTESIAN_POINT('Ctrl Pts',(-16.640415942359,-19.2660249077274,
17.9278810572489));
#168330=CARTESIAN_POINT('Ctrl Pts',(-16.6398109924286,-19.261964917865,
17.9276337277719));
#168331=CARTESIAN_POINT('Ctrl Pts',(-16.6381749599386,-19.2507615954838,
17.9269533405965));
#168332=CARTESIAN_POINT('Ctrl Pts',(-16.6371685812266,-19.243614632934,
17.9265216579451));
#168333=CARTESIAN_POINT('Ctrl Pts',(-16.6318742691093,-19.2045711290714,
17.9241755801043));
#168334=CARTESIAN_POINT('Ctrl Pts',(-16.6282773117048,-19.1725832672436,
17.9222977985801));
#168335=CARTESIAN_POINT('Ctrl Pts',(-16.6108971997941,-18.9781914165722,
17.9110876207304));
#168336=CARTESIAN_POINT('Ctrl Pts',(-16.615176113916,-18.8147090529558,
17.9024736817256));
#168337=CARTESIAN_POINT('Ctrl Pts',(-16.6546729276598,-18.5375589534647,
17.8871483232951));
#168338=CARTESIAN_POINT('Ctrl Pts',(-16.6807308552497,-18.423376311942,
17.8806207754489));
#168339=CARTESIAN_POINT('Ctrl Pts',(-16.7203991369298,-18.2983144447326,
17.872934518568));
#168340=CARTESIAN_POINT('Ctrl Pts',(-16.7248577776747,-18.2847363665848,
17.8720929300055));
#168341=CARTESIAN_POINT('Ctrl Pts',(-16.7321725086049,-18.2631987343387,
17.8707462452477));
#168342=CARTESIAN_POINT('Ctrl Pts',(-16.7349394521248,-18.2552092052508,
17.8702440909771));
#168343=CARTESIAN_POINT('Ctrl Pts',(-16.7399036960803,-18.2411479604066,
17.8693556510027));
#168344=CARTESIAN_POINT('Ctrl Pts',(-16.7420810653653,-18.2350692865287,
17.8689700314587));
#168345=CARTESIAN_POINT('Ctrl Pts',(-16.7466420067172,-18.2225174510772,
17.8681705208135));
#168346=CARTESIAN_POINT('Ctrl Pts',(-16.7490294738545,-18.2160457954264,
17.8677565034186));
#168347=CARTESIAN_POINT('Ctrl Pts',(-16.7552388514241,-18.199464197434,
17.8666910436713));
#168348=CARTESIAN_POINT('Ctrl Pts',(-16.7591065991258,-18.1893717382264,
17.8660380720966));
#168349=CARTESIAN_POINT('Ctrl Pts',(-16.7755712363579,-18.1473743888241,
17.8633018602378));
#168350=CARTESIAN_POINT('Ctrl Pts',(-16.7888647574681,-18.115749876861,
17.8611952853886));
#168351=CARTESIAN_POINT('Ctrl Pts',(-16.8254985865632,-18.0342053379851,
17.8556386846199));
#168352=CARTESIAN_POINT('Ctrl Pts',(-16.8500288197882,-17.9848513773637,
17.852150236659));
#168353=CARTESIAN_POINT('Ctrl Pts',(-16.9289261427216,-17.840531026078,
17.8415780836179));
#168354=CARTESIAN_POINT('Ctrl Pts',(-16.9887548601632,-17.7487665039285,
17.8343459963911));
#168355=CARTESIAN_POINT('Ctrl Pts',(-17.0844199624271,-17.6242790132634,
17.8239750033247));
#168356=CARTESIAN_POINT('Ctrl Pts',(-17.1147074189003,-17.5875040936933,
17.8208350019414));
#168357=CARTESIAN_POINT('Ctrl Pts',(-17.1586751012275,-17.5376465687959,
17.8164967139863));
#168358=CARTESIAN_POINT('Ctrl Pts',(-17.1713284933177,-17.5236786227049,
17.8152719797419));
#168359=CARTESIAN_POINT('Ctrl Pts',(-17.2202940475182,-17.4710557495798,
17.8106273512723));
#168360=CARTESIAN_POINT('Ctrl Pts',(-17.2578707559631,-17.4335978599135,
17.8072566589758));
#168361=CARTESIAN_POINT('Ctrl Pts',(-17.3032078547312,-17.3916799780263,
17.8034478289373));
#168362=CARTESIAN_POINT('Ctrl Pts',(-17.3096341987788,-17.3858113765512,
17.8029137080426));
#168363=CARTESIAN_POINT('Ctrl Pts',(-17.3194229320678,-17.3769822909379,
17.8021090595249));
#168364=CARTESIAN_POINT('Ctrl Pts',(-17.3227587389416,-17.3739926587881,
17.8018364052111));
#168365=CARTESIAN_POINT('Ctrl Pts',(-17.3287654079445,-17.3686436152918,
17.8013482697657));
#168366=CARTESIAN_POINT('Ctrl Pts',(-17.3314327487049,-17.366280350793,
17.8011325017971));
#168367=CARTESIAN_POINT('Ctrl Pts',(-17.3372437551414,-17.3611579314137,
17.8006645969034));
#168368=CARTESIAN_POINT('Ctrl Pts',(-17.340389624003,-17.3584013631583,
17.8004126520303));
#168369=CARTESIAN_POINT('Ctrl Pts',(-17.349254687633,-17.3506796758451,
17.7997064207209));
#168370=CARTESIAN_POINT('Ctrl Pts',(-17.354992453285,-17.3457358403098,
17.7992536868585));
#168371=CARTESIAN_POINT('Ctrl Pts',(-17.3895684469105,-17.3162659276918,
17.796550677727));
#168372=CARTESIAN_POINT('Ctrl Pts',(-17.4190357323694,-17.2924845491952,
17.7943514251423));
#168373=CARTESIAN_POINT('Ctrl Pts',(-17.5183858672402,-17.2166137233403,
17.7872144816035));
#168374=CARTESIAN_POINT('Ctrl Pts',(-17.5908502661414,-17.1680453090892,
17.7824434024078));
#168375=CARTESIAN_POINT('Ctrl Pts',(-17.817451341929,-17.0356623226124,
17.768164453403));
#168376=CARTESIAN_POINT('Ctrl Pts',(-17.9791705065439,-16.9663924702893,
17.7587402039719));
#168377=CARTESIAN_POINT('Ctrl Pts',(-18.1696788833234,-16.9114706480384,
17.7472193808982));
#168378=CARTESIAN_POINT('Ctrl Pts',(-18.1918880846909,-16.9054582903882,
17.7458714707137));
#168379=CARTESIAN_POINT('Ctrl Pts',(-18.2234468138566,-16.8974646205239,
17.7439475629521));
#168380=CARTESIAN_POINT('Ctrl Pts',(-18.2327190215832,-16.89518266306,17.7433812692646));
#168381=CARTESIAN_POINT('Ctrl Pts',(-18.2478102018781,-16.8915767207952,
17.7424577892536));
#168382=CARTESIAN_POINT('Ctrl Pts',(-18.253619958686,-16.8902144573037,
17.7421018397939));
#168383=CARTESIAN_POINT('Ctrl Pts',(-18.2657935338122,-16.8874142617773,
17.7413550601512));
#168384=CARTESIAN_POINT('Ctrl Pts',(-18.2721583863564,-16.8859811501632,
17.7409640793353));
#168385=CARTESIAN_POINT('Ctrl Pts',(-18.2873166923117,-16.8826416498728,
17.7400316206717));
#168386=CARTESIAN_POINT('Ctrl Pts',(-18.2961158216974,-16.8807618676034,
17.7394892961804));
#168387=CARTESIAN_POINT('Ctrl Pts',(-18.3258040470608,-16.8746171259111,
17.7376558202103));
#168388=CARTESIAN_POINT('Ctrl Pts',(-18.3467449882263,-16.8706117504819,
17.7363564238879));
#168389=CARTESIAN_POINT('Ctrl Pts',(-18.3967051818417,-16.8618359061918,
17.733240835881));
#168390=CARTESIAN_POINT('Ctrl Pts',(-18.4257697594218,-16.8573526029304,
17.7314159076659));
#168391=CARTESIAN_POINT('Ctrl Pts',(-18.6240074188167,-16.8309889644209,
17.7188822044678));
#168392=CARTESIAN_POINT('Ctrl Pts',(-18.7951749858893,-16.8290242793281,
17.7075589997895));
#168393=CARTESIAN_POINT('Ctrl Pts',(-19.0639324695801,-16.8584857817227,
17.6897454203541));
#168394=CARTESIAN_POINT('Ctrl Pts',(-19.1622974466557,-16.8763740102327,
17.6832372934216));
#168395=CARTESIAN_POINT('Ctrl Pts',(-19.2684333813919,-16.9035459636881,
17.6764682477308));
#168396=CARTESIAN_POINT('Ctrl Pts',(-19.2778083110832,-16.906014783282,
17.6758726031909));
#168397=CARTESIAN_POINT('Ctrl Pts',(-19.2916250249826,-16.909754992671,
17.6749984298098));
#168398=CARTESIAN_POINT('Ctrl Pts',(-19.2960799832256,-16.9109766214377,
17.6747171354141));
#168399=CARTESIAN_POINT('Ctrl Pts',(-19.3039761860761,-16.9131697146314,
17.6742196066378));
#168400=CARTESIAN_POINT('Ctrl Pts',(-19.3074190003406,-16.9141353244245,
17.6740030374042));
#168401=CARTESIAN_POINT('Ctrl Pts',(-19.3147899559618,-16.9162228228039,
17.6735401463265));
#168402=CARTESIAN_POINT('Ctrl Pts',(-19.3187172904802,-16.9173473566721,
17.6732939806903));
#168403=CARTESIAN_POINT('Ctrl Pts',(-19.3294884085617,-16.9204652684806,
17.6726200705718));
#168404=CARTESIAN_POINT('Ctrl Pts',(-19.3363254905344,-16.9224818757044,
17.6721936581587));
#168405=CARTESIAN_POINT('Ctrl Pts',(-19.3727667734363,-16.9334306575288,
17.6699275260774));
#168406=CARTESIAN_POINT('Ctrl Pts',(-19.4021844545463,-16.9429766196145,
17.6681215376675));
#168407=CARTESIAN_POINT('Ctrl Pts',(-19.4905803396192,-16.9738175161009,
17.662736428932));
#168408=CARTESIAN_POINT('Ctrl Pts',(-19.548834371254,-16.9970918574056,
17.6592440442081));
#168409=CARTESIAN_POINT('Ctrl Pts',(-19.7460347906743,-17.0862293796931,
17.6473504516521));
#168410=CARTESIAN_POINT('Ctrl Pts',(-19.8787811477698,-17.1646021563576,
17.6391831377827));
#168411=CARTESIAN_POINT('Ctrl Pts',(-20.0057612100994,-17.2595650699986,
17.6302909514503));
#168412=CARTESIAN_POINT('Ctrl Pts',(-20.0096389099454,-17.2624858867679,
17.6300183180715));
#168413=CARTESIAN_POINT('Ctrl Pts',(-20.0639398701358,-17.3036807498926,
17.6261849813003));
#168414=CARTESIAN_POINT('Ctrl Pts',(-20.1126276207476,-17.3441812369468,
17.6225577387224));
#168415=CARTESIAN_POINT('Ctrl Pts',(-20.1686735537514,-17.3952221498228,
17.6181060949458));
#168416=CARTESIAN_POINT('Ctrl Pts',(-20.177847238413,-17.4037265672025,
17.617368124686));
#168417=CARTESIAN_POINT('Ctrl Pts',(-20.1927722300276,-17.417810709638,
17.6161517888953));
#168418=CARTESIAN_POINT('Ctrl Pts',(-20.1985682625042,-17.4233427462219,
17.6156754718345));
#168419=CARTESIAN_POINT('Ctrl Pts',(-20.2089226982498,-17.4333385050625,
17.6148173198028));
#168420=CARTESIAN_POINT('Ctrl Pts',(-20.2134926128986,-17.4377902031027,
17.6144360111681));
#168421=CARTESIAN_POINT('Ctrl Pts',(-20.2223064923953,-17.4464540731883,
17.6136955645564));
#168422=CARTESIAN_POINT('Ctrl Pts',(-20.2265528757389,-17.4506637068841,
17.6133365402136));
#168423=CARTESIAN_POINT('Ctrl Pts',(-20.2380573690419,-17.4621656840978,
17.6123575628236));
#168424=CARTESIAN_POINT('Ctrl Pts',(-20.2452801728556,-17.4694929708463,
17.6117360590886));
#168425=CARTESIAN_POINT('Ctrl Pts',(-20.274574021194,-17.4996471239514,
17.6091868388208));
#168426=CARTESIAN_POINT('Ctrl Pts',(-20.2961826748662,-17.5229155693371,
17.607239247281));
#168427=CARTESIAN_POINT('Ctrl Pts',(-20.3503819733628,-17.5839766223115,
17.6021747762768));
#168428=CARTESIAN_POINT('Ctrl Pts',(-20.3821730448234,-17.6224498355758,
17.5990270878846));
#168429=CARTESIAN_POINT('Ctrl Pts',(-20.4577559662583,-17.7208004266969,
17.5910890524617));
#168430=CARTESIAN_POINT('Ctrl Pts',(-20.4998152237406,-17.7819221384846,
17.5862481251173));
#168431=CARTESIAN_POINT('Ctrl Pts',(-20.6124795016572,-17.9656020308039,
17.5720556264622));
#168432=CARTESIAN_POINT('Ctrl Pts',(-20.6741167587004,-18.0931629493534,
17.5626093903388));
#168433=CARTESIAN_POINT('Ctrl Pts',(-20.7225805855593,-18.2258896401121,
17.5536949999931));
#168434=CARTESIAN_POINT('Ctrl Pts',(-20.7225805737356,-18.2258896077308,
17.3329786086887));
#168435=CARTESIAN_POINT('Ctrl Pts',(-20.7104864421468,-18.1927677086508,
17.3349098494595));
#168436=CARTESIAN_POINT('Ctrl Pts',(-20.6975577347975,-18.1599286202259,
17.3368537579916));
#168437=CARTESIAN_POINT('Ctrl Pts',(-20.6624014074273,-18.0767995408689,
17.34187307398));
#168438=CARTESIAN_POINT('Ctrl Pts',(-20.6390395045528,-18.0270504459731,
17.3449716029928));
#168439=CARTESIAN_POINT('Ctrl Pts',(-20.5980248124357,-17.9478723399229,
17.3501020614207));
#168440=CARTESIAN_POINT('Ctrl Pts',(-20.5815450858772,-17.9178637326673,
17.3520948747823));
#168441=CARTESIAN_POINT('Ctrl Pts',(-20.5589189004514,-17.8789311986134,
17.3547506063541));
#168442=CARTESIAN_POINT('Ctrl Pts',(-20.5534207804574,-17.8696351526262,
17.3553901070576));
#168443=CARTESIAN_POINT('Ctrl Pts',(-20.5442958218112,-17.8544729633609,
17.3564421940304));
#168444=CARTESIAN_POINT('Ctrl Pts',(-20.540710980588,-17.8485816797273,
17.3568532425771));
#168445=CARTESIAN_POINT('Ctrl Pts',(-20.533713716258,-17.8372079834685,
17.3576512477811));
#168446=CARTESIAN_POINT('Ctrl Pts',(-20.5303048638004,-17.8317234558095,
17.3580380698636));
#168447=CARTESIAN_POINT('Ctrl Pts',(-20.5223725887378,-17.8190904513582,
17.3589337820094));
#168448=CARTESIAN_POINT('Ctrl Pts',(-20.5178313280707,-17.8119533556468,
17.3594433297405));
#168449=CARTESIAN_POINT('Ctrl Pts',(-20.5054952879657,-17.7928200701284,
17.3608189157874));
#168450=CARTESIAN_POINT('Ctrl Pts',(-20.4976215864081,-17.7808755193036,
17.3616878906464));
#168451=CARTESIAN_POINT('Ctrl Pts',(-20.4088268220344,-17.6490985903593,
17.3713906080218));
#168452=CARTESIAN_POINT('Ctrl Pts',(-20.3159688849382,-17.5378016068516,
17.3806984685398));
#168453=CARTESIAN_POINT('Ctrl Pts',(-20.1259489280883,-17.3523759933019,
17.3981791058077));
#168454=CARTESIAN_POINT('Ctrl Pts',(-20.0322997581734,-17.2754743683484,
17.4062464900393));
#168455=CARTESIAN_POINT('Ctrl Pts',(-19.9076880640577,-17.189882445696,
17.4159558849985));
#168456=CARTESIAN_POINT('Ctrl Pts',(-19.8824175958746,-17.1733097068011,
17.4178758980935));
#168457=CARTESIAN_POINT('Ctrl Pts',(-19.8462044475652,-17.1506542626023,
17.4205498398584));
#168458=CARTESIAN_POINT('Ctrl Pts',(-19.8355503603132,-17.1441194678071,
17.4213272722956));
#168459=CARTESIAN_POINT('Ctrl Pts',(-19.8191315180389,-17.1342478343637,
17.4225105122093));
#168460=CARTESIAN_POINT('Ctrl Pts',(-19.8134080365084,-17.1308433234689,
17.4229202450091));
#168461=CARTESIAN_POINT('Ctrl Pts',(-19.8039353093024,-17.1252689862117,
17.4235937542175));
#168462=CARTESIAN_POINT('Ctrl Pts',(-19.8001953462669,-17.1230835866061,
17.4238584827382));
#168463=CARTESIAN_POINT('Ctrl Pts',(-19.7929546010434,-17.1188823083169,
17.4243686892573));
#168464=CARTESIAN_POINT('Ctrl Pts',(-19.7894547080002,-17.116864942675,
17.4246142607741));
#168465=CARTESIAN_POINT('Ctrl Pts',(-19.7829360499672,-17.1131323545322,
17.4250696789485));
#168466=CARTESIAN_POINT('Ctrl Pts',(-19.7799188699792,-17.11141455723,17.425279687199));
#168467=CARTESIAN_POINT('Ctrl Pts',(-19.7729869984992,-17.1074905236333,
17.4257603926587));
#168468=CARTESIAN_POINT('Ctrl Pts',(-19.7690695086505,-17.1052893284072,
17.4260307642412));
#168469=CARTESIAN_POINT('Ctrl Pts',(-19.7574873619518,-17.0988298787264,
17.426826397402));
#168470=CARTESIAN_POINT('Ctrl Pts',(-19.7498031172166,-17.0946066890604,
17.4273494661493));
#168471=CARTESIAN_POINT('Ctrl Pts',(-19.6942554725164,-17.0645260506725,
17.4310977695132));
#168472=CARTESIAN_POINT('Ctrl Pts',(-19.645433006508,-17.0404719642183,
17.4342175375556));
#168473=CARTESIAN_POINT('Ctrl Pts',(-19.459347146141,-16.9575436709873,
17.4456647095087));
#168474=CARTESIAN_POINT('Ctrl Pts',(-19.3169061446843,-16.9113602014049,
17.4535772797177));
#168475=CARTESIAN_POINT('Ctrl Pts',(-19.0759200610691,-16.8605462661092,
17.4671151405275));
#168476=CARTESIAN_POINT('Ctrl Pts',(-18.9798058060513,-16.8470856630991,
17.4725462891269));
#168477=CARTESIAN_POINT('Ctrl Pts',(-18.8615918994072,-16.8387383429261,
17.4794457055602));
#168478=CARTESIAN_POINT('Ctrl Pts',(-18.8400481220496,-16.8375477614194,
17.4807115638795));
#168479=CARTESIAN_POINT('Ctrl Pts',(-18.8094568186734,-16.8363258744036,
17.4825224785959));
#168480=CARTESIAN_POINT('Ctrl Pts',(-18.8004210491932,-16.8360229260303,
17.4830590294245));
#168481=CARTESIAN_POINT('Ctrl Pts',(-18.7848540245107,-16.835600808806,
17.4839863754321));
#168482=CARTESIAN_POINT('Ctrl Pts',(-18.7783236000857,-16.8354539727905,
17.4843762985894));
#168483=CARTESIAN_POINT('Ctrl Pts',(-18.765835113166,-16.8352309929499,
17.4851237266227));
#168484=CARTESIAN_POINT('Ctrl Pts',(-18.7598771952045,-16.8351497754261,
17.4854810686031));
#168485=CARTESIAN_POINT('Ctrl Pts',(-18.7444196032331,-16.8350043269884,
17.4864101986601));
#168486=CARTESIAN_POINT('Ctrl Pts',(-18.7349197754839,-16.8349788860067,
17.486983196933));
#168487=CARTESIAN_POINT('Ctrl Pts',(-18.7027105527993,-16.8351094246879,
17.4889328328188));
#168488=CARTESIAN_POINT('Ctrl Pts',(-18.6800045690789,-16.8355668761448,
17.4903188547222));
#168489=CARTESIAN_POINT('Ctrl Pts',(-18.4783258766554,-16.842877548468,
17.50273725856));
#168490=CARTESIAN_POINT('Ctrl Pts',(-18.3009195556806,-16.8720521078611,
17.514506601087));
#168491=CARTESIAN_POINT('Ctrl Pts',(-18.0483550700515,-16.947324988999,
17.5319155793778));
#168492=CARTESIAN_POINT('Ctrl Pts',(-17.9688784480643,-16.9762920940486,
17.5374791670365));
#168493=CARTESIAN_POINT('Ctrl Pts',(-17.8572323808124,-17.0247350824564,
17.5452450742251));
#168494=CARTESIAN_POINT('Ctrl Pts',(-17.8235159660938,-17.0404323879336,
17.5475829398941));
#168495=CARTESIAN_POINT('Ctrl Pts',(-17.7834837272261,-17.0603698596369,
17.5503347481257));
#168496=CARTESIAN_POINT('Ctrl Pts',(-17.7767569975213,-17.0637649481949,
17.5507963096006));
#168497=CARTESIAN_POINT('Ctrl Pts',(-17.7663320408895,-17.069096618253,
17.5515101634834));
#168498=CARTESIAN_POINT('Ctrl Pts',(-17.7626212516536,-17.0710083062281,
17.5517639713802));
#168499=CARTESIAN_POINT('Ctrl Pts',(-17.7557522885665,-17.0745727390417,
17.5522332166924));
#168500=CARTESIAN_POINT('Ctrl Pts',(-17.7525926627584,-17.0762224695307,
17.5524488333306));
#168501=CARTESIAN_POINT('Ctrl Pts',(-17.7454618917507,-17.0799685973449,
17.5529349387837));
#168502=CARTESIAN_POINT('Ctrl Pts',(-17.741493251985,-17.0820696483594,
17.5532051290437));
#168503=CARTESIAN_POINT('Ctrl Pts',(-17.7298078531374,-17.0883037368409,
17.5539997343143));
#168504=CARTESIAN_POINT('Ctrl Pts',(-17.7221099010328,-17.0924720860575,
17.5545219649416));
#168505=CARTESIAN_POINT('Ctrl Pts',(-17.6669813545786,-17.1227672505914,
17.5582546395922));
#168506=CARTESIAN_POINT('Ctrl Pts',(-17.6205384994342,-17.1506600016381,
17.5613605901472));
#168507=CARTESIAN_POINT('Ctrl Pts',(-17.435217856908,-17.2718700897137,
17.5738056069297));
#168508=CARTESIAN_POINT('Ctrl Pts',(-17.3065629186422,-17.3797078871075,
17.5826127482353));
#168509=CARTESIAN_POINT('Ctrl Pts',(-17.1508616628789,-17.5452460902517,
17.5952017838381));
#168510=CARTESIAN_POINT('Ctrl Pts',(-17.1116611892639,-17.5906405533614,
17.5985705487878));
#168511=CARTESIAN_POINT('Ctrl Pts',(-17.0518068099685,-17.6662145567908,
17.6041067593827));
#168512=CARTESIAN_POINT('Ctrl Pts',(-17.0299149798136,-17.6953727107602,
17.606226459287));
#168513=CARTESIAN_POINT('Ctrl Pts',(-17.0023843709895,-17.7340844073729,
17.6090269959459));
#168514=CARTESIAN_POINT('Ctrl Pts',(-16.9960516197295,-17.7431383462476,
17.6096810293439));
#168515=CARTESIAN_POINT('Ctrl Pts',(-16.9858508129245,-17.7579682851499,
17.6107509427807));
#168516=CARTESIAN_POINT('Ctrl Pts',(-16.9819397704358,-17.7637145685701,
17.6111651815024));
#168517=CARTESIAN_POINT('Ctrl Pts',(-16.9744614332803,-17.7748192706471,
17.6119651152198));
#168518=CARTESIAN_POINT('Ctrl Pts',(-16.9708901353176,-17.7801749102472,
17.6123506529619));
#168519=CARTESIAN_POINT('Ctrl Pts',(-16.9627530154023,-17.7924990188325,
17.6132372819855));
#168520=CARTESIAN_POINT('Ctrl Pts',(-16.9582038125271,-17.7994782851359,
17.6137389890164));
#168521=CARTESIAN_POINT('Ctrl Pts',(-16.9461933422388,-17.8181443634005,
17.6150798397191));
#168522=CARTESIAN_POINT('Ctrl Pts',(-16.9388055900956,-17.8298777845196,
17.6159216937581));
#168523=CARTESIAN_POINT('Ctrl Pts',(-16.8813286698825,-17.9231846341802,
17.62260948816));
#168524=CARTESIAN_POINT('Ctrl Pts',(-16.8367161307349,-18.0079864276178,
17.6286545164905));
#168525=CARTESIAN_POINT('Ctrl Pts',(-16.7419254054438,-18.2222494063162,
17.6438220640093));
#168526=CARTESIAN_POINT('Ctrl Pts',(-16.6984367933057,-18.354191151171,
17.6530889356279));
#168527=CARTESIAN_POINT('Ctrl Pts',(-16.6568246718478,-18.5400277691299,
17.6655380253888));
#168528=CARTESIAN_POINT('Ctrl Pts',(-16.6473555017964,-18.5910375014303,
17.6688914276431));
#168529=CARTESIAN_POINT('Ctrl Pts',(-16.6357771673603,-18.6693434832353,
17.673895446549));
#168530=CARTESIAN_POINT('Ctrl Pts',(-16.6323075896126,-18.6964164758954,
17.6755994724613));
#168531=CARTESIAN_POINT('Ctrl Pts',(-16.6286234454546,-18.7303573949368,
17.6776970526797));
#168532=CARTESIAN_POINT('Ctrl Pts',(-16.6279175931669,-18.7371680205407,
17.6781160103822));
#168533=CARTESIAN_POINT('Ctrl Pts',(-16.6268494987093,-18.7479854218743,
17.6787782305216));
#168534=CARTESIAN_POINT('Ctrl Pts',(-16.6264656204226,-18.7519899435012,
17.6790226806623));
#168535=CARTESIAN_POINT('Ctrl Pts',(-16.6257609426452,-18.7595683188277,
17.6794839382517));
#168536=CARTESIAN_POINT('Ctrl Pts',(-16.6254378183752,-18.7631418488362,
17.6797008682422));
#168537=CARTESIAN_POINT('Ctrl Pts',(-16.6247171124215,-18.7713448333614,
17.680197536256));
#168538=CARTESIAN_POINT('Ctrl Pts',(-16.6243256855282,-18.7759747834404,
17.6804769261422));
#168539=CARTESIAN_POINT('Ctrl Pts',(-16.623321711021,-18.7883348272222,
17.681220359968));
#168540=CARTESIAN_POINT('Ctrl Pts',(-16.6227363791084,-18.7960671438983,
17.6816829187391));
#168541=CARTESIAN_POINT('Ctrl Pts',(-16.6188025926289,-18.8521234424839,
17.6850191174309));
#168542=CARTESIAN_POINT('Ctrl Pts',(-16.6170708242361,-18.9005505293486,
17.6878089138649));
#168543=CARTESIAN_POINT('Ctrl Pts',(-16.6169630320092,-18.9765706720492,
17.692102262049));
#168544=CARTESIAN_POINT('Ctrl Pts',(-16.6174626075037,-19.0041421183956,
17.6936416334007));
#168545=CARTESIAN_POINT('Ctrl Pts',(-16.6201528146951,-19.0755519656355,
17.6975997228564));
#168546=CARTESIAN_POINT('Ctrl Pts',(-16.6231683181137,-19.1193464267854,
17.6999990458829));
#168547=CARTESIAN_POINT('Ctrl Pts',(-16.6384409340647,-19.2718041924397,
17.7083409402699));
#168548=CARTESIAN_POINT('Ctrl Pts',(-16.6577499340344,-19.3795830892136,
17.7142281680917));
#168549=CARTESIAN_POINT('Ctrl Pts',(-16.7043608332299,-19.5586134350395,
17.724514928789));
#168550=CARTESIAN_POINT('Ctrl Pts',(-16.727336922796,-19.6307610478067,
17.7288045190204));
#168551=CARTESIAN_POINT('Ctrl Pts',(-16.7608127270424,-19.7191883226073,
17.7343248003963));
#168552=CARTESIAN_POINT('Ctrl Pts',(-16.7677377274275,-19.7367665753161,
17.7354353641098));
#168553=CARTESIAN_POINT('Ctrl Pts',(-16.7781445529553,-19.7621801743971,
17.7370611884304));
#168554=CARTESIAN_POINT('Ctrl Pts',(-16.7814402907764,-19.7700910849917,
17.7375701641849));
#168555=CARTESIAN_POINT('Ctrl Pts',(-16.787301175385,-19.7839220581577,
17.7384651761504));
#168556=CARTESIAN_POINT('Ctrl Pts',(-16.7898455360463,-19.7898508479875,
17.7388505012132));
#168557=CARTESIAN_POINT('Ctrl Pts',(-16.7948374900136,-19.8013377671802,
17.7396003458106));
#168558=CARTESIAN_POINT('Ctrl Pts',(-16.7972819800069,-19.8068971825513,
17.739964756213));
#168559=CARTESIAN_POINT('Ctrl Pts',(-16.8031808943796,-19.8201577168425,
17.7408375942988));
#168560=CARTESIAN_POINT('Ctrl Pts',(-16.8066574997269,-19.827848801652,
17.7413467803318));
#168561=CARTESIAN_POINT('Ctrl Pts',(-16.8193569630616,-19.8555012770227,
17.7431882643749));
#168562=CARTESIAN_POINT('Ctrl Pts',(-16.8288444500643,-19.8753389354907,
17.7445296614726));
#168563=CARTESIAN_POINT('Ctrl Pts',(-16.9218510373929,-20.0622704909225,
17.7573683548412));
#168564=CARTESIAN_POINT('Ctrl Pts',(-17.0268192268646,-20.2177369755839,
17.7696769687365));
#168565=CARTESIAN_POINT('Ctrl Pts',(-17.2034616585513,-20.4167317208172,
17.787242321993));
#168566=CARTESIAN_POINT('Ctrl Pts',(-17.2594428099543,-20.4730750846991,
17.7924544141475));
#168567=CARTESIAN_POINT('Ctrl Pts',(-17.3450908809074,-20.550093631775,
17.7997956008994));
#168568=CARTESIAN_POINT('Ctrl Pts',(-17.3723281792737,-20.5733642409973,
17.8020455053046));
#168569=CARTESIAN_POINT('Ctrl Pts',(-17.4059324225588,-20.6006300558802,
17.80470776851));
#168570=CARTESIAN_POINT('Ctrl Pts',(-17.4117450485827,-20.6052956174419,
17.8051642799506));
#168571=CARTESIAN_POINT('Ctrl Pts',(-17.4208374346113,-20.6125150866815,
17.8058720277955));
#168572=CARTESIAN_POINT('Ctrl Pts',(-17.4241002143388,-20.6150901444136,
17.8061247390986));
#168573=CARTESIAN_POINT('Ctrl Pts',(-17.4301764252852,-20.6198566495197,
17.8065929846737));
#168574=CARTESIAN_POINT('Ctrl Pts',(-17.4329877827856,-20.622050576558,
17.8068086916849));
#168575=CARTESIAN_POINT('Ctrl Pts',(-17.439370564266,-20.6270056723382,
17.8072963065327));
#168576=CARTESIAN_POINT('Ctrl Pts',(-17.4429452751425,-20.6297625208964,
17.807567907784));
#168577=CARTESIAN_POINT('Ctrl Pts',(-17.4535658423472,-20.6378991526213,
17.8083705281124));
#168578=CARTESIAN_POINT('Ctrl Pts',(-17.4606368025301,-20.6432462146099,
17.8088992965071));
#168579=CARTESIAN_POINT('Ctrl Pts',(-17.5135264577695,-20.6827216407256,
17.8128146302074));
#168580=CARTESIAN_POINT('Ctrl Pts',(-17.5606806517185,-20.7150303454308,
17.8160847411955));
#168581=CARTESIAN_POINT('Ctrl Pts',(-17.737338437242,-20.8258394240807,
17.8277763709364));
#168582=CARTESIAN_POINT('Ctrl Pts',(-17.8738528201643,-20.8922991633028,
17.8357920470868));
#168583=CARTESIAN_POINT('Ctrl Pts',(-18.1035142146527,-20.9750599276034,
17.8492378292061));
#168584=CARTESIAN_POINT('Ctrl Pts',(-18.1926930861591,-21.0007234428418,
17.8544436549559));
#168585=CARTESIAN_POINT('Ctrl Pts',(-18.3038460930482,-21.024944888954,
17.8610701804794));
#168586=CARTESIAN_POINT('Ctrl Pts',(-18.3244970938798,-21.0291230630333,
17.8623067194479));
#168587=CARTESIAN_POINT('Ctrl Pts',(-18.3540091854133,-21.0346368318015,
17.864082843278));
#168588=CARTESIAN_POINT('Ctrl Pts',(-18.362822130045,-21.0362255581988,
17.8646143673312));
#168589=CARTESIAN_POINT('Ctrl Pts',(-18.378065138894,-21.0388736999805,
17.8655357617358));
#168590=CARTESIAN_POINT('Ctrl Pts',(-18.3844905499111,-21.0399594363529,
17.8659247898351));
#168591=CARTESIAN_POINT('Ctrl Pts',(-18.3968182174948,-21.0419840102106,
17.8666724199752));
#168592=CARTESIAN_POINT('Ctrl Pts',(-18.4027196456649,-21.0429275556754,
17.8670308683749));
#168593=CARTESIAN_POINT('Ctrl Pts',(-18.4181095434045,-21.045321368904,
17.8679671022208));
#168594=CARTESIAN_POINT('Ctrl Pts',(-18.4276039423149,-21.0467321034362,
17.868546134905));
#168595=CARTESIAN_POINT('Ctrl Pts',(-18.4601864383012,-21.0513471503003,
17.8705383707068));
#168596=CARTESIAN_POINT('Ctrl Pts',(-18.4833170432897,-21.0542345994454,
17.8719615236971));
#168597=CARTESIAN_POINT('Ctrl Pts',(-18.6762847338172,-21.0750932844534,
17.8839119363672));
#168598=CARTESIAN_POINT('Ctrl Pts',(-18.8476462699626,-21.0728297901392,
17.8951010561562));
#168599=CARTESIAN_POINT('Ctrl Pts',(-19.1063774921774,-21.0379499887562,
17.9123531737725));
#168600=CARTESIAN_POINT('Ctrl Pts',(-19.1950597619262,-21.020158176893,
17.9183162470272));
#168601=CARTESIAN_POINT('Ctrl Pts',(-19.3196745965612,-20.9867404052281,
17.9265592915962));
#168602=CARTESIAN_POINT('Ctrl Pts',(-19.356732494316,-20.9757064821372,
17.9289921683682));
#168603=CARTESIAN_POINT('Ctrl Pts',(-19.4007095278454,-20.9612897872786,
17.9318403065271));
#168604=CARTESIAN_POINT('Ctrl Pts',(-19.4079363517236,-20.9588773858057,
17.9323070669527));
#168605=CARTESIAN_POINT('Ctrl Pts',(-19.4191196054225,-20.9550770585963,
17.9330272023617));
#168606=CARTESIAN_POINT('Ctrl Pts',(-19.4230851151679,-20.9537163338412,
17.933282135111));
#168607=CARTESIAN_POINT('Ctrl Pts',(-19.4304131744878,-20.9511774270268,
17.9337524204992));
#168608=CARTESIAN_POINT('Ctrl Pts',(-19.4337767641568,-20.9500025462919,
17.9339679589769));
#168609=CARTESIAN_POINT('Ctrl Pts',(-19.4413507606262,-20.9473355243079,
17.9344525822863));
#168610=CARTESIAN_POINT('Ctrl Pts',(-19.4455594078557,-20.9458385498973,
17.9347213765235));
#168611=CARTESIAN_POINT('Ctrl Pts',(-19.4578988445171,-20.9414054870869,
17.935508088406));
#168612=CARTESIAN_POINT('Ctrl Pts',(-19.466016537838,-20.9384328640199,
17.9360238860025));
#168613=CARTESIAN_POINT('Ctrl Pts',(-19.5224626353362,-20.9173698232454,
17.9395997175728));
#168614=CARTESIAN_POINT('Ctrl Pts',(-19.5701378628187,-20.8975657983281,
17.9425649535421));
#168615=CARTESIAN_POINT('Ctrl Pts',(-19.636926399806,-20.8669129019215,
17.9467037880634));
#168616=CARTESIAN_POINT('Ctrl Pts',(-19.6566651687567,-20.8574806578857,
17.9479250191211));
#168617=CARTESIAN_POINT('Ctrl Pts',(-19.7995540558099,-20.7864596119881,
17.9567751987166));
#168618=CARTESIAN_POINT('Ctrl Pts',(-19.9165827754788,-20.7132916122363,
17.9640985794818));
#168619=CARTESIAN_POINT('Ctrl Pts',(-20.0975672646288,-20.5739142383143,
17.9766928253087));
#168620=CARTESIAN_POINT('Ctrl Pts',(-20.1658130976267,-20.5139955191033,
17.9817933316599));
#168621=CARTESIAN_POINT('Ctrl Pts',(-20.244737861738,-20.4351702285474,
17.988292440638));
#168622=CARTESIAN_POINT('Ctrl Pts',(-20.2592564828365,-20.4202354816829,
17.9895150620323));
#168623=CARTESIAN_POINT('Ctrl Pts',(-20.2796703515502,-20.3986069334358,
17.9912746466735));
#168624=CARTESIAN_POINT('Ctrl Pts',(-20.2857476144952,-20.3920860365729,
17.9918037560683));
#168625=CARTESIAN_POINT('Ctrl Pts',(-20.29619112644,-20.3807372934515,17.9927222995741));
#168626=CARTESIAN_POINT('Ctrl Pts',(-20.3005766563314,-20.3759272971626,
17.9931109056582));
#168627=CARTESIAN_POINT('Ctrl Pts',(-20.3089521347045,-20.3666556467147,
17.9938586666956));
#168628=CARTESIAN_POINT('Ctrl Pts',(-20.3129454863746,-20.362197140582,
17.9942176725303));
#168629=CARTESIAN_POINT('Ctrl Pts',(-20.3233262549738,-20.3505078257506,
17.9951574588914));
#168630=CARTESIAN_POINT('Ctrl Pts',(-20.3296831900043,-20.3432502419594,
17.9957395052875));
#168631=CARTESIAN_POINT('Ctrl Pts',(-20.3514218849837,-20.3180866248662,
17.9977528279286));
#168632=CARTESIAN_POINT('Ctrl Pts',(-20.3665531929145,-20.2999674410712,
17.9991943389182));
#168633=CARTESIAN_POINT('Ctrl Pts',(-20.4850680329415,-20.1531271970523,
18.0108161680665));
#168634=CARTESIAN_POINT('Ctrl Pts',(-20.5733552535207,-20.0129893381239,
18.0216100156468));
#168635=CARTESIAN_POINT('Ctrl Pts',(-20.6994386073971,-19.7488857161959,
18.0409499403857));
#168636=CARTESIAN_POINT('Ctrl Pts',(-20.743899330609,-19.6289691343491,
18.049391053653));
#168637=CARTESIAN_POINT('Ctrl Pts',(-20.7804090241341,-19.4942558051151,
18.0580465438403));
#168638=CARTESIAN_POINT('Ctrl Pts',(-20.7834316356884,-19.4827176630822,
18.0587813177728));
#168639=CARTESIAN_POINT('Ctrl Pts',(-20.7875891298045,-19.4662819698134,
18.0598180620874));
#168640=CARTESIAN_POINT('Ctrl Pts',(-20.7888042692852,-19.4614052165508,
18.0601244459327));
#168641=CARTESIAN_POINT('Ctrl Pts',(-20.7908681042927,-19.4529948179474,
18.0606506488588));
#168642=CARTESIAN_POINT('Ctrl Pts',(-20.7917250853263,-19.4494632449383,
18.0608709418033));
#168643=CARTESIAN_POINT('Ctrl Pts',(-20.7933688051065,-19.4426126363481,
18.0612969665191));
#168644=CARTESIAN_POINT('Ctrl Pts',(-20.7941566162479,-19.4392939064884,
18.0615027621465));
#168645=CARTESIAN_POINT('Ctrl Pts',(-20.7962599600606,-19.4303370937807,
18.0620566247985));
#168646=CARTESIAN_POINT('Ctrl Pts',(-20.797560402491,-19.4246954465815,
18.0624038302745));
#168647=CARTESIAN_POINT('Ctrl Pts',(-20.8022980768276,-19.4037500213828,
18.063686978631));
#168648=CARTESIAN_POINT('Ctrl Pts',(-20.8055884395178,-19.3884130912177,
18.0646148752806));
#168649=CARTESIAN_POINT('Ctrl Pts',(-20.8354454595723,-19.2412904230449,
18.073416790184));
#168650=CARTESIAN_POINT('Ctrl Pts',(-20.8495760219943,-19.1072739809901,
18.0806879222332));
#168651=CARTESIAN_POINT('Ctrl Pts',(-20.850959537806,-18.9665205892282,
18.0883318492396));
#168652=CARTESIAN_POINT('Ctrl Pts',(-20.8509933270725,-18.9602331844887,
18.0886732825532));
#168653=CARTESIAN_POINT('Ctrl Pts',(-20.851133145328,-18.8081072307474,
18.0969355113093));
#168654=CARTESIAN_POINT('Ctrl Pts',(-20.8361978945779,-18.6626640240751,
18.1048962272042));
#168655=CARTESIAN_POINT('Ctrl Pts',(-20.8015323046563,-18.4963942884213,
18.1147554858428));
#168656=CARTESIAN_POINT('Ctrl Pts',(-20.796227954925,-18.4729570083998,
18.1161622683207));
#168657=CARTESIAN_POINT('Ctrl Pts',(-20.7882195557437,-18.4401743690809,
18.1181559976384));
#168658=CARTESIAN_POINT('Ctrl Pts',(-20.7858481758035,-18.4307490831353,
18.1187322497221));
#168659=CARTESIAN_POINT('Ctrl Pts',(-20.7819083814232,-18.4155335577363,
18.1196675576472));
#168660=CARTESIAN_POINT('Ctrl Pts',(-20.7803800925137,-18.4097330010024,
18.1200253122374));
#168661=CARTESIAN_POINT('Ctrl Pts',(-20.7771446746428,-18.3976615870928,
18.1207723451549));
#168662=CARTESIAN_POINT('Ctrl Pts',(-20.7754332824839,-18.391391946855,
18.1211617585408));
#168663=CARTESIAN_POINT('Ctrl Pts',(-20.7713216385888,-18.376597555618,
18.1220840563322));
#168664=CARTESIAN_POINT('Ctrl Pts',(-20.76889672323,-18.3680798392536,18.1226177386939));
#168665=CARTESIAN_POINT('Ctrl Pts',(-20.7606830652877,-18.3399013089528,
18.1243923132876));
#168666=CARTESIAN_POINT('Ctrl Pts',(-20.7546623986689,-18.3203098236069,
18.1256407462757));
#168667=CARTESIAN_POINT('Ctrl Pts',(-20.7402319475941,-18.2756714355429,
18.128519755806));
#168668=CARTESIAN_POINT('Ctrl Pts',(-20.7316376116202,-18.2506938917112,
18.1301558996124));
#168669=CARTESIAN_POINT('Ctrl Pts',(-20.7225805578636,-18.2258895642624,
18.13180632455));
#168670=CARTESIAN_POINT('Origin',(-18.734,-18.952,0.));
#168671=CARTESIAN_POINT('',(-20.7202230294519,-18.2267290932703,19.1554367770419));
#168672=CARTESIAN_POINT('',(-20.7225805608153,-18.2258895723463,18.9348455085272));
#168673=CARTESIAN_POINT('',(-20.7225805737622,-18.2258896078036,0.));
#168674=CARTESIAN_POINT('',(-20.8499619975019,-18.9538841873159,19.1109437209775));
#168675=CARTESIAN_POINT('Ctrl Pts',(-20.8499619975019,-18.9538841873159,
19.1109437209775));
#168676=CARTESIAN_POINT('Ctrl Pts',(-20.8478498472042,-18.7070537041303,
19.1257747396657));
#168677=CARTESIAN_POINT('Ctrl Pts',(-20.8034779751874,-18.4595580078992,
19.1406057583538));
#168678=CARTESIAN_POINT('Ctrl Pts',(-20.7202230294519,-18.2267290932703,
19.1554367770419));
#168679=CARTESIAN_POINT('Ctrl Pts',(-20.850999125527,-18.9539241928138,
19.1115402607454));
#168680=CARTESIAN_POINT('Ctrl Pts',(-20.8508551448554,-19.1123318916676,
19.1011622677739));
#168681=CARTESIAN_POINT('Ctrl Pts',(-20.8329326848977,-19.2702284518518,
19.0905102687625));
#168682=CARTESIAN_POINT('Ctrl Pts',(-20.7912029051883,-19.4524161307638,
19.0786804206076));
#168683=CARTESIAN_POINT('Ctrl Pts',(-20.7842844059529,-19.4800474757292,
19.0769005643253));
#168684=CARTESIAN_POINT('Ctrl Pts',(-20.7749880166316,-19.5142322698684,
19.074723505109));
#168685=CARTESIAN_POINT('Ctrl Pts',(-20.773133013378,-19.5209233394338,
19.0742985832489));
#168686=CARTESIAN_POINT('Ctrl Pts',(-20.7701454845392,-19.5314971281306,
19.0736291200915));
#168687=CARTESIAN_POINT('Ctrl Pts',(-20.7690347136989,-19.5353858674967,
19.0733833471956));
#168688=CARTESIAN_POINT('Ctrl Pts',(-20.766918738645,-19.5427141802028,
19.0729210452307));
#168689=CARTESIAN_POINT('Ctrl Pts',(-20.7659159576265,-19.5461543418567,
19.0727043853938));
#168690=CARTESIAN_POINT('Ctrl Pts',(-20.7636032678753,-19.5540139713706,
19.0722101932646));
#168691=CARTESIAN_POINT('Ctrl Pts',(-20.762287658381,-19.5584317129533,
19.0719329969515));
#168692=CARTESIAN_POINT('Ctrl Pts',(-20.758756505162,-19.5701490813827,
19.0711992300556));
#168693=CARTESIAN_POINT('Ctrl Pts',(-20.7565158944124,-19.5774411665578,
19.0707440842364));
#168694=CARTESIAN_POINT('Ctrl Pts',(-20.7405464091695,-19.628430657502,
19.0675709948821));
#168695=CARTESIAN_POINT('Ctrl Pts',(-20.7254408808252,-19.6716880002887,
19.0649279501887));
#168696=CARTESIAN_POINT('Ctrl Pts',(-20.6584791004688,-19.845142128339,
19.0544019844984));
#168697=CARTESIAN_POINT('Ctrl Pts',(-20.5951589428895,-19.9705363655188,
19.0469412897193));
#168698=CARTESIAN_POINT('Ctrl Pts',(-20.4745384933959,-20.1600369636971,
19.0346705631078));
#168699=CARTESIAN_POINT('Ctrl Pts',(-20.424946872753,-20.2285283032494,
19.0300002618005));
#168700=CARTESIAN_POINT('Ctrl Pts',(-20.3421887490743,-20.3295128457888,
19.0225609493452));
#168701=CARTESIAN_POINT('Ctrl Pts',(-20.3118242167303,-20.3641908420019,
19.0198954814367));
#168702=CARTESIAN_POINT('Ctrl Pts',(-20.2723344322215,-20.4064256773093,
19.0164915252927));
#168703=CARTESIAN_POINT('Ctrl Pts',(-20.2642438498836,-20.4149356198052,
19.0157972779396));
#168704=CARTESIAN_POINT('Ctrl Pts',(-20.2510482847131,-20.4285859189328,
19.0146697880743));
#168705=CARTESIAN_POINT('Ctrl Pts',(-20.2459869069728,-20.4337682225244,
19.0142384441464));
#168706=CARTESIAN_POINT('Ctrl Pts',(-20.2364228594554,-20.4434607492014,
19.0134254157127));
#168707=CARTESIAN_POINT('Ctrl Pts',(-20.2319262169406,-20.4479768254385,
19.0130439990868));
#168708=CARTESIAN_POINT('Ctrl Pts',(-20.2217842508737,-20.4580710500403,
19.0121855629858));
#168709=CARTESIAN_POINT('Ctrl Pts',(-20.2161278360035,-20.4636378732966,
19.0117080518042));
#168710=CARTESIAN_POINT('Ctrl Pts',(-20.2016527358749,-20.4777243522739,
19.0104891790842));
#168711=CARTESIAN_POINT('Ctrl Pts',(-20.1927911767316,-20.4861993498263,
19.0097458901678));
#168712=CARTESIAN_POINT('Ctrl Pts',(-20.1404571056509,-20.5353871238404,
19.0053724901324));
#168713=CARTESIAN_POINT('Ctrl Pts',(-20.0953593372162,-20.5743242650997,
19.0016676799959));
#168714=CARTESIAN_POINT('Ctrl Pts',(-20.0316930886739,-20.6247676297405,
18.9965181924037));
#168715=CARTESIAN_POINT('Ctrl Pts',(-20.014497268834,-20.6379672574055,
18.9951350650169));
#168716=CARTESIAN_POINT('Ctrl Pts',(-19.8794468682004,-20.7383748396772,
18.9843343767586));
#168717=CARTESIAN_POINT('Ctrl Pts',(-19.7530285424352,-20.81338584319,18.9745457590368));
#168718=CARTESIAN_POINT('Ctrl Pts',(-19.5428056802728,-20.9102458051805,
18.9593613002898));
#168719=CARTESIAN_POINT('Ctrl Pts',(-19.4636409328154,-20.9411004824349,
18.9538735221868));
#168720=CARTESIAN_POINT('Ctrl Pts',(-19.3742264924981,-20.9698901633591,
18.948076651573));
#168721=CARTESIAN_POINT('Ctrl Pts',(-19.3656062682177,-20.9726049098492,
18.9475218466409));
#168722=CARTESIAN_POINT('Ctrl Pts',(-19.3526781252441,-20.9765855210615,
18.9466961190504));
#168723=CARTESIAN_POINT('Ctrl Pts',(-19.3483832638059,-20.9778929786051,
18.9464228468279));
#168724=CARTESIAN_POINT('Ctrl Pts',(-19.3406711202252,-20.9802139572299,
18.9459340512265));
#168725=CARTESIAN_POINT('Ctrl Pts',(-19.3372554230306,-20.9812325149156,
18.9457182375612));
#168726=CARTESIAN_POINT('Ctrl Pts',(-19.3298331875,-20.983425421542,18.9452507443392));
#168727=CARTESIAN_POINT('Ctrl Pts',(-19.3258257556537,-20.98459654291,18.9449992540703));
#168728=CARTESIAN_POINT('Ctrl Pts',(-19.3147670694102,-20.9877928263123,
18.9443077227867));
#168729=CARTESIAN_POINT('Ctrl Pts',(-19.307708634938,-20.9897932246301,
18.9438690992699));
#168730=CARTESIAN_POINT('Ctrl Pts',(-19.2715731226257,-20.999831587648,
18.9416369955832));
#168731=CARTESIAN_POINT('Ctrl Pts',(-19.2423354437312,-21.0072844962874,
18.9398752897849));
#168732=CARTESIAN_POINT('Ctrl Pts',(-19.2027335650158,-21.0164824490094,
18.9375362327433));
#168733=CARTESIAN_POINT('Ctrl Pts',(-19.192502676619,-21.0187787109349,
18.9369361567872));
#168734=CARTESIAN_POINT('Ctrl Pts',(-19.1705246523172,-21.0235403175917,
18.9356552658465));
#168735=CARTESIAN_POINT('Ctrl Pts',(-19.1587727230442,-21.0259819678006,
18.9349753548543));
#168736=CARTESIAN_POINT('Ctrl Pts',(-19.1234977608104,-21.0329984927052,
18.9329477864644));
#168737=CARTESIAN_POINT('Ctrl Pts',(-19.0999167355877,-21.0372741391224,
18.9316099902256));
#168738=CARTESIAN_POINT('Ctrl Pts',(-18.9283590008404,-21.0653806393162,
18.9219730308797));
#168739=CARTESIAN_POINT('Ctrl Pts',(-18.7782941981129,-21.0738374330462,
18.9140271191554));
#168740=CARTESIAN_POINT('Ctrl Pts',(-18.5704646403503,-21.0634762923353,
18.9024847385498));
#168741=CARTESIAN_POINT('Ctrl Pts',(-18.5124872451802,-21.0581831131055,
18.8992105558202));
#168742=CARTESIAN_POINT('Ctrl Pts',(-18.419428987557,-21.0458021992431,
18.8938159508115));
#168743=CARTESIAN_POINT('Ctrl Pts',(-18.3841799002073,-21.040202157071,
18.8917401443556));
#168744=CARTESIAN_POINT('Ctrl Pts',(-18.3383089138505,-21.0317206023909,
18.8889896322473));
#168745=CARTESIAN_POINT('Ctrl Pts',(-18.3275430028109,-21.0296433578121,
18.8883405318056));
#168746=CARTESIAN_POINT('Ctrl Pts',(-18.3099974312121,-21.0261164093798,
18.8872766718811));
#168747=CARTESIAN_POINT('Ctrl Pts',(-18.3032078124744,-21.0247168517207,
18.8868635182677));
#168748=CARTESIAN_POINT('Ctrl Pts',(-18.2901206645844,-21.0219520905929,
18.8860642642592));
#168749=CARTESIAN_POINT('Ctrl Pts',(-18.2838222460605,-21.0205914314318,
18.8856783135041));
#168750=CARTESIAN_POINT('Ctrl Pts',(-18.2693539428215,-21.0173966089358,
18.8847887083027));
#168751=CARTESIAN_POINT('Ctrl Pts',(-18.2611885711994,-21.0155426965062,
18.8842844243636));
#168752=CARTESIAN_POINT('Ctrl Pts',(-18.2393911307814,-21.0104575144856,
18.8829321912848));
#168753=CARTESIAN_POINT('Ctrl Pts',(-18.2257799554528,-21.0071393247082,
18.8820814586356));
#168754=CARTESIAN_POINT('Ctrl Pts',(-18.1136118692846,-20.978612072223,
18.8750170282548));
#168755=CARTESIAN_POINT('Ctrl Pts',(-18.0169708302706,-20.9464678091623,
18.8685773986194));
#168756=CARTESIAN_POINT('Ctrl Pts',(-17.8305334408218,-20.8691497678742,
18.8554747869802));
#168757=CARTESIAN_POINT('Ctrl Pts',(-17.7408830926317,-20.8242798951722,
18.8488338622719));
#168758=CARTESIAN_POINT('Ctrl Pts',(-17.589756719946,-20.7347236982332,
18.8372454021194));
#168759=CARTESIAN_POINT('Ctrl Pts',(-17.5268671467347,-20.692755096443,
18.8322926809812));
#168760=CARTESIAN_POINT('Ctrl Pts',(-17.438510254664,-20.6266951421875,
18.825268033006));
#168761=CARTESIAN_POINT('Ctrl Pts',(-17.4111831235301,-20.6051948871866,
18.8230858169131));
#168762=CARTESIAN_POINT('Ctrl Pts',(-17.3787042536051,-20.5783200856179,
18.8204927089629));
#168763=CARTESIAN_POINT('Ctrl Pts',(-17.3730368862902,-20.5735803982237,
18.8200402488417));
#168764=CARTESIAN_POINT('Ctrl Pts',(-17.3642308490207,-20.5661371164649,
18.819337402556));
#168765=CARTESIAN_POINT('Ctrl Pts',(-17.3610751693034,-20.5634538676797,
18.8190855737166));
#168766=CARTESIAN_POINT('Ctrl Pts',(-17.3552161736274,-20.5584423078902,
18.8186181219436));
#168767=CARTESIAN_POINT('Ctrl Pts',(-17.3525108949523,-20.5561164488094,
18.8184023315147));
#168768=CARTESIAN_POINT('Ctrl Pts',(-17.3463808826382,-20.550819171255,
18.817913453326));
#168769=CARTESIAN_POINT('Ctrl Pts',(-17.3429598154517,-20.5478435897952,
18.8176406788191));
#168770=CARTESIAN_POINT('Ctrl Pts',(-17.3341210604825,-20.5401057848045,
18.8169360099627));
#168771=CARTESIAN_POINT('Ctrl Pts',(-17.3287180535502,-20.5353267771954,
18.8165053323724));
#168772=CARTESIAN_POINT('Ctrl Pts',(-17.2950320836536,-20.5052229696398,
18.8138198992678));
#168773=CARTESIAN_POINT('Ctrl Pts',(-17.2674082788896,-20.4791671100277,
18.8116163808876));
#168774=CARTESIAN_POINT('Ctrl Pts',(-17.2308562317907,-20.4427826482404,
18.8086742361685));
#168775=CARTESIAN_POINT('Ctrl Pts',(-17.2213066264068,-20.4330917809823,
18.8079030088112));
#168776=CARTESIAN_POINT('Ctrl Pts',(-17.2112952552922,-20.422734476272,
18.807090887949));
#168777=CARTESIAN_POINT('Ctrl Pts',(-17.2107399080521,-20.4221592878094,
18.807045826408));
#168778=CARTESIAN_POINT('Ctrl Pts',(-17.1944161843139,-20.4052331777018,
18.8057209460512));
#168779=CARTESIAN_POINT('Ctrl Pts',(-17.1789112679958,-20.3886294167988,
18.8044527961303));
#168780=CARTESIAN_POINT('Ctrl Pts',(-17.1329880829459,-20.3378368123648,
18.8006557411102));
#168781=CARTESIAN_POINT('Ctrl Pts',(-17.1034075887493,-20.3029076412833,
18.7981536164331));
#168782=CARTESIAN_POINT('Ctrl Pts',(-17.0070546926899,-20.1813520597451,
18.7897086840485));
#168783=CARTESIAN_POINT('Ctrl Pts',(-16.9458702353789,-20.0905243267209,
18.783820547421));
#168784=CARTESIAN_POINT('Ctrl Pts',(-16.8648158224065,-19.9474279256523,
18.7746761031606));
#168785=CARTESIAN_POINT('Ctrl Pts',(-16.8395383235755,-19.8984357115446,
18.7715685248052));
#168786=CARTESIAN_POINT('Ctrl Pts',(-16.8016731365264,-19.8174356950758,
18.766424420314));
#168787=CARTESIAN_POINT('Ctrl Pts',(-16.7879025051405,-19.7860086291589,
18.764427283714));
#168788=CARTESIAN_POINT('Ctrl Pts',(-16.770805923096,-19.7442593327396,
18.7617666083343));
#168789=CARTESIAN_POINT('Ctrl Pts',(-16.7667864623853,-19.7342254948354,
18.7611265985202));
#168790=CARTESIAN_POINT('Ctrl Pts',(-16.7603280058484,-19.7177384961508,
18.7600738874625));
#168791=CARTESIAN_POINT('Ctrl Pts',(-16.7578433705078,-19.7113033379144,
18.7596627275281));
#168792=CARTESIAN_POINT('Ctrl Pts',(-16.753094050289,-19.6988214706448,
18.7588646586925));
#168793=CARTESIAN_POINT('Ctrl Pts',(-16.7508254878549,-19.6927763114206,
18.7584778851739));
#168794=CARTESIAN_POINT('Ctrl Pts',(-16.7456503700919,-19.6787917384499,
18.757582507869));
#168795=CARTESIAN_POINT('Ctrl Pts',(-16.7427636652246,-19.6708451416441,
18.7570732479592));
#168796=CARTESIAN_POINT('Ctrl Pts',(-16.7351261853733,-19.6494214459058,
18.7556989424269));
#168797=CARTESIAN_POINT('Ctrl Pts',(-16.7304642018614,-19.6359133643013,
18.7548309687565));
#168798=CARTESIAN_POINT('Ctrl Pts',(-16.6889407429399,-19.5115299004638,
18.7468240931555));
#168799=CARTESIAN_POINT('Ctrl Pts',(-16.6611867852816,-19.3978459886919,
18.7393834481075));
#168800=CARTESIAN_POINT('Ctrl Pts',(-16.617554813345,-19.1217642921793,
18.7211261676592));
#168801=CARTESIAN_POINT('Ctrl Pts',(-16.6107676288211,-18.9586716078051,
18.7101695359371));
#168802=CARTESIAN_POINT('Ctrl Pts',(-16.625116472538,-18.763962999007,18.6977634339929));
#168803=CARTESIAN_POINT('Ctrl Pts',(-16.6282556713315,-18.7315714681105,
18.6957241277608));
#168804=CARTESIAN_POINT('Ctrl Pts',(-16.6330050910102,-18.6920734080976,
18.6932777762389));
#168805=CARTESIAN_POINT('Ctrl Pts',(-16.6339065251174,-18.6848879616618,
18.6928343800313));
#168806=CARTESIAN_POINT('Ctrl Pts',(-16.635377360365,-18.6736317018907,
18.6921425093426));
#168807=CARTESIAN_POINT('Ctrl Pts',(-16.6359217663822,-18.6695577594204,
18.6918926631901));
#168808=CARTESIAN_POINT('Ctrl Pts',(-16.6369614490486,-18.6619464295358,
18.6914269575609));
#168809=CARTESIAN_POINT('Ctrl Pts',(-16.637453807932,-18.6584087489876,
18.6912109424627));
#168810=CARTESIAN_POINT('Ctrl Pts',(-16.6385980423542,-18.6503369122301,
18.6907190560538));
#168811=CARTESIAN_POINT('Ctrl Pts',(-16.6392556808069,-18.6458036238921,
18.6904435137001));
#168812=CARTESIAN_POINT('Ctrl Pts',(-16.6410093635184,-18.6339851099412,
18.6897269298364));
#168813=CARTESIAN_POINT('Ctrl Pts',(-16.6421287422083,-18.6267033367755,
18.6892871742542));
#168814=CARTESIAN_POINT('Ctrl Pts',(-16.6496775325287,-18.5792479470982,
18.6864318726787));
#168815=CARTESIAN_POINT('Ctrl Pts',(-16.6572263447316,-18.5392580568182,
18.6840752747795));
#168816=CARTESIAN_POINT('Ctrl Pts',(-16.7012325912737,-18.3381313288946,
18.6723623766029));
#168817=CARTESIAN_POINT('Ctrl Pts',(-16.755311159214,-18.1814295429752,
18.6636540561542));
#168818=CARTESIAN_POINT('Ctrl Pts',(-16.8688103461087,-17.9460203983827,
18.6492830447601));
#168819=CARTESIAN_POINT('Ctrl Pts',(-16.9163963096844,-17.8623940612575,
18.6438960223989));
#168820=CARTESIAN_POINT('Ctrl Pts',(-16.981361537848,-17.7643937083535,
18.6370500809416));
#168821=CARTESIAN_POINT('Ctrl Pts',(-16.9934998848225,-17.7466744912295,
18.6357899162245));
#168822=CARTESIAN_POINT('Ctrl Pts',(-17.011118166293,-17.7217770018929,
18.6339857522627));
#168823=CARTESIAN_POINT('Ctrl Pts',(-17.0163779179723,-17.7144440144058,
18.6334501712852));
#168824=CARTESIAN_POINT('Ctrl Pts',(-17.0255236048591,-17.7018639930273,
18.6325239752543));
#168825=CARTESIAN_POINT('Ctrl Pts',(-17.0293872533033,-17.696600855899,
18.6321342264623));
#168826=CARTESIAN_POINT('Ctrl Pts',(-17.0368253580583,-17.6865661698451,
18.6313867666064));
#168827=CARTESIAN_POINT('Ctrl Pts',(-17.0403957501144,-17.6817916755942,
18.6310292166688));
#168828=CARTESIAN_POINT('Ctrl Pts',(-17.0497187927543,-17.6694336596269,
18.63009874572));
#168829=CARTESIAN_POINT('Ctrl Pts',(-17.0555024594921,-17.6618738029092,
18.6295246075421));
#168830=CARTESIAN_POINT('Ctrl Pts',(-17.075326604212,-17.6363205327975,
18.6275669241029));
#168831=CARTESIAN_POINT('Ctrl Pts',(-17.0896066152183,-17.6185157569683,
18.6261738888624));
#168832=CARTESIAN_POINT('Ctrl Pts',(-17.2175908351106,-17.4641234547488,
18.6138322323236));
#168833=CARTESIAN_POINT('Ctrl Pts',(-17.347767950318,-17.3421522553987,
18.6021595051791));
#168834=CARTESIAN_POINT('Ctrl Pts',(-17.5608059625954,-17.1877414484718,
18.5847774815365));
#168835=CARTESIAN_POINT('Ctrl Pts',(-17.6329801407193,-17.1418205527485,
18.5791489341356));
#168836=CARTESIAN_POINT('Ctrl Pts',(-17.7404724239291,-17.0822425911255,
18.5713050471948));
#168837=CARTESIAN_POINT('Ctrl Pts',(-17.7736857697627,-17.0649687893629,
18.5689513812888));
#168838=CARTESIAN_POINT('Ctrl Pts',(-17.8141293276727,-17.0452792722294,
18.5661835257967));
#168839=CARTESIAN_POINT('Ctrl Pts',(-17.8209344618584,-17.0420111742423,
18.5657210818046));
#168840=CARTESIAN_POINT('Ctrl Pts',(-17.831532257993,-17.0369912729783,
18.5650061613102));
#168841=CARTESIAN_POINT('Ctrl Pts',(-17.8353127896917,-17.0352142141969,
18.5647521621775));
#168842=CARTESIAN_POINT('Ctrl Pts',(-17.8423286386088,-17.0319416971265,
18.5642827410658));
#168843=CARTESIAN_POINT('Ctrl Pts',(-17.8455624437339,-17.0304432321504,
18.5640671387365));
#168844=CARTESIAN_POINT('Ctrl Pts',(-17.8528754370741,-17.0270769802079,
18.5635812899009));
#168845=CARTESIAN_POINT('Ctrl Pts',(-17.8569567760462,-17.0252139943197,
18.5633113405767));
#168846=CARTESIAN_POINT('Ctrl Pts',(-17.8690017601801,-17.0197620892181,
18.5625181001704));
#168847=CARTESIAN_POINT('Ctrl Pts',(-17.8769818422535,-17.0162094168027,
18.5619969822795));
#168848=CARTESIAN_POINT('Ctrl Pts',(-17.9342274191187,-16.9911475003937,
18.5582886788683));
#168849=CARTESIAN_POINT('Ctrl Pts',(-17.9842788334147,-16.9714702931428,
18.5552044604606));
#168850=CARTESIAN_POINT('Ctrl Pts',(-18.0364923719037,-16.9532067363277,
18.5520946784626));
#168851=CARTESIAN_POINT('Ctrl Pts',(-18.0379559090074,-16.9526966149244,
18.5520075976884));
#168852=CARTESIAN_POINT('Ctrl Pts',(-18.1787996364259,-16.9037783967077,
18.5436355128065));
#168853=CARTESIAN_POINT('Ctrl Pts',(-18.3228650501247,-16.8700699364164,
18.5358120090095));
#168854=CARTESIAN_POINT('Ctrl Pts',(-18.5662389656421,-16.8393956746015,
18.5223331392241));
#168855=CARTESIAN_POINT('Ctrl Pts',(-18.6639242859854,-16.8339048778165,
18.5168604198529));
#168856=CARTESIAN_POINT('Ctrl Pts',(-18.7832992610546,-16.8354631813626,
18.5099106098063));
#168857=CARTESIAN_POINT('Ctrl Pts',(-18.8049596250557,-16.8360786398982,
18.50863940879));
#168858=CARTESIAN_POINT('Ctrl Pts',(-18.8356538421519,-16.8374226157459,
18.5068221617254));
#168859=CARTESIAN_POINT('Ctrl Pts',(-18.8446987867519,-16.8378768265888,
18.5062847035758));
#168860=CARTESIAN_POINT('Ctrl Pts',(-18.8602649170903,-16.8387586800772,
18.5053562810387));
#168861=CARTESIAN_POINT('Ctrl Pts',(-18.8667875975498,-16.8391585109201,
18.5049661940694));
#168862=CARTESIAN_POINT('Ctrl Pts',(-18.8792507408218,-16.8399804241266,
18.5042187928254));
#168863=CARTESIAN_POINT('Ctrl Pts',(-18.8851914873641,-16.8403973859639,
18.5038616430946));
#168864=CARTESIAN_POINT('Ctrl Pts',(-18.9005867810982,-16.8415432333615,
18.5029337550768));
#168865=CARTESIAN_POINT('Ctrl Pts',(-18.9100382548807,-16.842310580268,
18.5023618130409));
#168866=CARTESIAN_POINT('Ctrl Pts',(-18.9420026249255,-16.845121998504,
18.5004196024337));
#168867=CARTESIAN_POINT('Ctrl Pts',(-18.9644872258126,-16.8474630956609,
18.4990400465018));
#168868=CARTESIAN_POINT('Ctrl Pts',(-19.1659646252665,-16.8717083478782,
18.48655401906));
#168869=CARTESIAN_POINT('Ctrl Pts',(-19.3414814959413,-16.916036429476,
18.4746990812069));
#168870=CARTESIAN_POINT('Ctrl Pts',(-19.5870799694235,-17.0126844155213,
18.4572659613174));
#168871=CARTESIAN_POINT('Ctrl Pts',(-19.6630624637443,-17.0479161956431,
18.4517594236141));
#168872=CARTESIAN_POINT('Ctrl Pts',(-19.7693192400267,-17.1050648387745,
18.4440621305226));
#168873=CARTESIAN_POINT('Ctrl Pts',(-19.801412629804,-17.1234251229429,
18.4417382564612));
#168874=CARTESIAN_POINT('Ctrl Pts',(-19.8394398813312,-17.1465227084929,
18.4390006679966));
#168875=CARTESIAN_POINT('Ctrl Pts',(-19.8458481765314,-17.1504619855159,
18.4385398941677));
#168876=CARTESIAN_POINT('Ctrl Pts',(-19.8557774679868,-17.156638834849,
18.4378269923529));
#168877=CARTESIAN_POINT('Ctrl Pts',(-19.8593130024129,-17.1588527533109,
18.4375733552395));
#168878=CARTESIAN_POINT('Ctrl Pts',(-19.8658576198338,-17.1629779108889,
18.437104266573));
#168879=CARTESIAN_POINT('Ctrl Pts',(-19.8688683922354,-17.1648862824385,
18.4368886368044));
#168880=CARTESIAN_POINT('Ctrl Pts',(-19.875664115456,-17.1692178360058,
18.4364023005712));
#168881=CARTESIAN_POINT('Ctrl Pts',(-19.8794461686522,-17.1716454644224,
18.4361318938939));
#168882=CARTESIAN_POINT('Ctrl Pts',(-19.8905864547267,-17.178846397086,
18.4353360617012));
#168883=CARTESIAN_POINT('Ctrl Pts',(-19.8979228908496,-17.1836534737331,
18.4348128306544));
#168884=CARTESIAN_POINT('Ctrl Pts',(-19.9507598073018,-17.2187452588739,
18.4310491803284));
#168885=CARTESIAN_POINT('Ctrl Pts',(-19.9951063287632,-17.2507391902587,
18.4279152484629));
#168886=CARTESIAN_POINT('Ctrl Pts',(-20.170748993613,-17.3881042084054,
18.4153889146402));
#168887=CARTESIAN_POINT('Ctrl Pts',(-20.2904970130694,-17.5072362487569,
18.4065304642861));
#168888=CARTESIAN_POINT('Ctrl Pts',(-20.4314208538506,-17.6855384677565,
18.3939311762484));
#168889=CARTESIAN_POINT('Ctrl Pts',(-20.4660160948721,-17.7332786000341,
18.3906172558238));
#168890=CARTESIAN_POINT('Ctrl Pts',(-20.5184690035989,-17.8124140110896,
18.3851631042797));
#168891=CARTESIAN_POINT('Ctrl Pts',(-20.5375947632265,-17.8429321234849,
18.3830687895095));
#168892=CARTESIAN_POINT('Ctrl Pts',(-20.561533971098,-17.8833889434387,
18.3802971754126));
#168893=CARTESIAN_POINT('Ctrl Pts',(-20.5670618765798,-17.8928993648179,
18.3796459830346));
#168894=CARTESIAN_POINT('Ctrl Pts',(-20.5759561220545,-17.908479606408,
18.3785795562632));
#168895=CARTESIAN_POINT('Ctrl Pts',(-20.5793672184751,-17.9145237377989,
18.3781659427359));
#168896=CARTESIAN_POINT('Ctrl Pts',(-20.585886554327,-17.9262092439177,
18.377366403494));
#168897=CARTESIAN_POINT('Ctrl Pts',(-20.5889988936711,-17.9318482522595,
18.3769806306582));
#168898=CARTESIAN_POINT('Ctrl Pts',(-20.5960893389943,-17.9448346202786,
18.3760923004983));
#168899=CARTESIAN_POINT('Ctrl Pts',(-20.6000497593598,-17.9521914678435,
18.3755891195677));
#168900=CARTESIAN_POINT('Ctrl Pts',(-20.6105051183036,-17.9718917994043,
18.3742417625404));
#168901=CARTESIAN_POINT('Ctrl Pts',(-20.6169217092727,-17.9842761933128,
18.373394834383));
#168902=CARTESIAN_POINT('Ctrl Pts',(-20.66082896707,-18.0711099103844,18.3674561459947));
#168903=CARTESIAN_POINT('Ctrl Pts',(-20.69400575322,-18.1476324499798,18.3622161288494));
#168904=CARTESIAN_POINT('Ctrl Pts',(-20.7225805841812,-18.2258896363379,
18.3568546368673));
#168905=CARTESIAN_POINT('',(-20.8509999550625,-18.9515638056372,18.8870728069919));
#168906=CARTESIAN_POINT('Ctrl Pts',(-20.7225805578636,-18.2258895642624,
18.13180632455));
#168907=CARTESIAN_POINT('Ctrl Pts',(-20.7014549938187,-18.1680335083984,
18.1356559381945));
#168908=CARTESIAN_POINT('Ctrl Pts',(-20.6778120416058,-18.1111198991202,
18.1395843440012));
#168909=CARTESIAN_POINT('Ctrl Pts',(-20.5968951827222,-17.9380659014343,
18.1519521181181));
#168910=CARTESIAN_POINT('Ctrl Pts',(-20.5314382088161,-17.826099002912,
18.1605860373068));
#168911=CARTESIAN_POINT('Ctrl Pts',(-20.4404277236397,-17.6987934812837,
18.1708507178815));
#168912=CARTESIAN_POINT('Ctrl Pts',(-20.4242591457825,-17.6770701000627,
18.1726185562031));
#168913=CARTESIAN_POINT('Ctrl Pts',(-20.3725006369513,-17.610245633393,
18.1780953939198));
#168914=CARTESIAN_POINT('Ctrl Pts',(-20.335485787003,-17.5662750447385,
18.1817561699393));
#168915=CARTESIAN_POINT('Ctrl Pts',(-20.2907365793565,-17.5173087400105,
18.185849353701));
#168916=CARTESIAN_POINT('Ctrl Pts',(-20.2847072997032,-17.5107940237516,
18.1863942725033));
#168917=CARTESIAN_POINT('Ctrl Pts',(-20.2755484278858,-17.5010217627692,
18.1872119191199));
#168918=CARTESIAN_POINT('Ctrl Pts',(-20.2724491807455,-17.4977360901224,
18.1874868754641));
#168919=CARTESIAN_POINT('Ctrl Pts',(-20.2668840417111,-17.4918738982177,
18.1879774801173));
#168920=CARTESIAN_POINT('Ctrl Pts',(-20.2644221416631,-17.4892936769958,
18.1881934280994));
#168921=CARTESIAN_POINT('Ctrl Pts',(-20.2590780218465,-17.4837209772744,
18.1886598439083));
#168922=CARTESIAN_POINT('Ctrl Pts',(-20.2561935187446,-17.480730767851,
18.1889101298111));
#168923=CARTESIAN_POINT('Ctrl Pts',(-20.2481155729387,-17.4724059812058,
18.1896070398517));
#168924=CARTESIAN_POINT('Ctrl Pts',(-20.2429027058825,-17.467090219379,
18.1900521765677));
#168925=CARTESIAN_POINT('Ctrl Pts',(-20.2125449124321,-17.4364581461821,
18.1926188135647));
#168926=CARTESIAN_POINT('Ctrl Pts',(-20.1867895801381,-17.4117516615915,
18.1946950947449));
#168927=CARTESIAN_POINT('Ctrl Pts',(-20.1021479413093,-17.3345701398256,
18.2012497117177));
#168928=CARTESIAN_POINT('Ctrl Pts',(-20.0409471990332,-17.2847270473925,
18.2055909871369));
#168929=CARTESIAN_POINT('Ctrl Pts',(-19.903373021049,-17.1849253647089,
18.2148602753393));
#168930=CARTESIAN_POINT('Ctrl Pts',(-19.8262683337281,-17.1362533788287,
18.2197672875293));
#168931=CARTESIAN_POINT('Ctrl Pts',(-19.6529455460105,-17.0418903602357,
18.230613276237));
#168932=CARTESIAN_POINT('Ctrl Pts',(-19.5559411864842,-16.998186246701,
18.2365761377173));
#168933=CARTESIAN_POINT('Ctrl Pts',(-19.442814703661,-16.9571391848231,
18.2436279543692));
#168934=CARTESIAN_POINT('Ctrl Pts',(-19.4295078667641,-16.9524608658553,
18.2444587326609));
#168935=CARTESIAN_POINT('Ctrl Pts',(-19.4082025585544,-16.9452089078474,
18.2457913443706));
#168936=CARTESIAN_POINT('Ctrl Pts',(-19.4002336548818,-16.9425492562635,
18.2462903324053));
#168937=CARTESIAN_POINT('Ctrl Pts',(-19.3861206984003,-16.937932182544,
18.2471750914626));
#168938=CARTESIAN_POINT('Ctrl Pts',(-19.3799831034924,-16.9359552566532,
18.2475602140492));
#168939=CARTESIAN_POINT('Ctrl Pts',(-19.3672398197472,-16.931914797986,
18.2483605946615));
#168940=CARTESIAN_POINT('Ctrl Pts',(-19.3606328603838,-16.9298555567845,
18.2487759883668));
#168941=CARTESIAN_POINT('Ctrl Pts',(-19.3435841033661,-16.9246334186211,
18.2498490264013));
#168942=CARTESIAN_POINT('Ctrl Pts',(-19.3331278345741,-16.9215188094375,
18.2505082421391));
#168943=CARTESIAN_POINT('Ctrl Pts',(-19.2888353712428,-16.9086973267133,
18.253305627886));
#168944=CARTESIAN_POINT('Ctrl Pts',(-19.2547854885508,-16.8997548038335,
18.2554684570319));
#168945=CARTESIAN_POINT('Ctrl Pts',(-19.1649573471851,-16.8785426694681,
18.2612098529141));
#168946=CARTESIAN_POINT('Ctrl Pts',(-19.1088807585081,-16.8676744384256,
18.2648301037279));
#168947=CARTESIAN_POINT('Ctrl Pts',(-18.9020629067177,-16.8362070632004,
18.2782981352708));
#168948=CARTESIAN_POINT('Ctrl Pts',(-18.7496651390731,-16.8296021315434,
18.2884844088056));
#168949=CARTESIAN_POINT('Ctrl Pts',(-18.5754010006632,-16.840828870881,
18.2998902146444));
#168950=CARTESIAN_POINT('Ctrl Pts',(-18.5529288208721,-16.8426374286151,
18.3013554564997));
#168951=CARTESIAN_POINT('Ctrl Pts',(-18.4793873770739,-16.849739983946,
18.3061241724256));
#168952=CARTESIAN_POINT('Ctrl Pts',(-18.4284771731252,-16.8565331066087,
18.3093838584664));
#168953=CARTESIAN_POINT('Ctrl Pts',(-18.3700974592668,-16.8664962344705,
18.3130366263678));
#168954=CARTESIAN_POINT('Ctrl Pts',(-18.3623420350525,-16.8678643574166,
18.3135201223377));
#168955=CARTESIAN_POINT('Ctrl Pts',(-18.3499884060835,-16.8701147932966,
18.3142872879271));
#168956=CARTESIAN_POINT('Ctrl Pts',(-18.3453852680358,-16.8709691234335,
18.3145724800176));
#168957=CARTESIAN_POINT('Ctrl Pts',(-18.3372545430383,-16.8725060828346,
18.3150750056348));
#168958=CARTESIAN_POINT('Ctrl Pts',(-18.3337258118384,-16.8731824312398,
18.3152926927288));
#168959=CARTESIAN_POINT('Ctrl Pts',(-18.3262688272122,-16.8746313957052,
18.3157518340066));
#168960=CARTESIAN_POINT('Ctrl Pts',(-18.3223410457445,-16.8754061703439,
18.3159931635101));
#168961=CARTESIAN_POINT('Ctrl Pts',(-18.3117872920027,-16.8775190715405,
18.3166402846104));
#168962=CARTESIAN_POINT('Ctrl Pts',(-18.3051654272027,-16.8788778122531,
18.3170449155871));
#168963=CARTESIAN_POINT('Ctrl Pts',(-18.2728534276812,-16.8856693564059,
18.3190130075689));
#168964=CARTESIAN_POINT('Ctrl Pts',(-18.2472581438509,-16.8915483509178,
18.3205523838813));
#168965=CARTESIAN_POINT('Ctrl Pts',(-18.1742477755915,-16.90975466547,18.3249042227588));
#168966=CARTESIAN_POINT('Ctrl Pts',(-18.1271404442043,-16.9232539168036,
18.3276643906846));
#168967=CARTESIAN_POINT('Ctrl Pts',(-17.9886552848986,-16.9681949688881,
18.3357480313417));
#168968=CARTESIAN_POINT('Ctrl Pts',(-17.8989149530236,-17.0042691253555,
18.3409499996545));
#168969=CARTESIAN_POINT('Ctrl Pts',(-17.6849954408331,-17.1077741520989,
18.3538813167751));
#168970=CARTESIAN_POINT('Ctrl Pts',(-17.5645156751023,-17.1817236301917,
18.3616604519692));
#168971=CARTESIAN_POINT('Ctrl Pts',(-17.4409213177332,-17.2757421061207,
18.3707579533706));
#168972=CARTESIAN_POINT('Ctrl Pts',(-17.4296415644068,-17.284504254298,
18.3715990630707));
#168973=CARTESIAN_POINT('Ctrl Pts',(-17.4118290307724,-17.2986324133433,
18.3729451247101));
#168974=CARTESIAN_POINT('Ctrl Pts',(-17.4052381145669,-17.3039246688532,
18.373447139033));
#168975=CARTESIAN_POINT('Ctrl Pts',(-17.3936690413186,-17.3133287066519,
18.3743354160077));
#168976=CARTESIAN_POINT('Ctrl Pts',(-17.388677641671,-17.3174240803199,
18.3747210132844));
#168977=CARTESIAN_POINT('Ctrl Pts',(-17.3783916763289,-17.3259425997679,
18.37552056087));
#168978=CARTESIAN_POINT('Ctrl Pts',(-17.3730998476463,-17.3303689169152,
18.3759346378823));
#168979=CARTESIAN_POINT('Ctrl Pts',(-17.3595700160993,-17.3417987292534,
18.3770004261615));
#168980=CARTESIAN_POINT('Ctrl Pts',(-17.3513639371501,-17.3488395514256,
18.3776536684712));
#168981=CARTESIAN_POINT('Ctrl Pts',(-17.3173224481639,-17.3785029531639,
18.3803925052116));
#168982=CARTESIAN_POINT('Ctrl Pts',(-17.2919866618019,-17.4016885610366,
18.3825014902353));
#168983=CARTESIAN_POINT('Ctrl Pts',(-17.2274363561534,-17.4637123686315,
18.3880659656966));
#168984=CARTESIAN_POINT('Ctrl Pts',(-17.1891587191538,-17.5034839733387,
18.3915600140813));
#168985=CARTESIAN_POINT('Ctrl Pts',(-17.0797163025748,-17.6264752538766,
18.4021429232626));
#168986=CARTESIAN_POINT('Ctrl Pts',(-17.01340853863,-17.7137625578543,18.4093801300626));
#168987=CARTESIAN_POINT('Ctrl Pts',(-16.9253080517563,-17.8505644145418,
18.4201285403013));
#168988=CARTESIAN_POINT('Ctrl Pts',(-16.8981645098223,-17.8964265525134,
18.423639715754));
#168989=CARTESIAN_POINT('Ctrl Pts',(-16.8669008644352,-17.954111221494,
18.427909920835));
#168990=CARTESIAN_POINT('Ctrl Pts',(-16.8611173129325,-17.9650087916164,
18.4287103743481));
#168991=CARTESIAN_POINT('Ctrl Pts',(-16.8307021557992,-18.0235482119487,
18.4329747682623));
#168992=CARTESIAN_POINT('Ctrl Pts',(-16.8077901522222,-18.072067002497,
18.4363847848929));
#168993=CARTESIAN_POINT('Ctrl Pts',(-16.7833144611587,-18.1294482757529,
18.4402332104567));
#168994=CARTESIAN_POINT('Ctrl Pts',(-16.7799346250494,-18.137510020333,
18.4407697408754));
#168995=CARTESIAN_POINT('Ctrl Pts',(-16.7748952826621,-18.1497420325298,
18.4415772919435));
#168996=CARTESIAN_POINT('Ctrl Pts',(-16.7731989912835,-18.1538969083261,
18.4418504618232));
#168997=CARTESIAN_POINT('Ctrl Pts',(-16.7701792125227,-18.1613612593019,
18.4423391479487));
#168998=CARTESIAN_POINT('Ctrl Pts',(-16.7688508649702,-18.1646686966084,
18.4425549539098));
#168999=CARTESIAN_POINT('Ctrl Pts',(-16.7659841878458,-18.1718588561873,
18.4430225146984));
#169000=CARTESIAN_POINT('Ctrl Pts',(-16.7644489974607,-18.175742767991,
18.4432740797828));
#169001=CARTESIAN_POINT('Ctrl Pts',(-16.7601728693944,-18.1866553893398,
18.4439781737629));
#169002=CARTESIAN_POINT('Ctrl Pts',(-16.7574579633875,-18.1936943255065,
18.4444291651366));
#169003=CARTESIAN_POINT('Ctrl Pts',(-16.7415285455325,-18.2356613359817,
18.4471000682885));
#169004=CARTESIAN_POINT('Ctrl Pts',(-16.7292016041059,-18.2709219166159,
18.4492703570656));
#169005=CARTESIAN_POINT('Ctrl Pts',(-16.6918543298198,-18.3875728993103,
18.4562669189845));
#169006=CARTESIAN_POINT('Ctrl Pts',(-16.6708078754535,-18.470152062287,
18.4609339761303));
#169007=CARTESIAN_POINT('Ctrl Pts',(-16.6212760910681,-18.7287702646486,
18.4752677833373));
#169008=CARTESIAN_POINT('Ctrl Pts',(-16.6099881174692,-18.9072697929849,
18.4848334076854));
#169009=CARTESIAN_POINT('Ctrl Pts',(-16.6226185942617,-19.1078098802962,
18.496511988687));
#169010=CARTESIAN_POINT('Ctrl Pts',(-16.6244177980262,-19.1305246007929,
18.4978470478919));
#169011=CARTESIAN_POINT('Ctrl Pts',(-16.6274872989933,-19.1626744502725,
18.4997557511401));
#169012=CARTESIAN_POINT('Ctrl Pts',(-16.6284551712544,-19.1721373506553,
18.5003199016387));
#169013=CARTESIAN_POINT('Ctrl Pts',(-16.6301332275919,-19.1875188617696,
18.5012408416864));
#169014=CARTESIAN_POINT('Ctrl Pts',(-16.6308047001797,-19.1934416285285,
18.5015964080893));
#169015=CARTESIAN_POINT('Ctrl Pts',(-16.6322641807379,-19.2058467804165,
18.5023431651883));
#169016=CARTESIAN_POINT('Ctrl Pts',(-16.6330571853879,-19.212328504286,
18.5027345099705));
#169017=CARTESIAN_POINT('Ctrl Pts',(-16.6350181931231,-19.2277642331831,
18.5036692839637));
#169018=CARTESIAN_POINT('Ctrl Pts',(-16.6362135141718,-19.2367145831018,
18.504213570953));
#169019=CARTESIAN_POINT('Ctrl Pts',(-16.6404498328217,-19.2669593542716,
18.5060606148373));
#169020=CARTESIAN_POINT('Ctrl Pts',(-16.6437580302272,-19.288214442803,
18.5073717834588));
#169021=CARTESIAN_POINT('Ctrl Pts',(-16.6777802826256,-19.4868385184168,
18.5197515419801));
#169022=CARTESIAN_POINT('Ctrl Pts',(-16.7306709314759,-19.6596290421803,
18.5315691562101));
#169023=CARTESIAN_POINT('Ctrl Pts',(-16.8541184655078,-19.9328720739976,
18.5513774986948));
#169024=CARTESIAN_POINT('Ctrl Pts',(-16.9126820524977,-20.037758815324,
18.5592673568977));
#169025=CARTESIAN_POINT('Ctrl Pts',(-16.9851454801079,-20.1450160974773,
18.5672622957592));
#169026=CARTESIAN_POINT('Ctrl Pts',(-16.9905255044399,-20.1528647849307,
18.5678468110743));
#169027=CARTESIAN_POINT('Ctrl Pts',(-16.9985758131628,-20.1644408887967,
18.5687078162743));
#169028=CARTESIAN_POINT('Ctrl Pts',(-17.00120549438,-20.1681962092081,18.5689869552935));
#169029=CARTESIAN_POINT('Ctrl Pts',(-17.0059058651723,-20.1748623885648,
18.5694821102408));
#169030=CARTESIAN_POINT('Ctrl Pts',(-17.0079717397612,-20.1777765725071,
18.5696984490793));
#169031=CARTESIAN_POINT('Ctrl Pts',(-17.0124290475295,-20.1840305710991,
18.5701624510054));
#169032=CARTESIAN_POINT('Ctrl Pts',(-17.0148228206061,-20.187368649037,
18.5704099494688));
#169033=CARTESIAN_POINT('Ctrl Pts',(-17.0214568979823,-20.1965631364438,
18.5710912782805));
#169034=CARTESIAN_POINT('Ctrl Pts',(-17.0257175581805,-20.2024048861329,
18.5715237272842));
#169035=CARTESIAN_POINT('Ctrl Pts',(-17.0492173292415,-20.2342808840726,
18.5738817153347));
#169036=CARTESIAN_POINT('Ctrl Pts',(-17.0690228394063,-20.2598945776802,
18.5757702005519));
#169037=CARTESIAN_POINT('Ctrl Pts',(-17.1919348780031,-20.4115323205803,
18.5869796760874));
#169038=CARTESIAN_POINT('Ctrl Pts',(-17.3087208292305,-20.5257822670265,
18.5955854718404));
#169039=CARTESIAN_POINT('Ctrl Pts',(-17.5298999304642,-20.6971376954425,
18.610902358248));
#169040=CARTESIAN_POINT('Ctrl Pts',(-17.6281001113012,-20.7609617786794,
18.6174301598351));
#169041=CARTESIAN_POINT('Ctrl Pts',(-17.7436186511363,-20.8231058718173,
18.6251150119545));
#169042=CARTESIAN_POINT('Ctrl Pts',(-17.7562461383815,-20.829735277134,
18.6259548894507));
#169043=CARTESIAN_POINT('Ctrl Pts',(-17.7764572901219,-20.8400869427208,
18.6272993475603));
#169044=CARTESIAN_POINT('Ctrl Pts',(-17.7839980528673,-20.8438923441368,
18.6278010016303));
#169045=CARTESIAN_POINT('Ctrl Pts',(-17.7973418336955,-20.8505263108383,
18.6286888591268));
#169046=CARTESIAN_POINT('Ctrl Pts',(-17.8031354274767,-20.8533736664966,
18.6290743991974));
#169047=CARTESIAN_POINT('Ctrl Pts',(-17.8151496499936,-20.8592101785023,
18.6298740424715));
#169048=CARTESIAN_POINT('Ctrl Pts',(-17.821372046916,-20.8621954999907,
18.6302882734354));
#169049=CARTESIAN_POINT('Ctrl Pts',(-17.8373906645247,-20.8697846228885,
18.6313549100218));
#169050=CARTESIAN_POINT('Ctrl Pts',(-17.8472077081316,-20.8743437737609,
18.6320088513913));
#169051=CARTESIAN_POINT('Ctrl Pts',(-17.8884051872439,-20.8930936385064,
18.6347544773383));
#169052=CARTESIAN_POINT('Ctrl Pts',(-17.9200931354962,-20.9065921564061,
18.6368696977604));
#169053=CARTESIAN_POINT('Ctrl Pts',(-18.0035804676893,-20.9397740837947,
18.6424545636297));
#169054=CARTESIAN_POINT('Ctrl Pts',(-18.055845678762,-20.9582064660818,
18.6459631202118));
#169055=CARTESIAN_POINT('Ctrl Pts',(-18.213522134828,-21.0069484979291,
18.6565738782987));
#169056=CARTESIAN_POINT('Ctrl Pts',(-18.3206243946559,-21.031141093652,
18.6638243294742));
#169057=CARTESIAN_POINT('Ctrl Pts',(-18.4914030110207,-21.0559958421014,
18.6752237102989));
#169058=CARTESIAN_POINT('Ctrl Pts',(-18.554073482309,-21.0622793377801,
18.6793704933246));
#169059=CARTESIAN_POINT('Ctrl Pts',(-18.6249919884791,-21.0662070382063,
18.6839676911707));
#169060=CARTESIAN_POINT('Ctrl Pts',(-18.6330535776426,-21.0666072849378,
18.6844888706592));
#169061=CARTESIAN_POINT('Ctrl Pts',(-18.6891859357658,-21.0690724469979,
18.6881072421441));
#169062=CARTESIAN_POINT('Ctrl Pts',(-18.7373167833852,-21.069544292762,
18.6911561306833));
#169063=CARTESIAN_POINT('Ctrl Pts',(-18.7931633851969,-21.0681872793371,
18.6946006466039));
#169064=CARTESIAN_POINT('Ctrl Pts',(-18.8009001333698,-21.0679568246359,
18.6950757527208));
#169065=CARTESIAN_POINT('Ctrl Pts',(-18.813274915212,-21.0675202759734,
18.6958321571785));
#169066=CARTESIAN_POINT('Ctrl Pts',(-18.8179137527612,-21.0673413514798,
18.6961149132475));
#169067=CARTESIAN_POINT('Ctrl Pts',(-18.8261364253347,-21.0669971039327,
18.6966146704961));
#169068=CARTESIAN_POINT('Ctrl Pts',(-18.829720472994,-21.0668379281398,
18.6968320120634));
#169069=CARTESIAN_POINT('Ctrl Pts',(-18.837324939827,-21.0664808249313,
18.6972921050877));
#169070=CARTESIAN_POINT('Ctrl Pts',(-18.8413451955132,-21.0662805423629,
18.6975347232917));
#169071=CARTESIAN_POINT('Ctrl Pts',(-18.852212987385,-21.0657080489349,
18.6981889670667));
#169072=CARTESIAN_POINT('Ctrl Pts',(-18.8590593945063,-21.0653140271393,
18.6985993874125));
#169073=CARTESIAN_POINT('Ctrl Pts',(-18.8932695928021,-21.0631783434983,
18.7006420411886));
#169074=CARTESIAN_POINT('Ctrl Pts',(-18.9206010225113,-21.0609383635452,
18.7022479382413));
#169075=CARTESIAN_POINT('Ctrl Pts',(-18.9998397304387,-21.0528916237394,
18.7068478344047));
#169076=CARTESIAN_POINT('Ctrl Pts',(-19.0515874262013,-21.0456941857535,
18.7097821218539));
#169077=CARTESIAN_POINT('Ctrl Pts',(-19.2434591622088,-21.0117285807831,
18.7205711117203));
#169078=CARTESIAN_POINT('Ctrl Pts',(-19.3810286281969,-20.9727391869252,
18.7281483031524));
#169079=CARTESIAN_POINT('Ctrl Pts',(-19.5986152830153,-20.8865500668099,
18.7410970678788));
#169080=CARTESIAN_POINT('Ctrl Pts',(-19.681315743512,-20.8474243523152,
18.7462633657484));
#169081=CARTESIAN_POINT('Ctrl Pts',(-19.7742999114314,-20.7958244878542,
18.7524977771358));
#169082=CARTESIAN_POINT('Ctrl Pts',(-19.7872987516286,-20.7884297891322,
18.7533793034606));
#169083=CARTESIAN_POINT('Ctrl Pts',(-19.8070974068586,-20.776887494625,
18.7547378239759));
#169084=CARTESIAN_POINT('Ctrl Pts',(-19.8139541451335,-20.7728381186709,
18.7552112631254));
#169085=CARTESIAN_POINT('Ctrl Pts',(-19.8261168622928,-20.7655623288055,
18.7560564085619));
#169086=CARTESIAN_POINT('Ctrl Pts',(-19.8314318250461,-20.7623510569701,
18.7564275586831));
#169087=CARTESIAN_POINT('Ctrl Pts',(-19.8427245918092,-20.7554600228029,
18.7572200952087));
#169088=CARTESIAN_POINT('Ctrl Pts',(-19.8486983646158,-20.7517738270142,
18.7576417152163));
#169089=CARTESIAN_POINT('Ctrl Pts',(-19.8609114982971,-20.7441534202578,
18.7585086321117));
#169090=CARTESIAN_POINT('Ctrl Pts',(-19.867148845742,-20.7402161776401,
18.758954037484));
#169091=CARTESIAN_POINT('Ctrl Pts',(-19.8826137461638,-20.7303407633873,
18.7600650822019));
#169092=CARTESIAN_POINT('Ctrl Pts',(-19.8918158673302,-20.7243633427829,
18.7607321761089));
#169093=CARTESIAN_POINT('Ctrl Pts',(-20.0261796544709,-20.6355917126041,
18.7705618694351));
#169094=CARTESIAN_POINT('Ctrl Pts',(-20.1422134237702,-20.5398061363553,
18.7802400241385));
#169095=CARTESIAN_POINT('Ctrl Pts',(-20.3517752295694,-20.3256375691789,
18.7999877219203));
#169096=CARTESIAN_POINT('Ctrl Pts',(-20.4447938226567,-20.2078931310709,
18.8099925747814));
#169097=CARTESIAN_POINT('Ctrl Pts',(-20.5330045107872,-20.0680280605751,
18.8203082801053));
#169098=CARTESIAN_POINT('Ctrl Pts',(-20.5412380994583,-20.0546451591922,
18.8212804206672));
#169099=CARTESIAN_POINT('Ctrl Pts',(-20.5523029246649,-20.0362034124847,
18.822598444156));
#169100=CARTESIAN_POINT('Ctrl Pts',(-20.5552632834292,-20.0312231556703,
18.8229522502487));
#169101=CARTESIAN_POINT('Ctrl Pts',(-20.5599344129934,-20.0232908845442,
18.8235123170366));
#169102=CARTESIAN_POINT('Ctrl Pts',(-20.56165853141,-20.0203468223416,18.823719433486));
#169103=CARTESIAN_POINT('Ctrl Pts',(-20.5652041562149,-20.0142586977605,
18.8241461642087));
#169104=CARTESIAN_POINT('Ctrl Pts',(-20.5670246862172,-20.0111141121592,
18.8243657098303));
#169105=CARTESIAN_POINT('Ctrl Pts',(-20.5713425418894,-20.0036114363162,
18.8248874981458));
#169106=CARTESIAN_POINT('Ctrl Pts',(-20.5738324899966,-19.9992490817204,
18.8251892650863));
#169107=CARTESIAN_POINT('Ctrl Pts',(-20.5821739629807,-19.9845133642999,
18.8262032984603));
#169108=CARTESIAN_POINT('Ctrl Pts',(-20.587953592802,-19.9740992786041,
18.826911096927));
#169109=CARTESIAN_POINT('Ctrl Pts',(-20.6534232358866,-19.8537494480221,
18.8349959405946));
#169110=CARTESIAN_POINT('Ctrl Pts',(-20.7033526973828,-19.7387633066903,
18.8418238728466));
#169111=CARTESIAN_POINT('Ctrl Pts',(-20.7942050477999,-19.4655590440802,
18.8574732205239));
#169112=CARTESIAN_POINT('Ctrl Pts',(-20.8275799265213,-19.3057012584407,
18.8662583302302));
#169113=CARTESIAN_POINT('Ctrl Pts',(-20.8447697715777,-19.1165532345429,
18.8772499428655));
#169114=CARTESIAN_POINT('Ctrl Pts',(-20.846707235207,-19.0894584832142,
18.8788369536102));
#169115=CARTESIAN_POINT('Ctrl Pts',(-20.8486554031477,-19.0521296886354,
18.8810434997841));
#169116=CARTESIAN_POINT('Ctrl Pts',(-20.8491140970807,-19.0419209618802,
18.8816490081777));
#169117=CARTESIAN_POINT('Ctrl Pts',(-20.8497282756523,-19.0256205847214,
18.8826192609571));
#169118=CARTESIAN_POINT('Ctrl Pts',(-20.849931406149,-19.0195308090262,
18.8829825085533));
#169119=CARTESIAN_POINT('Ctrl Pts',(-20.8502862993211,-19.0073076836303,
18.8837131702452));
#169120=CARTESIAN_POINT('Ctrl Pts',(-20.8504376956036,-19.0011743831896,
18.8840805922278));
#169121=CARTESIAN_POINT('Ctrl Pts',(-20.8507174561178,-18.9874168814135,
18.8849065617177));
#169122=CARTESIAN_POINT('Ctrl Pts',(-20.8508312920819,-18.9797924991866,
18.8853655601581));
#169123=CARTESIAN_POINT('Ctrl Pts',(-20.8509693632245,-18.965299885361,
18.8862404589823));
#169124=CARTESIAN_POINT('Ctrl Pts',(-20.8510013701741,-18.9584318247995,
18.8866561084519));
#169125=CARTESIAN_POINT('Ctrl Pts',(-20.8509999550625,-18.9515638056372,
18.8870728069919));
#169126=CARTESIAN_POINT('Ctrl Pts',(-20.8509999552294,-18.9515646165639,
18.8870727577911));
#169127=CARTESIAN_POINT('Ctrl Pts',(-20.8509977754035,-18.9409654736441,
18.8877158320748));
#169128=CARTESIAN_POINT('Ctrl Pts',(-20.8509159958824,-18.9303666120166,
18.8883613944822));
#169129=CARTESIAN_POINT('Ctrl Pts',(-20.8504276848002,-18.8982971073801,
18.8903224437704));
#169130=CARTESIAN_POINT('Ctrl Pts',(-20.8497740635919,-18.8768321572957,
18.8916455393117));
#169131=CARTESIAN_POINT('Ctrl Pts',(-20.8411283389369,-18.6875938653183,
18.9034051797753));
#169132=CARTESIAN_POINT('Ctrl Pts',(-20.8135225495725,-18.5213410133495,
18.9144672333324));
#169133=CARTESIAN_POINT('Ctrl Pts',(-20.7534085349207,-18.3148990616014,
18.9286689878955));
#169134=CARTESIAN_POINT('Ctrl Pts',(-20.7387334245607,-18.2701270183631,
18.931773307545));
#169135=CARTESIAN_POINT('Ctrl Pts',(-20.7225805608153,-18.2258895723463,
18.9348455085272));
#169136=CARTESIAN_POINT('Origin',(-18.734,-18.952,0.));
#169137=CARTESIAN_POINT('',(-20.7225805743325,-18.2258896093654,19.9537493095993));
#169138=CARTESIAN_POINT('',(-20.7225805414791,-18.2258895193907,19.7345260867578));
#169139=CARTESIAN_POINT('',(-20.7225805737622,-18.2258896078036,0.));
#169140=CARTESIAN_POINT('',(-20.8479141116672,-18.9511715446921,19.9109957148815));
#169141=CARTESIAN_POINT('Ctrl Pts',(-20.7225805743325,-18.2258896093654,
19.9537493095993));
#169142=CARTESIAN_POINT('Ctrl Pts',(-20.7405652798718,-18.2751438777686,
19.9507625960589));
#169143=CARTESIAN_POINT('Ctrl Pts',(-20.7567161784059,-18.3250557419143,
19.9478476276529));
#169144=CARTESIAN_POINT('Ctrl Pts',(-20.8240164173824,-18.5628627648768,
19.934264720273));
#169145=CARTESIAN_POINT('Ctrl Pts',(-20.8509329970543,-18.7565969413757,
19.9239834015846));
#169146=CARTESIAN_POINT('Ctrl Pts',(-20.8509998750795,-18.9512727356193,
19.9127740399324));
#169147=CARTESIAN_POINT('Ctrl Pts',(-20.7202230294519,-18.2267290932703,
19.1554367770419));
#169148=CARTESIAN_POINT('Ctrl Pts',(-20.6328469384039,-17.9823750760586,
19.1710019356974));
#169149=CARTESIAN_POINT('Ctrl Pts',(-20.1480308738017,-17.1326717534008,
19.2289590299134));
#169150=CARTESIAN_POINT('Ctrl Pts',(-18.3741968410994,-16.4747290082863,
19.3293080596899));
#169151=CARTESIAN_POINT('Ctrl Pts',(-16.456252502104,-17.9136376975394,
19.4564838663714));
#169152=CARTESIAN_POINT('Ctrl Pts',(-16.6280001175491,-20.3051793956671,
19.5836596730528));
#169153=CARTESIAN_POINT('Ctrl Pts',(-18.7318719157577,-21.4552629005109,
19.7108354797342));
#169154=CARTESIAN_POINT('Ctrl Pts',(-20.5383021339267,-20.4717616627176,
19.8199301623757));
#169155=CARTESIAN_POINT('Ctrl Pts',(-20.8463943782946,-19.3568003242117,
19.8866329094569));
#169156=CARTESIAN_POINT('Ctrl Pts',(-20.847823891442,-18.9511685861152,
19.9109437209775));
#169157=CARTESIAN_POINT('Ctrl Pts',(-20.7225805608153,-18.2258895723463,
18.9348455085272));
#169158=CARTESIAN_POINT('Ctrl Pts',(-20.7101483133892,-18.191841685665,
18.9372100652618));
#169159=CARTESIAN_POINT('Ctrl Pts',(-20.6968406754583,-18.1581104763876,
18.9395554959463));
#169160=CARTESIAN_POINT('Ctrl Pts',(-20.6682555312599,-18.0907769770335,
18.9442220241356));
#169161=CARTESIAN_POINT('Ctrl Pts',(-20.6529555715504,-18.0572042398701,
18.946540783944));
#169162=CARTESIAN_POINT('Ctrl Pts',(-20.6334898971761,-18.0172895412496,
18.9492731725517));
#169163=CARTESIAN_POINT('Ctrl Pts',(-20.6301587436143,-18.0105503018847,
18.9497336570361));
#169164=CARTESIAN_POINT('Ctrl Pts',(-20.624923832368,-18.0001000826112,
18.9504462090837));
#169165=CARTESIAN_POINT('Ctrl Pts',(-20.6230449261506,-17.9963768210117,
18.9506997834402));
#169166=CARTESIAN_POINT('Ctrl Pts',(-20.6195395988019,-17.9894813617797,
18.9511688146376));
#169167=CARTESIAN_POINT('Ctrl Pts',(-20.6179161827287,-17.9863077486529,
18.9513844493235));
#169168=CARTESIAN_POINT('Ctrl Pts',(-20.6142273513526,-17.9791411633206,
18.951870870775));
#169169=CARTESIAN_POINT('Ctrl Pts',(-20.6121572347693,-17.975150671178,
18.9521413572984));
#169170=CARTESIAN_POINT('Ctrl Pts',(-20.6060078757759,-17.9633885748988,
18.9529376423619));
#169171=CARTESIAN_POINT('Ctrl Pts',(-20.601892937943,-17.9556356011869,
18.953461242705));
#169172=CARTESIAN_POINT('Ctrl Pts',(-20.5717300485923,-17.899649204765,
18.9572347038645));
#169173=CARTESIAN_POINT('Ctrl Pts',(-20.5438632214111,-17.852413648208,
18.960377446766));
#169174=CARTESIAN_POINT('Ctrl Pts',(-20.4242375867613,-17.6665375375298,
18.9727934453743));
#169175=CARTESIAN_POINT('Ctrl Pts',(-20.3181325105313,-17.5378400653005,
18.9815481062807));
#169176=CARTESIAN_POINT('Ctrl Pts',(-20.154583850435,-17.3812508164102,
18.9940889063644));
#169177=CARTESIAN_POINT('Ctrl Pts',(-20.1093578780004,-17.3415027549366,
18.997470164347));
#169178=CARTESIAN_POINT('Ctrl Pts',(-20.0340386896833,-17.2807953691487,
19.003025047076));
#169179=CARTESIAN_POINT('Ctrl Pts',(-20.0049868156137,-17.2585957980946,
19.0051505037588));
#169180=CARTESIAN_POINT('Ctrl Pts',(-19.9687427476027,-17.2323586408162,
19.0077883404947));
#169181=CARTESIAN_POINT('Ctrl Pts',(-19.9620817909277,-17.2275954161152,
19.0082725606268));
#169182=CARTESIAN_POINT('Ctrl Pts',(-19.9491828911,-17.2184841053645,19.0092092622059));
#169183=CARTESIAN_POINT('Ctrl Pts',(-19.9429488194956,-17.2141307398694,
19.0096615327218));
#169184=CARTESIAN_POINT('Ctrl Pts',(-19.9366515643159,-17.2097835331961,
19.0101179815018));
#169185=CARTESIAN_POINT('Ctrl Pts',(-19.9366116357795,-17.2097559712136,
19.0101208756562));
#169186=CARTESIAN_POINT('Ctrl Pts',(-19.9365301503012,-17.2096997273242,
19.0101267819639));
#169187=CARTESIAN_POINT('Ctrl Pts',(-19.9364885933154,-17.2096710455554,
19.0101297941191));
#169188=CARTESIAN_POINT('Ctrl Pts',(-19.9364037426463,-17.209612487867,
19.0101359442734));
#169189=CARTESIAN_POINT('Ctrl Pts',(-19.9363604488869,-17.2095826120819,
19.0101390822766));
#169190=CARTESIAN_POINT('Ctrl Pts',(-19.9362720061143,-17.20952158512,19.0101454927157));
#169191=CARTESIAN_POINT('Ctrl Pts',(-19.9362268569848,-17.2094904340712,
19.0101487651583));
#169192=CARTESIAN_POINT('Ctrl Pts',(-19.936134573514,-17.2094267675529,
19.0101554538906));
#169193=CARTESIAN_POINT('Ctrl Pts',(-19.9360874389634,-17.2093942521714,
19.0101588701935));
#169194=CARTESIAN_POINT('Ctrl Pts',(-19.9359910413571,-17.2093277588489,
19.0101658570264));
#169195=CARTESIAN_POINT('Ctrl Pts',(-19.9359417782042,-17.2092937811012,
19.0101694275615));
#169196=CARTESIAN_POINT('Ctrl Pts',(-19.9358409654384,-17.2092242548982,
19.0101767343007));
#169197=CARTESIAN_POINT('Ctrl Pts',(-19.9357894157444,-17.2091887066794,
19.0101804705084));
#169198=CARTESIAN_POINT('Ctrl Pts',(-19.9356838552768,-17.2091159200133,
19.0101881212419));
#169199=CARTESIAN_POINT('Ctrl Pts',(-19.9356298443481,-17.2090786817886,
19.0101920357762));
#169200=CARTESIAN_POINT('Ctrl Pts',(-19.9355191677221,-17.2090023825796,
19.0102000571928));
#169201=CARTESIAN_POINT('Ctrl Pts',(-19.9354625017867,-17.2089633218038,
19.0102041640894));
#169202=CARTESIAN_POINT('Ctrl Pts',(-19.9353462991118,-17.208883229718,
19.0102125858786));
#169203=CARTESIAN_POINT('Ctrl Pts',(-19.9352867622703,-17.2088421987604,
19.0102169007752));
#169204=CARTESIAN_POINT('Ctrl Pts',(-19.935164576904,-17.2087580016018,
19.0102257560118));
#169205=CARTESIAN_POINT('Ctrl Pts',(-19.9351019281163,-17.2087148357014,
19.0102302963669));
#169206=CARTESIAN_POINT('Ctrl Pts',(-19.9349732486296,-17.2086261839453,
19.010239622093));
#169207=CARTESIAN_POINT('Ctrl Pts',(-19.934907217613,-17.2085806984222,
19.0102444074825));
#169208=CARTESIAN_POINT('Ctrl Pts',(-19.9347714693171,-17.208487199462,
19.0102542453208));
#169209=CARTESIAN_POINT('Ctrl Pts',(-19.9347017517542,-17.2084391864635,
19.010259297785));
#169210=CARTESIAN_POINT('Ctrl Pts',(-19.9345582862882,-17.2083403975427,
19.0102696946925));
#169211=CARTESIAN_POINT('Ctrl Pts',(-19.9344845380962,-17.2082896221537,
19.010275039151));
#169212=CARTESIAN_POINT('Ctrl Pts',(-19.9343326207668,-17.2081850417752,
19.0102860483358));
#169213=CARTESIAN_POINT('Ctrl Pts',(-19.9342544512108,-17.2081312373478,
19.0102917130858));
#169214=CARTESIAN_POINT('Ctrl Pts',(-19.9340932450911,-17.2080202944855,
19.0103033951579));
#169215=CARTESIAN_POINT('Ctrl Pts',(-19.9340102080862,-17.2079631567398,
19.0103094125041));
#169216=CARTESIAN_POINT('Ctrl Pts',(-19.9338387550747,-17.2078451980006,
19.0103218368465));
#169217=CARTESIAN_POINT('Ctrl Pts',(-19.9337503385751,-17.2077843778347,
19.0103282438691));
#169218=CARTESIAN_POINT('Ctrl Pts',(-19.933567535728,-17.2076586514248,
19.0103414903509));
#169219=CARTESIAN_POINT('Ctrl Pts',(-19.9334731486601,-17.2075937460657,
19.0103483298514));
#169220=CARTESIAN_POINT('Ctrl Pts',(-19.933277716491,-17.2074593803058,
19.0103624911224));
#169221=CARTESIAN_POINT('Ctrl Pts',(-19.9331766706376,-17.2073899210335,
19.0103698129347));
#169222=CARTESIAN_POINT('Ctrl Pts',(-19.9329671231812,-17.2072459041853,
19.0103849965917));
#169223=CARTESIAN_POINT('Ctrl Pts',(-19.9328586171266,-17.207171345526,
19.0103928587434));
#169224=CARTESIAN_POINT('Ctrl Pts',(-19.9326331949499,-17.2070164802836,
19.0104091921796));
#169225=CARTESIAN_POINT('Ctrl Pts',(-19.9325162787512,-17.2069361760419,
19.0104176634505));
#169226=CARTESIAN_POINT('Ctrl Pts',(-19.9272497993052,-17.2033196577882,
19.0107992449026));
#169227=CARTESIAN_POINT('Ctrl Pts',(-19.9220846628211,-17.1998062734238,
19.0111732180024));
#169228=CARTESIAN_POINT('Ctrl Pts',(-19.9101877741213,-17.1917906641275,
19.0120340236554));
#169229=CARTESIAN_POINT('Ctrl Pts',(-19.9034456171162,-17.1873041248282,
19.0125214411161));
#169230=CARTESIAN_POINT('Ctrl Pts',(-19.8836696498884,-17.1743073949284,
19.0139500135982));
#169231=CARTESIAN_POINT('Ctrl Pts',(-19.8705677326564,-17.1659022784926,
19.0148950717558));
#169232=CARTESIAN_POINT('Ctrl Pts',(-19.7583330406485,-17.0956366784126,
19.0229804842031));
#169233=CARTESIAN_POINT('Ctrl Pts',(-19.6543443052849,-17.0419472486438,
19.0304217705248));
#169234=CARTESIAN_POINT('Ctrl Pts',(-19.3961508642354,-16.9346390465809,
19.0486855589556));
#169235=CARTESIAN_POINT('Ctrl Pts',(-19.2391284953313,-16.8897113999657,
19.0596483580096));
#169236=CARTESIAN_POINT('Ctrl Pts',(-19.0465105225225,-16.8579422165123,
19.0720522004168));
#169237=CARTESIAN_POINT('Ctrl Pts',(-19.0143918159746,-16.8534001039692,
19.0740847793175));
#169238=CARTESIAN_POINT('Ctrl Pts',(-18.9749949391518,-16.848749473756,
19.0765241962998));
#169239=CARTESIAN_POINT('Ctrl Pts',(-18.9678059825353,-16.8479381893932,
19.076967147741));
#169240=CARTESIAN_POINT('Ctrl Pts',(-18.9565279679913,-16.8467239650184,
19.077658479534));
#169241=CARTESIAN_POINT('Ctrl Pts',(-18.9524417342475,-16.8462960584621,
19.0779082281117));
#169242=CARTESIAN_POINT('Ctrl Pts',(-18.9448005496863,-16.8455183628175,
19.0783738492124));
#169243=CARTESIAN_POINT('Ctrl Pts',(-18.9412459985656,-16.8451656790714,
19.078589876769));
#169244=CARTESIAN_POINT('Ctrl Pts',(-18.9331286933074,-16.8443810192673,
19.0790819176182));
#169245=CARTESIAN_POINT('Ctrl Pts',(-18.928565427183,-16.8439548629371,
19.0793576011537));
#169246=CARTESIAN_POINT('Ctrl Pts',(-18.914530882507,-16.8426901585234,
19.0802027353073));
#169247=CARTESIAN_POINT('Ctrl Pts',(-18.9050551594078,-16.8419005836319,
19.0807695059423));
#169248=CARTESIAN_POINT('Ctrl Pts',(-18.7758513589094,-16.8320106096061,
19.088449157343));
#169249=CARTESIAN_POINT('Ctrl Pts',(-18.6555472623204,-16.8330473991746,
19.0950401932027));
#169250=CARTESIAN_POINT('Ctrl Pts',(-18.4276535225468,-16.8544595463309,
19.1074983522716));
#169251=CARTESIAN_POINT('Ctrl Pts',(-18.3202880838129,-16.8729700285359,
19.1133590281367));
#169252=CARTESIAN_POINT('Ctrl Pts',(-18.1422882174557,-16.9179979169929,
19.1235738221552));
#169253=CARTESIAN_POINT('Ctrl Pts',(-18.0707816757159,-16.9401781713834,
19.1278173256892));
#169254=CARTESIAN_POINT('Ctrl Pts',(-17.9829885357855,-16.9726002433909,
19.1332820626392));
#169255=CARTESIAN_POINT('Ctrl Pts',(-17.9654610696231,-16.9793394882244,
19.1343859786424));
#169256=CARTESIAN_POINT('Ctrl Pts',(-17.9400880896355,-16.9894847866668,
19.1360038334498));
#169257=CARTESIAN_POINT('Ctrl Pts',(-17.9321695884559,-16.9927067417471,
19.1365115750622));
#169258=CARTESIAN_POINT('Ctrl Pts',(-17.9183127948655,-16.9984429965021,
19.1374051606786));
#169259=CARTESIAN_POINT('Ctrl Pts',(-17.9123660346458,-17.0009366468277,
19.1377903006078));
#169260=CARTESIAN_POINT('Ctrl Pts',(-17.900835242363,-17.0058339113044,
19.1385403385857));
#169261=CARTESIAN_POINT('Ctrl Pts',(-17.8952499828551,-17.0082344879853,
19.1389051301054));
#169262=CARTESIAN_POINT('Ctrl Pts',(-17.8819136279847,-17.0140347135778,
19.1397797771414));
#169263=CARTESIAN_POINT('Ctrl Pts',(-17.8741724737975,-17.0174568346295,
19.1402903981253));
#169264=CARTESIAN_POINT('Ctrl Pts',(-17.8462580594494,-17.029997566416,
19.1421424261568));
#169265=CARTESIAN_POINT('Ctrl Pts',(-17.8262081668378,-17.0393858107417,
19.143493068673));
#169266=CARTESIAN_POINT('Ctrl Pts',(-17.6397246871797,-17.1302984564891,
19.1562520690146));
#169267=CARTESIAN_POINT('Ctrl Pts',(-17.4845546907044,-17.2330195161703,
19.1684571195222));
#169268=CARTESIAN_POINT('Ctrl Pts',(-17.284157874126,-17.4072996309446,
19.1859916809906));
#169269=CARTESIAN_POINT('Ctrl Pts',(-17.2265910897872,-17.4634229881563,
19.1912698442899));
#169270=CARTESIAN_POINT('Ctrl Pts',(-17.1479917538631,-17.549299577346,
19.1986912316919));
#169271=CARTESIAN_POINT('Ctrl Pts',(-17.1243158052112,-17.5765336117748,
19.2009579947399));
#169272=CARTESIAN_POINT('Ctrl Pts',(-17.0965912909633,-17.6101216491536,
19.203637447941));
#169273=CARTESIAN_POINT('Ctrl Pts',(-17.0918669906679,-17.6159071991872,
19.2040949456575));
#169274=CARTESIAN_POINT('Ctrl Pts',(-17.0845593030779,-17.6249537715524,
19.2048038863541));
#169275=CARTESIAN_POINT('Ctrl Pts',(-17.0819547944477,-17.6281975432115,
19.2050568121235));
#169276=CARTESIAN_POINT('Ctrl Pts',(-17.0771355599793,-17.634236006639,
19.2055252520864));
#169277=CARTESIAN_POINT('Ctrl Pts',(-17.0749183543924,-17.6370285903149,
19.2057409402898));
#169278=CARTESIAN_POINT('Ctrl Pts',(-17.0699130514561,-17.6433656112877,
19.206228254774));
#169279=CARTESIAN_POINT('Ctrl Pts',(-17.0671292243886,-17.6469133538681,
19.206499576062));
#169280=CARTESIAN_POINT('Ctrl Pts',(-17.0599715841504,-17.6560953980065,
19.2071980117624));
#169281=CARTESIAN_POINT('Ctrl Pts',(-17.0556148306113,-17.6617430097167,
19.2076239448919));
#169282=CARTESIAN_POINT('Ctrl Pts',(-17.0290541481358,-17.696535516794,
19.2102263355417));
#169283=CARTESIAN_POINT('Ctrl Pts',(-17.0075799347702,-17.7262326698287,
19.2123551159605));
#169284=CARTESIAN_POINT('Ctrl Pts',(-16.890539391678,-17.8972730372875,
19.2241944910592));
#169285=CARTESIAN_POINT('Ctrl Pts',(-16.8115572535784,-18.0492143334176,
19.2331708284439));
#169286=CARTESIAN_POINT('Ctrl Pts',(-16.7182073512736,-18.2982738125913,
19.2478021752191));
#169287=CARTESIAN_POINT('Ctrl Pts',(-16.6908195419361,-18.3896936088725,
19.2531477559489));
#169288=CARTESIAN_POINT('Ctrl Pts',(-16.6649450735421,-18.5034935746245,
19.2599434909318));
#169289=CARTESIAN_POINT('Ctrl Pts',(-16.6605202634838,-18.5244160488914,
19.2611982872611));
#169290=CARTESIAN_POINT('Ctrl Pts',(-16.6546830461206,-18.5542423340368,
19.2629960837188));
#169291=CARTESIAN_POINT('Ctrl Pts',(-16.653009285874,-18.5630940995251,
19.2635307474836));
#169292=CARTESIAN_POINT('Ctrl Pts',(-16.6502205088103,-18.578376361172,
19.2644558566976));
#169293=CARTESIAN_POINT('Ctrl Pts',(-16.6490786283418,-18.5848018737439,
19.2648454413258));
#169294=CARTESIAN_POINT('Ctrl Pts',(-16.646949950947,-18.5971103341509,
19.2655929344194));
#169295=CARTESIAN_POINT('Ctrl Pts',(-16.6459582705416,-18.60299238248,19.2659506834388));
#169296=CARTESIAN_POINT('Ctrl Pts',(-16.643445826809,-18.6182887609983,
19.2668824354375));
#169297=CARTESIAN_POINT('Ctrl Pts',(-16.6419638054525,-18.6277092382887,
19.267457662252));
#169298=CARTESIAN_POINT('Ctrl Pts',(-16.6371349041361,-18.6598157692268,
19.2694230470449));
#169299=CARTESIAN_POINT('Ctrl Pts',(-16.6340930910722,-18.6825454325821,
19.2708227967042));
#169300=CARTESIAN_POINT('Ctrl Pts',(-16.6108742340152,-18.8804510061067,
19.2830870664644));
#169301=CARTESIAN_POINT('Ctrl Pts',(-16.6122925456928,-19.0574323901985,
19.2946629473972));
#169302=CARTESIAN_POINT('Ctrl Pts',(-16.6470546155064,-19.3178097049176,
19.3120182724925));
#169303=CARTESIAN_POINT('Ctrl Pts',(-16.663726550155,-19.4026967079917,
19.3177125441004));
#169304=CARTESIAN_POINT('Ctrl Pts',(-16.6950510195942,-19.5227848349962,
19.3256351705694));
#169305=CARTESIAN_POINT('Ctrl Pts',(-16.7055318301905,-19.5589806934331,
19.3280046819857));
#169306=CARTESIAN_POINT('Ctrl Pts',(-16.7192706293368,-19.602085967026,
19.330788619515));
#169307=CARTESIAN_POINT('Ctrl Pts',(-16.7216060145436,-19.609279737099,
19.331251941267));
#169308=CARTESIAN_POINT('Ctrl Pts',(-16.7252920372529,-19.6204300980979,
19.3319679224975));
#169309=CARTESIAN_POINT('Ctrl Pts',(-16.7266158990158,-19.6243953803083,
19.3322221117235));
#169310=CARTESIAN_POINT('Ctrl Pts',(-16.729090130019,-19.6317338556515,
19.3326917080113));
#169311=CARTESIAN_POINT('Ctrl Pts',(-16.7302372613418,-19.6351080359124,
19.3329072965428));
#169312=CARTESIAN_POINT('Ctrl Pts',(-16.7328464284257,-19.6427195338902,
19.3333928922242));
#169313=CARTESIAN_POINT('Ctrl Pts',(-16.7343134001171,-19.6469551025934,
19.3336626035485));
#169314=CARTESIAN_POINT('Ctrl Pts',(-16.7386725704694,-19.6594131906992,
19.3344544967689));
#169315=CARTESIAN_POINT('Ctrl Pts',(-16.7416021509993,-19.6676226593819,
19.3349745164931));
#169316=CARTESIAN_POINT('Ctrl Pts',(-16.7628005644233,-19.7258869357973,
19.338653853538));
#169317=CARTESIAN_POINT('Ctrl Pts',(-16.78290438591,-19.7752588447044,19.3417120238881));
#169318=CARTESIAN_POINT('Ctrl Pts',(-16.8121247842516,-19.8399169720583,
19.3457025569934));
#169319=CARTESIAN_POINT('Ctrl Pts',(-16.8195989883718,-19.8559190699414,
19.346688934853));
#169320=CARTESIAN_POINT('Ctrl Pts',(-16.8444620114034,-19.9074581669546,
19.3498674665437));
#169321=CARTESIAN_POINT('Ctrl Pts',(-16.8626472551777,-19.942602440803,
19.3520375368829));
#169322=CARTESIAN_POINT('Ctrl Pts',(-16.8864672287967,-19.9856364239982,
19.3547212921827));
#169323=CARTESIAN_POINT('Ctrl Pts',(-16.8911846929554,-19.9940236768286,
19.355245625933));
#169324=CARTESIAN_POINT('Ctrl Pts',(-16.9501050331804,-20.0971274527719,
19.3617101411828));
#169325=CARTESIAN_POINT('Ctrl Pts',(-17.0114956169318,-20.1875467927259,
19.367587427947));
#169326=CARTESIAN_POINT('Ctrl Pts',(-17.1265936104555,-20.3317143463212,
19.3778472346854));
#169327=CARTESIAN_POINT('Ctrl Pts',(-17.1767131752537,-20.3880442198723,
19.3821195574633));
#169328=CARTESIAN_POINT('Ctrl Pts',(-17.2429883901071,-20.4549732852334,
19.3876190271278));
#169329=CARTESIAN_POINT('Ctrl Pts',(-17.2564296321415,-20.4681893321695,
19.3887271038609));
#169330=CARTESIAN_POINT('Ctrl Pts',(-17.2762301306267,-20.4871447220901,
19.3903499471542));
#169331=CARTESIAN_POINT('Ctrl Pts',(-17.2824508029408,-20.4930279799684,
19.3908584617271));
#169332=CARTESIAN_POINT('Ctrl Pts',(-17.293420241668,-20.5032770767062,
19.3917529404323));
#169333=CARTESIAN_POINT('Ctrl Pts',(-17.2981536205257,-20.5076592756639,
19.3921381960605));
#169334=CARTESIAN_POINT('Ctrl Pts',(-17.3073839052033,-20.5161267304554,
19.392888111906));
#169335=CARTESIAN_POINT('Ctrl Pts',(-17.3118785190972,-20.520214399633,
19.3932526639616));
#169336=CARTESIAN_POINT('Ctrl Pts',(-17.3226657296067,-20.5299404185947,
19.3941261748342));
#169337=CARTESIAN_POINT('Ctrl Pts',(-17.3289745711554,-20.5355605225199,
19.3946358946464));
#169338=CARTESIAN_POINT('Ctrl Pts',(-17.3518645674362,-20.5557071424222,
19.3964812864004));
#169339=CARTESIAN_POINT('Ctrl Pts',(-17.3686382833067,-20.5700118286111,
19.3978261078191));
#169340=CARTESIAN_POINT('Ctrl Pts',(-17.5292301135471,-20.7026895677109,
19.4106359539574));
#169341=CARTESIAN_POINT('Ctrl Pts',(-17.6878329156799,-20.8018353899521,
19.4229069649804));
#169342=CARTESIAN_POINT('Ctrl Pts',(-17.9298612685993,-20.9119498112448,
19.440461057947));
#169343=CARTESIAN_POINT('Ctrl Pts',(-18.0042246878999,-20.9408368607195,
19.4456970283631));
#169344=CARTESIAN_POINT('Ctrl Pts',(-18.1141992882798,-20.9765556763063,
19.4530672197101));
#169345=CARTESIAN_POINT('Ctrl Pts',(-18.1486332409006,-20.9867787892037,
19.4553232345235));
#169346=CARTESIAN_POINT('Ctrl Pts',(-18.190515166339,-20.9980617960486,
19.4579917297661));
#169347=CARTESIAN_POINT('Ctrl Pts',(-18.1977277797753,-20.9999640493162,
19.4584485996968));
#169348=CARTESIAN_POINT('Ctrl Pts',(-18.2089762261266,-21.0028672125696,
19.4591567811294));
#169349=CARTESIAN_POINT('Ctrl Pts',(-18.2130051255652,-21.0038943998716,
19.4594095703964));
#169350=CARTESIAN_POINT('Ctrl Pts',(-18.2204951135059,-21.0057805257495,
19.459877886552));
#169351=CARTESIAN_POINT('Ctrl Pts',(-18.2239553130831,-21.0066425806023,
19.4600935866421));
#169352=CARTESIAN_POINT('Ctrl Pts',(-18.2317991610488,-21.0085757170738,
19.4605810919392));
#169353=CARTESIAN_POINT('Ctrl Pts',(-18.2361840544666,-21.0096415256161,
19.4608525911412));
#169354=CARTESIAN_POINT('Ctrl Pts',(-18.2475181281418,-21.0123580764884,
19.4615517891884));
#169355=CARTESIAN_POINT('Ctrl Pts',(-18.2544723794457,-21.0139877010777,
19.4619783024377));
#169356=CARTESIAN_POINT('Ctrl Pts',(-18.2973043473353,-21.0237963221259,
19.4645906634016));
#169357=CARTESIAN_POINT('Ctrl Pts',(-18.3333843796563,-21.0310744540621,
19.4667284137824));
#169358=CARTESIAN_POINT('Ctrl Pts',(-18.5372432908988,-21.0666926058822,
19.4785484183481));
#169359=CARTESIAN_POINT('Ctrl Pts',(-18.7077821135932,-21.0756672566111,
19.4875020754519));
#169360=CARTESIAN_POINT('Ctrl Pts',(-18.97292910807,-21.0576441602349,19.5021196386494));
#169361=CARTESIAN_POINT('Ctrl Pts',(-19.0677297480415,-21.0447125498654,
19.5074781566405));
#169362=CARTESIAN_POINT('Ctrl Pts',(-19.1822988813553,-21.0211002048489,
19.5142895635556));
#169363=CARTESIAN_POINT('Ctrl Pts',(-19.203204364688,-21.0164599195375,
19.5155460379922));
#169364=CARTESIAN_POINT('Ctrl Pts',(-19.2328040485607,-21.0094170129046,
19.5173458251005));
#169365=CARTESIAN_POINT('Ctrl Pts',(-19.241559262988,-21.0072746372635,
19.5178807758486));
#169366=CARTESIAN_POINT('Ctrl Pts',(-19.2566304395562,-21.0034845908973,
19.5188062250182));
#169367=CARTESIAN_POINT('Ctrl Pts',(-19.2629530005789,-21.0018634892955,
19.519195860917));
#169368=CARTESIAN_POINT('Ctrl Pts',(-19.2750381887715,-20.9987052177558,
19.519943343238));
#169369=CARTESIAN_POINT('Ctrl Pts',(-19.2808020232943,-20.9971728817603,
19.5203010296874));
#169370=CARTESIAN_POINT('Ctrl Pts',(-19.2957596466676,-20.993128593397,
19.5212323794074));
#169371=CARTESIAN_POINT('Ctrl Pts',(-19.3049430088916,-20.9905788950537,
19.5218072644184));
#169372=CARTESIAN_POINT('Ctrl Pts',(-19.3361297546822,-20.9816928469804,
19.5237702306762));
#169373=CARTESIAN_POINT('Ctrl Pts',(-19.3580468242027,-20.9750617368602,
19.5251678716111));
#169374=CARTESIAN_POINT('Ctrl Pts',(-19.548199806244,-20.9141461138245,
19.5374569004443));
#169375=CARTESIAN_POINT('Ctrl Pts',(-19.7091002162916,-20.8393511398131,
19.5490637032728));
#169376=CARTESIAN_POINT('Ctrl Pts',(-19.931755790896,-20.6997087010685,
19.5664275169328));
#169377=CARTESIAN_POINT('Ctrl Pts',(-20.0018543448731,-20.6495428984462,
19.5721007360978));
#169378=CARTESIAN_POINT('Ctrl Pts',(-20.0978873299732,-20.5715412053722,
19.5799981582999));
#169379=CARTESIAN_POINT('Ctrl Pts',(-20.1264344625499,-20.5470639596866,
19.5823626094695));
#169380=CARTESIAN_POINT('Ctrl Pts',(-20.1599214405646,-20.5167664933397,
19.5851414124359));
#169381=CARTESIAN_POINT('Ctrl Pts',(-20.1654993780857,-20.511665242236,
19.5856044546681));
#169382=CARTESIAN_POINT('Ctrl Pts',(-20.1741189508785,-20.5036970950474,
19.586320098126));
#169383=CARTESIAN_POINT('Ctrl Pts',(-20.1771795548684,-20.5008509420098,
19.5865742268315));
#169384=CARTESIAN_POINT('Ctrl Pts',(-20.1828344231619,-20.4955609855554,
19.5870437673393));
#169385=CARTESIAN_POINT('Ctrl Pts',(-20.1854309222924,-20.4931197163027,
19.5872593602544));
#169386=CARTESIAN_POINT('Ctrl Pts',(-20.1912800867429,-20.4875923455621,
19.587745036444));
#169387=CARTESIAN_POINT('Ctrl Pts',(-20.1945291111164,-20.4845024696222,
19.5880148234617));
#169388=CARTESIAN_POINT('Ctrl Pts',(-20.2040695793198,-20.4753714283376,
19.5888071448289));
#169389=CARTESIAN_POINT('Ctrl Pts',(-20.2103336212087,-20.4693015921458,
19.5893275135088));
#169390=CARTESIAN_POINT('Ctrl Pts',(-20.2546644095094,-20.4258107519157,
19.5930128190976));
#169391=CARTESIAN_POINT('Ctrl Pts',(-20.291344719402,-20.3869971516115,
19.5960762463696));
#169392=CARTESIAN_POINT('Ctrl Pts',(-20.3355344069428,-20.3365445712775,
19.5998479353816));
#169393=CARTESIAN_POINT('Ctrl Pts',(-20.3444475999265,-20.3261668988453,
19.6006131056275));
#169394=CARTESIAN_POINT('Ctrl Pts',(-20.3868892527341,-20.2757717336107,
19.6042819764768));
#169395=CARTESIAN_POINT('Ctrl Pts',(-20.4190314109285,-20.2346082846777,
19.6071384888453));
#169396=CARTESIAN_POINT('Ctrl Pts',(-20.5137302287811,-20.103617783417,
19.6159390577793));
#169397=CARTESIAN_POINT('Ctrl Pts',(-20.5708677304338,-20.0101017306773,
19.6218309140156));
#169398=CARTESIAN_POINT('Ctrl Pts',(-20.6549212413534,-19.8450280149816,
19.6321302259222));
#169399=CARTESIAN_POINT('Ctrl Pts',(-20.6856664651168,-19.7756708746541,
19.6364278586011));
#169400=CARTESIAN_POINT('Ctrl Pts',(-20.71934941304,-19.6871424346948,19.6419578335176));
#169401=CARTESIAN_POINT('Ctrl Pts',(-20.7258375543615,-19.6693770374386,
19.6430695541002));
#169402=CARTESIAN_POINT('Ctrl Pts',(-20.7349196704995,-19.6434354486702,
19.6446967649728));
#169403=CARTESIAN_POINT('Ctrl Pts',(-20.7377034740661,-19.6353263438405,
19.6452059550948));
#169404=CARTESIAN_POINT('Ctrl Pts',(-20.7424958172422,-19.6210853339409,
19.6461012150884));
#169405=CARTESIAN_POINT('Ctrl Pts',(-20.7445257366996,-19.6149607021688,
19.6464865725825));
#169406=CARTESIAN_POINT('Ctrl Pts',(-20.7484115458999,-19.603054524388,
19.6472363846186));
#169407=CARTESIAN_POINT('Ctrl Pts',(-20.7502706244743,-19.597274079495,
19.6476007295784));
#169408=CARTESIAN_POINT('Ctrl Pts',(-20.7546531721575,-19.5834435284464,
19.6484732565121));
#169409=CARTESIAN_POINT('Ctrl Pts',(-20.757153425305,-19.5753862255621,
19.6489821956122));
#169410=CARTESIAN_POINT('Ctrl Pts',(-20.7659891983743,-19.5462989926952,
19.6508218766976));
#169411=CARTESIAN_POINT('Ctrl Pts',(-20.7720453441935,-19.5251862812417,
19.6521616945787));
#169412=CARTESIAN_POINT('Ctrl Pts',(-20.8265422864656,-19.3234062360452,
19.665013519989));
#169413=CARTESIAN_POINT('Ctrl Pts',(-20.8511563473453,-19.1371933086967,
19.677339284135));
#169414=CARTESIAN_POINT('Ctrl Pts',(-20.8509463099948,-18.887209432531,
19.6938412930769));
#169415=CARTESIAN_POINT('Ctrl Pts',(-20.8480800908105,-18.8242283125836,
19.6979837889211));
#169416=CARTESIAN_POINT('Ctrl Pts',(-20.8379188596087,-18.7117861112607,
19.7052635376531));
#169417=CARTESIAN_POINT('Ctrl Pts',(-20.8316744040226,-18.6622755763367,
19.7084278926623));
#169418=CARTESIAN_POINT('Ctrl Pts',(-20.8224344764443,-18.6053135194725,
19.711986642042));
#169419=CARTESIAN_POINT('Ctrl Pts',(-20.8211403742769,-18.5976059529908,
19.7124664260019));
#169420=CARTESIAN_POINT('Ctrl Pts',(-20.8190058158766,-18.5853100723495,
19.7132288325168));
#169421=CARTESIAN_POINT('Ctrl Pts',(-20.8181928414099,-18.5807171481805,
19.7135129487449));
#169422=CARTESIAN_POINT('Ctrl Pts',(-20.8167271896856,-18.57259343029,19.7140142493685));
#169423=CARTESIAN_POINT('Ctrl Pts',(-20.8160807013085,-18.5690615639899,
19.7142317815118));
#169424=CARTESIAN_POINT('Ctrl Pts',(-20.8146926433247,-18.5615858259236,
19.7146913321523));
#169425=CARTESIAN_POINT('Ctrl Pts',(-20.8139488463912,-18.5576424207429,
19.7149332222231));
#169426=CARTESIAN_POINT('Ctrl Pts',(-20.8119140369176,-18.5470203389648,
19.7155834406428));
#169427=CARTESIAN_POINT('Ctrl Pts',(-20.8106020277839,-18.5403456647312,
19.7159905890604));
#169428=CARTESIAN_POINT('Ctrl Pts',(-20.803970731503,-18.5074484527189,
19.7179907208875));
#169429=CARTESIAN_POINT('Ctrl Pts',(-20.7981865537565,-18.4813207785408,
19.7195586651717));
#169430=CARTESIAN_POINT('Ctrl Pts',(-20.7800922390971,-18.4063518374011,
19.7240162882166));
#169431=CARTESIAN_POINT('Ctrl Pts',(-20.7665321585851,-18.357829091126,
19.7268505746596));
#169432=CARTESIAN_POINT('Ctrl Pts',(-20.7422796918877,-18.2816442556438,
19.7312843315893));
#169433=CARTESIAN_POINT('Ctrl Pts',(-20.7327195762116,-18.2536570392336,
19.7329094971324));
#169434=CARTESIAN_POINT('Ctrl Pts',(-20.7225805414791,-18.2258895193907,
19.7345260867578));
#169435=CARTESIAN_POINT('Origin',(-18.734,-18.952,0.));
#169436=CARTESIAN_POINT('',(-20.7225805788317,-18.2258896216872,20.755413772291));
#169437=CARTESIAN_POINT('',(-20.7225805737622,-18.2258896078036,20.5336910569984));
#169438=CARTESIAN_POINT('',(-20.7225805737622,-18.2258896078036,0.));
#169439=CARTESIAN_POINT('Ctrl Pts',(-20.7225805788317,-18.2258896216873,
20.755413772291));
#169440=CARTESIAN_POINT('Ctrl Pts',(-20.7319594498863,-18.2515753044535,
20.7536068528629));
#169441=CARTESIAN_POINT('Ctrl Pts',(-20.7408447755382,-18.277453954992,
20.7517982257749));
#169442=CARTESIAN_POINT('Ctrl Pts',(-20.7725200329136,-18.375887392365,
20.7449760667245));
#169443=CARTESIAN_POINT('Ctrl Pts',(-20.7918958199826,-18.4494703633789,
20.7399904291453));
#169444=CARTESIAN_POINT('Ctrl Pts',(-20.8143280497788,-18.5581190996573,
20.732925459953));
#169445=CARTESIAN_POINT('Ctrl Pts',(-20.8205389606962,-18.5924691228743,
20.7307345037727));
#169446=CARTESIAN_POINT('Ctrl Pts',(-20.8270336495132,-18.6342676521286,
20.7281324773479));
#169447=CARTESIAN_POINT('Ctrl Pts',(-20.8281309523597,-18.6415821188121,
20.7276795047987));
#169448=CARTESIAN_POINT('Ctrl Pts',(-20.8297832008251,-18.6530034342135,
20.7269760486136));
#169449=CARTESIAN_POINT('Ctrl Pts',(-20.8303644475973,-18.6571063331596,
20.7267241180626));
#169450=CARTESIAN_POINT('Ctrl Pts',(-20.8314236225145,-18.6647442395575,
20.7262565992299));
#169451=CARTESIAN_POINT('Ctrl Pts',(-20.8319046584193,-18.6682787131087,
20.726040842706));
#169452=CARTESIAN_POINT('Ctrl Pts',(-20.8329764089929,-18.6763053106689,
20.7255521954007));
#169453=CARTESIAN_POINT('Ctrl Pts',(-20.8335616364932,-18.680798114541,
20.7252796168897));
#169454=CARTESIAN_POINT('Ctrl Pts',(-20.835259186705,-18.6941651342987,
20.7244713321322));
#169455=CARTESIAN_POINT('Ctrl Pts',(-20.8363297185985,-18.7030446860307,
20.7239379246181));
#169456=CARTESIAN_POINT('Ctrl Pts',(-20.8440773295531,-18.7709246959512,
20.7198853747505));
#169457=CARTESIAN_POINT('Ctrl Pts',(-20.8483264214979,-18.8301815006446,
20.7164921316396));
#169458=CARTESIAN_POINT('Ctrl Pts',(-20.8506770340003,-18.9098227212251,
20.7120328634702));
#169459=CARTESIAN_POINT('Ctrl Pts',(-20.8509840406084,-18.9301095183887,
20.710905785112));
#169460=CARTESIAN_POINT('Ctrl Pts',(-20.8511051846752,-19.0901947745642,
20.7020608620862));
#169461=CARTESIAN_POINT('Ctrl Pts',(-20.8373639001827,-19.2296587432821,
20.6946257986704));
#169462=CARTESIAN_POINT('Ctrl Pts',(-20.7922497624043,-19.4554696483924,
20.6818795550826));
#169463=CARTESIAN_POINT('Ctrl Pts',(-20.7688587852084,-19.542948911302,
20.6767638662586));
#169464=CARTESIAN_POINT('Ctrl Pts',(-20.7355595809391,-19.6416641653536,
20.6706561060802));
#169465=CARTESIAN_POINT('Ctrl Pts',(-20.7310458544951,-19.6546273968654,
20.6698473346312));
#169466=CARTESIAN_POINT('Ctrl Pts',(-20.7236045398111,-19.6753474230732,
20.6685434430718));
#169467=CARTESIAN_POINT('Ctrl Pts',(-20.720756848974,-19.6831326414369,
20.6680509769946));
#169468=CARTESIAN_POINT('Ctrl Pts',(-20.7156191670394,-19.6969267247075,
20.6671737914043));
#169469=CARTESIAN_POINT('Ctrl Pts',(-20.7133473731812,-19.7029422902152,
20.6667896842574));
#169470=CARTESIAN_POINT('Ctrl Pts',(-20.7085566075865,-19.7154551479226,
20.6659873958386));
#169471=CARTESIAN_POINT('Ctrl Pts',(-20.7060328946614,-19.7219505308911,
20.6655690589631));
#169472=CARTESIAN_POINT('Ctrl Pts',(-20.6993949321713,-19.7387881859352,
20.6644796971704));
#169473=CARTESIAN_POINT('Ctrl Pts',(-20.6952311444706,-19.7491105817125,
20.663807008012));
#169474=CARTESIAN_POINT('Ctrl Pts',(-20.6767885703737,-19.7938119503979,
20.6608724366708));
#169475=CARTESIAN_POINT('Ctrl Pts',(-20.6616864867406,-19.8278420644715,
20.6585827761449));
#169476=CARTESIAN_POINT('Ctrl Pts',(-20.619174332485,-19.9172036395332,
20.6524167790992));
#169477=CARTESIAN_POINT('Ctrl Pts',(-20.5902290846934,-19.9717611426819,
20.6484906701569));
#169478=CARTESIAN_POINT('Ctrl Pts',(-20.4847189653704,-20.1512159401868,
20.6350415698986));
#169479=CARTESIAN_POINT('Ctrl Pts',(-20.3975957566837,-20.2694140260674,
20.6252362741343));
#169480=CARTESIAN_POINT('Ctrl Pts',(-20.2858382990858,-20.3920930540122,
20.614403749887));
#169481=CARTESIAN_POINT('Ctrl Pts',(-20.2724921822452,-20.4063424454815,
20.6131349579298));
#169482=CARTESIAN_POINT('Ctrl Pts',(-20.2223182615595,-20.4584484551818,
20.6084615483341));
#169483=CARTESIAN_POINT('Ctrl Pts',(-20.1842716892352,-20.4951108945269,
20.6051053299749));
#169484=CARTESIAN_POINT('Ctrl Pts',(-20.138409392091,-20.5361082115037,
20.6013107909744));
#169485=CARTESIAN_POINT('Ctrl Pts',(-20.1318927170487,-20.5418617939658,
20.6007772680363));
#169486=CARTESIAN_POINT('Ctrl Pts',(-20.1219663773764,-20.5505175565522,
20.5999733611395));
#169487=CARTESIAN_POINT('Ctrl Pts',(-20.118582734132,-20.5534492488146,
20.5997008556792));
#169488=CARTESIAN_POINT('Ctrl Pts',(-20.1124893257787,-20.558695016444,
20.5992128912468));
#169489=CARTESIAN_POINT('Ctrl Pts',(-20.1097830088015,-20.56101299262,20.5989971462405));
#169490=CARTESIAN_POINT('Ctrl Pts',(-20.1038860686669,-20.5660380002131,
20.5985291750485));
#169491=CARTESIAN_POINT('Ctrl Pts',(-20.1006932791657,-20.5687424002105,
20.5982771415332));
#169492=CARTESIAN_POINT('Ctrl Pts',(-20.0916937761393,-20.5763195717387,
20.5975704278406));
#169493=CARTESIAN_POINT('Ctrl Pts',(-20.0858688111858,-20.581170703819,
20.5971173035557));
#169494=CARTESIAN_POINT('Ctrl Pts',(-20.0507102080234,-20.6101329930512,
20.5944071623565));
#169495=CARTESIAN_POINT('Ctrl Pts',(-20.0207562855254,-20.6334843026105,
20.5922014799787));
#169496=CARTESIAN_POINT('Ctrl Pts',(-19.9196809192604,-20.7079962177203,
20.5850331461083));
#169497=CARTESIAN_POINT('Ctrl Pts',(-19.8460095528,-20.755551813513,20.5802387771415));
#169498=CARTESIAN_POINT('Ctrl Pts',(-19.6172811145266,-20.8838391130274,
20.5659714918296));
#169499=CARTESIAN_POINT('Ctrl Pts',(-19.4549978447177,-20.9500848969404,
20.5565785128704));
#169500=CARTESIAN_POINT('Ctrl Pts',(-19.264170593288,-21.0016681998836,
20.5450925586047));
#169501=CARTESIAN_POINT('Ctrl Pts',(-19.241817119652,-21.0073204857568,
20.5437418553941));
#169502=CARTESIAN_POINT('Ctrl Pts',(-19.2100738002255,-21.0147976335202,
20.5418146221661));
#169503=CARTESIAN_POINT('Ctrl Pts',(-19.2007565735709,-21.016925818666,
20.5412478413817));
#169504=CARTESIAN_POINT('Ctrl Pts',(-19.1855972553012,-21.0202805780205,
20.5403237679748));
#169505=CARTESIAN_POINT('Ctrl Pts',(-19.1797637579931,-21.0215456751057,
20.5399677152002));
#169506=CARTESIAN_POINT('Ctrl Pts',(-19.1675440245699,-21.0241416779993,
20.5392208822395));
#169507=CARTESIAN_POINT('Ctrl Pts',(-19.1611568397807,-21.0254677686649,
20.5388299521328));
#169508=CARTESIAN_POINT('Ctrl Pts',(-19.1459514913743,-21.0285514241805,
20.5378979157298));
#169509=CARTESIAN_POINT('Ctrl Pts',(-19.1371281120967,-21.0302823604723,
20.5373559650466));
#169510=CARTESIAN_POINT('Ctrl Pts',(-19.1073845519166,-21.0359207989474,
20.5355251823452));
#169511=CARTESIAN_POINT('Ctrl Pts',(-19.0864170712646,-21.0395689391925,
20.5342281393105));
#169512=CARTESIAN_POINT('Ctrl Pts',(-18.9079848837578,-21.0678496769323,
20.523132286479));
#169513=CARTESIAN_POINT('Ctrl Pts',(-18.7482861853164,-21.074938602777,
20.5127600434867));
#169514=CARTESIAN_POINT('Ctrl Pts',(-18.4580291623978,-21.0550577038001,
20.4935418429057));
#169515=CARTESIAN_POINT('Ctrl Pts',(-18.327834767814,-21.0338375356172,
20.4848031189808));
#169516=CARTESIAN_POINT('Ctrl Pts',(-18.1852107812422,-20.9966924555746,
20.4756084986054));
#169517=CARTESIAN_POINT('Ctrl Pts',(-18.1700201228866,-20.9925547226939,
20.4746343977949));
#169518=CARTESIAN_POINT('Ctrl Pts',(-18.1492990980026,-20.9866615146536,
20.4733141354613));
#169519=CARTESIAN_POINT('Ctrl Pts',(-18.143728128247,-20.9850523218168,
20.4729600180005));
#169520=CARTESIAN_POINT('Ctrl Pts',(-18.1348888083314,-20.9824596593075,
20.4723995676275));
#169521=CARTESIAN_POINT('Ctrl Pts',(-18.1316161515394,-20.9814911548351,
20.4721923771189));
#169522=CARTESIAN_POINT('Ctrl Pts',(-18.124864557165,-20.9794753295323,
20.4717655975538));
#169523=CARTESIAN_POINT('Ctrl Pts',(-18.1213859719914,-20.9784269669583,
20.4715460767376));
#169524=CARTESIAN_POINT('Ctrl Pts',(-18.1131075513809,-20.9759087839327,
20.4710244962207));
#169525=CARTESIAN_POINT('Ctrl Pts',(-18.108310175003,-20.974430825148,20.470722911176));
#169526=CARTESIAN_POINT('Ctrl Pts',(-18.0921660941982,-20.9693942714715,
20.4697101479295));
#169527=CARTESIAN_POINT('Ctrl Pts',(-18.0808438912191,-20.9657570661299,
20.4690034223074));
#169528=CARTESIAN_POINT('Ctrl Pts',(-17.9458112460332,-20.9211197588971,
20.460610617561));
#169529=CARTESIAN_POINT('Ctrl Pts',(-17.8260924564993,-20.8688692962793,
20.4535207494897));
#169530=CARTESIAN_POINT('Ctrl Pts',(-17.5698440899828,-20.7275994400364,
20.4376243946124));
#169531=CARTESIAN_POINT('Ctrl Pts',(-17.4372537334809,-20.6332062600607,
20.4288424937918));
#169532=CARTESIAN_POINT('Ctrl Pts',(-17.2991230565875,-20.5087209211266,
20.4180452046454));
#169533=CARTESIAN_POINT('Ctrl Pts',(-17.2817679447368,-20.4925433651398,
20.416655948622));
#169534=CARTESIAN_POINT('Ctrl Pts',(-17.2577286955992,-20.4693679530358,
20.4146830356628));
#169535=CARTESIAN_POINT('Ctrl Pts',(-17.2508146540427,-20.4626103713148,
20.4141097737895));
#169536=CARTESIAN_POINT('Ctrl Pts',(-17.2396928871838,-20.4515903180152,
20.4131780217954));
#169537=CARTESIAN_POINT('Ctrl Pts',(-17.2354564877059,-20.4473568837989,
20.4128208134773));
#169538=CARTESIAN_POINT('Ctrl Pts',(-17.2266554700819,-20.4384870667187,
20.412073881593));
#169539=CARTESIAN_POINT('Ctrl Pts',(-17.2220941534652,-20.4338475094095,
20.4116840183707));
#169540=CARTESIAN_POINT('Ctrl Pts',(-17.2113459825874,-20.4228136885758,
20.4107587695479));
#169541=CARTESIAN_POINT('Ctrl Pts',(-17.2051779456261,-20.4164013403187,
20.410222571876));
#169542=CARTESIAN_POINT('Ctrl Pts',(-17.1847720438394,-20.3949177373855,
20.4084309937269));
#169543=CARTESIAN_POINT('Ctrl Pts',(-17.1707155232986,-20.3796765929037,
20.4071678726075));
#169544=CARTESIAN_POINT('Ctrl Pts',(-17.0968741218778,-20.2972139694611,
20.4003731490595));
#169545=CARTESIAN_POINT('Ctrl Pts',(-17.0412031231709,-20.2264476832418,
20.3946735584241));
#169546=CARTESIAN_POINT('Ctrl Pts',(-16.9134063284424,-20.0407945271189,
20.3800670199015));
#169547=CARTESIAN_POINT('Ctrl Pts',(-16.8474928229997,-19.9221143400743,
20.371014339092));
#169548=CARTESIAN_POINT('Ctrl Pts',(-16.7632115370659,-19.7287745988722,
20.3572224489953));
#169549=CARTESIAN_POINT('Ctrl Pts',(-16.7367684475921,-19.6580131598617,
20.3523635289208));
#169550=CARTESIAN_POINT('Ctrl Pts',(-16.7113174135762,-19.5769273899586,
20.3471145792649));
#169551=CARTESIAN_POINT('Ctrl Pts',(-16.7085358505008,-19.5678523158582,
20.3465315437632));
#169552=CARTESIAN_POINT('Ctrl Pts',(-16.7045027522383,-19.5543710610501,
20.3456722940923));
#169553=CARTESIAN_POINT('Ctrl Pts',(-16.7032043731267,-19.549979177435,
20.3453934460292));
#169554=CARTESIAN_POINT('Ctrl Pts',(-16.7009187949656,-19.5421547003413,
20.3448986132645));
#169555=CARTESIAN_POINT('Ctrl Pts',(-16.6999260225646,-19.5387237949614,
20.3446823072442));
#169556=CARTESIAN_POINT('Ctrl Pts',(-16.6978093309882,-19.5313388098229,
20.3442181594933));
#169557=CARTESIAN_POINT('Ctrl Pts',(-16.6966882472189,-19.5273839759487,
20.3439704835246));
#169558=CARTESIAN_POINT('Ctrl Pts',(-16.6936233321182,-19.5164506446258,
20.3432881531373));
#169559=CARTESIAN_POINT('Ctrl Pts',(-16.6917037686742,-19.5094653209097,
20.3428548868364));
#169560=CARTESIAN_POINT('Ctrl Pts',(-16.6813498343758,-19.4710158172424,
20.3404840398845));
#169561=CARTESIAN_POINT('Ctrl Pts',(-16.6736061942495,-19.4393681863663,
20.3385839924498));
#169562=CARTESIAN_POINT('Ctrl Pts',(-16.6315963079364,-19.2487174569867,
20.3273754004952));
#169563=CARTESIAN_POINT('Ctrl Pts',(-16.6150140975621,-19.0863618491143,
20.3187785306604));
#169564=CARTESIAN_POINT('Ctrl Pts',(-16.6187513230299,-18.8068744552872,
20.3034766474504));
#169565=CARTESIAN_POINT('Ctrl Pts',(-16.6299804197431,-18.690399666584,
20.2969545227988));
#169566=CARTESIAN_POINT('Ctrl Pts',(-16.6532984925502,-18.5613922235532,
20.2892743737388));
#169567=CARTESIAN_POINT('Ctrl Pts',(-16.6559824485171,-18.5473566521685,
20.2884328726693));
#169568=CARTESIAN_POINT('Ctrl Pts',(-16.6604801968123,-18.5250619410746,
20.2870863059099));
#169569=CARTESIAN_POINT('Ctrl Pts',(-16.6622017631394,-18.5167844867783,
20.2865841814317));
#169570=CARTESIAN_POINT('Ctrl Pts',(-16.6653254436715,-18.5022041914738,
20.2856957812265));
#169571=CARTESIAN_POINT('Ctrl Pts',(-16.6667069045332,-18.495897001349,
20.2853101715272));
#169572=CARTESIAN_POINT('Ctrl Pts',(-16.6696238864007,-18.4828647905564,
20.2845106686236));
#169573=CARTESIAN_POINT('Ctrl Pts',(-16.6711634649905,-18.4761407653336,
20.2840966490654));
#169574=CARTESIAN_POINT('Ctrl Pts',(-16.6751997356624,-18.458900314784,
20.2830311571573));
#169575=CARTESIAN_POINT('Ctrl Pts',(-16.6777441326717,-18.4483953641108,
20.2823781553349));
#169576=CARTESIAN_POINT('Ctrl Pts',(-16.6886998490004,-18.4046306092178,
20.2796415923445));
#169577=CARTESIAN_POINT('Ctrl Pts',(-16.6978381947843,-18.3715597840504,
20.277534688551));
#169578=CARTESIAN_POINT('Ctrl Pts',(-16.7237400994648,-18.285981135677,
20.2719769974288));
#169579=CARTESIAN_POINT('Ctrl Pts',(-16.7417568792228,-18.2338826544624,
20.2684877683368));
#169580=CARTESIAN_POINT('Ctrl Pts',(-16.8015464442778,-18.080633104425,
20.2579141275802));
#169581=CARTESIAN_POINT('Ctrl Pts',(-16.8491461704739,-17.9819589765353,
20.2506813367646));
#169582=CARTESIAN_POINT('Ctrl Pts',(-16.9285139381713,-17.8455389585049,
20.2402556475015));
#169583=CARTESIAN_POINT('Ctrl Pts',(-16.954306752471,-17.8045122494924,
20.2370618076706));
#169584=CARTESIAN_POINT('Ctrl Pts',(-16.9913899411259,-17.7497891474341,
20.2327493449413));
#169585=CARTESIAN_POINT('Ctrl Pts',(-17.0014775419252,-17.7352967872106,
20.2316021016933));
#169586=CARTESIAN_POINT('Ctrl Pts',(-17.0427688014109,-17.6775306344351,
20.2270129848426));
#169587=CARTESIAN_POINT('Ctrl Pts',(-17.0754246199141,-17.6353132960956,
20.2236215821015));
#169588=CARTESIAN_POINT('Ctrl Pts',(-17.1152357822057,-17.587680591574,
20.2197920781617));
#169589=CARTESIAN_POINT('Ctrl Pts',(-17.1208693983504,-17.5810241763437,
20.2192568622761));
#169590=CARTESIAN_POINT('Ctrl Pts',(-17.1294614193724,-17.5709985365952,
20.2184508970899));
#169591=CARTESIAN_POINT('Ctrl Pts',(-17.1323895817939,-17.5676036810949,
20.2181780108231));
#169592=CARTESIAN_POINT('Ctrl Pts',(-17.1376648141155,-17.5615268159373,
20.2176896291212));
#169593=CARTESIAN_POINT('Ctrl Pts',(-17.1400078814604,-17.5588414204019,
20.217473845552));
#169594=CARTESIAN_POINT('Ctrl Pts',(-17.1451136751808,-17.5530194007646,
20.2170060997205));
#169595=CARTESIAN_POINT('Ctrl Pts',(-17.1478789038048,-17.549885047818,
20.2167543284641));
#169596=CARTESIAN_POINT('Ctrl Pts',(-17.1556717595684,-17.5411044967379,
20.216049077642));
#169597=CARTESIAN_POINT('Ctrl Pts',(-17.1607204333561,-17.535476945208,
20.2155971437204));
#169598=CARTESIAN_POINT('Ctrl Pts',(-17.1910710203988,-17.5020088162227,
20.2129089615556));
#169599=CARTESIAN_POINT('Ctrl Pts',(-17.2170829332868,-17.4748177921317,
20.2107230867002));
#169600=CARTESIAN_POINT('Ctrl Pts',(-17.3050419776655,-17.3876469742849,
20.2036512497106));
#169601=CARTESIAN_POINT('Ctrl Pts',(-17.3699313674244,-17.3307534011999,
20.1989284466934));
#169602=CARTESIAN_POINT('Ctrl Pts',(-17.5777740462778,-17.1698598044226,
20.1846244361364));
#169603=CARTESIAN_POINT('Ctrl Pts',(-17.7303956652488,-17.0796608677314,
20.1751347597826));
#169604=CARTESIAN_POINT('Ctrl Pts',(-17.9134594916861,-17.0003527365709,
20.1635408625699));
#169605=CARTESIAN_POINT('Ctrl Pts',(-17.9346252643696,-16.9915883752631,
20.1621987222171));
#169606=CARTESIAN_POINT('Ctrl Pts',(-17.9647938324817,-16.9796659155622,
20.1602816379588));
#169607=CARTESIAN_POINT('Ctrl Pts',(-17.9736826110846,-16.9762223474342,
20.1597163031272));
#169608=CARTESIAN_POINT('Ctrl Pts',(-17.9881703118271,-16.9707219653485,
20.1587939573545));
#169609=CARTESIAN_POINT('Ctrl Pts',(-17.9937552662259,-16.9686285503337,
20.1584381771129));
#169610=CARTESIAN_POINT('Ctrl Pts',(-18.0054702381554,-16.9642937876832,
20.1576914019823));
#169611=CARTESIAN_POINT('Ctrl Pts',(-18.0116019152963,-16.962057134963,
20.1573002549101));
#169612=CARTESIAN_POINT('Ctrl Pts',(-18.0262244633854,-16.9567997571908,
20.1563667515129));
#169613=CARTESIAN_POINT('Ctrl Pts',(-18.0347244213131,-16.9538048443001,
20.1558235435568));
#169614=CARTESIAN_POINT('Ctrl Pts',(-18.0634768852977,-16.9438799991201,
20.1539839864242));
#169615=CARTESIAN_POINT('Ctrl Pts',(-18.0838147826669,-16.9372031577252,
20.1526793179631));
#169616=CARTESIAN_POINT('Ctrl Pts',(-18.1954372001421,-16.9024240726618,
20.1454976501836));
#169617=CARTESIAN_POINT('Ctrl Pts',(-18.2884304783548,-16.8802193870545,
20.1394304838841));
#169618=CARTESIAN_POINT('Ctrl Pts',(-18.5505747220782,-16.8360933339181,
20.1221541194405));
#169619=CARTESIAN_POINT('Ctrl Pts',(-18.7213427941413,-16.8281961998806,
20.1106611848412));
#169620=CARTESIAN_POINT('Ctrl Pts',(-18.9278180397878,-16.843571348049,
20.0974473662598));
#169621=CARTESIAN_POINT('Ctrl Pts',(-18.964354763366,-16.8472496891824,
20.0951381494348));
#169622=CARTESIAN_POINT('Ctrl Pts',(-19.0078600839502,-16.8527761922972,
20.0924375781891));
#169623=CARTESIAN_POINT('Ctrl Pts',(-19.0149359624417,-16.8537114286337,
20.0919999066417));
#169624=CARTESIAN_POINT('Ctrl Pts',(-19.0264760932945,-16.8552961383495,
20.0912888007074));
#169625=CARTESIAN_POINT('Ctrl Pts',(-19.0309431718657,-16.8559241182242,
20.0910141988322));
#169626=CARTESIAN_POINT('Ctrl Pts',(-19.0389378162342,-16.8570740720078,
20.0905239744681));
#169627=CARTESIAN_POINT('Ctrl Pts',(-19.0424660887609,-16.8575906827378,
20.0903080542874));
#169628=CARTESIAN_POINT('Ctrl Pts',(-19.0501066447412,-16.8587291417745,
20.0898414121081));
#169629=CARTESIAN_POINT('Ctrl Pts',(-19.0542183931129,-16.8593541919041,
20.089590873572));
#169630=CARTESIAN_POINT('Ctrl Pts',(-19.065704759539,-16.8611349464289,
20.0888925480148));
#169631=CARTESIAN_POINT('Ctrl Pts',(-19.0730752303257,-16.8623175572134,
20.0884462582198));
#169632=CARTESIAN_POINT('Ctrl Pts',(-19.1159556285201,-16.8694306712002,
20.0858595223938));
#169633=CARTESIAN_POINT('Ctrl Pts',(-19.1513181919386,-16.8762276169945,
20.083765127398));
#169634=CARTESIAN_POINT('Ctrl Pts',(-19.2646840987895,-16.901031933425,
20.0771269191575));
#169635=CARTESIAN_POINT('Ctrl Pts',(-19.3418489569868,-16.9225623266271,
20.0727242248211));
#169636=CARTESIAN_POINT('Ctrl Pts',(-19.593408753145,-17.0083933092205,
20.0582339605817));
#169637=CARTESIAN_POINT('Ctrl Pts',(-19.7605250780659,-17.0912392324931,
20.0483000400703));
#169638=CARTESIAN_POINT('Ctrl Pts',(-19.9330199989337,-17.2071424343612,
20.0362131102457));
#169639=CARTESIAN_POINT('Ctrl Pts',(-19.9511593239992,-17.2197471292946,
20.0349182819175));
#169640=CARTESIAN_POINT('Ctrl Pts',(-19.9759653213987,-17.2375663780687,
20.0331128256876));
#169641=CARTESIAN_POINT('Ctrl Pts',(-19.9828033284739,-17.2425408027082,
20.0326114133183));
#169642=CARTESIAN_POINT('Ctrl Pts',(-19.9945041971574,-17.2511604714736,
20.0317469096588));
#169643=CARTESIAN_POINT('Ctrl Pts',(-19.9993815356592,-17.2547859590266,
20.0313845884453));
#169644=CARTESIAN_POINT('Ctrl Pts',(-20.0092368961525,-17.2621778718111,
20.0306484352683));
#169645=CARTESIAN_POINT('Ctrl Pts',(-20.0142140025671,-17.2659454123421,
20.0302745617791));
#169646=CARTESIAN_POINT('Ctrl Pts',(-20.0257427231244,-17.2747528325057,
20.0294035921968));
#169647=CARTESIAN_POINT('Ctrl Pts',(-20.0322815947566,-17.2798091552391,
20.0289058491875));
#169648=CARTESIAN_POINT('Ctrl Pts',(-20.0459650165516,-17.2905187939899,
20.0278562766694));
#169649=CARTESIAN_POINT('Ctrl Pts',(-20.0531030052954,-17.2961801849448,
20.0273041306485));
#169650=CARTESIAN_POINT('Ctrl Pts',(-20.0720088326311,-17.3113748974776,
20.0258292016242));
#169651=CARTESIAN_POINT('Ctrl Pts',(-20.0837111263355,-17.3209885898692,
20.0249032040786));
#169652=CARTESIAN_POINT('Ctrl Pts',(-20.1190845990346,-17.3506900790787,
20.02206357292));
#169653=CARTESIAN_POINT('Ctrl Pts',(-20.1424171217152,-17.3711730444877,
20.0201341054808));
#169654=CARTESIAN_POINT('Ctrl Pts',(-20.2894060406967,-17.5060483329457,
20.0076072380144));
#169655=CARTESIAN_POINT('Ctrl Pts',(-20.3994705267636,-17.63432960631,19.996420106974));
#169656=CARTESIAN_POINT('Ctrl Pts',(-20.5482438239332,-17.8565485344146,
19.9788036085486));
#169657=CARTESIAN_POINT('Ctrl Pts',(-20.5974983410433,-17.9426075318654,
19.9723513825577));
#169658=CARTESIAN_POINT('Ctrl Pts',(-20.6447646758537,-18.0405388980323,
19.9656328485742));
#169659=CARTESIAN_POINT('Ctrl Pts',(-20.648918712693,-18.0492988762204,
19.9650371755358));
#169660=CARTESIAN_POINT('Ctrl Pts',(-20.6549630923326,-18.0622746844772,
19.9641629690021));
#169661=CARTESIAN_POINT('Ctrl Pts',(-20.6568999800886,-18.066468517389,
19.9638816696384));
#169662=CARTESIAN_POINT('Ctrl Pts',(-20.6603117271959,-18.0739197560062,
19.96338413591));
#169663=CARTESIAN_POINT('Ctrl Pts',(-20.6617920753388,-18.0771745887519,
19.9631675666609));
#169664=CARTESIAN_POINT('Ctrl Pts',(-20.6649460104449,-18.0841560092352,
19.9627046797831));
#169665=CARTESIAN_POINT('Ctrl Pts',(-20.6666170550987,-18.0878836845945,
19.9624585183398));
#169666=CARTESIAN_POINT('Ctrl Pts',(-20.6711741824252,-18.0981288195111,
19.9617846298524));
#169667=CARTESIAN_POINT('Ctrl Pts',(-20.6740381863277,-18.1046561236399,
19.9613582347434));
#169668=CARTESIAN_POINT('Ctrl Pts',(-20.6891489338429,-18.139573026485,
19.9590923501057));
#169669=CARTESIAN_POINT('Ctrl Pts',(-20.70080629668,-18.1682154893823,19.9572865832381));
#169670=CARTESIAN_POINT('Ctrl Pts',(-20.7154850933187,-18.2066740726829,
19.9549187825041));
#169671=CARTESIAN_POINT('Ctrl Pts',(-20.7190678131875,-18.2162692972679,
19.9543326725714));
#169672=CARTESIAN_POINT('Ctrl Pts',(-20.7225805743325,-18.2258896093654,
19.9537493095993));
#169673=CARTESIAN_POINT('',(-20.8509996091575,-18.9532864007368,20.489056279057));
#169674=CARTESIAN_POINT('Ctrl Pts',(-20.7225805414791,-18.2258895193907,
19.7345260867578));
#169675=CARTESIAN_POINT('Ctrl Pts',(-20.6874528713457,-18.1296862512102,
19.7401269184544));
#169676=CARTESIAN_POINT('Ctrl Pts',(-20.6453764095337,-18.0361204043018,
19.7456315150547));
#169677=CARTESIAN_POINT('Ctrl Pts',(-20.5472452507785,-17.854436844477,
19.7569907277832));
#169678=CARTESIAN_POINT('Ctrl Pts',(-20.4911569404231,-17.7667157894665,
19.7628328457669));
#169679=CARTESIAN_POINT('Ctrl Pts',(-20.4204318628533,-17.6722210247135,
19.7697495964571));
#169680=CARTESIAN_POINT('Ctrl Pts',(-20.4118958804628,-17.6610499414193,
19.7705776882396));
#169681=CARTESIAN_POINT('Ctrl Pts',(-20.3980907440664,-17.6433513279784,
19.7719068005496));
#169682=CARTESIAN_POINT('Ctrl Pts',(-20.3928928721193,-17.6367685424178,
19.7724049994506));
#169683=CARTESIAN_POINT('Ctrl Pts',(-20.383631408929,-17.6251817134121,
19.7732888433485));
#169684=CARTESIAN_POINT('Ctrl Pts',(-20.3795838018406,-17.6201649874514,
19.7736738443173));
#169685=CARTESIAN_POINT('Ctrl Pts',(-20.3711396579048,-17.6097963221909,
19.7744744530363));
#169686=CARTESIAN_POINT('Ctrl Pts',(-20.3667396468177,-17.6044473234249,
19.7748901988436));
#169687=CARTESIAN_POINT('Ctrl Pts',(-20.3553245586717,-17.5907082312258,
19.7759651738961));
#169688=CARTESIAN_POINT('Ctrl Pts',(-20.3482706386027,-17.5823508103896,
19.7766259853985));
#169689=CARTESIAN_POINT('Ctrl Pts',(-20.31808827668,-17.5471480791616,19.7794392211317));
#169690=CARTESIAN_POINT('Ctrl Pts',(-20.2943536028448,-17.520832300646,
19.7816166541245));
#169691=CARTESIAN_POINT('Ctrl Pts',(-20.2303135476179,-17.4533153872665,
19.7874063674094));
#169692=CARTESIAN_POINT('Ctrl Pts',(-20.1889687607384,-17.4131449788479,
19.7910612098951));
#169693=CARTESIAN_POINT('Ctrl Pts',(-20.0462319705667,-17.2853622112502,
19.8033999413777));
#169694=CARTESIAN_POINT('Ctrl Pts',(-19.9381730377295,-17.205690623948,
19.8123263508122));
#169695=CARTESIAN_POINT('Ctrl Pts',(-19.7463729477041,-17.0905908192682,
19.8270271496118));
#169696=CARTESIAN_POINT('Ctrl Pts',(-19.6665527468826,-17.0493459947494,
19.8328476782571));
#169697=CARTESIAN_POINT('Ctrl Pts',(-19.575507996463,-17.0094124349534,
19.8389896805927));
#169698=CARTESIAN_POINT('Ctrl Pts',(-19.5666425075101,-17.0055959775086,
19.8395826821297));
#169699=CARTESIAN_POINT('Ctrl Pts',(-19.553503339794,-17.0000459692206,
19.8404537305182));
#169700=CARTESIAN_POINT('Ctrl Pts',(-19.5492497454052,-16.9982655974378,
19.8407345150701));
#169701=CARTESIAN_POINT('Ctrl Pts',(-19.5416882445545,-16.9951296724862,
19.8412314805884));
#169702=CARTESIAN_POINT('Ctrl Pts',(-19.5383826918266,-16.9937685875106,
19.8414479935852));
#169703=CARTESIAN_POINT('Ctrl Pts',(-19.5312874495523,-16.9908680682834,
19.841911139503));
#169704=CARTESIAN_POINT('Ctrl Pts',(-19.5274967521628,-16.9893312465497,
19.8421576142544));
#169705=CARTESIAN_POINT('Ctrl Pts',(-19.5170660144579,-16.9851375835843,
19.8428332436832));
#169706=CARTESIAN_POINT('Ctrl Pts',(-19.5104168572306,-16.9825033599321,
19.84326105494));
#169707=CARTESIAN_POINT('Ctrl Pts',(-19.4746420408568,-16.9685396355155,
19.8455480814061));
#169708=CARTESIAN_POINT('Ctrl Pts',(-19.4452799012861,-16.9578217767478,
19.8473728240998));
#169709=CARTESIAN_POINT('Ctrl Pts',(-19.2606291227351,-16.8950177553075,
19.8585873066993));
#169710=CARTESIAN_POINT('Ctrl Pts',(-19.0999558447015,-16.8604448758089,
19.8672421922195));
#169711=CARTESIAN_POINT('Ctrl Pts',(-18.8202504708911,-16.8335146080889,
19.8826237010964));
#169712=CARTESIAN_POINT('Ctrl Pts',(-18.702897242282,-16.8319889566493,
19.8891640627748));
#169713=CARTESIAN_POINT('Ctrl Pts',(-18.5717696808636,-16.8411767827914,
19.89686474355));
#169714=CARTESIAN_POINT('Ctrl Pts',(-18.557520965006,-16.8423202930212,
19.8977065146238));
#169715=CARTESIAN_POINT('Ctrl Pts',(-18.5348635405685,-16.8443697727556,
19.8990534368197));
#169716=CARTESIAN_POINT('Ctrl Pts',(-18.5264466389595,-16.8451819956567,
19.8995556443727));
#169717=CARTESIAN_POINT('Ctrl Pts',(-18.5116115646932,-16.8467033279711,
19.9004441463527));
#169718=CARTESIAN_POINT('Ctrl Pts',(-18.5051913110712,-16.8473914197982,
19.9008297743207));
#169719=CARTESIAN_POINT('Ctrl Pts',(-18.4919194257524,-16.8488752835143,
19.9016292707508));
#169720=CARTESIAN_POINT('Ctrl Pts',(-18.4850683420084,-16.8496751903146,
19.9020432653503));
#169721=CARTESIAN_POINT('Ctrl Pts',(-18.467494003228,-16.8518142143035,
19.9031085997143));
#169722=CARTESIAN_POINT('Ctrl Pts',(-18.4567769684261,-16.8532019714273,
19.9037614680075));
#169723=CARTESIAN_POINT('Ctrl Pts',(-18.4121029153976,-16.8593349870864,
19.9064966798583));
#169724=CARTESIAN_POINT('Ctrl Pts',(-18.3782546313789,-16.8648225743609,
19.9086023366605));
#169725=CARTESIAN_POINT('Ctrl Pts',(-18.2904311408629,-16.8812591230351,
19.9141559393124));
#169726=CARTESIAN_POINT('Ctrl Pts',(-18.2367261389649,-16.8934959314496,
19.9176422555395));
#169727=CARTESIAN_POINT('Ctrl Pts',(-18.0779620642814,-16.9362462346191,
19.9282103144687));
#169728=CARTESIAN_POINT('Ctrl Pts',(-17.9747308797145,-16.9728193735862,
19.9354404529297));
#169729=CARTESIAN_POINT('Ctrl Pts',(-17.8336085213,-17.03548881982,19.9456405414657));
#169730=CARTESIAN_POINT('Ctrl Pts',(-17.7930149545006,-17.0550900800902,
19.9486120582263));
#169731=CARTESIAN_POINT('Ctrl Pts',(-17.7315247515292,-17.0872416036616,
19.9531456726464));
#169732=CARTESIAN_POINT('Ctrl Pts',(-17.7101675392357,-17.0988816399811,
19.9547264897884));
#169733=CARTESIAN_POINT('Ctrl Pts',(-17.6764326838586,-17.118028982989,
19.9572285006724));
#169734=CARTESIAN_POINT('Ctrl Pts',(-17.6639235343898,-17.125299506022,
19.9581573866627));
#169735=CARTESIAN_POINT('Ctrl Pts',(-17.6195647019962,-17.1516936347483,
19.9614528844623));
#169736=CARTESIAN_POINT('Ctrl Pts',(-17.5881429798286,-17.1715278381798,
19.9637902390719));
#169737=CARTESIAN_POINT('Ctrl Pts',(-17.5513021557437,-17.1961622703615,
19.9665195003504));
#169738=CARTESIAN_POINT('Ctrl Pts',(-17.5453669772867,-17.2001747049735,
19.9669588353227));
#169739=CARTESIAN_POINT('Ctrl Pts',(-17.5357212599401,-17.2067672123169,
19.9676720954521));
#169740=CARTESIAN_POINT('Ctrl Pts',(-17.5319984685038,-17.2093291357115,
19.9679471997032));
#169741=CARTESIAN_POINT('Ctrl Pts',(-17.5253523535291,-17.2139342398943,
19.9684379640804));
#169742=CARTESIAN_POINT('Ctrl Pts',(-17.5224259733483,-17.2159728981589,
19.9686539247014));
#169743=CARTESIAN_POINT('Ctrl Pts',(-17.5161031271706,-17.2204014743542,
19.9691202496244));
#169744=CARTESIAN_POINT('Ctrl Pts',(-17.512708548118,-17.2227939865051,
19.9693704326359));
#169745=CARTESIAN_POINT('Ctrl Pts',(-17.5032547022296,-17.229498818016,
19.9700667645002));
#169746=CARTESIAN_POINT('Ctrl Pts',(-17.497211017662,-17.2338331493093,
19.9705114299368));
#169747=CARTESIAN_POINT('Ctrl Pts',(-17.4624098105271,-17.2590702037981,
19.9730698971643));
#169748=CARTESIAN_POINT('Ctrl Pts',(-17.4341577892071,-17.2806641666623,
19.9751388159078));
#169749=CARTESIAN_POINT('Ctrl Pts',(-17.3454026609008,-17.352115394916,
19.9816596593925));
#169750=CARTESIAN_POINT('Ctrl Pts',(-17.2871162323678,-17.4046271959472,
19.9859761467133));
#169751=CARTESIAN_POINT('Ctrl Pts',(-17.0992045780821,-17.593846606142,
20.0005222676099));
#169752=CARTESIAN_POINT('Ctrl Pts',(-16.9849636737446,-17.7445220969915,
20.0105785088926));
#169753=CARTESIAN_POINT('Ctrl Pts',(-16.8813887038695,-17.9273064227458,
20.022800862881));
#169754=CARTESIAN_POINT('Ctrl Pts',(-16.8709212628747,-17.9464637705268,
20.024080782655));
#169755=CARTESIAN_POINT('Ctrl Pts',(-16.8568320153054,-17.9732251689446,
20.0258686990049));
#169756=CARTESIAN_POINT('Ctrl Pts',(-16.8529562855613,-17.9806945104997,
20.0263677156111));
#169757=CARTESIAN_POINT('Ctrl Pts',(-16.8463633348376,-17.9935879683895,
20.0272291852752));
#169758=CARTESIAN_POINT('Ctrl Pts',(-16.8436246879338,-17.9990010596264,
20.0275908806638));
#169759=CARTESIAN_POINT('Ctrl Pts',(-16.8380199428566,-18.0101983784794,
20.0283391517862));
#169760=CARTESIAN_POINT('Ctrl Pts',(-16.8351569621256,-18.0159840880259,
20.0287258317863));
#169761=CARTESIAN_POINT('Ctrl Pts',(-16.8285446692681,-18.0295018568292,
20.0296294206712));
#169762=CARTESIAN_POINT('Ctrl Pts',(-16.8248159040004,-18.0372437888982,
20.0301470383833));
#169763=CARTESIAN_POINT('Ctrl Pts',(-16.8129860181424,-18.0621932751953,
20.0318156182407));
#169764=CARTESIAN_POINT('Ctrl Pts',(-16.8050697911191,-18.0794869982543,
20.0329729368148));
#169765=CARTESIAN_POINT('Ctrl Pts',(-16.7664422086887,-18.1669683439524,
20.0388325837442));
#169766=CARTESIAN_POINT('Ctrl Pts',(-16.7393271200857,-18.2386724539092,
20.043655426877));
#169767=CARTESIAN_POINT('Ctrl Pts',(-16.6828933440818,-18.4165126865405,
20.0556550719475));
#169768=CARTESIAN_POINT('Ctrl Pts',(-16.6578495633768,-18.5237698133059,
20.0629300907546));
#169769=CARTESIAN_POINT('Ctrl Pts',(-16.6304745517221,-18.7030651948591,
20.0749094501698));
#169770=CARTESIAN_POINT('Ctrl Pts',(-16.6232748135076,-18.7741571841864,
20.0796099927936));
#169771=CARTESIAN_POINT('Ctrl Pts',(-16.6173234463805,-18.8922862261699,
20.0872201671401));
#169772=CARTESIAN_POINT('Ctrl Pts',(-16.6165200639996,-18.9391617433935,
20.0901875453526));
#169773=CARTESIAN_POINT('Ctrl Pts',(-16.6173969601522,-18.993707969292,
20.093550872544));
#169774=CARTESIAN_POINT('Ctrl Pts',(-16.617562198295,-19.0013864213163,
20.0940222534842));
#169775=CARTESIAN_POINT('Ctrl Pts',(-16.6178938788572,-19.0136868803939,
20.0947738746448));
#169776=CARTESIAN_POINT('Ctrl Pts',(-16.6180336854372,-19.0183094542451,
20.0950555442425));
#169777=CARTESIAN_POINT('Ctrl Pts',(-16.6183087667263,-19.0265148275123,
20.0955540730967));
#169778=CARTESIAN_POINT('Ctrl Pts',(-16.6184379964238,-19.0300977836996,
20.0957712668605));
#169779=CARTESIAN_POINT('Ctrl Pts',(-16.6187320247361,-19.037712754986,
20.0962318134139));
#169780=CARTESIAN_POINT('Ctrl Pts',(-16.6188992490171,-19.0417446230268,
20.0964750290214));
#169781=CARTESIAN_POINT('Ctrl Pts',(-16.6193837843089,-19.0526723023102,
20.0971325791456));
#169782=CARTESIAN_POINT('Ctrl Pts',(-16.61972330015,-19.0595671491852,20.0975456874863));
#169783=CARTESIAN_POINT('Ctrl Pts',(-16.6216091496217,-19.0943958454679,
20.0996240509918));
#169784=CARTESIAN_POINT('Ctrl Pts',(-16.6236754513212,-19.122300181698,
20.1012618532593));
#169785=CARTESIAN_POINT('Ctrl Pts',(-16.6313320027011,-19.2037394886876,
20.1059829262815));
#169786=CARTESIAN_POINT('Ctrl Pts',(-16.6384114199252,-19.2571143661314,
20.1090026672967));
#169787=CARTESIAN_POINT('Ctrl Pts',(-16.6713309287523,-19.4488863426291,
20.1197625732026));
#169788=CARTESIAN_POINT('Ctrl Pts',(-16.7089186590469,-19.5848881569915,
20.1272454922137));
#169789=CARTESIAN_POINT('Ctrl Pts',(-16.7925855979229,-19.8010498797979,
20.1400721858099));
#169790=CARTESIAN_POINT('Ctrl Pts',(-16.8308817460597,-19.8837261216597,
20.1452182594085));
#169791=CARTESIAN_POINT('Ctrl Pts',(-16.8809429791038,-19.9757468040221,
20.1513597057753));
#169792=CARTESIAN_POINT('Ctrl Pts',(-16.8876272709988,-19.9877536259923,
20.1521693788542));
#169793=CARTESIAN_POINT('Ctrl Pts',(-16.8985329186672,-20.0069020791808,
20.1534744781851));
#169794=CARTESIAN_POINT('Ctrl Pts',(-16.9026802493365,-20.014085576193,
20.1539672431839));
#169795=CARTESIAN_POINT('Ctrl Pts',(-16.9101181252263,-20.026795456499,
20.15484481216));
#169796=CARTESIAN_POINT('Ctrl Pts',(-16.9133918572463,-20.0323315951911,
20.1552290023748));
#169797=CARTESIAN_POINT('Ctrl Pts',(-16.920264496237,-20.0438338097025,
20.1560313138591));
#169798=CARTESIAN_POINT('Ctrl Pts',(-16.9238677257642,-20.049797200572,
20.1564495900041));
#169799=CARTESIAN_POINT('Ctrl Pts',(-16.9332997739112,-20.0652346690286,
20.1575384654385));
#169800=CARTESIAN_POINT('Ctrl Pts',(-16.9391738857544,-20.0746806958294,
20.1582107256199));
#169801=CARTESIAN_POINT('Ctrl Pts',(-16.9649894067295,-20.1154735916245,
20.1611403459296));
#169802=CARTESIAN_POINT('Ctrl Pts',(-16.9856786284744,-20.1463372158215,
20.1634253634136));
#169803=CARTESIAN_POINT('Ctrl Pts',(-17.0427802356745,-20.2268547124876,
20.1695754983652));
#169804=CARTESIAN_POINT('Ctrl Pts',(-17.0805627792012,-20.27548897554,20.1734900625096));
#169805=CARTESIAN_POINT('Ctrl Pts',(-17.2176828067909,-20.4369418703856,
20.1871730860358));
#169806=CARTESIAN_POINT('Ctrl Pts',(-17.3268663024046,-20.5407855280383,
20.1972435375032));
#169807=CARTESIAN_POINT('Ctrl Pts',(-17.5000731974876,-20.6735503208341,
20.2114657080261));
#169808=CARTESIAN_POINT('Ctrl Pts',(-17.5559969615214,-20.7122902158823,
20.2158241259982));
#169809=CARTESIAN_POINT('Ctrl Pts',(-17.621585001016,-20.7531963703818,
20.2205966389122));
#169810=CARTESIAN_POINT('Ctrl Pts',(-17.6295087770583,-20.758066067549,
20.221167784964));
#169811=CARTESIAN_POINT('Ctrl Pts',(-17.6413497800566,-20.7652360923487,
20.2220129377211));
#169812=CARTESIAN_POINT('Ctrl Pts',(-17.6452426111969,-20.7675762112767,
20.2222894567441));
#169813=CARTESIAN_POINT('Ctrl Pts',(-17.652207156455,-20.7717323914563,
20.2227817516946));
#169814=CARTESIAN_POINT('Ctrl Pts',(-17.6552759503767,-20.7735532268517,
20.2229978359914));
#169815=CARTESIAN_POINT('Ctrl Pts',(-17.6619121768641,-20.7774681071625,
20.2234633060435));
#169816=CARTESIAN_POINT('Ctrl Pts',(-17.6654811363374,-20.7795594516879,
20.2237125165007));
#169817=CARTESIAN_POINT('Ctrl Pts',(-17.6754189477816,-20.7853437635344,
20.2244034058939));
#169818=CARTESIAN_POINT('Ctrl Pts',(-17.6818010391035,-20.7890140308966,
20.2248436388042));
#169819=CARTESIAN_POINT('Ctrl Pts',(-17.7180746128179,-20.8096234901797,
20.2273269816597));
#169820=CARTESIAN_POINT('Ctrl Pts',(-17.7483576777707,-20.8258673756419,
20.2293282352224));
#169821=CARTESIAN_POINT('Ctrl Pts',(-17.845167782707,-20.874799753902,20.235544061566));
#169822=CARTESIAN_POINT('Ctrl Pts',(-17.9130262181056,-20.9047379090595,
20.2396373940959));
#169823=CARTESIAN_POINT('Ctrl Pts',(-18.1646960184479,-21.0003264703336,
20.2543461995866));
#169824=CARTESIAN_POINT('Ctrl Pts',(-18.3557503211861,-21.0440493740088,
20.2647305712193));
#169825=CARTESIAN_POINT('Ctrl Pts',(-18.5710172382166,-21.0628213983424,
20.2773123779564));
#169826=CARTESIAN_POINT('Ctrl Pts',(-18.5919717205753,-21.064334792938,
20.2785448561205));
#169827=CARTESIAN_POINT('Ctrl Pts',(-18.6212107689498,-21.0660094940934,
20.2802766793572));
#169828=CARTESIAN_POINT('Ctrl Pts',(-18.6294794356704,-21.0664344398512,
20.2807677725091));
#169829=CARTESIAN_POINT('Ctrl Pts',(-18.6437752406276,-21.0670850734583,
20.2816192302153));
#169830=CARTESIAN_POINT('Ctrl Pts',(-18.649801282694,-21.0673335316246,
20.2819788777301));
#169831=CARTESIAN_POINT('Ctrl Pts',(-18.6623001742401,-21.067795377132,
20.2827264010955));
#169832=CARTESIAN_POINT('Ctrl Pts',(-18.6687730985218,-21.0680048187054,
20.2831143967306));
#169833=CARTESIAN_POINT('Ctrl Pts',(-18.6839663537912,-21.0684266401192,
20.2840271820159));
#169834=CARTESIAN_POINT('Ctrl Pts',(-18.6926871898646,-21.0686148296087,
20.2845527242529));
#169835=CARTESIAN_POINT('Ctrl Pts',(-18.7211448221247,-21.0690529860537,
20.286273041614));
#169836=CARTESIAN_POINT('Ctrl Pts',(-18.7408835413631,-21.0690808148962,
20.287474738067));
#169837=CARTESIAN_POINT('Ctrl Pts',(-18.8426899691093,-21.06780059505,20.2937180913376));
#169838=CARTESIAN_POINT('Ctrl Pts',(-18.9246215312924,-21.0619967595135,
20.2988987108291));
#169839=CARTESIAN_POINT('Ctrl Pts',(-19.1014577366167,-21.0390861545677,
20.3104043008588));
#169840=CARTESIAN_POINT('Ctrl Pts',(-19.1959536109683,-21.0202239775568,
20.316760858635));
#169841=CARTESIAN_POINT('Ctrl Pts',(-19.408567270004,-20.9624830253628,
20.3313187746994));
#169842=CARTESIAN_POINT('Ctrl Pts',(-19.5252266600362,-20.919498513639,
20.3394986164437));
#169843=CARTESIAN_POINT('Ctrl Pts',(-19.6459813842652,-20.8625150512887,
20.3477444034768));
#169844=CARTESIAN_POINT('Ctrl Pts',(-19.6544770805945,-20.8584364028467,
20.3483232252808));
#169845=CARTESIAN_POINT('Ctrl Pts',(-19.667048763378,-20.8522973076676,
20.3491774844709));
#169846=CARTESIAN_POINT('Ctrl Pts',(-19.6711456406842,-20.8502802483878,
20.3494555123114));
#169847=CARTESIAN_POINT('Ctrl Pts',(-19.6784341736302,-20.8466624607093,
20.3499494521817));
#169848=CARTESIAN_POINT('Ctrl Pts',(-19.6816283298214,-20.8450669025439,
20.3501656809456));
#169849=CARTESIAN_POINT('Ctrl Pts',(-19.6884253704846,-20.8416501022892,
20.3506252931843));
#169850=CARTESIAN_POINT('Ctrl Pts',(-19.6920270743343,-20.8398266399154,
20.350868534611));
#169851=CARTESIAN_POINT('Ctrl Pts',(-19.7018628016953,-20.8348116329862,
20.3515320190684));
#169852=CARTESIAN_POINT('Ctrl Pts',(-19.708086303349,-20.8315994054487,
20.3519509839734));
#169853=CARTESIAN_POINT('Ctrl Pts',(-19.7219629531984,-20.8243496126087,
20.3528835050296));
#169854=CARTESIAN_POINT('Ctrl Pts',(-19.7296075627843,-20.8202958692774,
20.353396097376));
#169855=CARTESIAN_POINT('Ctrl Pts',(-19.7531083550483,-20.8076487849892,
20.3549690551881));
#169856=CARTESIAN_POINT('Ctrl Pts',(-19.7688801489266,-20.7988993946727,
20.3560206888475));
#169857=CARTESIAN_POINT('Ctrl Pts',(-19.8292097129774,-20.7644161006235,
20.3600352851188));
#169858=CARTESIAN_POINT('Ctrl Pts',(-19.8729380917612,-20.7372610939267,
20.3629281934109));
#169859=CARTESIAN_POINT('Ctrl Pts',(-20.029494426291,-20.6319444752037,
20.3733821140651));
#169860=CARTESIAN_POINT('Ctrl Pts',(-20.1356376904219,-20.5444614472474,
20.3806823136807));
#169861=CARTESIAN_POINT('Ctrl Pts',(-20.3014488632376,-20.3782896964381,
20.3936323161404));
#169862=CARTESIAN_POINT('Ctrl Pts',(-20.3654679332443,-20.3045927518625,
20.3991276302478));
#169863=CARTESIAN_POINT('Ctrl Pts',(-20.4325704368393,-20.2156224953328,
20.4056590619318));
#169864=CARTESIAN_POINT('Ctrl Pts',(-20.4408544633794,-20.2044101431239,
20.4064802772414));
#169865=CARTESIAN_POINT('Ctrl Pts',(-20.453924079103,-20.1863500052783,
20.4078004313522));
#169866=CARTESIAN_POINT('Ctrl Pts',(-20.4587810067739,-20.179554173562,
20.4082966089618));
#169867=CARTESIAN_POINT('Ctrl Pts',(-20.4673114115778,-20.1674678244488,
20.4091781163726));
#169868=CARTESIAN_POINT('Ctrl Pts',(-20.4710012225956,-20.1621889245329,
20.4095628134441));
#169869=CARTESIAN_POINT('Ctrl Pts',(-20.4786175055421,-20.1511859492998,
20.4103640381269));
#169870=CARTESIAN_POINT('Ctrl Pts',(-20.4825400239823,-20.1454592428685,
20.4107807099763));
#169871=CARTESIAN_POINT('Ctrl Pts',(-20.4926083156445,-20.1306037909207,
20.4118607634172));
#169872=CARTESIAN_POINT('Ctrl Pts',(-20.4987111411793,-20.1214463155108,
20.4125257557873));
#169873=CARTESIAN_POINT('Ctrl Pts',(-20.5245008363533,-20.0820865016081,
20.4153809048838));
#169874=CARTESIAN_POINT('Ctrl Pts',(-20.5434849140851,-20.0514329633956,
20.4175970072924));
#169875=CARTESIAN_POINT('Ctrl Pts',(-20.5914634161642,-19.9693509097231,
20.4235153408445));
#169876=CARTESIAN_POINT('Ctrl Pts',(-20.6191038822203,-19.9171712668829,
20.4272625224157));
#169877=CARTESIAN_POINT('Ctrl Pts',(-20.7103212337429,-19.7260631148771,
20.4409158349975));
#169878=CARTESIAN_POINT('Ctrl Pts',(-20.761002043115,-19.5815043387839,
20.4511527917293));
#169879=CARTESIAN_POINT('Ctrl Pts',(-20.8019773180527,-19.4057911539328,
20.4629187022516));
#169880=CARTESIAN_POINT('Ctrl Pts',(-20.8077392224272,-19.378687636761,
20.4647138326753));
#169881=CARTESIAN_POINT('Ctrl Pts',(-20.8211288655409,-19.3090051099935,
20.4692668387034));
#169882=CARTESIAN_POINT('Ctrl Pts',(-20.8279872927794,-19.2662886519038,
20.4719989986381));
#169883=CARTESIAN_POINT('Ctrl Pts',(-20.8344943174084,-19.2159486775211,
20.4751271999216));
#169884=CARTESIAN_POINT('Ctrl Pts',(-20.8354165124151,-19.208503269007,
20.4755875273787));
#169885=CARTESIAN_POINT('Ctrl Pts',(-20.8368427989704,-19.1964637388768,
20.4763279424358));
#169886=CARTESIAN_POINT('Ctrl Pts',(-20.8373714508299,-19.1918726695058,
20.4766093594304));
#169887=CARTESIAN_POINT('Ctrl Pts',(-20.8382824835703,-19.1837261659555,
20.4771070231343));
#169888=CARTESIAN_POINT('Ctrl Pts',(-20.8386708939738,-19.180171460507,
20.4773236053863));
#169889=CARTESIAN_POINT('Ctrl Pts',(-20.8394063448191,-19.1732789727038,
20.4777424356568));
#169890=CARTESIAN_POINT('Ctrl Pts',(-20.8397544539967,-19.1699413691777,
20.4779447451182));
#169891=CARTESIAN_POINT('Ctrl Pts',(-20.8405037112363,-19.1625882231517,
20.4783893752405));
#169892=CARTESIAN_POINT('Ctrl Pts',(-20.8409013174799,-19.1585723219416,
20.4786314984297));
#169893=CARTESIAN_POINT('Ctrl Pts',(-20.8418560162692,-19.148640095738,
20.4792286215703));
#169894=CARTESIAN_POINT('Ctrl Pts',(-20.842399689828,-19.14272247474,20.4795828954843));
#169895=CARTESIAN_POINT('Ctrl Pts',(-20.844583901369,-19.117796825005,20.48106914855));
#169896=CARTESIAN_POINT('Ctrl Pts',(-20.8459924221905,-19.0987687150597,
20.4821890985016));
#169897=CARTESIAN_POINT('Ctrl Pts',(-20.8496863090821,-19.0376545415139,
20.4857465687598));
#169898=CARTESIAN_POINT('Ctrl Pts',(-20.8509723412701,-18.9955169026794,
20.4881393720512));
#169899=CARTESIAN_POINT('Ctrl Pts',(-20.8509995586429,-18.9533670061129,
20.490497217366));
#169900=CARTESIAN_POINT('Ctrl Pts',(-20.7225805737622,-18.2258896078036,
20.5336910569984));
#169901=CARTESIAN_POINT('Ctrl Pts',(-20.7472974566424,-18.2935811236775,
20.5293719648838));
#169902=CARTESIAN_POINT('Ctrl Pts',(-20.7685452928513,-18.3625125368533,
20.5250528727692));
#169903=CARTESIAN_POINT('Ctrl Pts',(-20.7862157788573,-18.4322891217137,
20.5207337806546));
#169904=CARTESIAN_POINT('Ctrl Pts',(-20.803893991431,-18.502096216969,20.5164127999808));
#169905=CARTESIAN_POINT('Ctrl Pts',(-20.8179916434005,-18.5727487327075,
20.5120918193071));
#169906=CARTESIAN_POINT('Ctrl Pts',(-20.8284516637963,-18.6438422027255,
20.5077708386333));
#169907=CARTESIAN_POINT('Ctrl Pts',(-20.8389271742135,-18.7150409535491,
20.5034434591113));
#169908=CARTESIAN_POINT('Ctrl Pts',(-20.8457542576745,-18.7866814680688,
20.4991160795893));
#169909=CARTESIAN_POINT('Ctrl Pts',(-20.8489278328486,-18.8583556630536,
20.4947887000673));
#169910=CARTESIAN_POINT('Ctrl Pts',(-20.8503291635241,-18.8900042746542,
20.4928778930639));
#169911=CARTESIAN_POINT('Ctrl Pts',(-20.8510188273478,-18.9216594744888,
20.4909670860604));
#169912=CARTESIAN_POINT('Ctrl Pts',(-20.8509996091575,-18.9532864007368,
20.489056279057));
#169913=CARTESIAN_POINT('Origin',(-18.734,-18.952,0.));
#169914=CARTESIAN_POINT('',(-20.7225805737622,-18.2258896078036,21.5555703780636));
#169915=CARTESIAN_POINT('',(-20.7225805737622,-18.2258896078036,21.3335535462005));
#169916=CARTESIAN_POINT('',(-20.7225805737622,-18.2258896078036,0.));
#169917=CARTESIAN_POINT('',(-20.8509993841958,-18.953614718169,21.5109437210328));
#169918=CARTESIAN_POINT('Ctrl Pts',(-20.8509993841958,-18.953614718169,
21.5109437210328));
#169919=CARTESIAN_POINT('Ctrl Pts',(-20.8510540300824,-18.8819704457194,
21.5152671815625));
#169920=CARTESIAN_POINT('Ctrl Pts',(-20.8474675421558,-18.8101916547056,
21.5195906420923));
#169921=CARTESIAN_POINT('Ctrl Pts',(-20.840225458876,-18.7386849363444,
21.523914102622));
#169922=CARTESIAN_POINT('Ctrl Pts',(-20.83299097412,-18.6672532441145,21.5282330268994));
#169923=CARTESIAN_POINT('Ctrl Pts',(-20.8221085457459,-18.5960935495738,
21.5325519511768));
#169924=CARTESIAN_POINT('Ctrl Pts',(-20.807615734365,-18.525611930052,21.5368708754542));
#169925=CARTESIAN_POINT('Ctrl Pts',(-20.7931333503066,-18.4551810208142,
21.5411866923416));
#169926=CARTESIAN_POINT('Ctrl Pts',(-20.7750458352844,-18.3854277039634,
21.5455025092291));
#169927=CARTESIAN_POINT('Ctrl Pts',(-20.7534422763024,-18.316750527208,
21.5498183261165));
#169928=CARTESIAN_POINT('Ctrl Pts',(-20.7438446499629,-18.2862399117533,
21.5517356767656));
#169929=CARTESIAN_POINT('Ctrl Pts',(-20.7335537446294,-18.2559415594814,
21.5536530274146));
#169930=CARTESIAN_POINT('Ctrl Pts',(-20.7225805737622,-18.2258896078036,
21.5555703780636));
#169931=CARTESIAN_POINT('Ctrl Pts',(-20.8509994311328,-18.953551961105,
21.509989519712));
#169932=CARTESIAN_POINT('Ctrl Pts',(-20.8509485267258,-19.022989655363,
21.5054226551334));
#169933=CARTESIAN_POINT('Ctrl Pts',(-20.8474812907043,-19.0923897728265,
21.500900987759));
#169934=CARTESIAN_POINT('Ctrl Pts',(-20.8382974849423,-19.1847367233776,
21.4950377275334));
#169935=CARTESIAN_POINT('Ctrl Pts',(-20.8356021939193,-19.2079347726058,
21.4935780223835));
#169936=CARTESIAN_POINT('Ctrl Pts',(-20.8317147194992,-19.2371659041953,
21.4917592813289));
#169937=CARTESIAN_POINT('Ctrl Pts',(-20.8308795084294,-19.2432438265875,
21.4913822453896));
#169938=CARTESIAN_POINT('Ctrl Pts',(-20.8294396375592,-19.25339455379,21.4907545413536));
#169939=CARTESIAN_POINT('Ctrl Pts',(-20.8288495023032,-19.2574693357115,
21.4905030984012));
#169940=CARTESIAN_POINT('Ctrl Pts',(-20.8277537589393,-19.2648827230509,
21.4900466455369));
#169941=CARTESIAN_POINT('Ctrl Pts',(-20.8272520454091,-19.2682218781408,
21.4898414207734));
#169942=CARTESIAN_POINT('Ctrl Pts',(-20.8262054097198,-19.2750761148474,
21.4894209425127));
#169943=CARTESIAN_POINT('Ctrl Pts',(-20.8256596197261,-19.2785910105254,
21.489205745317));
#169944=CARTESIAN_POINT('Ctrl Pts',(-20.8244066869482,-19.286527930997,
21.4887207763407));
#169945=CARTESIAN_POINT('Ctrl Pts',(-20.8236943731061,-19.2909490836633,
21.4884513018776));
#169946=CARTESIAN_POINT('Ctrl Pts',(-20.8214990062823,-19.3043051658924,
21.4876391708809));
#169947=CARTESIAN_POINT('Ctrl Pts',(-20.8199726159162,-19.313233004385,
21.4870989280484));
#169948=CARTESIAN_POINT('Ctrl Pts',(-20.8078182965081,-19.3816762404416,
21.4829755341491));
#169949=CARTESIAN_POINT('Ctrl Pts',(-20.7947015599908,-19.4407274473077,
21.4795238028164));
#169950=CARTESIAN_POINT('Ctrl Pts',(-20.7741842858873,-19.517415715384,
21.4750859567501));
#169951=CARTESIAN_POINT('Ctrl Pts',(-20.7690503570717,-19.5356239562734,
21.4740356752781));
#169952=CARTESIAN_POINT('Ctrl Pts',(-20.752036519566,-19.5930097141763,
21.4707296572627));
#169953=CARTESIAN_POINT('Ctrl Pts',(-20.7392637897188,-19.6319133317566,
21.4684943567092));
#169954=CARTESIAN_POINT('Ctrl Pts',(-20.7134200740027,-19.703548601181,
21.4643516799029));
#169955=CARTESIAN_POINT('Ctrl Pts',(-20.700644664369,-19.7363710280158,
21.4624428384245));
#169956=CARTESIAN_POINT('Ctrl Pts',(-20.6589738879128,-19.8360030588782,
21.45657927303));
#169957=CARTESIAN_POINT('Ctrl Pts',(-20.6274484736872,-19.9016515661354,
21.4526164834016));
#169958=CARTESIAN_POINT('Ctrl Pts',(-20.5661674190936,-20.0140269091526,
21.4455035225684));
#169959=CARTESIAN_POINT('Ctrl Pts',(-20.5378432111702,-20.0614537505821,
21.4423911736075));
#169960=CARTESIAN_POINT('Ctrl Pts',(-20.4889701482696,-20.1364600956493,
21.4372424305058));
#169961=CARTESIAN_POINT('Ctrl Pts',(-20.4695463826916,-20.1647425511322,
21.4352459081717));
#169962=CARTESIAN_POINT('Ctrl Pts',(-20.4431384531694,-20.2012600073017,
21.4325885793575));
#169963=CARTESIAN_POINT('Ctrl Pts',(-20.4367657948285,-20.2099322157393,
21.4319514664983));
#169964=CARTESIAN_POINT('Ctrl Pts',(-20.4262255532679,-20.2240490093817,
21.4309042295645));
#169965=CARTESIAN_POINT('Ctrl Pts',(-20.4220971023159,-20.2295226717532,
21.4304956466839));
#169966=CARTESIAN_POINT('Ctrl Pts',(-20.4140583306678,-20.2400737850873,
21.4297031032962));
#169967=CARTESIAN_POINT('Ctrl Pts',(-20.410151395252,-20.2451537298637,
21.4293192798396));
#169968=CARTESIAN_POINT('Ctrl Pts',(-20.4010835076038,-20.2568340039861,
21.4284315172956));
#169969=CARTESIAN_POINT('Ctrl Pts',(-20.3959063430362,-20.2634215581138,
21.4279269323589));
#169970=CARTESIAN_POINT('Ctrl Pts',(-20.381893156061,-20.2810360464795,
21.426567108629));
#169971=CARTESIAN_POINT('Ctrl Pts',(-20.3729857267863,-20.2920053875725,
21.4257089935978));
#169972=CARTESIAN_POINT('Ctrl Pts',(-20.2682886291546,-20.4183322891219,
21.4156928769048));
#169973=CARTESIAN_POINT('Ctrl Pts',(-20.1606324264817,-20.5232656833021,
21.4060183990526));
#169974=CARTESIAN_POINT('Ctrl Pts',(-19.9681077757239,-20.6747021725785,
21.3898620876248));
#169975=CARTESIAN_POINT('Ctrl Pts',(-19.8895203929384,-20.7283721356634,
21.3835369424866));
#169976=CARTESIAN_POINT('Ctrl Pts',(-19.7687964020942,-20.799406702276,
21.3744151972906));
#169977=CARTESIAN_POINT('Ctrl Pts',(-19.7292807463733,-20.8209922089922,
21.3715174048873));
#169978=CARTESIAN_POINT('Ctrl Pts',(-19.667082796194,-20.852435315658,21.3671222453147));
#169979=CARTESIAN_POINT('Ctrl Pts',(-19.6448669637259,-20.8631827207263,
21.3655841186835));
#169980=CARTESIAN_POINT('Ctrl Pts',(-19.6165112336334,-20.8762936314066,
21.3636654433987));
#169981=CARTESIAN_POINT('Ctrl Pts',(-19.6105424043741,-20.8790198424845,
21.3632640343944));
#169982=CARTESIAN_POINT('Ctrl Pts',(-19.6014988122009,-20.8830997114459,
21.3626596782316));
#169983=CARTESIAN_POINT('Ctrl Pts',(-19.5984334106001,-20.8844738455462,
21.3624554896844));
#169984=CARTESIAN_POINT('Ctrl Pts',(-19.5921218303903,-20.8872851280853,
21.3620364532144));
#169985=CARTESIAN_POINT('Ctrl Pts',(-19.5888753552478,-20.8887213867573,
21.3618216677972));
#169986=CARTESIAN_POINT('Ctrl Pts',(-19.5815844043418,-20.8919250393223,
21.3613409679369));
#169987=CARTESIAN_POINT('Ctrl Pts',(-19.5775380097716,-20.8936879531881,
21.361075329669));
#169988=CARTESIAN_POINT('Ctrl Pts',(-19.5672267492065,-20.8981419974324,
21.3604012509681));
#169989=CARTESIAN_POINT('Ctrl Pts',(-19.5609542871364,-20.9008155632606,
21.3599938570443));
#169990=CARTESIAN_POINT('Ctrl Pts',(-19.525258987277,-20.9158269091106,
21.3576899172704));
#169991=CARTESIAN_POINT('Ctrl Pts',(-19.4955714171562,-20.9275293307902,
21.3558293488611));
#169992=CARTESIAN_POINT('Ctrl Pts',(-19.2794561049982,-21.0071224262951,
21.342605264977));
#169993=CARTESIAN_POINT('Ctrl Pts',(-19.084552194699,-21.0491845593995,
21.3322948172777));
#169994=CARTESIAN_POINT('Ctrl Pts',(-18.8308771116841,-21.0675206426042,
21.3181607866529));
#169995=CARTESIAN_POINT('Ctrl Pts',(-18.774997640159,-21.0693406171215,
21.3150108687555));
#169996=CARTESIAN_POINT('Ctrl Pts',(-18.6844306692982,-21.0687037816697,
21.3098016289188));
#169997=CARTESIAN_POINT('Ctrl Pts',(-18.6497597955011,-21.0676075730561,
21.3077829067633));
#169998=CARTESIAN_POINT('Ctrl Pts',(-18.6042813203144,-21.0650499740806,
21.3050966179787));
#169999=CARTESIAN_POINT('Ctrl Pts',(-18.593434775635,-21.0643561583848,
21.3044530871149));
#170000=CARTESIAN_POINT('Ctrl Pts',(-18.5756893554948,-21.063083764776,
21.3033953861573));
#170001=CARTESIAN_POINT('Ctrl Pts',(-18.5687870400536,-21.062554808145,
21.3029827754469));
#170002=CARTESIAN_POINT('Ctrl Pts',(-18.5554387656461,-21.0614659865788,
21.3021824555244));
#170003=CARTESIAN_POINT('Ctrl Pts',(-18.5489925275103,-21.0609104050745,
21.3017948850868));
#170004=CARTESIAN_POINT('Ctrl Pts',(-18.5341249892073,-21.0595603263143,
21.3008984733759));
#170005=CARTESIAN_POINT('Ctrl Pts',(-18.5257057434526,-21.0587448940124,
21.3003889799265));
#170006=CARTESIAN_POINT('Ctrl Pts',(-18.5030993884878,-21.0564185568567,
21.2990158239832));
#170007=CARTESIAN_POINT('Ctrl Pts',(-18.4889224797778,-21.0548146728429,
21.2981492569185));
#170008=CARTESIAN_POINT('Ctrl Pts',(-18.3611878658061,-21.0390543419627,
21.2902911432454));
#170009=CARTESIAN_POINT('Ctrl Pts',(-18.2489541415696,-21.015857531346,
21.2830116140944));
#170010=CARTESIAN_POINT('Ctrl Pts',(-17.9820874112819,-20.9377247165375,
21.2648714388788));
#170011=CARTESIAN_POINT('Ctrl Pts',(-17.8308835810645,-20.8736804146279,
21.2538542156912));
#170012=CARTESIAN_POINT('Ctrl Pts',(-17.6600660801652,-20.7766723789927,
21.2413718810939));
#170013=CARTESIAN_POINT('Ctrl Pts',(-17.6319421012103,-20.75982521716,21.2393174949565));
#170014=CARTESIAN_POINT('Ctrl Pts',(-17.5980639138651,-20.7384465231899,
21.2368541846157));
#170015=CARTESIAN_POINT('Ctrl Pts',(-17.5919287755815,-20.7345305870816,
21.2364085626905));
#170016=CARTESIAN_POINT('Ctrl Pts',(-17.5823450909889,-20.7283437216201,
21.2357133475665));
#170017=CARTESIAN_POINT('Ctrl Pts',(-17.5788828526622,-20.7260942543688,
21.2354623748231));
#170018=CARTESIAN_POINT('Ctrl Pts',(-17.5724302582162,-20.7218750116092,
21.2349950117687));
#170019=CARTESIAN_POINT('Ctrl Pts',(-17.5694383446513,-20.7199077953743,
21.2347784624356));
#170020=CARTESIAN_POINT('Ctrl Pts',(-17.5626252435353,-20.7154033056093,
21.2342856861504));
#170021=CARTESIAN_POINT('Ctrl Pts',(-17.5588073113675,-20.7128612051516,
21.2340097869724));
#170022=CARTESIAN_POINT('Ctrl Pts',(-17.5471006926868,-20.705011532934,
21.2331644701471));
#170023=CARTESIAN_POINT('Ctrl Pts',(-17.5392393508416,-20.6996631251867,
21.2325977265799));
#170024=CARTESIAN_POINT('Ctrl Pts',(-17.4690650479913,-20.6512257302489,
21.2275443409458));
#170025=CARTESIAN_POINT('Ctrl Pts',(-17.4090637257419,-20.6048687098913,
21.2232630108996));
#170026=CARTESIAN_POINT('Ctrl Pts',(-17.2444652312138,-20.4629635446243,
21.2112324759176));
#170027=CARTESIAN_POINT('Ctrl Pts',(-17.1467977966924,-20.360018520536,
21.2037083659344));
#170028=CARTESIAN_POINT('Ctrl Pts',(-17.0222841640855,-20.1992127960163,
21.192456219598));
#170029=CARTESIAN_POINT('Ctrl Pts',(-16.9865970645232,-20.1487008749523,
21.1889869145585));
#170030=CARTESIAN_POINT('Ctrl Pts',(-16.9330236535886,-20.065356093378,
21.183300741611));
#170031=CARTESIAN_POINT('Ctrl Pts',(-16.9137065451066,-20.0334846644639,
21.1811350177436));
#170032=CARTESIAN_POINT('Ctrl Pts',(-16.8897212650156,-19.9914464986765,
21.1782819047434));
#170033=CARTESIAN_POINT('Ctrl Pts',(-16.8842776702087,-19.981728299811,
21.1776225832733));
#170034=CARTESIAN_POINT('Ctrl Pts',(-16.8755514268846,-19.9658572515203,
21.1765460343363));
#170035=CARTESIAN_POINT('Ctrl Pts',(-16.8722219963749,-19.9597302658975,
21.1761304847091));
#170036=CARTESIAN_POINT('Ctrl Pts',(-16.8658787582937,-19.9479183834283,
21.1753294144832));
#170037=CARTESIAN_POINT('Ctrl Pts',(-16.8628604741948,-19.9422359687051,
21.1749440587556));
#170038=CARTESIAN_POINT('Ctrl Pts',(-16.8560107188025,-19.9291970413597,
21.1740598207672));
#170039=CARTESIAN_POINT('Ctrl Pts',(-16.8521965013089,-19.9218316282696,
21.1735603356746));
#170040=CARTESIAN_POINT('Ctrl Pts',(-16.8421821529314,-19.9022119969455,
21.1722297439669));
#170041=CARTESIAN_POINT('Ctrl Pts',(-16.8360578920201,-19.8899196908249,
21.1713959949471));
#170042=CARTESIAN_POINT('Ctrl Pts',(-16.790517079691,-19.7962397296996,
21.1650403130209));
#170043=CARTESIAN_POINT('Ctrl Pts',(-16.7562372080106,-19.7124716821331,
21.1593415150642));
#170044=CARTESIAN_POINT('Ctrl Pts',(-16.6828132220643,-19.4941315697377,
21.1444672100533));
#170045=CARTESIAN_POINT('Ctrl Pts',(-16.6514713629923,-19.3573928277871,
21.1351153440828));
#170046=CARTESIAN_POINT('Ctrl Pts',(-16.6269164194993,-19.1639450369983,
21.1223445127553));
#170047=CARTESIAN_POINT('Ctrl Pts',(-16.6221156279491,-19.1090577748662,
21.1187756336227));
#170048=CARTESIAN_POINT('Ctrl Pts',(-16.6180913201353,-19.0256653698077,
21.113491487971));
#170049=CARTESIAN_POINT('Ctrl Pts',(-16.6172932042516,-18.9972620455094,
21.1117160264734));
#170050=CARTESIAN_POINT('Ctrl Pts',(-16.617011841326,-18.9619126873634,
21.1095435982719));
#170051=CARTESIAN_POINT('Ctrl Pts',(-16.6169907237174,-18.9549753233616,
21.1091190403129));
#170052=CARTESIAN_POINT('Ctrl Pts',(-16.6170112736636,-18.9439953278897,
21.108450035994));
#170053=CARTESIAN_POINT('Ctrl Pts',(-16.6170304189174,-18.939952775636,
21.1082043603217));
#170054=CARTESIAN_POINT('Ctrl Pts',(-16.6170883626996,-18.9323290679206,
21.1077422775837));
#170055=CARTESIAN_POINT('Ctrl Pts',(-16.6171246681997,-18.9287479998222,
21.1075257396181));
#170056=CARTESIAN_POINT('Ctrl Pts',(-16.6172284559512,-18.9205602942581,
21.1070318079626));
#170057=CARTESIAN_POINT('Ctrl Pts',(-16.617301888378,-18.9159537801199,
21.106754750254));
#170058=CARTESIAN_POINT('Ctrl Pts',(-16.6175368217481,-18.9037217612884,
21.1060211892931));
#170059=CARTESIAN_POINT('Ctrl Pts',(-16.6177244972546,-18.8960967471679,
21.1055661123605));
#170060=CARTESIAN_POINT('Ctrl Pts',(-16.619329749684,-18.8426269241492,
21.1023893126151));
#170061=CARTESIAN_POINT('Ctrl Pts',(-16.6221958022221,-18.7968341408434,
21.0997427792956));
#170062=CARTESIAN_POINT('Ctrl Pts',(-16.630125607129,-18.7136222305225,
21.0950110828089));
#170063=CARTESIAN_POINT('Ctrl Pts',(-16.634706330537,-18.6761780606287,
21.0929106702665));
#170064=CARTESIAN_POINT('Ctrl Pts',(-16.6596435950099,-18.5094347611808,
21.0836107017199));
#170065=CARTESIAN_POINT('Ctrl Pts',(-16.6909636048286,-18.3820682065839,
21.0766335490723));
#170066=CARTESIAN_POINT('Ctrl Pts',(-16.7627868872662,-18.1749472393378,
21.0645331902965));
#170067=CARTESIAN_POINT('Ctrl Pts',(-16.7969204146279,-18.0933893530314,
21.059561163438));
#170068=CARTESIAN_POINT('Ctrl Pts',(-16.845136893778,-17.9958062862303,
21.0532176623386));
#170069=CARTESIAN_POINT('Ctrl Pts',(-16.8544957140584,-17.977539201562,
21.0520126536466));
#170070=CARTESIAN_POINT('Ctrl Pts',(-16.8682708154767,-17.9515890626519,
21.0502743160111));
#170071=CARTESIAN_POINT('Ctrl Pts',(-16.8724722134385,-17.9437928140642,
21.0497485918527));
#170072=CARTESIAN_POINT('Ctrl Pts',(-16.879839066429,-17.9303256837383,
21.0488343255088));
#170073=CARTESIAN_POINT('Ctrl Pts',(-16.8829819479648,-17.9246425424038,
21.0484465936424));
#170074=CARTESIAN_POINT('Ctrl Pts',(-16.8890742005738,-17.9137448849469,
21.0476993804587));
#170075=CARTESIAN_POINT('Ctrl Pts',(-16.8920196575953,-17.9085282436169,
21.0473400426678));
#170076=CARTESIAN_POINT('Ctrl Pts',(-16.8997915891383,-17.8948989772083,
21.0463968450716));
#170077=CARTESIAN_POINT('Ctrl Pts',(-16.9046537624411,-17.8865069661934,
21.0458116978628));
#170078=CARTESIAN_POINT('Ctrl Pts',(-16.9217171616442,-17.8575169915387,
21.0437748597726));
#170079=CARTESIAN_POINT('Ctrl Pts',(-16.9342096439647,-17.8370933929544,
21.0423125956436));
#170080=CARTESIAN_POINT('Ctrl Pts',(-17.0303083072501,-17.6858098651131,
21.0312706867671));
#170081=CARTESIAN_POINT('Ctrl Pts',(-17.1277255615655,-17.5643153454577,
21.0211549202071));
#170082=CARTESIAN_POINT('Ctrl Pts',(-17.2901100872525,-17.4020330559754,
21.0059879943424));
#170083=CARTESIAN_POINT('Ctrl Pts',(-17.345426591608,-17.3522875107012,
21.0010643315316));
#170084=CARTESIAN_POINT('Ctrl Pts',(-17.4390035944696,-17.2766531277653,
20.9932277162184));
#170085=CARTESIAN_POINT('Ctrl Pts',(-17.4756950823505,-17.2489227520531,
20.9902669459361));
#170086=CARTESIAN_POINT('Ctrl Pts',(-17.5269190623262,-17.2127691336375,
20.9863123278379));
#170087=CARTESIAN_POINT('Ctrl Pts',(-17.5406895079049,-17.2032923334854,
20.9852661703942));
#170088=CARTESIAN_POINT('Ctrl Pts',(-17.5644677783493,-17.1873398606836,
20.9834904712766));
#170089=CARTESIAN_POINT('Ctrl Pts',(-17.574420510733,-17.18078390707,20.982756283555));
#170090=CARTESIAN_POINT('Ctrl Pts',(-17.5886445862378,-17.1715856699061,
20.9817204145142));
#170091=CARTESIAN_POINT('Ctrl Pts',(-17.59287057489,-17.1688741359681,20.9814143215289));
#170092=CARTESIAN_POINT('Ctrl Pts',(-17.6001692037068,-17.1642276684102,
20.9808885916387));
#170093=CARTESIAN_POINT('Ctrl Pts',(-17.6032372335233,-17.162285567204,
20.9806684816669));
#170094=CARTESIAN_POINT('Ctrl Pts',(-17.6091971208153,-17.1585343275622,
20.9802426318139));
#170095=CARTESIAN_POINT('Ctrl Pts',(-17.612088350825,-17.1567242866175,
20.9800368289607));
#170096=CARTESIAN_POINT('Ctrl Pts',(-17.6198980245481,-17.1518613110809,
20.9794829963599));
#170097=CARTESIAN_POINT('Ctrl Pts',(-17.6248246783332,-17.1488215233521,
20.9791358277436));
#170098=CARTESIAN_POINT('Ctrl Pts',(-17.6431404597721,-17.1376239978535,
20.9778531015));
#170099=CARTESIAN_POINT('Ctrl Pts',(-17.6566079933588,-17.1295946361591,
20.9769255817702));
#170100=CARTESIAN_POINT('Ctrl Pts',(-17.7862430427947,-17.0542454583023,
20.9681340851487));
#170101=CARTESIAN_POINT('Ctrl Pts',(-17.9084942705672,-16.997961680057,
20.9608714200922));
#170102=CARTESIAN_POINT('Ctrl Pts',(-18.1869591142976,-16.9005959526035,
20.9448516764622));
#170103=CARTESIAN_POINT('Ctrl Pts',(-18.3441739376419,-16.86500700228,20.9361044514156));
#170104=CARTESIAN_POINT('Ctrl Pts',(-18.5224430219259,-16.8455145698628,
20.9256316433863));
#170105=CARTESIAN_POINT('Ctrl Pts',(-18.5410187256382,-16.84373165439,20.9245345206191));
#170106=CARTESIAN_POINT('Ctrl Pts',(-18.5681154391477,-16.8414919897973,
20.9229246961221));
#170107=CARTESIAN_POINT('Ctrl Pts',(-18.5766198066782,-16.8408407875857,
20.9224180998174));
#170108=CARTESIAN_POINT('Ctrl Pts',(-18.5915593296888,-16.8397875992689,
20.9215257112069));
#170109=CARTESIAN_POINT('Ctrl Pts',(-18.5979928579074,-16.8393635839924,
20.9211406155685));
#170110=CARTESIAN_POINT('Ctrl Pts',(-18.610505430169,-16.8385963085087,
20.9203900514181));
#170111=CARTESIAN_POINT('Ctrl Pts',(-18.6165842213919,-16.838249871504,
20.9200246866073));
#170112=CARTESIAN_POINT('Ctrl Pts',(-18.6311460222534,-16.8374829872647,
20.9191476686883));
#170113=CARTESIAN_POINT('Ctrl Pts',(-18.6396301836557,-16.8370873605842,
20.9186352418486));
#170114=CARTESIAN_POINT('Ctrl Pts',(-18.6704146048268,-16.8358374525823,
20.9167705396065));
#170115=CARTESIAN_POINT('Ctrl Pts',(-18.6927250273156,-16.8352847743723,
20.9154088693828));
#170116=CARTESIAN_POINT('Ctrl Pts',(-18.8983629538489,-16.8334429315233,
20.9027594792591));
#170117=CARTESIAN_POINT('Ctrl Pts',(-19.0810906891775,-16.8556220084415,
20.8906948986998));
#170118=CARTESIAN_POINT('Ctrl Pts',(-19.337623703182,-16.9212426786108,
20.8732108564779));
#170119=CARTESIAN_POINT('Ctrl Pts',(-19.4153870026047,-16.9459964148468,
20.8678507079561));
#170120=CARTESIAN_POINT('Ctrl Pts',(-19.5255257817737,-16.9882023664138,
20.8603297433804));
#170121=CARTESIAN_POINT('Ctrl Pts',(-19.5591795516302,-17.0021042887357,
20.8580420997372));
#170122=CARTESIAN_POINT('Ctrl Pts',(-19.5993085431524,-17.0199062511952,
20.8553411458936));
#170123=CARTESIAN_POINT('Ctrl Pts',(-19.6061407962664,-17.0229806728898,
20.8548822451438));
#170124=CARTESIAN_POINT('Ctrl Pts',(-19.6167470999459,-17.0278212356537,
20.8541715103574));
#170125=CARTESIAN_POINT('Ctrl Pts',(-19.6205324220766,-17.0295623222269,
20.8539181837581));
#170126=CARTESIAN_POINT('Ctrl Pts',(-19.6275485583982,-17.0328145751237,
20.8534492878169));
#170127=CARTESIAN_POINT('Ctrl Pts',(-19.6307806650478,-17.0343227173574,
20.8532335425427));
#170128=CARTESIAN_POINT('Ctrl Pts',(-19.6380868132466,-17.0377543702729,
20.8527464286674));
#170129=CARTESIAN_POINT('Ctrl Pts',(-19.6421585242702,-17.0396827165784,
20.8524753631437));
#170130=CARTESIAN_POINT('Ctrl Pts',(-19.6544481791575,-17.0455511527693,
20.8516583326395));
#170131=CARTESIAN_POINT('Ctrl Pts',(-19.6626469890034,-17.0495313841809,
20.8511147944127));
#170132=CARTESIAN_POINT('Ctrl Pts',(-19.7255935316432,-17.0805935830074,
20.8469516357087));
#170133=CARTESIAN_POINT('Ctrl Pts',(-19.7791771967552,-17.1099832236455,
20.8434651876825));
#170134=CARTESIAN_POINT('Ctrl Pts',(-19.9708583098656,-17.2261788969541,
20.8309359318723));
#170135=CARTESIAN_POINT('Ctrl Pts',(-20.1000686775985,-17.3265342065346,
20.8223349060213));
#170136=CARTESIAN_POINT('Ctrl Pts',(-20.2731076958554,-17.4962774860746,
20.8088863626249));
#170137=CARTESIAN_POINT('Ctrl Pts',(-20.3265596629551,-17.5549558728225,
20.8043990523465));
#170138=CARTESIAN_POINT('Ctrl Pts',(-20.3888154825006,-17.6315265031988,
20.7986404092466));
#170139=CARTESIAN_POINT('Ctrl Pts',(-20.4008332352514,-17.6467293514953,
20.79750168058));
#170140=CARTESIAN_POINT('Ctrl Pts',(-20.4179160356804,-17.6689603452835,
20.7958421240072));
#170141=CARTESIAN_POINT('Ctrl Pts',(-20.4231495398368,-17.6758582369229,
20.7953279585968));
#170142=CARTESIAN_POINT('Ctrl Pts',(-20.4322170744103,-17.6879629844478,
20.7944269154874));
#170143=CARTESIAN_POINT('Ctrl Pts',(-20.436069863554,-17.6931556940374,
20.7940407786994));
#170144=CARTESIAN_POINT('Ctrl Pts',(-20.4434805340365,-17.7032398597072,
20.7932916276387));
#170145=CARTESIAN_POINT('Ctrl Pts',(-20.4470413638276,-17.7081290786947,
20.7929287332013));
#170146=CARTESIAN_POINT('Ctrl Pts',(-20.4554655364922,-17.7198007223967,
20.7920631596206));
#170147=CARTESIAN_POINT('Ctrl Pts',(-20.4603097930576,-17.7265967405258,
20.7915597506624));
#170148=CARTESIAN_POINT('Ctrl Pts',(-20.47743436792,-17.7509239195865,20.7897596960242));
#170149=CARTESIAN_POINT('Ctrl Pts',(-20.4894885235742,-17.7686120091074,
20.788454475028));
#170150=CARTESIAN_POINT('Ctrl Pts',(-20.5919346977185,-17.923950535541,
20.7770191365605));
#170151=CARTESIAN_POINT('Ctrl Pts',(-20.6661822790493,-18.0714329895054,
20.7662793853259));
#170152=CARTESIAN_POINT('Ctrl Pts',(-20.7225805788317,-18.2258896216873,
20.755413772291));
#170153=CARTESIAN_POINT('',(-20.8509997094765,-18.9531090880733,21.2890562789773));
#170154=CARTESIAN_POINT('Ctrl Pts',(-20.8509997094765,-18.9531090880733,
21.2890562789773));
#170155=CARTESIAN_POINT('Ctrl Pts',(-20.8509573539261,-19.0339563084801,
21.2842160173539));
#170156=CARTESIAN_POINT('Ctrl Pts',(-20.8462795783447,-19.1146414750005,
21.2793757557306));
#170157=CARTESIAN_POINT('Ctrl Pts',(-20.8370465901719,-19.1946603378517,
21.2745354941073));
#170158=CARTESIAN_POINT('Ctrl Pts',(-20.8277795525455,-19.2749742946103,
21.2696773825463));
#170159=CARTESIAN_POINT('Ctrl Pts',(-20.8139237784189,-19.354616746761,
21.2648192709853));
#170160=CARTESIAN_POINT('Ctrl Pts',(-20.7956102733323,-19.4330946693642,
21.2599611594243));
#170161=CARTESIAN_POINT('Ctrl Pts',(-20.7772067235592,-19.5119584558372,
21.2550791612762));
#170162=CARTESIAN_POINT('Ctrl Pts',(-20.754301638724,-19.5896459636135,
21.2501971631282));
#170163=CARTESIAN_POINT('Ctrl Pts',(-20.7270762122811,-19.6656779470036,
21.2453151649801));
#170164=CARTESIAN_POINT('Ctrl Pts',(-20.714146733797,-19.7017858807181,
21.2429966819199));
#170165=CARTESIAN_POINT('Ctrl Pts',(-20.700243557214,-19.7375207682869,
21.2406781988597));
#170166=CARTESIAN_POINT('Ctrl Pts',(-20.6853897271448,-19.7728331942566,
21.2383597157995));
#170167=CARTESIAN_POINT('Ctrl Pts',(-20.6572744235311,-19.8396724924615,
21.2339712951122));
#170168=CARTESIAN_POINT('Ctrl Pts',(-20.6256662222363,-19.9051959792736,
21.229582874425));
#170169=CARTESIAN_POINT('Ctrl Pts',(-20.5907099161381,-19.9690139071392,
21.2251944537377));
#170170=CARTESIAN_POINT('Ctrl Pts',(-20.5558054761045,-20.0327371458015,
21.2208125443251));
#170171=CARTESIAN_POINT('Ctrl Pts',(-20.5175630226924,-20.0947594296034,
21.2164306349125));
#170172=CARTESIAN_POINT('Ctrl Pts',(-20.4761752538898,-20.1547112640755,
21.2120487254999));
#170173=CARTESIAN_POINT('Ctrl Pts',(-20.434836104603,-20.214592671239,21.2076719636544));
#170174=CARTESIAN_POINT('Ctrl Pts',(-20.3903592525526,-20.2724080657538,
21.2032952018088));
#170175=CARTESIAN_POINT('Ctrl Pts',(-20.342982262568,-20.3278143329467,
21.1989184399633));
#170176=CARTESIAN_POINT('Ctrl Pts',(-20.295635309639,-20.3831854725149,
21.1945444529888));
#170177=CARTESIAN_POINT('Ctrl Pts',(-20.2453921796757,-20.4361501496307,
21.1901704660143));
#170178=CARTESIAN_POINT('Ctrl Pts',(-20.1925316651773,-20.4863970743179,
21.1857964790398));
#170179=CARTESIAN_POINT('Ctrl Pts',(-20.139687231237,-20.5366287135202,
21.1814238226644));
#170180=CARTESIAN_POINT('Ctrl Pts',(-20.0842273429024,-20.584143909571,
21.177051166289));
#170181=CARTESIAN_POINT('Ctrl Pts',(-20.0264675343393,-20.6286683251851,
21.1726785099136));
#170182=CARTESIAN_POINT('Ctrl Pts',(-19.9687062484273,-20.6731938796203,
21.1683057416968));
#170183=CARTESIAN_POINT('Ctrl Pts',(-19.9086453087151,-20.7147282088577,
21.16393297348));
#170184=CARTESIAN_POINT('Ctrl Pts',(-19.8466318572416,-20.7530384088772,
21.1595602052632));
#170185=CARTESIAN_POINT('Ctrl Pts',(-19.7845540695746,-20.7913883540227,
21.1551829004941));
#170186=CARTESIAN_POINT('Ctrl Pts',(-19.7205201370247,-20.8265072376108,
21.1508055957251));
#170187=CARTESIAN_POINT('Ctrl Pts',(-19.654903893158,-20.8582069718597,
21.146428290956));
#170188=CARTESIAN_POINT('Ctrl Pts',(-19.589251822749,-20.8899240141987,
21.1420485961737));
#170189=CARTESIAN_POINT('Ctrl Pts',(-19.5220161657843,-20.9182180030709,
21.1376689013914));
#170190=CARTESIAN_POINT('Ctrl Pts',(-19.4535904234765,-20.9429491762576,
21.133289206609));
#170191=CARTESIAN_POINT('Ctrl Pts',(-19.3850434522868,-20.9677241653004,
21.1289017523858));
#170192=CARTESIAN_POINT('Ctrl Pts',(-19.3153026471293,-20.9889235930605,
21.1245142981626));
#170193=CARTESIAN_POINT('Ctrl Pts',(-19.2447757667322,-21.0064578642842,
21.1201268439394));
#170194=CARTESIAN_POINT('Ctrl Pts',(-19.1968575236042,-21.018371215149,
21.1171458656656));
#170195=CARTESIAN_POINT('Ctrl Pts',(-19.1485766551865,-21.028593691043,
21.1141648873919));
#170196=CARTESIAN_POINT('Ctrl Pts',(-19.1000625450044,-21.0371108395347,
21.1111839091181));
#170197=CARTESIAN_POINT('Ctrl Pts',(-19.0286448032708,-21.0496489549201,
21.1067956036196));
#170198=CARTESIAN_POINT('Ctrl Pts',(-18.9564428174331,-21.0585380613871,
21.102407298121));
#170199=CARTESIAN_POINT('Ctrl Pts',(-18.8838626580299,-21.0636889410442,
21.0980189926225));
#170200=CARTESIAN_POINT('Ctrl Pts',(-18.8113901771551,-21.0688321789552,
21.0936371975296));
#170201=CARTESIAN_POINT('Ctrl Pts',(-18.7385411136489,-21.0702481657021,
21.0892554024367));
#170202=CARTESIAN_POINT('Ctrl Pts',(-18.6657304393715,-21.0678989264829,
21.0848736073437));
#170203=CARTESIAN_POINT('Ctrl Pts',(-18.5930052691539,-21.0655524460555,
21.0804969579424));
#170204=CARTESIAN_POINT('Ctrl Pts',(-18.5203188783214,-21.059449538749,
21.076120308541));
#170205=CARTESIAN_POINT('Ctrl Pts',(-18.448088343777,-21.049604234558,21.0717436591396));
#170206=CARTESIAN_POINT('Ctrl Pts',(-18.3759035845749,-21.0397651697252,
21.0673697833938));
#170207=CARTESIAN_POINT('Ctrl Pts',(-18.3041745852159,-21.0261884787699,
21.062995907648));
#170208=CARTESIAN_POINT('Ctrl Pts',(-18.2333139789055,-21.0089400837848,
21.0586220319021));
#170209=CARTESIAN_POINT('Ctrl Pts',(-18.1624749070484,-20.9916969305662,
21.0542494853719));
#170210=CARTESIAN_POINT('Ctrl Pts',(-18.0925041726962,-20.9707844025933,
21.0498769388417));
#170211=CARTESIAN_POINT('Ctrl Pts',(-18.0238032249561,-20.9463193176413,
21.0455043923115));
#170212=CARTESIAN_POINT('Ctrl Pts',(-17.9551004955794,-20.9218535982309,
21.041131732387));
#170213=CARTESIAN_POINT('Ctrl Pts',(-17.8876680719231,-20.8938353026274,
21.0367590724626));
#170214=CARTESIAN_POINT('Ctrl Pts',(-17.8218896723665,-20.8624302526458,
21.0323864125382));
#170215=CARTESIAN_POINT('Ctrl Pts',(-17.7560429813199,-20.8309925977715,
21.0280092128946));
#170216=CARTESIAN_POINT('Ctrl Pts',(-17.6918541791272,-20.7961613765664,
21.023632013251));
#170217=CARTESIAN_POINT('Ctrl Pts',(-17.6296837477988,-20.7581491120958,
21.0192548136074));
#170218=CARTESIAN_POINT('Ctrl Pts',(-17.5674793476667,-20.7201160784086,
21.0148752223408));
#170219=CARTESIAN_POINT('Ctrl Pts',(-17.5072959123103,-20.6788988137273,
21.0104956310741));
#170220=CARTESIAN_POINT('Ctrl Pts',(-17.4494639340252,-20.634752535345,
21.0061160398075));
#170221=CARTESIAN_POINT('Ctrl Pts',(-17.3915294434579,-20.5905280037906,
21.0017286853291));
#170222=CARTESIAN_POINT('Ctrl Pts',(-17.3359551017082,-20.5433644028354,
20.9973413308507));
#170223=CARTESIAN_POINT('Ctrl Pts',(-17.2830369348489,-20.4935560916059,
20.9929539763722));
#170224=CARTESIAN_POINT('Ctrl Pts',(-17.2470699869645,-20.4597028226716,
20.9899720183937));
#170225=CARTESIAN_POINT('Ctrl Pts',(-17.2123293058517,-20.4246286086914,
20.9869900604152));
#170226=CARTESIAN_POINT('Ctrl Pts',(-17.1788971544343,-20.3884345232949,
20.9840081024366));
#170227=CARTESIAN_POINT('Ctrl Pts',(-17.1297001013421,-20.3351731486785,
20.979620004789));
#170228=CARTESIAN_POINT('Ctrl Pts',(-17.0831463900084,-20.2792773756617,
20.9752319071414));
#170229=CARTESIAN_POINT('Ctrl Pts',(-17.0395308416818,-20.2210402954628,
20.9708438094938));
#170230=CARTESIAN_POINT('Ctrl Pts',(-16.9959800453897,-20.1628896745558,
20.9664622264554));
#170231=CARTESIAN_POINT('Ctrl Pts',(-16.9553590396968,-20.1024050295693,
20.9620806434169));
#170232=CARTESIAN_POINT('Ctrl Pts',(-16.9179243810532,-20.0399146778434,
20.9576990603784));
#170233=CARTESIAN_POINT('Ctrl Pts',(-16.8805337302903,-19.9774977892675,
20.9533226282934));
#170234=CARTESIAN_POINT('Ctrl Pts',(-16.8463222321173,-19.9130802896936,
20.9489461962084));
#170235=CARTESIAN_POINT('Ctrl Pts',(-16.8155038577208,-19.8470204199123,
20.9445697641234));
#170236=CARTESIAN_POINT('Ctrl Pts',(-16.7847050371391,-19.781002464167,
20.9401961088215));
#170237=CARTESIAN_POINT('Ctrl Pts',(-16.7572952721812,-19.7133446418889,
20.9358224535196));
#170238=CARTESIAN_POINT('Ctrl Pts',(-16.7334424981437,-19.6444295500383,
20.9314487982177));
#170239=CARTESIAN_POINT('Ctrl Pts',(-16.7095969886214,-19.5755354467209,
20.9270764749406));
#170240=CARTESIAN_POINT('Ctrl Pts',(-16.6893064770216,-19.5053852896205,
20.9227041516635));
#170241=CARTESIAN_POINT('Ctrl Pts',(-16.6726900512339,-19.4343798245343,
20.9183318283864));
#170242=CARTESIAN_POINT('Ctrl Pts',(-16.6560732039841,-19.3633725584528,
20.9139593942089));
#170243=CARTESIAN_POINT('Ctrl Pts',(-16.6431307355402,-19.2915104114853,
20.9095869600314));
#170244=CARTESIAN_POINT('Ctrl Pts',(-16.6339309326538,-19.2192057491441,
20.9052145258539));
#170245=CARTESIAN_POINT('Ctrl Pts',(-16.6247215828182,-19.1468260537894,
20.9008375542524));
#170246=CARTESIAN_POINT('Ctrl Pts',(-16.6192627140126,-19.0740034057825,
20.8964605826508));
#170247=CARTESIAN_POINT('Ctrl Pts',(-16.6175707675104,-19.0011559138216,
20.8920836110493));
#170248=CARTESIAN_POINT('Ctrl Pts',(-16.6158778971444,-18.9282686444977,
20.8877042494631));
#170249=CARTESIAN_POINT('Ctrl Pts',(-16.6179560305416,-18.8553569867552,
20.8833248878769));
#170250=CARTESIAN_POINT('Ctrl Pts',(-16.6237694768944,-18.782836944478,
20.8789455262907));
#170251=CARTESIAN_POINT('Ctrl Pts',(-16.6295932284966,-18.7101883490033,
20.8745584015963));
#170252=CARTESIAN_POINT('Ctrl Pts',(-16.6391654523683,-18.6379332339321,
20.8701712769019));
#170253=CARTESIAN_POINT('Ctrl Pts',(-16.6523988893426,-18.5664798110215,
20.8657841522075));
#170254=CARTESIAN_POINT('Ctrl Pts',(-16.6613997601799,-18.5178799626416,
20.8628002000567));
#170255=CARTESIAN_POINT('Ctrl Pts',(-16.6720933057598,-18.4696507787821,
20.859816247906));
#170256=CARTESIAN_POINT('Ctrl Pts',(-16.6844389804171,-18.4219163962107,
20.8568322957552));
#170257=CARTESIAN_POINT('Ctrl Pts',(-16.7025947174696,-18.3517174866827,
20.8524440503065));
#170258=CARTESIAN_POINT('Ctrl Pts',(-16.7243966047991,-18.2823154178057,
20.8480558048578));
#170259=CARTESIAN_POINT('Ctrl Pts',(-16.7497577485801,-18.2141167519993,
20.8436675594091));
#170260=CARTESIAN_POINT('Ctrl Pts',(-16.7750812545399,-18.1460192980786,
20.8392858264426));
#170261=CARTESIAN_POINT('Ctrl Pts',(-16.8039533643146,-18.0791221502751,
20.834904093476));
#170262=CARTESIAN_POINT('Ctrl Pts',(-16.8362368533681,-18.0138187598946,
20.8305223605095));
#170263=CARTESIAN_POINT('Ctrl Pts',(-16.8684824095669,-17.9485921005021,
20.826145776046));
#170264=CARTESIAN_POINT('Ctrl Pts',(-16.9041311697296,-17.8849559087621,
20.8217691915824));
#170265=CARTESIAN_POINT('Ctrl Pts',(-16.9429976989673,-17.8232840225745,
20.8173926071189));
#170266=CARTESIAN_POINT('Ctrl Pts',(-16.9818395815048,-17.7616512448053,
20.813018798009));
#170267=CARTESIAN_POINT('Ctrl Pts',(-17.0238949279354,-17.7019807081629,
20.8086449888991));
#170268=CARTESIAN_POINT('Ctrl Pts',(-17.0689329066922,-17.6446207226732,
20.8042711797893));
#170269=CARTESIAN_POINT('Ctrl Pts',(-17.1139571817387,-17.587278190112,
20.7998987014987));
#170270=CARTESIAN_POINT('Ctrl Pts',(-17.1619619896782,-17.5322451921335,
20.7955262232082));
#170271=CARTESIAN_POINT('Ctrl Pts',(-17.2126747998581,-17.4798387875598,
20.7911537449176));
#170272=CARTESIAN_POINT('Ctrl Pts',(-17.2633889076796,-17.4274310420089,
20.7867811547439));
#170273=CARTESIAN_POINT('Ctrl Pts',(-17.3168108184396,-17.3776503685512,
20.7824085645702));
#170274=CARTESIAN_POINT('Ctrl Pts',(-17.3726307347287,-17.3307773985123,
20.7780359743965));
#170275=CARTESIAN_POINT('Ctrl Pts',(-17.428508580755,-17.2838557838494,
20.7736588463622));
#170276=CARTESIAN_POINT('Ctrl Pts',(-17.4867890308601,-17.2398482083165,
20.7692817183279));
#170277=CARTESIAN_POINT('Ctrl Pts',(-17.547129396645,-17.1989948172091,
20.7649045902936));
#170278=CARTESIAN_POINT('Ctrl Pts',(-17.6075027159868,-17.1581191149253,
20.7605250717876));
#170279=CARTESIAN_POINT('Ctrl Pts',(-17.6699377776663,-17.1204012763226,
20.7561455532815));
#170280=CARTESIAN_POINT('Ctrl Pts',(-17.7340654457233,-17.0860364721776,
20.7517660347755));
#170281=CARTESIAN_POINT('Ctrl Pts',(-17.7983067720839,-17.0516107606978,
20.7473787541185));
#170282=CARTESIAN_POINT('Ctrl Pts',(-17.864246258806,-17.0205501570155,
20.7429914734614));
#170283=CARTESIAN_POINT('Ctrl Pts',(-17.9314934095092,-16.9930022531359,
20.7386041928044));
#170284=CARTESIAN_POINT('Ctrl Pts',(-17.9772094713291,-16.9742745945867,
20.7356216248942));
#170285=CARTESIAN_POINT('Ctrl Pts',(-18.0235294787558,-16.9571693380886,
20.732639056984));
#170286=CARTESIAN_POINT('Ctrl Pts',(-18.0703272882045,-16.9417195390648,
20.7296564890738));
#170287=CARTESIAN_POINT('Ctrl Pts',(-18.139180375299,-16.9189884247175,
20.7252682706827));
#170288=CARTESIAN_POINT('Ctrl Pts',(-18.2093370331468,-16.8997544122152,
20.7208800522916));
#170289=CARTESIAN_POINT('Ctrl Pts',(-18.2804083783847,-16.884164503448,
20.7164918339006));
#170290=CARTESIAN_POINT('Ctrl Pts',(-18.3513742467947,-16.8685977316303,
20.7121101280548));
#170291=CARTESIAN_POINT('Ctrl Pts',(-18.4232516405218,-16.8566644300181,
20.707728422209));
#170292=CARTESIAN_POINT('Ctrl Pts',(-18.4956354571152,-16.8484621836783,
20.7033467163632));
#170293=CARTESIAN_POINT('Ctrl Pts',(-18.5679342234102,-16.8402695749002,
20.6989701589803));
#170294=CARTESIAN_POINT('Ctrl Pts',(-18.6407377535873,-16.8357993666837,
20.6945936015973));
#170295=CARTESIAN_POINT('Ctrl Pts',(-18.7136313412727,-16.8350979905197,
20.6902170442144));
#170296=CARTESIAN_POINT('Ctrl Pts',(-18.7864787048096,-16.8343970591207,
20.685843262146));
#170297=CARTESIAN_POINT('Ctrl Pts',(-18.8594155313779,-16.837460222459,
20.6814694800777));
#170298=CARTESIAN_POINT('Ctrl Pts',(-18.932024006899,-16.8442819228626,
20.6770956980093));
#170299=CARTESIAN_POINT('Ctrl Pts',(-19.0046103910108,-16.8511015477375,
20.6727232466811));
#170300=CARTESIAN_POINT('Ctrl Pts',(-19.0768681424401,-16.8616773942849,
20.6683507953528));
#170301=CARTESIAN_POINT('Ctrl Pts',(-19.1483831533474,-16.8759519268037,
20.6639783440246));
#170302=CARTESIAN_POINT('Ctrl Pts',(-19.2198999961485,-16.890226824972,
20.6596057806937));
#170303=CARTESIAN_POINT('Ctrl Pts',(-19.2906735880014,-16.9082005008351,
20.6552332173629));
#170304=CARTESIAN_POINT('Ctrl Pts',(-19.3603002789774,-16.9297643657197,
20.6508606540321));
#170305=CARTESIAN_POINT('Ctrl Pts',(-19.4299992346993,-16.951350611493,
20.6464835524678));
#170306=CARTESIAN_POINT('Ctrl Pts',(-19.4985484511517,-16.976534342916,
20.6421064509035));
#170307=CARTESIAN_POINT('Ctrl Pts',(-19.5655605174569,-17.005157400865,
20.6377293493392));
#170308=CARTESIAN_POINT('Ctrl Pts',(-19.6326091837084,-17.033796091855,
20.6333498571355));
#170309=CARTESIAN_POINT('Ctrl Pts',(-19.6981185947722,-17.0658776370537,
20.6289703649319));
#170310=CARTESIAN_POINT('Ctrl Pts',(-19.7617248407813,-17.1011972953226,
20.6245908727283));
#170311=CARTESIAN_POINT('Ctrl Pts',(-19.8254438298318,-17.1365795582247,
20.6202036178079));
#170312=CARTESIAN_POINT('Ctrl Pts',(-19.8872525078967,-17.1752111400653,
20.6158163628875));
#170313=CARTESIAN_POINT('Ctrl Pts',(-19.9468154094471,-17.2168435855498,
20.6114291079671));
#170314=CARTESIAN_POINT('Ctrl Pts',(-19.9873110573495,-17.2451486682401,
20.6084462994422));
#170315=CARTESIAN_POINT('Ctrl Pts',(-20.0267692624342,-17.2748399740111,
20.6054634909173));
#170316=CARTESIAN_POINT('Ctrl Pts',(-20.0650939280144,-17.3058293056906,
20.6024806823923));
#170317=CARTESIAN_POINT('Ctrl Pts',(-20.1207334278707,-17.3508194155695,
20.5981502604048));
#170318=CARTESIAN_POINT('Ctrl Pts',(-20.174211694955,-17.3987327328762,
20.5938198384172));
#170319=CARTESIAN_POINT('Ctrl Pts',(-20.2251992647985,-17.4493311234127,
20.5894894164297));
#170320=CARTESIAN_POINT('Ctrl Pts',(-20.2761150683178,-17.4998582954048,
20.5851650896231));
#170321=CARTESIAN_POINT('Ctrl Pts',(-20.3245467768446,-17.5530627009004,
20.5808407628166));
#170322=CARTESIAN_POINT('Ctrl Pts',(-20.3701971545491,-17.6086653911086,
20.5765164360101));
#170323=CARTESIAN_POINT('Ctrl Pts',(-20.4157961614946,-17.6642055111358,
20.5721969754054));
#170324=CARTESIAN_POINT('Ctrl Pts',(-20.4586197368312,-17.7221381775607,
20.5678775148007));
#170325=CARTESIAN_POINT('Ctrl Pts',(-20.498408150765,-17.782148352348,20.5635580541959));
#170326=CARTESIAN_POINT('Ctrl Pts',(-20.5381709755269,-17.8421199327174,
20.5592413715713));
#170327=CARTESIAN_POINT('Ctrl Pts',(-20.574902238587,-17.9041659577839,
20.5549246889466));
#170328=CARTESIAN_POINT('Ctrl Pts',(-20.6083841459909,-17.967940513354,
20.5506080063219));
#170329=CARTESIAN_POINT('Ctrl Pts',(-20.6418605335062,-18.0317045549341,
20.5462920353534));
#170330=CARTESIAN_POINT('Ctrl Pts',(-20.6720883940015,-18.0971961244752,
20.5419760643849));
#170331=CARTESIAN_POINT('Ctrl Pts',(-20.6988955789411,-18.1640441866084,
20.5376600934164));
#170332=CARTESIAN_POINT('Ctrl Pts',(-20.7071130186217,-18.184535704818,
20.5363370812771));
#170333=CARTESIAN_POINT('Ctrl Pts',(-20.7150093677705,-18.2051545331966,
20.5350140691378));
#170334=CARTESIAN_POINT('Ctrl Pts',(-20.7225805737622,-18.2258896078036,
20.5336910569984));
#170335=CARTESIAN_POINT('Ctrl Pts',(-20.7225805737622,-18.2258896078036,
21.3335535462005));
#170336=CARTESIAN_POINT('Ctrl Pts',(-20.7478889850652,-18.2952011279398,
21.3291191954399));
#170337=CARTESIAN_POINT('Ctrl Pts',(-20.7695971613257,-18.3659128814929,
21.3246848446794));
#170338=CARTESIAN_POINT('Ctrl Pts',(-20.7875590779851,-18.4376225965061,
21.3202504939188));
#170339=CARTESIAN_POINT('Ctrl Pts',(-20.8055066098553,-18.5092748828416,
21.3158196944051));
#170340=CARTESIAN_POINT('Ctrl Pts',(-20.8197137296134,-18.5819230936247,
21.3113888948915));
#170341=CARTESIAN_POINT('Ctrl Pts',(-20.830084178873,-18.6551496756305,
21.3069580953778));
#170342=CARTESIAN_POINT('Ctrl Pts',(-20.8404495304526,-18.728340262505,
21.3025294738602));
#170343=CARTESIAN_POINT('Ctrl Pts',(-20.8469818942704,-18.8021081961854,
21.2981008523426));
#170344=CARTESIAN_POINT('Ctrl Pts',(-20.8496363359742,-18.8760270185819,
21.2936722308251));
#170345=CARTESIAN_POINT('Ctrl Pts',(-20.8505585774226,-18.9017088791887,
21.2921335802242));
#170346=CARTESIAN_POINT('Ctrl Pts',(-20.8510131736972,-18.9274089012658,
21.2905949296234));
#170347=CARTESIAN_POINT('Ctrl Pts',(-20.8509997094769,-18.9531090873175,
21.2890562790225));
#170348=CARTESIAN_POINT('Origin',(18.734,-18.952,0.));
#170349=CARTESIAN_POINT('',(16.7454193692319,-18.2258897639242,0.755484063719886));
#170350=CARTESIAN_POINT('',(16.7454193692601,-18.2258897638472,0.534177402183209));
#170351=CARTESIAN_POINT('',(16.7454193692319,-18.2258897639242,0.));
#170352=CARTESIAN_POINT('',(16.6170002905275,-18.9508909042358,0.710943721022754));
#170353=CARTESIAN_POINT('Ctrl Pts',(16.6170002905275,-18.9508909042358,
0.710943721022754));
#170354=CARTESIAN_POINT('Ctrl Pts',(16.6170426220087,-18.8700901868306,
0.715781198687434));
#170355=CARTESIAN_POINT('Ctrl Pts',(16.6217150376884,-18.7894513354829,
0.720618676352114));
#170356=CARTESIAN_POINT('Ctrl Pts',(16.6309374829181,-18.7094777345376,
0.725456154016795));
#170357=CARTESIAN_POINT('Ctrl Pts',(16.6404786381714,-18.6267403992884,
0.730460805633977));
#170358=CARTESIAN_POINT('Ctrl Pts',(16.6548898613221,-18.5447154887152,
0.735465457251158));
#170359=CARTESIAN_POINT('Ctrl Pts',(16.6740271623484,-18.4639416959648,
0.74047010886834));
#170360=CARTESIAN_POINT('Ctrl Pts',(16.6931644633748,-18.3831679032145,
0.745474760485522));
#170361=CARTESIAN_POINT('Ctrl Pts',(16.7170276379269,-18.303645515244,0.750479412102703));
#170362=CARTESIAN_POINT('Ctrl Pts',(16.7454193692319,-18.2258897639242,
0.755484063719885));
#170363=CARTESIAN_POINT('',(17.1140597194292,-17.5891051077268,2.19245913216589E-7));
#170364=CARTESIAN_POINT('Ctrl Pts',(17.1140597194292,-17.5891051077268,
2.19245913216589E-7));
#170365=CARTESIAN_POINT('Ctrl Pts',(17.1607064768662,-17.5336606550705,
0.00438522828538332));
#170366=CARTESIAN_POINT('Ctrl Pts',(17.2102946586576,-17.480504861525,0.00877023732485342));
#170367=CARTESIAN_POINT('Ctrl Pts',(17.2625708870035,-17.4299667002899,
0.0131552463643235));
#170368=CARTESIAN_POINT('Ctrl Pts',(17.3147694940965,-17.3795035795756,
0.0175337444157921));
#170369=CARTESIAN_POINT('Ctrl Pts',(17.3696478802627,-17.3316507087742,
0.0219122424672607));
#170370=CARTESIAN_POINT('Ctrl Pts',(17.4269129074637,-17.2867035301409,
0.0262907405187293));
#170371=CARTESIAN_POINT('Ctrl Pts',(17.4841105391582,-17.2418092500745,
0.0306640854932059));
#170372=CARTESIAN_POINT('Ctrl Pts',(17.5436888539646,-17.1998141657851,
0.0350374304676826));
#170373=CARTESIAN_POINT('Ctrl Pts',(17.6053196809547,-17.1609752270279,
0.0394107754421593));
#170374=CARTESIAN_POINT('Ctrl Pts',(17.6669115101639,-17.1221608641606,
0.0437813531205117));
#170375=CARTESIAN_POINT('Ctrl Pts',(17.7305528669284,-17.0864989413484,
0.0481519307988641));
#170376=CARTESIAN_POINT('Ctrl Pts',(17.7958856448177,-17.0542037894966,
0.0525225084772165));
#170377=CARTESIAN_POINT('Ctrl Pts',(17.8611987192176,-17.0219183774295,
0.0568917680479646));
#170378=CARTESIAN_POINT('Ctrl Pts',(17.9282017691103,-16.9929979344005,
0.0612610276187128));
#170379=CARTESIAN_POINT('Ctrl Pts',(17.9965125678453,-16.9676106008614,
0.065630287189461));
#170380=CARTESIAN_POINT('Ctrl Pts',(18.0648253874043,-16.9422225162941,
0.0699996760151008));
#170381=CARTESIAN_POINT('Ctrl Pts',(18.1344455789652,-16.9203679149719,
0.0743690648407405));
#170382=CARTESIAN_POINT('Ctrl Pts',(18.20497303869,-16.9021659886208,0.0787384536663803));
#170383=CARTESIAN_POINT('Ctrl Pts',(18.2755722935749,-16.8839455331716,
0.0831122904187001));
#170384=CARTESIAN_POINT('Ctrl Pts',(18.3470801915498,-16.8693852963437,
0.0874861271710198));
#170385=CARTESIAN_POINT('Ctrl Pts',(18.4190844938148,-16.8585537446679,
0.0918599639233396));
#170386=CARTESIAN_POINT('Ctrl Pts',(18.4911286186645,-16.8477162025113,
0.0962362196628415));
#170387=CARTESIAN_POINT('Ctrl Pts',(18.563669213288,-16.8406114978773,0.100612475402343));
#170388=CARTESIAN_POINT('Ctrl Pts',(18.6362896320945,-16.8372561185799,
0.104988731141845));
#170389=CARTESIAN_POINT('Ctrl Pts',(18.7090341909997,-16.8338950034698,
0.109372467818922));
#170390=CARTESIAN_POINT('Ctrl Pts',(18.7818583632858,-16.8342960068782,
0.113756204495998));
#170391=CARTESIAN_POINT('Ctrl Pts',(18.8543469087348,-16.8384234999513,
0.118139941173075));
#170392=CARTESIAN_POINT('Ctrl Pts',(18.8963550317498,-16.8408154397493,
0.120680377713149));
#170393=CARTESIAN_POINT('Ctrl Pts',(18.9382505435929,-16.8444579003275,
0.123220814253224));
#170394=CARTESIAN_POINT('Ctrl Pts',(18.9799541383555,-16.8493360796775,
0.125761250793299));
#170395=CARTESIAN_POINT('Ctrl Pts',(19.0521147745614,-16.8577768994061,
0.130157023340392));
#170396=CARTESIAN_POINT('Ctrl Pts',(19.1239757332627,-16.8699525193612,
0.134552795887486));
#170397=CARTESIAN_POINT('Ctrl Pts',(19.1951211678868,-16.8858305324764,
0.13894856843458));
#170398=CARTESIAN_POINT('Ctrl Pts',(19.2661637754886,-16.901685596982,0.143337987739133));
#170399=CARTESIAN_POINT('Ctrl Pts',(19.3364924469683,-16.9212323267425,
0.147727407043687));
#170400=CARTESIAN_POINT('Ctrl Pts',(19.4056976986062,-16.9443866901997,
0.152116826348241));
#170401=CARTESIAN_POINT('Ctrl Pts',(19.4748249321718,-16.9675149507419,
0.156501297270635));
#170402=CARTESIAN_POINT('Ctrl Pts',(19.5428308084352,-16.9942426135354,
0.160885768193029));
#170403=CARTESIAN_POINT('Ctrl Pts',(19.6093188916083,-17.0244352571201,
0.165270239115423));
#170404=CARTESIAN_POINT('Ctrl Pts',(19.6757666906327,-17.0546096074275,
0.169652053551575));
#170405=CARTESIAN_POINT('Ctrl Pts',(19.7406980849853,-17.088244574323,0.174033867987726));
#170406=CARTESIAN_POINT('Ctrl Pts',(19.8037359157051,-17.125157349236,0.178415682423878));
#170407=CARTESIAN_POINT('Ctrl Pts',(19.8667561395948,-17.1620598141978,
0.182796272993961));
#170408=CARTESIAN_POINT('Ctrl Pts',(19.9278834356516,-17.2022380266861,
0.187176863564045));
#170409=CARTESIAN_POINT('Ctrl Pts',(19.9867660616864,-17.24546368492,0.191557454134129));
#170410=CARTESIAN_POINT('Ctrl Pts',(20.0456514706291,-17.2886913860829,
0.195938251739475));
#170411=CARTESIAN_POINT('Ctrl Pts',(20.1022916128046,-17.3349665330801,
0.200319049344822));
#170412=CARTESIAN_POINT('Ctrl Pts',(20.1563658617049,-17.3840190194213,
0.204699846950169));
#170413=CARTESIAN_POINT('Ctrl Pts',(20.2104972294522,-17.4331233201015,
0.209085272009677));
#170414=CARTESIAN_POINT('Ctrl Pts',(20.2620569360997,-17.4850104938254,
0.213470697069185));
#170415=CARTESIAN_POINT('Ctrl Pts',(20.31076005625,-17.5393724039881,0.217856122128693));
#170416=CARTESIAN_POINT('Ctrl Pts',(20.3594904212649,-17.5937647245818,
0.222244000425515));
#170417=CARTESIAN_POINT('Ctrl Pts',(20.4053607162011,-17.6506341638861,
0.226631878722337));
#170418=CARTESIAN_POINT('Ctrl Pts',(20.448127016551,-17.7096403213521,0.231019757019159));
#170419=CARTESIAN_POINT('Ctrl Pts',(20.490969053225,-17.7687509748683,0.23541540596179));
#170420=CARTESIAN_POINT('Ctrl Pts',(20.530695856384,-17.8300054996601,0.239811054904422));
#170421=CARTESIAN_POINT('Ctrl Pts',(20.5671077585182,-17.8930359091734,
0.244206703847054));
#170422=CARTESIAN_POINT('Ctrl Pts',(20.5912140801738,-17.9347648834029,
0.247116821722947));
#170423=CARTESIAN_POINT('Ctrl Pts',(20.6138684164928,-17.9772717133338,
0.25002693959884));
#170424=CARTESIAN_POINT('Ctrl Pts',(20.6350244530402,-18.0204448331188,
0.252937057474733));
#170425=CARTESIAN_POINT('Ctrl Pts',(20.6668851000169,-18.0854628493841,
0.257319647668148));
#170426=CARTESIAN_POINT('Ctrl Pts',(20.6954700316101,-18.1522473407963,
0.261702237861564));
#170427=CARTESIAN_POINT('Ctrl Pts',(20.7205801862023,-18.2204344432736,
0.266084828054979));
#170428=CARTESIAN_POINT('Ctrl Pts',(20.7456525615807,-18.2885189555772,
0.270460824469325));
#170429=CARTESIAN_POINT('Ctrl Pts',(20.767260371406,-18.3580014400402,0.274836820883671));
#170430=CARTESIAN_POINT('Ctrl Pts',(20.7852512326706,-18.428495099863,0.279212817298018));
#170431=CARTESIAN_POINT('Ctrl Pts',(20.8032205403916,-18.4989043063546,
0.283583571149047));
#170432=CARTESIAN_POINT('Ctrl Pts',(20.8175813879169,-18.5703218155193,
0.287954325000076));
#170433=CARTESIAN_POINT('Ctrl Pts',(20.8282307190733,-18.6423442309759,
0.292325078851105));
#170434=CARTESIAN_POINT('Ctrl Pts',(20.8388731539879,-18.7143200065093,
0.296693002310748));
#170435=CARTESIAN_POINT('Ctrl Pts',(20.845808770299,-18.7868994338195,0.301060925770392));
#170436=CARTESIAN_POINT('Ctrl Pts',(20.8489855691776,-18.8596688450712,
0.305428849230036));
#170437=CARTESIAN_POINT('Ctrl Pts',(20.8521613662237,-18.9324153078248,
0.309795395225144));
#170438=CARTESIAN_POINT('Ctrl Pts',(20.8515806778355,-19.0053511525544,
0.314161941220252));
#170439=CARTESIAN_POINT('Ctrl Pts',(20.8472434965741,-19.0780592090538,
0.31852848721536));
#170440=CARTESIAN_POINT('Ctrl Pts',(20.8429062422304,-19.1507684906964,
0.322895106787516));
#170441=CARTESIAN_POINT('Ctrl Pts',(20.8348124001615,-19.2232494936619,
0.327261726359673));
#170442=CARTESIAN_POINT('Ctrl Pts',(20.8230139692876,-19.2950883794611,
0.331628345931829));
#170443=CARTESIAN_POINT('Ctrl Pts',(20.8112033262544,-19.3670016232775,
0.335999485245201));
#170444=CARTESIAN_POINT('Ctrl Pts',(20.7956805170945,-19.4382709444889,
0.340370624558573));
#170445=CARTESIAN_POINT('Ctrl Pts',(20.7765488721863,-19.5084917831654,
0.344741763871945));
#170446=CARTESIAN_POINT('Ctrl Pts',(20.757406850392,-19.5787507091908,0.349115274064266));
#170447=CARTESIAN_POINT('Ctrl Pts',(20.7346522472,-19.6479595605984,0.353488784256587));
#170448=CARTESIAN_POINT('Ctrl Pts',(20.7084377550415,-19.7157306799303,
0.357862294448908));
#170449=CARTESIAN_POINT('Ctrl Pts',(20.682176526986,-19.7836226234244,0.362243601852049));
#170450=CARTESIAN_POINT('Ctrl Pts',(20.6524432899172,-19.8500712742597,
0.366624909255189));
#170451=CARTESIAN_POINT('Ctrl Pts',(20.6194379320409,-19.914711173936,0.37100621665833));
#170452=CARTESIAN_POINT('Ctrl Pts',(20.5965704686666,-19.9594963431776,
0.374041765824275));
#170453=CARTESIAN_POINT('Ctrl Pts',(20.5721332694026,-20.0034137682888,
0.377077314990221));
#170454=CARTESIAN_POINT('Ctrl Pts',(20.5462048528608,-20.0463502964169,
0.380112864156167));
#170455=CARTESIAN_POINT('Ctrl Pts',(20.5087129331597,-20.1084355711665,
0.384502201445418));
#170456=CARTESIAN_POINT('Ctrl Pts',(20.4679538690257,-20.1687127167994,
0.388891538734668));
#170457=CARTESIAN_POINT('Ctrl Pts',(20.424127447363,-20.2268169326104,0.393280876023919));
#170458=CARTESIAN_POINT('Ctrl Pts',(20.3803660122869,-20.2848349904712,
0.397663704726859));
#170459=CARTESIAN_POINT('Ctrl Pts',(20.333546536813,-20.3406861331264,0.4020465334298));
#170460=CARTESIAN_POINT('Ctrl Pts',(20.2839132740569,-20.3940325387807,
0.40642936213274));
#170461=CARTESIAN_POINT('Ctrl Pts',(20.234338311065,-20.4473162831732,0.410807042717946));
#170462=CARTESIAN_POINT('Ctrl Pts',(20.181956453283,-20.4981007839427,0.415184723303152));
#170463=CARTESIAN_POINT('Ctrl Pts',(20.1270525278191,-20.5460808181321,
0.419562403888358));
#170464=CARTESIAN_POINT('Ctrl Pts',(20.0721834146416,-20.5940304301855,
0.42393730876912));
#170465=CARTESIAN_POINT('Ctrl Pts',(20.0147957688626,-20.6391787874444,
0.428312213649883));
#170466=CARTESIAN_POINT('Ctrl Pts',(19.9552106047207,-20.6812581238548,
0.432687118530645));
#170467=CARTESIAN_POINT('Ctrl Pts',(19.8956435930083,-20.72332464093,0.437060690610634));
#170468=CARTESIAN_POINT('Ctrl Pts',(19.8338807856146,-20.7623237154589,
0.441434262690624));
#170469=CARTESIAN_POINT('Ctrl Pts',(19.7702742054051,-20.7980294610899,
0.445807834770614));
#170470=CARTESIAN_POINT('Ctrl Pts',(19.7066660505843,-20.8337360906338,
0.450181515120482));
#170471=CARTESIAN_POINT('Ctrl Pts',(19.6412144536897,-20.8661489951701,
0.454555195470349));
#170472=CARTESIAN_POINT('Ctrl Pts',(19.5742967209256,-20.8950878572009,
0.458928875820217));
#170473=CARTESIAN_POINT('Ctrl Pts',(19.5073097608989,-20.92405665686,0.463307080799151));
#170474=CARTESIAN_POINT('Ctrl Pts',(19.4388540801552,-20.949544046669,0.467685285778084));
#170475=CARTESIAN_POINT('Ctrl Pts',(19.3693269154526,-20.9714179137815,
0.472063490757018));
#170476=CARTESIAN_POINT('Ctrl Pts',(19.2997618805805,-20.9933036951876,
0.476444080463786));
#170477=CARTESIAN_POINT('Ctrl Pts',(19.2291246668025,-21.0115719142762,
0.480824670170555));
#170478=CARTESIAN_POINT('Ctrl Pts',(19.1578249890647,-21.0261411183052,
0.485205259877324));
#170479=CARTESIAN_POINT('Ctrl Pts',(19.0863993186969,-21.0407360673641,
0.489593590460847));
#170480=CARTESIAN_POINT('Ctrl Pts',(19.0143093237696,-21.0516188761684,
0.493981921044371));
#170481=CARTESIAN_POINT('Ctrl Pts',(18.9419715779474,-21.0587597923746,
0.498370251627894));
#170482=CARTESIAN_POINT('Ctrl Pts',(18.892967495442,-21.0635972951603,0.50134305803113));
#170483=CARTESIAN_POINT('Ctrl Pts',(18.843849807491,-21.0667186668706,0.504315864434366));
#170484=CARTESIAN_POINT('Ctrl Pts',(18.7947475334652,-21.0681282421389,
0.507288670837602));
#170485=CARTESIAN_POINT('Ctrl Pts',(18.7222522711166,-21.0702093581544,
0.511677762471143));
#170486=CARTESIAN_POINT('Ctrl Pts',(18.6495091063873,-21.0685648466706,
0.516066854104684));
#170487=CARTESIAN_POINT('Ctrl Pts',(18.5769328970345,-21.0631653002941,
0.520455945738226));
#170488=CARTESIAN_POINT('Ctrl Pts',(18.5044640538338,-21.0577737417766,
0.524838544336597));
#170489=CARTESIAN_POINT('Ctrl Pts',(18.4321621525778,-21.0486382115291,
0.529221142934969));
#170490=CARTESIAN_POINT('Ctrl Pts',(18.3604434250555,-21.0357812949817,
0.533603741533341));
#170491=CARTESIAN_POINT('Ctrl Pts',(18.2888085422895,-21.0229394091672,
0.537981216533957));
#170492=CARTESIAN_POINT('Ctrl Pts',(18.2177559511463,-21.0063848642472,
0.542358691534574));
#170493=CARTESIAN_POINT('Ctrl Pts',(18.1476964269544,-20.9861920067275,
0.54673616653519));
#170494=CARTESIAN_POINT('Ctrl Pts',(18.0776810830246,-20.966011883033,0.551110881054699));
#170495=CARTESIAN_POINT('Ctrl Pts',(18.0086580256524,-20.9421981323211,
0.555485595574208));
#170496=CARTESIAN_POINT('Ctrl Pts',(17.9410261110428,-20.9148758013262,
0.559860310093717));
#170497=CARTESIAN_POINT('Ctrl Pts',(17.8734145608305,-20.8875616972581,
0.564233707359009));
#170498=CARTESIAN_POINT('Ctrl Pts',(17.8071937685407,-20.8567412908305,
0.568607104624301));
#170499=CARTESIAN_POINT('Ctrl Pts',(17.742744149092,-20.8225883668089,0.572980501889593));
#170500=CARTESIAN_POINT('Ctrl Pts',(17.6782926999987,-20.7884344732282,
0.577354023310199));
#170501=CARTESIAN_POINT('Ctrl Pts',(17.6156129486706,-20.7509481017458,
0.581727544730805));
#170502=CARTESIAN_POINT('Ctrl Pts',(17.5550606677984,-20.7103489559778,
0.58610106615141));
#170503=CARTESIAN_POINT('Ctrl Pts',(17.4944453857489,-20.6697075691258,
0.590479137970356));
#170504=CARTESIAN_POINT('Ctrl Pts',(17.4359623948805,-20.6259472108894,
0.594857209789301));
#170505=CARTESIAN_POINT('Ctrl Pts',(17.3799377143115,-20.5793304294076,
0.599235281608247));
#170506=CARTESIAN_POINT('Ctrl Pts',(17.3238823352031,-20.5326881044139,
0.603615752377234));
#170507=CARTESIAN_POINT('Ctrl Pts',(17.2702883027459,-20.4831865672914,
0.607996223146221));
#170508=CARTESIAN_POINT('Ctrl Pts',(17.2194457820157,-20.4311262693854,
0.612376693915207));
#170509=CARTESIAN_POINT('Ctrl Pts',(17.1685131321094,-20.3789736835344,
0.616764929999832));
#170510=CARTESIAN_POINT('Ctrl Pts',(17.1203420532452,-20.3242536410108,
0.621153166084457));
#170511=CARTESIAN_POINT('Ctrl Pts',(17.0751829425931,-20.2673003345457,
0.625541402169081));
#170512=CARTESIAN_POINT('Ctrl Pts',(17.0445739735742,-20.228697227267,0.628515760619066));
#170513=CARTESIAN_POINT('Ctrl Pts',(17.0153478864754,-20.1890687880074,
0.631490119069051));
#170514=CARTESIAN_POINT('Ctrl Pts',(16.987570942693,-20.1485260330615,0.634464477519036));
#170515=CARTESIAN_POINT('Ctrl Pts',(16.9460128045002,-20.0878684810299,
0.638914527908589));
#170516=CARTESIAN_POINT('Ctrl Pts',(16.9075409804496,-20.0249304000689,
0.643364578298142));
#170517=CARTESIAN_POINT('Ctrl Pts',(16.872410053225,-19.9600535055572,0.647814628687695));
#170518=CARTESIAN_POINT('Ctrl Pts',(16.8373354187658,-19.8952805678748,
0.652257548447269));
#170519=CARTESIAN_POINT('Ctrl Pts',(16.8055912687537,-19.828575391364,0.656700468206843));
#170520=CARTESIAN_POINT('Ctrl Pts',(16.7773892711312,-19.7603090100176,
0.661143387966416));
#170521=CARTESIAN_POINT('Ctrl Pts',(16.7492305789296,-19.692147454734,0.665579485425226));
#170522=CARTESIAN_POINT('Ctrl Pts',(16.7246033993889,-19.6224298886478,
0.670015582884037));
#170523=CARTESIAN_POINT('Ctrl Pts',(16.703672960778,-19.5515507599895,0.674451680342847));
#170524=CARTESIAN_POINT('Ctrl Pts',(16.6827615111997,-19.4807359360554,
0.6788837531751));
#170525=CARTESIAN_POINT('Ctrl Pts',(16.6655402725696,-19.4087620863505,
0.683315826007353));
#170526=CARTESIAN_POINT('Ctrl Pts',(16.6521255619375,-19.3360414354493,
0.687747898839606));
#170527=CARTESIAN_POINT('Ctrl Pts',(16.6387183935307,-19.2633616706726,
0.6921774798036));
#170528=CARTESIAN_POINT('Ctrl Pts',(16.6291135877664,-19.1899363945333,
0.696607060767594));
#170529=CARTESIAN_POINT('Ctrl Pts',(16.6233766675227,-19.1161893675075,
0.701036641731588));
#170530=CARTESIAN_POINT('Ctrl Pts',(16.6190996547199,-19.0612091751119,
0.704339001480227));
#170531=CARTESIAN_POINT('Ctrl Pts',(16.6169713924744,-19.0060504437676,
0.707641361228867));
#170532=CARTESIAN_POINT('Ctrl Pts',(16.6170002905271,-18.9508909049915,
0.710943720977506));
#170533=CARTESIAN_POINT('',(20.3539256943887,-17.5890877707427,0.));
#170534=CARTESIAN_POINT('Origin',(18.734,-18.952,0.));
#170535=CARTESIAN_POINT('',(16.6170006157907,-18.95038529957,0.489056278967188));
#170536=CARTESIAN_POINT('Ctrl Pts',(16.6170006157907,-18.95038529957,0.489056278967188));
#170537=CARTESIAN_POINT('Ctrl Pts',(16.6169439873006,-19.0246297083089,
0.484575909845401));
#170538=CARTESIAN_POINT('Ctrl Pts',(16.6207979226554,-19.0990186013218,
0.480095540723614));
#170539=CARTESIAN_POINT('Ctrl Pts',(16.6285774659328,-19.1730994189093,
0.475615171601827));
#170540=CARTESIAN_POINT('Ctrl Pts',(16.6360763306427,-19.2445074706266,
0.471296449962676));
#170541=CARTESIAN_POINT('Ctrl Pts',(16.6472223424282,-19.3156287493154,
0.466977728323525));
#170542=CARTESIAN_POINT('Ctrl Pts',(16.661976057202,-19.3860573469854,0.462659006684374));
#170543=CARTESIAN_POINT('Ctrl Pts',(16.6767199431933,-19.4564390258024,
0.458343162135962));
#170544=CARTESIAN_POINT('Ctrl Pts',(16.6950666659208,-19.5261284537002,
0.45402731758755));
#170545=CARTESIAN_POINT('Ctrl Pts',(16.7169252820585,-19.5947274556461,
0.449711473039138));
#170546=CARTESIAN_POINT('Ctrl Pts',(16.7387770070935,-19.6633048312107,
0.445396989095061));
#170547=CARTESIAN_POINT('Ctrl Pts',(16.7641382780629,-19.7307919900002,
0.441082505150984));
#170548=CARTESIAN_POINT('Ctrl Pts',(16.7928681311363,-19.7968053430712,
0.436768021206907));
#170549=CARTESIAN_POINT('Ctrl Pts',(16.8215990084979,-19.8628210496769,
0.432453383441104));
#170550=CARTESIAN_POINT('Ctrl Pts',(16.8536985050873,-19.9273623922351,
0.428138745675302));
#170551=CARTESIAN_POINT('Ctrl Pts',(16.8889780480199,-19.9900669519407,
0.4238241079095));
#170552=CARTESIAN_POINT('Ctrl Pts',(16.9242924792532,-20.0528335208266,
0.419505203354288));
#170553=CARTESIAN_POINT('Ctrl Pts',(16.9627929852641,-20.1137592505177,
0.415186298799076));
#170554=CARTESIAN_POINT('Ctrl Pts',(17.0042462475466,-20.1725084825078,
0.410867394243864));
#170555=CARTESIAN_POINT('Ctrl Pts',(17.0457241648865,-20.2312926566376,
0.406545920944149));
#170556=CARTESIAN_POINT('Ctrl Pts',(17.0901580230918,-20.287897369665,0.402224447644434));
#170557=CARTESIAN_POINT('Ctrl Pts',(17.1372743346935,-20.3420201976056,
0.397902974344718));
#170558=CARTESIAN_POINT('Ctrl Pts',(17.1844652344071,-20.3962287054183,
0.393574659878474));
#170559=CARTESIAN_POINT('Ctrl Pts',(17.2343467098505,-20.4479471389023,
0.389246345412231));
#170560=CARTESIAN_POINT('Ctrl Pts',(17.2866094096999,-20.4969108320906,
0.384918030945987));
#170561=CARTESIAN_POINT('Ctrl Pts',(17.3002561753745,-20.5096961655967,
0.383787827312092));
#170562=CARTESIAN_POINT('Ctrl Pts',(17.3140651344993,-20.5222938940567,
0.382657623678198));
#170563=CARTESIAN_POINT('Ctrl Pts',(17.328030443818,-20.5346997842577,0.381527420044303));
#170564=CARTESIAN_POINT('Ctrl Pts',(17.3823195205318,-20.5829267378796,
0.377133839466686));
#170565=CARTESIAN_POINT('Ctrl Pts',(17.4391958931759,-20.628448704409,0.372740258889068));
#170566=CARTESIAN_POINT('Ctrl Pts',(17.498359246263,-20.6709767094712,0.368346678311451));
#170567=CARTESIAN_POINT('Ctrl Pts',(17.5574363013708,-20.7134426815229,
0.363959506382193));
#170568=CARTESIAN_POINT('Ctrl Pts',(17.6187933267003,-20.7529230838071,
0.359572334452935));
#170569=CARTESIAN_POINT('Ctrl Pts',(17.6820956518213,-20.7891679951172,
0.355185162523678));
#170570=CARTESIAN_POINT('Ctrl Pts',(17.7453255105041,-20.8253714144342,
0.350803012885832));
#170571=CARTESIAN_POINT('Ctrl Pts',(17.8104958295947,-20.8583464631661,
0.346420863247986));
#170572=CARTESIAN_POINT('Ctrl Pts',(17.8772429582996,-20.8878864562512,
0.342038713610141));
#170573=CARTESIAN_POINT('Ctrl Pts',(17.9439489461201,-20.9174082417899,
0.33765926499503));
#170574=CARTESIAN_POINT('Ctrl Pts',(18.0122293762549,-20.9434989788705,
0.33327981637992));
#170575=CARTESIAN_POINT('Ctrl Pts',(18.081697252437,-20.9659985415888,0.32890036776481));
#170576=CARTESIAN_POINT('Ctrl Pts',(18.1511450535803,-20.9884916023148,
0.324522184736119));
#170577=CARTESIAN_POINT('Ctrl Pts',(18.2217791621869,-21.0073954011508,
0.320144001707428));
#170578=CARTESIAN_POINT('Ctrl Pts',(18.2931954849952,-21.0225990388174,
0.315765818678737));
#170579=CARTESIAN_POINT('Ctrl Pts',(18.3646145496345,-21.0378032601853,
0.311387467561894));
#170580=CARTESIAN_POINT('Ctrl Pts',(18.4368154173397,-21.0493069401342,
0.307009116445052));
#170581=CARTESIAN_POINT('Ctrl Pts',(18.5093834475756,-21.0570502142175,
0.302630765328209));
#170582=CARTESIAN_POINT('Ctrl Pts',(18.5820274277171,-21.0648015924333,
0.298247831816703));
#170583=CARTESIAN_POINT('Ctrl Pts',(18.6550388584148,-21.0687846559847,
0.293864898305197));
#170584=CARTESIAN_POINT('Ctrl Pts',(18.7279984288039,-21.0689914929312,
0.289481964793692));
#170585=CARTESIAN_POINT('Ctrl Pts',(18.8009983528725,-21.0691984442785,
0.285096607097214));
#170586=CARTESIAN_POINT('Ctrl Pts',(18.8739458788801,-21.0656250338833,
0.280711249400737));
#170587=CARTESIAN_POINT('Ctrl Pts',(18.946424858768,-21.0583154273227,0.27632589170426));
#170588=CARTESIAN_POINT('Ctrl Pts',(19.0190319251111,-21.0509929030637,
0.271932784106734));
#170589=CARTESIAN_POINT('Ctrl Pts',(19.091168316046,-21.0399210701979,0.267539676509208));
#170590=CARTESIAN_POINT('Ctrl Pts',(19.1624267103003,-21.0251954934114,
0.263146568911682));
#170591=CARTESIAN_POINT('Ctrl Pts',(19.2099795641009,-21.0153686764113,
0.260214917062078));
#170592=CARTESIAN_POINT('Ctrl Pts',(19.2571416600211,-21.003915800001,0.257283265212473));
#170593=CARTESIAN_POINT('Ctrl Pts',(19.3037962227791,-20.9908774520571,
0.254351613362869));
#170594=CARTESIAN_POINT('Ctrl Pts',(19.3728933262966,-20.971567184758,0.250009730396774));
#170595=CARTESIAN_POINT('Ctrl Pts',(19.4411588243116,-20.9486979955926,
0.245667847430679));
#170596=CARTESIAN_POINT('Ctrl Pts',(19.5081940324577,-20.9223584953269,
0.241325964464583));
#170597=CARTESIAN_POINT('Ctrl Pts',(19.5751282952576,-20.8960586585461,
0.236990619747436));
#170598=CARTESIAN_POINT('Ctrl Pts',(19.6408354886486,-20.8662990562217,
0.232655275030289));
#170599=CARTESIAN_POINT('Ctrl Pts',(19.7049304077652,-20.833218526189,0.228319930313142));
#170600=CARTESIAN_POINT('Ctrl Pts',(19.7689516598175,-20.8001760170412,
0.223989568395299));
#170601=CARTESIAN_POINT('Ctrl Pts',(19.8313638797399,-20.7638203813565,
0.219659206477455));
#170602=CARTESIAN_POINT('Ctrl Pts',(19.8918019327492,-20.7243384791067,
0.215328844559612));
#170603=CARTESIAN_POINT('Ctrl Pts',(19.952202841651,-20.6848808417024,0.211001144001965));
#170604=CARTESIAN_POINT('Ctrl Pts',(20.0106315769706,-20.6423010159659,
0.206673443444318));
#170605=CARTESIAN_POINT('Ctrl Pts',(20.0667491221407,-20.5968309267013,
0.202345742886671));
#170606=CARTESIAN_POINT('Ctrl Pts',(20.1228516204485,-20.5513730293844,
0.198019202720377));
#170607=CARTESIAN_POINT('Ctrl Pts',(20.1766437747633,-20.5030267163447,
0.193692662554083));
#170608=CARTESIAN_POINT('Ctrl Pts',(20.2278184819436,-20.4520651129214,
0.189366122387789));
#170609=CARTESIAN_POINT('Ctrl Pts',(20.2789971971884,-20.401099518124,0.18503924336167));
#170610=CARTESIAN_POINT('Ctrl Pts',(20.3275577103422,-20.3475185761416,
0.180712364335552));
#170611=CARTESIAN_POINT('Ctrl Pts',(20.3732300428321,-20.2916319892705,
0.176385485309434));
#170612=CARTESIAN_POINT('Ctrl Pts',(20.4189571873855,-20.2356783320532,
0.172053413529732));
#170613=CARTESIAN_POINT('Ctrl Pts',(20.461788919467,-20.1774138895481,0.167721341750031));
#170614=CARTESIAN_POINT('Ctrl Pts',(20.5014963977798,-20.11718045119,0.163389269970329));
#170615=CARTESIAN_POINT('Ctrl Pts',(20.5412283831299,-20.0569098373883,
0.159054524481558));
#170616=CARTESIAN_POINT('Ctrl Pts',(20.5778320305151,-19.994668236685,0.154719778992786));
#170617=CARTESIAN_POINT('Ctrl Pts',(20.6111241303052,-19.9308227620085,
0.150385033504014));
#170618=CARTESIAN_POINT('Ctrl Pts',(20.6444832806256,-19.8668487020833,
0.146041557806415));
#170619=CARTESIAN_POINT('Ctrl Pts',(20.6745173629453,-19.8012647680478,
0.141698082108817));
#170620=CARTESIAN_POINT('Ctrl Pts',(20.7010912717234,-19.7344582600432,
0.137354606411219));
#170621=CARTESIAN_POINT('Ctrl Pts',(20.721849646991,-19.6822719379232,0.133961673167958));
#170622=CARTESIAN_POINT('Ctrl Pts',(20.7404975804328,-19.6293400279684,
0.130568739924696));
#170623=CARTESIAN_POINT('Ctrl Pts',(20.7569922863659,-19.5758519129603,
0.127175806681435));
#170624=CARTESIAN_POINT('Ctrl Pts',(20.7789195445138,-19.5047474197739,
0.12266540659273));
#170625=CARTESIAN_POINT('Ctrl Pts',(20.7971288584811,-19.4323721967961,
0.118155006504025));
#170626=CARTESIAN_POINT('Ctrl Pts',(20.8114809541406,-19.3591386559676,
0.113644606415321));
#170627=CARTESIAN_POINT('Ctrl Pts',(20.8265483375802,-19.2822552609233,
0.108909414481349));
#170628=CARTESIAN_POINT('Ctrl Pts',(20.8373637838653,-19.2044262083738,
0.104174222547377));
#170629=CARTESIAN_POINT('Ctrl Pts',(20.8438249724136,-19.1261481719107,
0.0994390306134055));
#170630=CARTESIAN_POINT('Ctrl Pts',(20.8499589701725,-19.0518340891932,
0.0949436260150769));
#170631=CARTESIAN_POINT('Ctrl Pts',(20.852168892667,-18.9771159048155,0.0904482214167483));
#170632=CARTESIAN_POINT('Ctrl Pts',(20.8504195396485,-18.9024285143068,
0.0859528168184197));
#170633=CARTESIAN_POINT('Ctrl Pts',(20.848671831534,-18.8278113518075,0.0814616392162973));
#170634=CARTESIAN_POINT('Ctrl Pts',(20.842972258343,-18.7532253737159,0.0769704616141749));
#170635=CARTESIAN_POINT('Ctrl Pts',(20.833337630623,-18.6791071407126,0.0724792840120526));
#170636=CARTESIAN_POINT('Ctrl Pts',(20.8237095451823,-18.6050392368129,
0.067991156090602));
#170637=CARTESIAN_POINT('Ctrl Pts',(20.810151776091,-18.5314388917089,0.0635030281691514));
#170638=CARTESIAN_POINT('Ctrl Pts',(20.7927329926196,-18.4587379346641,
0.0590149002477008));
#170639=CARTESIAN_POINT('Ctrl Pts',(20.775321490724,-18.3860673688074,0.0545286484988));
#170640=CARTESIAN_POINT('Ctrl Pts',(20.7540522902898,-18.3142958801147,
0.0500423967498992));
#170641=CARTESIAN_POINT('Ctrl Pts',(20.7290449663564,-18.2438442387327,
0.0455561450009983));
#170642=CARTESIAN_POINT('Ctrl Pts',(20.704034536135,-18.1733838461909,0.0410693359917531));
#170643=CARTESIAN_POINT('Ctrl Pts',(20.6752851982857,-18.1042440551513,
0.0365825269825079));
#170644=CARTESIAN_POINT('Ctrl Pts',(20.6429658444502,-18.0368287566131,
0.0320957179732627));
#170645=CARTESIAN_POINT('Ctrl Pts',(20.610644937254,-17.9694102179022,0.0276086933151065));
#170646=CARTESIAN_POINT('Ctrl Pts',(20.5747538739462,-17.9037167392705,
0.0231216686569502));
#170647=CARTESIAN_POINT('Ctrl Pts',(20.5355082322583,-17.8401290141812,
0.018634643998794));
#170648=CARTESIAN_POINT('Ctrl Pts',(20.496235508383,-17.7764974091956,0.0141445229855435));
#170649=CARTESIAN_POINT('Ctrl Pts',(20.4536038273032,-17.7149748381304,
0.00965440197229298));
#170650=CARTESIAN_POINT('Ctrl Pts',(20.4078725225403,-17.6559136686608,
0.0051642809590425));
#170651=CARTESIAN_POINT('Ctrl Pts',(20.3903400101855,-17.6332707397352,
0.003442853972695));
#170652=CARTESIAN_POINT('Ctrl Pts',(20.3723523439628,-17.6109892567414,
0.0017214269863475));
#170653=CARTESIAN_POINT('Ctrl Pts',(20.3539256943887,-17.5890877707427,
0.));
#170654=CARTESIAN_POINT('Ctrl Pts',(16.6170005688548,-18.9504480557866,
0.490010467130569));
#170655=CARTESIAN_POINT('Ctrl Pts',(16.6170514726509,-18.881010439057,0.494577327914728));
#170656=CARTESIAN_POINT('Ctrl Pts',(16.6205187004332,-18.8116103989348,
0.4990989912545));
#170657=CARTESIAN_POINT('Ctrl Pts',(16.6297024906936,-18.7192634938256,
0.504962249724503));
#170658=CARTESIAN_POINT('Ctrl Pts',(16.6323977830403,-18.696065413783,0.506421957048484));
#170659=CARTESIAN_POINT('Ctrl Pts',(16.6362852621,-18.6668342307142,0.508240701531616));
#170660=CARTESIAN_POINT('Ctrl Pts',(16.6371204756518,-18.6607562875839,
0.508617738798077));
#170661=CARTESIAN_POINT('Ctrl Pts',(16.6385603498371,-18.6506055337555,
0.509245444537397));
#170662=CARTESIAN_POINT('Ctrl Pts',(16.6391504857804,-18.646530745929,0.509496887875124));
#170663=CARTESIAN_POINT('Ctrl Pts',(16.640246229322,-18.6391173555341,0.509953340961934));
#170664=CARTESIAN_POINT('Ctrl Pts',(16.6407479422945,-18.635778203287,0.510158565565758));
#170665=CARTESIAN_POINT('Ctrl Pts',(16.6417945762328,-18.628923976198,0.510579043266343));
#170666=CARTESIAN_POINT('Ctrl Pts',(16.6423403650127,-18.6254090872902,
0.510794240062932));
#170667=CARTESIAN_POINT('Ctrl Pts',(16.6435932922711,-18.6174721992057,
0.51127920709439));
#170668=CARTESIAN_POINT('Ctrl Pts',(16.644305601679,-18.6130510721356,0.511548680018681));
#170669=CARTESIAN_POINT('Ctrl Pts',(16.6465009453004,-18.5996951238187,
0.512360802943133));
#170670=CARTESIAN_POINT('Ctrl Pts',(16.6480273156697,-18.5907673934348,
0.51290103930551));
#170671=CARTESIAN_POINT('Ctrl Pts',(16.6601810646459,-18.5223272731401,
0.517024246191999));
#170672=CARTESIAN_POINT('Ctrl Pts',(16.6732969949638,-18.4632790241335,
0.520475810165007));
#170673=CARTESIAN_POINT('Ctrl Pts',(16.6938140193657,-18.3865902843641,
0.524913687944728));
#170674=CARTESIAN_POINT('Ctrl Pts',(16.6989488457143,-18.3683787117175,
0.525964161652573));
#170675=CARTESIAN_POINT('Ctrl Pts',(16.7159637402776,-18.3109894546689,
0.529270380732414));
#170676=CARTESIAN_POINT('Ctrl Pts',(16.7287365520966,-18.2720856477678,
0.531505691843595));
#170677=CARTESIAN_POINT('Ctrl Pts',(16.7435546348056,-18.2310120132186,
0.533880985320879));
#170678=CARTESIAN_POINT('Ctrl Pts',(16.7444845345614,-18.2284499731407,
0.53402921203008));
#170679=CARTESIAN_POINT('Ctrl Pts',(16.7454193692601,-18.2258897638472,
0.53417740218321));
#170680=CARTESIAN_POINT('Origin',(18.734,-18.952,0.));
#170681=CARTESIAN_POINT('',(16.7454191832631,-18.2258902732327,1.55576066005867));
#170682=CARTESIAN_POINT('',(16.7454193692336,-18.2258897639197,1.33163196665472));
#170683=CARTESIAN_POINT('',(16.7454193692319,-18.2258897639242,0.));
#170684=CARTESIAN_POINT('',(16.6170003908423,-18.9507135995066,1.51094372094299));
#170685=CARTESIAN_POINT('Ctrl Pts',(16.7454191832631,-18.2258902732327,
1.55576066005867));
#170686=CARTESIAN_POINT('Ctrl Pts',(16.7161439153024,-18.3060658088651,
1.55013147756805));
#170687=CARTESIAN_POINT('Ctrl Pts',(16.6917244024261,-18.3879928335124,
1.54446140094733));
#170688=CARTESIAN_POINT('Ctrl Pts',(16.66602267378,-18.4982088831121,1.53708123670477));
#170689=CARTESIAN_POINT('Ctrl Pts',(16.6602607693149,-18.5253124031872,
1.53528610611094));
#170690=CARTESIAN_POINT('Ctrl Pts',(16.6468711293343,-18.5949949214027,
1.53073310070744));
#170691=CARTESIAN_POINT('Ctrl Pts',(16.6400127044978,-18.6377113678681,
1.52800094154312));
#170692=CARTESIAN_POINT('Ctrl Pts',(16.6335056815886,-18.6880513304626,
1.52487274099519));
#170693=CARTESIAN_POINT('Ctrl Pts',(16.6325834866175,-18.69549673892,1.52441241354194));
#170694=CARTESIAN_POINT('Ctrl Pts',(16.6311572000861,-18.7075362692343,
1.52367199847394));
#170695=CARTESIAN_POINT('Ctrl Pts',(16.6306285482168,-18.712127338848,1.52339058146462));
#170696=CARTESIAN_POINT('Ctrl Pts',(16.6297175154369,-18.7202738430539,
1.52289291772099));
#170697=CARTESIAN_POINT('Ctrl Pts',(16.6293291050042,-18.723828548914,1.52267633544412));
#170698=CARTESIAN_POINT('Ctrl Pts',(16.628593654091,-18.7307210376584,1.5222575051168));
#170699=CARTESIAN_POINT('Ctrl Pts',(16.6282455448752,-18.7340586417142,
1.52205519562351));
#170700=CARTESIAN_POINT('Ctrl Pts',(16.6274962875417,-18.7414117890565,
1.52161056542226));
#170701=CARTESIAN_POINT('Ctrl Pts',(16.6270986812446,-18.7454276910519,
1.52136844218618));
#170702=CARTESIAN_POINT('Ctrl Pts',(16.6261439823156,-18.7553599193906,
1.52077131891836));
#170703=CARTESIAN_POINT('Ctrl Pts',(16.6256003086776,-18.7612775417385,
1.52041704492448));
#170704=CARTESIAN_POINT('Ctrl Pts',(16.6234160973003,-18.7862031920286,
1.51893079183033));
#170705=CARTESIAN_POINT('Ctrl Pts',(16.6220075766885,-18.8052313011762,
1.51781084192716));
#170706=CARTESIAN_POINT('Ctrl Pts',(16.6183136906642,-18.8663454677846,
1.51425337207207));
#170707=CARTESIAN_POINT('Ctrl Pts',(16.6170276587882,-18.9084831004558,
1.51186056911543));
#170708=CARTESIAN_POINT('Ctrl Pts',(16.617000441359,-18.9506329908568,1.50950272412443));
#170709=CARTESIAN_POINT('Ctrl Pts',(16.7454193692319,-18.2258897639242,
0.755484063719885));
#170710=CARTESIAN_POINT('Ctrl Pts',(16.7570609226712,-18.1940073216569,
0.757536137213414));
#170711=CARTESIAN_POINT('Ctrl Pts',(16.7694632458252,-18.1624216014919,
0.759588210706942));
#170712=CARTESIAN_POINT('Ctrl Pts',(16.7826102689518,-18.1311668150229,
0.761640284200471));
#170713=CARTESIAN_POINT('Ctrl Pts',(16.8107255694665,-18.0643275232961,
0.766028704483401));
#170714=CARTESIAN_POINT('Ctrl Pts',(16.8423337670678,-17.9988040424724,
0.770417124766331));
#170715=CARTESIAN_POINT('Ctrl Pts',(16.8772900689618,-17.9349861200633,
0.774805545049261));
#170716=CARTESIAN_POINT('Ctrl Pts',(16.9121945047598,-17.8712628869177,
0.779187454053404));
#170717=CARTESIAN_POINT('Ctrl Pts',(16.9504369534201,-17.8092406080986,
0.783569363057546));
#170718=CARTESIAN_POINT('Ctrl Pts',(16.9918247170348,-17.7492887780415,
0.787951272061689));
#170719=CARTESIAN_POINT('Ctrl Pts',(17.0331638610962,-17.6894073753507,
0.792328033494681));
#170720=CARTESIAN_POINT('Ctrl Pts',(17.0776407074798,-17.6315919847378,
0.796704794927673));
#170721=CARTESIAN_POINT('Ctrl Pts',(17.1250176914327,-17.5761857208484,
0.801081556360666));
#170722=CARTESIAN_POINT('Ctrl Pts',(17.1723646383057,-17.5208145846146,
0.805455542920259));
#170723=CARTESIAN_POINT('Ctrl Pts',(17.2226077618452,-17.4678499102326,
0.809829529479853));
#170724=CARTESIAN_POINT('Ctrl Pts',(17.2754682696248,-17.4176029876565,
0.814203516039446));
#170725=CARTESIAN_POINT('Ctrl Pts',(17.328312696826,-17.3673713505858,0.818576171998238));
#170726=CARTESIAN_POINT('Ctrl Pts',(17.3837725781244,-17.319856156042,0.82294882795703));
#170727=CARTESIAN_POINT('Ctrl Pts',(17.4415323794237,-17.2753317412911,
0.827321483915821));
#170728=CARTESIAN_POINT('Ctrl Pts',(17.499293658057,-17.2308061877305,0.831694251714908));
#170729=CARTESIAN_POINT('Ctrl Pts',(17.5593545902617,-17.1892718587225,
0.836067019513995));
#170730=CARTESIAN_POINT('Ctrl Pts',(17.6213680340651,-17.1509616582705,
0.840439787313082));
#170731=CARTESIAN_POINT('Ctrl Pts',(17.6834458140768,-17.112611712678,0.844817091665573));
#170732=CARTESIAN_POINT('Ctrl Pts',(17.7474797388099,-17.0774928279821,
0.849194396018063));
#170733=CARTESIAN_POINT('Ctrl Pts',(17.8130959747628,-17.0457930919489,
0.853571700370554));
#170734=CARTESIAN_POINT('Ctrl Pts',(17.8787480372569,-17.0140760478229,
0.857951394736325));
#170735=CARTESIAN_POINT('Ctrl Pts',(17.9459836862096,-16.9857820564869,
0.862331089102096));
#170736=CARTESIAN_POINT('Ctrl Pts',(18.0144094204716,-16.9610508801443,
0.866710783467866));
#170737=CARTESIAN_POINT('Ctrl Pts',(18.0829563836852,-16.9362758879098,
0.871098237279143));
#170738=CARTESIAN_POINT('Ctrl Pts',(18.1526971808355,-16.9150764562721,
0.87548569109042));
#170739=CARTESIAN_POINT('Ctrl Pts',(18.2232240532573,-16.8975421804697,
0.879873144901697));
#170740=CARTESIAN_POINT('Ctrl Pts',(18.2711423552575,-16.8856288105101,
0.882854126895099));
#170741=CARTESIAN_POINT('Ctrl Pts',(18.3194232835352,-16.8754063197374,
0.885835108888502));
#170742=CARTESIAN_POINT('Ctrl Pts',(18.3679374540643,-16.8668891606288,
0.888816090881905));
#170743=CARTESIAN_POINT('Ctrl Pts',(18.4393551942814,-16.8543510454768,
0.893204396304316));
#170744=CARTESIAN_POINT('Ctrl Pts',(18.5115571786451,-16.8454619390755,
0.897592701726727));
#170745=CARTESIAN_POINT('Ctrl Pts',(18.5841373366349,-16.8403110593345,
0.901981007149137));
#170746=CARTESIAN_POINT('Ctrl Pts',(18.6566098160556,-16.8351678213426,
0.906362802163441));
#170747=CARTESIAN_POINT('Ctrl Pts',(18.7294588781678,-16.8337518343611,
0.910744597177744));
#170748=CARTESIAN_POINT('Ctrl Pts',(18.8022695511268,-16.8361010732105,
0.915126392192048));
#170749=CARTESIAN_POINT('Ctrl Pts',(18.8749947199703,-16.8384475532667,
0.919503041511469));
#170750=CARTESIAN_POINT('Ctrl Pts',(18.9476811095042,-16.8445504600611,
0.92387969083089));
#170751=CARTESIAN_POINT('Ctrl Pts',(19.0199116428383,-16.8543957636176,
0.928256340150311));
#170752=CARTESIAN_POINT('Ctrl Pts',(19.0920964007967,-16.8642348278118,
0.932630215812144));
#170753=CARTESIAN_POINT('Ctrl Pts',(19.1638253990005,-16.8778115180026,
0.937004091473978));
#170754=CARTESIAN_POINT('Ctrl Pts',(19.2346860042546,-16.8950599121162,
0.941377967135811));
#170755=CARTESIAN_POINT('Ctrl Pts',(19.3055250750244,-16.9123030644558,
0.945750513580145));
#170756=CARTESIAN_POINT('Ctrl Pts',(19.3754958083888,-16.9332155914393,
0.950123060024478));
#170757=CARTESIAN_POINT('Ctrl Pts',(19.4441967552487,-16.9576806753094,
0.954495606468812));
#170758=CARTESIAN_POINT('Ctrl Pts',(19.512899483717,-16.9821463936279,0.958868266305556));
#170759=CARTESIAN_POINT('Ctrl Pts',(19.5803319065734,-17.0101646880441,
0.9632409261423));
#170760=CARTESIAN_POINT('Ctrl Pts',(19.6461103054445,-17.0415697367603,
0.967613585979044));
#170761=CARTESIAN_POINT('Ctrl Pts',(19.7119569957736,-17.073007390353,0.971990785532794));
#170762=CARTESIAN_POINT('Ctrl Pts',(19.776145797365,-17.1078386101949,0.976367985086543));
#170763=CARTESIAN_POINT('Ctrl Pts',(19.8383162282127,-17.1458508732372,
0.980745184640292));
#170764=CARTESIAN_POINT('Ctrl Pts',(19.9005206278453,-17.1838839054839,
0.985124775815712));
#170765=CARTESIAN_POINT('Ctrl Pts',(19.9607040628243,-17.2251011686578,
0.989504366991133));
#170766=CARTESIAN_POINT('Ctrl Pts',(20.0185360408569,-17.2692474454811,
0.993883958166554));
#170767=CARTESIAN_POINT('Ctrl Pts',(20.0764705311577,-17.3134719754634,
0.99827131255258));
#170768=CARTESIAN_POINT('Ctrl Pts',(20.1320448727674,-17.3606355747934,
1.00265866693861));
#170769=CARTESIAN_POINT('Ctrl Pts',(20.1849630396155,-17.4104438843592,
1.00704602132463));
#170770=CARTESIAN_POINT('Ctrl Pts',(20.2209299975094,-17.4442971615911,
1.01002798007087));
#170771=CARTESIAN_POINT('Ctrl Pts',(20.2556706880075,-17.4793713845315,
1.0130099388171));
#170772=CARTESIAN_POINT('Ctrl Pts',(20.2891028481193,-17.5155654794696,
1.01599189756334));
#170773=CARTESIAN_POINT('Ctrl Pts',(20.3382999033156,-17.568826856554,1.02037999538716));
#170774=CARTESIAN_POINT('Ctrl Pts',(20.3848536164314,-17.6247226321812,
1.02476809321097));
#170775=CARTESIAN_POINT('Ctrl Pts',(20.4284691662198,-17.6829597150876,
1.02915619103479));
#170776=CARTESIAN_POINT('Ctrl Pts',(20.4720199640021,-17.741110338739,1.03353777425227));
#170777=CARTESIAN_POINT('Ctrl Pts',(20.5126409708618,-17.8015949865701,
1.03791935746975));
#170778=CARTESIAN_POINT('Ctrl Pts',(20.5500756303539,-17.8640853411987,
1.04230094068724));
#170779=CARTESIAN_POINT('Ctrl Pts',(20.5874662819946,-17.9265022327246,
1.04667737295463));
#170780=CARTESIAN_POINT('Ctrl Pts',(20.6216777807228,-17.9909197353098,
1.05105380522201));
#170781=CARTESIAN_POINT('Ctrl Pts',(20.6524961553591,-18.0569796081249,
1.0554302374894));
#170782=CARTESIAN_POINT('Ctrl Pts',(20.6832949761952,-18.1229975669334,
1.05980389297562));
#170783=CARTESIAN_POINT('Ctrl Pts',(20.7107047410892,-18.1906553922989,
1.06417754846184));
#170784=CARTESIAN_POINT('Ctrl Pts',(20.7345575147539,-18.2595704872252,
1.06855120394807));
#170785=CARTESIAN_POINT('Ctrl Pts',(20.7584030239131,-18.3284645936452,
1.07292352741122));
#170786=CARTESIAN_POINT('Ctrl Pts',(20.778693534838,-18.3986147538376,1.07729585087438));
#170787=CARTESIAN_POINT('Ctrl Pts',(20.7953099596495,-18.4696202219725,
1.08166817433753));
#170788=CARTESIAN_POINT('Ctrl Pts',(20.8119268059284,-18.5406274911261,
1.08604060870252));
#170789=CARTESIAN_POINT('Ctrl Pts',(20.8248692730975,-18.6124896411231,
1.0904130430675));
#170790=CARTESIAN_POINT('Ctrl Pts',(20.834069074416,-18.6847943064204,1.09478547743249));
#170791=CARTESIAN_POINT('Ctrl Pts',(20.8432784226837,-18.7571740047468,
1.09916244922245));
#170792=CARTESIAN_POINT('Ctrl Pts',(20.8487372896263,-18.8299966556521,
1.10353942101241));
#170793=CARTESIAN_POINT('Ctrl Pts',(20.8504292339814,-18.9028441504098,
1.10791639280238));
#170794=CARTESIAN_POINT('Ctrl Pts',(20.8521221021995,-18.9757314225439,
1.11229575457781));
#170795=CARTESIAN_POINT('Ctrl Pts',(20.8500439663687,-19.0486430829948,
1.11667511635325));
#170796=CARTESIAN_POINT('Ctrl Pts',(20.8442305173074,-19.1211631278514,
1.12105447812869));
#170797=CARTESIAN_POINT('Ctrl Pts',(20.8384067629935,-19.1938117258918,
1.12544160301156));
#170798=CARTESIAN_POINT('Ctrl Pts',(20.8288345361362,-19.2660668433993,
1.12982872789443));
#170799=CARTESIAN_POINT('Ctrl Pts',(20.8156010959129,-19.3375202685906,
1.1342158527773));
#170800=CARTESIAN_POINT('Ctrl Pts',(20.8066002282646,-19.3861200893717,
1.13719980326646));
#170801=CARTESIAN_POINT('Ctrl Pts',(20.7959066877834,-19.4343492460054,
1.14018375375562));
#170802=CARTESIAN_POINT('Ctrl Pts',(20.7835610200617,-19.482083601938,1.14316770424478));
#170803=CARTESIAN_POINT('Ctrl Pts',(20.7654052834301,-19.5522825100999,
1.14755594961346));
#170804=CARTESIAN_POINT('Ctrl Pts',(20.7436033966526,-19.6216845776909,
1.15194419498214));
#170805=CARTESIAN_POINT('Ctrl Pts',(20.7182422535391,-19.689883242302,1.15633244035082));
#170806=CARTESIAN_POINT('Ctrl Pts',(20.6929187482514,-19.7579806950138,
1.16071417323644));
#170807=CARTESIAN_POINT('Ctrl Pts',(20.6640466392656,-19.8248778416993,
1.16509590612206));
#170808=CARTESIAN_POINT('Ctrl Pts',(20.6317631511028,-19.8901812310617,
1.16947763900768));
#170809=CARTESIAN_POINT('Ctrl Pts',(20.5995175958008,-19.9554078894224,
1.17385422338941));
#170810=CARTESIAN_POINT('Ctrl Pts',(20.563868836638,-20.0190440802309,1.17823080777115));
#170811=CARTESIAN_POINT('Ctrl Pts',(20.5250023084886,-20.0807159655947,
1.18260739215288));
#170812=CARTESIAN_POINT('Ctrl Pts',(20.4861604270437,-20.1423487425328,
1.18698120118042));
#170813=CARTESIAN_POINT('Ctrl Pts',(20.4441050817949,-20.2020192784522,
1.19135501020796));
#170814=CARTESIAN_POINT('Ctrl Pts',(20.3990671042951,-20.2593792633335,
1.1957288192355));
#170815=CARTESIAN_POINT('Ctrl Pts',(20.3540428305095,-20.316721795281,1.20010129744332));
#170816=CARTESIAN_POINT('Ctrl Pts',(20.3060380239067,-20.3717547927606,
1.20447377565114));
#170817=CARTESIAN_POINT('Ctrl Pts',(20.2553252151259,-20.4241611969557,
1.20884625385896));
#170818=CARTESIAN_POINT('Ctrl Pts',(20.2046111087068,-20.4765689421249,
1.21321884394967));
#170819=CARTESIAN_POINT('Ctrl Pts',(20.1511891994121,-20.5263496153214,
1.21759143404038));
#170820=CARTESIAN_POINT('Ctrl Pts',(20.0953692846382,-20.5732225852251,
1.22196402413109));
#170821=CARTESIAN_POINT('Ctrl Pts',(20.0394914401257,-20.6201441997549,
1.22634115208255));
#170822=CARTESIAN_POINT('Ctrl Pts',(19.9812109915843,-20.6641517752805,
1.23071828003401));
#170823=CARTESIAN_POINT('Ctrl Pts',(19.9208706274007,-20.7050051665108,
1.23509540798547));
#170824=CARTESIAN_POINT('Ctrl Pts',(19.8604973096611,-20.7458808689175,
1.2394749264086));
#170825=CARTESIAN_POINT('Ctrl Pts',(19.7980622496215,-20.7835987077736,
1.24385444483173));
#170826=CARTESIAN_POINT('Ctrl Pts',(19.7339345832298,-20.817963512307,1.24823396325486));
#170827=CARTESIAN_POINT('Ctrl Pts',(19.6696932585229,-20.8523892241836,
1.25262124382984));
#170828=CARTESIAN_POINT('Ctrl Pts',(19.6037537734795,-20.8834498283967,
1.25700852440483));
#170829=CARTESIAN_POINT('Ctrl Pts',(19.5365066244677,-20.9109977329455,
1.26139580497982));
#170830=CARTESIAN_POINT('Ctrl Pts',(19.4907905516214,-20.9297253969375,
1.26437837362862));
#170831=CARTESIAN_POINT('Ctrl Pts',(19.4444705328526,-20.9468306580778,
1.26736094227741));
#170832=CARTESIAN_POINT('Ctrl Pts',(19.3976727118431,-20.9622804609195,
1.27034351092621));
#170833=CARTESIAN_POINT('Ctrl Pts',(19.3288196249197,-20.9850115752121,
1.27473172930904));
#170834=CARTESIAN_POINT('Ctrl Pts',(19.2586629672397,-21.0042455876802,
1.27911994769187));
#170835=CARTESIAN_POINT('Ctrl Pts',(19.1875916221637,-21.0198354964317,
1.2835081660747));
#170836=CARTESIAN_POINT('Ctrl Pts',(19.1166257539218,-21.0354022682323,
1.28788987191184));
#170837=CARTESIAN_POINT('Ctrl Pts',(19.044748360357,-21.0473355698463,1.29227157774898));
#170838=CARTESIAN_POINT('Ctrl Pts',(18.9723645439181,-21.0555378162046,
1.29665328358612));
#170839=CARTESIAN_POINT('Ctrl Pts',(18.9000657777863,-21.0637304250001,
1.30102984095989));
#170840=CARTESIAN_POINT('Ctrl Pts',(18.8272622477646,-21.0682006332517,
1.30540639833367));
#170841=CARTESIAN_POINT('Ctrl Pts',(18.7543686602251,-21.0689020094659,
1.30978295570745));
#170842=CARTESIAN_POINT('Ctrl Pts',(18.6815212968394,-21.069602940915,1.3141567377663));
#170843=CARTESIAN_POINT('Ctrl Pts',(18.6085844704128,-21.0665397776425,
1.31853051982516));
#170844=CARTESIAN_POINT('Ctrl Pts',(18.5359759950225,-21.0597180773179,
1.32290430188402));
#170845=CARTESIAN_POINT('Ctrl Pts',(18.4633896110466,-21.0528984525225,
1.32727675320246));
#170846=CARTESIAN_POINT('Ctrl Pts',(18.3911318597423,-21.0423226060684,
1.33164920452091));
#170847=CARTESIAN_POINT('Ctrl Pts',(18.3196168489478,-21.0280480736544,
1.33602165583936));
#170848=CARTESIAN_POINT('Ctrl Pts',(18.2481000062642,-21.0137731755918,
1.34039421916011));
#170849=CARTESIAN_POINT('Ctrl Pts',(18.1773264145167,-20.9957994998463,
1.34476678248086));
#170850=CARTESIAN_POINT('Ctrl Pts',(18.1076997236331,-20.9742356350887,
1.34913934580161));
#170851=CARTESIAN_POINT('Ctrl Pts',(18.0380007680099,-20.9526493894446,
1.35351644735541));
#170852=CARTESIAN_POINT('Ctrl Pts',(17.9694515516428,-20.927465658161,1.35789354890922));
#170853=CARTESIAN_POINT('Ctrl Pts',(17.9024394854094,-20.8988426003593,
1.36227065046302));
#170854=CARTESIAN_POINT('Ctrl Pts',(17.8353908192331,-20.8702039095181,
1.36665014265594));
#170855=CARTESIAN_POINT('Ctrl Pts',(17.7698814082307,-20.8381223644766,
1.37102963484885));
#170856=CARTESIAN_POINT('Ctrl Pts',(17.7062751622688,-20.8028027063711,
1.37540912704176));
#170857=CARTESIAN_POINT('Ctrl Pts',(17.6425561732691,-20.7674204436346,
1.37979638195116));
#170858=CARTESIAN_POINT('Ctrl Pts',(17.5807474952407,-20.7287888619662,
1.38418363686056));
#170859=CARTESIAN_POINT('Ctrl Pts',(17.5211845937122,-20.6871564166584,
1.38857089176995));
#170860=CARTESIAN_POINT('Ctrl Pts',(17.4806889445335,-20.6588513331858,
1.39155370038252));
#170861=CARTESIAN_POINT('Ctrl Pts',(17.4412307382319,-20.6291600265461,
1.39453650899508));
#170862=CARTESIAN_POINT('Ctrl Pts',(17.4029060715036,-20.5981706939196,
1.39751931760764));
#170863=CARTESIAN_POINT('Ctrl Pts',(17.3472596999084,-20.5531750275244,
1.40185027442008));
#170864=CARTESIAN_POINT('Ctrl Pts',(17.2937750955671,-20.5052554307103,
1.40618123123253));
#170865=CARTESIAN_POINT('Ctrl Pts',(17.2427818432682,-20.4546501286173,
1.41051218804497));
#170866=CARTESIAN_POINT('Ctrl Pts',(17.1918753395658,-20.4041309151483,
1.41483577712918));
#170867=CARTESIAN_POINT('Ctrl Pts',(17.1434521212288,-20.3509354147135,
1.41915936621338));
#170868=CARTESIAN_POINT('Ctrl Pts',(17.0978092707351,-20.2953424349241,
1.42348295529758));
#170869=CARTESIAN_POINT('Ctrl Pts',(17.0522098693201,-20.239802376101,1.42780242860111));
#170870=CARTESIAN_POINT('Ctrl Pts',(17.0093859027454,-20.1818697428219,
1.43212190190463));
#170871=CARTESIAN_POINT('Ctrl Pts',(16.9695971048709,-20.1218595743336,
1.43644137520815));
#170872=CARTESIAN_POINT('Ctrl Pts',(16.929832242749,-20.0618855061706,1.44075825004552));
#170873=CARTESIAN_POINT('Ctrl Pts',(16.8930992020878,-19.9998367937591,
1.44507512488289));
#170874=CARTESIAN_POINT('Ctrl Pts',(16.8596158068745,-19.9360593968666,
1.44939199972026));
#170875=CARTESIAN_POINT('Ctrl Pts',(16.8261408254926,-19.872298026194,1.45370778979737));
#170876=CARTESIAN_POINT('Ctrl Pts',(16.7959140985895,-19.8068092726922,
1.45802357987448));
#170877=CARTESIAN_POINT('Ctrl Pts',(16.7691077540283,-19.7399641246403,
1.46233936995159));
#170878=CARTESIAN_POINT('Ctrl Pts',(16.7422828062938,-19.6730725871276,
1.4666581551178));
#170879=CARTESIAN_POINT('Ctrl Pts',(16.7188831702512,-19.6048232350479,
1.470976940284));
#170880=CARTESIAN_POINT('Ctrl Pts',(16.6990325461928,-19.5356064272652,
1.47529572545021));
#170881=CARTESIAN_POINT('Ctrl Pts',(16.6791751535563,-19.4663660182415,
1.47961598321668));
#170882=CARTESIAN_POINT('Ctrl Pts',(16.6628692972426,-19.3961579800252,
1.48393624098314));
#170883=CARTESIAN_POINT('Ctrl Pts',(16.6501878709477,-19.325384534782,1.48825649874961));
#170884=CARTESIAN_POINT('Ctrl Pts',(16.6374866783545,-19.2545007763142,
1.49258349041979));
#170885=CARTESIAN_POINT('Ctrl Pts',(16.6284212611835,-19.1830503436799,
1.49691048208997));
#170886=CARTESIAN_POINT('Ctrl Pts',(16.6230126895585,-19.1114414474182,
1.50123747376015));
#170887=CARTESIAN_POINT('Ctrl Pts',(16.6189685454895,-19.0578974226401,
1.50447288948776));
#170888=CARTESIAN_POINT('Ctrl Pts',(16.6169678502335,-19.0042649285282,
1.50770830521537));
#170889=CARTESIAN_POINT('Ctrl Pts',(16.6170003908423,-18.9507135995066,
1.51094372094299));
#170890=CARTESIAN_POINT('Ctrl Pts',(16.7454193692601,-18.2258897638472,
0.53417740218321));
#170891=CARTESIAN_POINT('Ctrl Pts',(16.756562733977,-18.1953716990493,0.535943850225965));
#170892=CARTESIAN_POINT('Ctrl Pts',(16.7684073022959,-18.1651137736251,
0.537705175197931));
#170893=CARTESIAN_POINT('Ctrl Pts',(16.8090263232043,-18.0679964736271,
0.543420742649993));
#170894=CARTESIAN_POINT('Ctrl Pts',(16.8405517957402,-18.0023478894375,
0.547383536916499));
#170895=CARTESIAN_POINT('Ctrl Pts',(16.901832881024,-17.8899725787147,0.554496496727182));
#170896=CARTESIAN_POINT('Ctrl Pts',(16.9301570455683,-17.8425458373681,
0.55760883953424));
#170897=CARTESIAN_POINT('Ctrl Pts',(16.9790300312968,-17.7675396399683,
0.562757572939678));
#170898=CARTESIAN_POINT('Ctrl Pts',(16.9984537680169,-17.7392572348252,
0.56475409184634));
#170899=CARTESIAN_POINT('Ctrl Pts',(17.024861657968,-17.7027398407844,0.567411416226571));
#170900=CARTESIAN_POINT('Ctrl Pts',(17.0312343077344,-17.6940676455638,
0.568048528130771));
#170901=CARTESIAN_POINT('Ctrl Pts',(17.0417745351712,-17.6799508730185,
0.56909576351756));
#170902=CARTESIAN_POINT('Ctrl Pts',(17.0459029806939,-17.6744772186107,
0.56950434580879));
#170903=CARTESIAN_POINT('Ctrl Pts',(17.0539417418228,-17.6639261204056,
0.570296888065913));
#170904=CARTESIAN_POINT('Ctrl Pts',(17.0578486721602,-17.6588461828019,
0.570680710981603));
#170905=CARTESIAN_POINT('Ctrl Pts',(17.0669165480924,-17.6471659249275,
0.571568472289102));
#170906=CARTESIAN_POINT('Ctrl Pts',(17.0720937059783,-17.640578379844,0.572073056529223));
#170907=CARTESIAN_POINT('Ctrl Pts',(17.0861068749037,-17.6229639153252,
0.573432878399449));
#170908=CARTESIAN_POINT('Ctrl Pts',(17.0950142926235,-17.6119945888838,
0.574290992264062));
#170909=CARTESIAN_POINT('Ctrl Pts',(17.1997115915247,-17.4856674459239,
0.584307127752185));
#170910=CARTESIAN_POINT('Ctrl Pts',(17.3073680598168,-17.3807338434297,
0.593981628734713));
#170911=CARTESIAN_POINT('Ctrl Pts',(17.4998931155373,-17.229297183926,0.610137970609044));
#170912=CARTESIAN_POINT('Ctrl Pts',(17.57848060266,-17.1756272118375,0.616463122468588));
#170913=CARTESIAN_POINT('Ctrl Pts',(17.6992045390509,-17.1045927755265,
0.625584859652264));
#170914=CARTESIAN_POINT('Ctrl Pts',(17.7387200255397,-17.0830073848608,
0.628482638642888));
#170915=CARTESIAN_POINT('Ctrl Pts',(17.8009177282364,-17.0515644279514,
0.632877779770675));
#170916=CARTESIAN_POINT('Ctrl Pts',(17.8231334874371,-17.0408170653403,
0.634415901067499));
#170917=CARTESIAN_POINT('Ctrl Pts',(17.8514891312786,-17.0277062012849,
0.636334570305523));
#170918=CARTESIAN_POINT('Ctrl Pts',(17.8574579488358,-17.0249799968968,
0.636735978481852));
#170919=CARTESIAN_POINT('Ctrl Pts',(17.8665015249334,-17.0209001371136,
0.637340333513583));
#170920=CARTESIAN_POINT('Ctrl Pts',(17.8695669222081,-17.0195260055909,
0.637544521753834));
#170921=CARTESIAN_POINT('Ctrl Pts',(17.8758784976567,-17.0167147264572,
0.63796355787036));
#170922=CARTESIAN_POINT('Ctrl Pts',(17.8791249723721,-17.0152784686316,
0.638178343239903));
#170923=CARTESIAN_POINT('Ctrl Pts',(17.8864159254181,-17.0120748165946,
0.638659043199251));
#170924=CARTESIAN_POINT('Ctrl Pts',(17.8904623225654,-17.0103119024273,
0.638924681612913));
#170925=CARTESIAN_POINT('Ctrl Pts',(17.9007735920885,-17.005857856422,0.63959876083953));
#170926=CARTESIAN_POINT('Ctrl Pts',(17.9070460605558,-17.0031842891783,
0.640006155141074));
#170927=CARTESIAN_POINT('Ctrl Pts',(17.9427414388296,-16.9881729179746,
0.642310099755358));
#170928=CARTESIAN_POINT('Ctrl Pts',(17.9724290821328,-16.9764704755102,
0.644170672464985));
#170929=CARTESIAN_POINT('Ctrl Pts',(18.188544046162,-16.8968775790697,0.657394732564471));
#170930=CARTESIAN_POINT('Ctrl Pts',(18.3834474872641,-16.8548155383701,
0.667705158228814));
#170931=CARTESIAN_POINT('Ctrl Pts',(18.637122414328,-16.836479370595,0.681839177325682));
#170932=CARTESIAN_POINT('Ctrl Pts',(18.6930022077351,-16.8346593773269,
0.68498911271661));
#170933=CARTESIAN_POINT('Ctrl Pts',(18.7835696532868,-16.8352962233804,
0.690198379327331));
#170934=CARTESIAN_POINT('Ctrl Pts',(18.8182406796866,-16.8363924433602,
0.692217110253768));
#170935=CARTESIAN_POINT('Ctrl Pts',(18.8637193294802,-16.8389500656925,
0.694903409369141));
#170936=CARTESIAN_POINT('Ctrl Pts',(18.8745658967328,-16.83964388624,0.695546941582073));
#170937=CARTESIAN_POINT('Ctrl Pts',(18.8923113478785,-16.8409162879418,
0.696604644414029));
#170938=CARTESIAN_POINT('Ctrl Pts',(18.899213671785,-16.841445247549,0.697017255642141));
#170939=CARTESIAN_POINT('Ctrl Pts',(18.9125619584686,-16.8425340747035,
0.697817576326137));
#170940=CARTESIAN_POINT('Ctrl Pts',(18.9190082004218,-16.8430896587722,
0.698205147006114));
#170941=CARTESIAN_POINT('Ctrl Pts',(18.9338757417168,-16.8444397430067,
0.699101558928685));
#170942=CARTESIAN_POINT('Ctrl Pts',(18.942294986643,-16.8452551781747,0.699611052345321));
#170943=CARTESIAN_POINT('Ctrl Pts',(18.9649013266819,-16.8475815217057,
0.700984207427924));
#170944=CARTESIAN_POINT('Ctrl Pts',(18.9790782212912,-16.8491854089576,
0.701850773653737));
#170945=CARTESIAN_POINT('Ctrl Pts',(19.1068116688505,-16.8649456383207,
0.709708815719299));
#170946=CARTESIAN_POINT('Ctrl Pts',(19.2190442667893,-16.8881421586555,
0.716988267721187));
#170947=CARTESIAN_POINT('Ctrl Pts',(19.4859089498574,-16.9662739949165,
0.735128286995092));
#170948=CARTESIAN_POINT('Ctrl Pts',(19.6371119043171,-17.0303175560788,
0.746145432696012));
#170949=CARTESIAN_POINT('Ctrl Pts',(19.807930229791,-17.1273254183587,0.75862782643242));
#170950=CARTESIAN_POINT('Ctrl Pts',(19.8360557092467,-17.144173416957,0.760682322494398));
#170951=CARTESIAN_POINT('Ctrl Pts',(19.8699354611918,-17.1655530789304,
0.763145746535472));
#170952=CARTESIAN_POINT('Ctrl Pts',(19.8760707044643,-17.1694690792802,
0.763591376072764));
#170953=CARTESIAN_POINT('Ctrl Pts',(19.8856545194286,-17.1756560257318,
0.764286600623958));
#170954=CARTESIAN_POINT('Ctrl Pts',(19.8891167837211,-17.1779055088088,
0.764537575238687));
#170955=CARTESIAN_POINT('Ctrl Pts',(19.8955694038979,-17.1821247666374,
0.765004940135757));
#170956=CARTESIAN_POINT('Ctrl Pts',(19.8985613173316,-17.1840919819673,
0.765221489450688));
#170957=CARTESIAN_POINT('Ctrl Pts',(19.9053743893457,-17.1885964506168,
0.765714263610307));
#170958=CARTESIAN_POINT('Ctrl Pts',(19.9091922926673,-17.1911385306746,
0.765990160693723));
#170959=CARTESIAN_POINT('Ctrl Pts',(19.9208987306908,-17.198988077657,0.76683546444715));
#170960=CARTESIAN_POINT('Ctrl Pts',(19.928759921992,-17.2043363787021,0.7674021971589));
#170961=CARTESIAN_POINT('Ctrl Pts',(19.9989279786235,-17.2527694101189,
0.772455133012804));
#170962=CARTESIAN_POINT('Ctrl Pts',(20.0589236708848,-17.2991215283063,
0.776736064714976));
#170963=CARTESIAN_POINT('Ctrl Pts',(20.2235242540584,-17.4410253283913,
0.788766691494084));
#170964=CARTESIAN_POINT('Ctrl Pts',(20.3211978704125,-17.5439757776493,
0.796291212775601));
#170965=CARTESIAN_POINT('Ctrl Pts',(20.4457162138202,-17.7047877383316,
0.807543794352667));
#170966=CARTESIAN_POINT('Ctrl Pts',(20.481403118573,-17.7552994087573,0.811013082463597));
#170967=CARTESIAN_POINT('Ctrl Pts',(20.5349762828834,-17.8386438084752,
0.81669923004443));
#170968=CARTESIAN_POINT('Ctrl Pts',(20.554293322639,-17.8705151176844,0.818864946077263));
#170969=CARTESIAN_POINT('Ctrl Pts',(20.5782785347725,-17.91255314625,0.82171805014904));
#170970=CARTESIAN_POINT('Ctrl Pts',(20.5837221241766,-17.9222713310008,
0.822377370749431));
#170971=CARTESIAN_POINT('Ctrl Pts',(20.5924483618978,-17.9381423613318,
0.823453918609312));
#170972=CARTESIAN_POINT('Ctrl Pts',(20.5957777920247,-17.9442693431958,
0.823869468035583));
#170973=CARTESIAN_POINT('Ctrl Pts',(20.6021210313214,-17.9560812219315,
0.824670538111188));
#170974=CARTESIAN_POINT('Ctrl Pts',(20.6051393169819,-17.9617636366996,
0.825055893890783));
#170975=CARTESIAN_POINT('Ctrl Pts',(20.6119890785312,-17.9748025690981,
0.825940132333222));
#170976=CARTESIAN_POINT('Ctrl Pts',(20.6158033005595,-17.9821679872317,
0.826439617829988));
#170977=CARTESIAN_POINT('Ctrl Pts',(20.625817666256,-18.0017876427368,0.827770211341403));
#170978=CARTESIAN_POINT('Ctrl Pts',(20.6319419396316,-18.0140799681767,
0.828603961772518));
#170979=CARTESIAN_POINT('Ctrl Pts',(20.67748316056,-18.1077607295877,0.83495969875425));
#170980=CARTESIAN_POINT('Ctrl Pts',(20.7117633269927,-18.1915296052101,
0.840658553926819));
#170981=CARTESIAN_POINT('Ctrl Pts',(20.7851879883555,-18.4098724996177,
0.855533050089258));
#170982=CARTESIAN_POINT('Ctrl Pts',(20.8165299550453,-18.5466132606371,
0.864885055398191));
#170983=CARTESIAN_POINT('Ctrl Pts',(20.8410841531538,-18.740061165054,0.877655875524083));
#170984=CARTESIAN_POINT('Ctrl Pts',(20.845884637824,-18.7949464858018,0.881224623349047));
#170985=CARTESIAN_POINT('Ctrl Pts',(20.8499087278744,-18.8783362681687,
0.88650859906527));
#170986=CARTESIAN_POINT('Ctrl Pts',(20.8507068074099,-18.9067389214647,
0.88828401775567));
#170987=CARTESIAN_POINT('Ctrl Pts',(20.8509881596209,-18.9420875532205,
0.890456401079072));
#170988=CARTESIAN_POINT('Ctrl Pts',(20.8510092763639,-18.9490248623917,
0.890880955648094));
#170989=CARTESIAN_POINT('Ctrl Pts',(20.8509887258657,-18.9600047900095,
0.891549955799514));
#170990=CARTESIAN_POINT('Ctrl Pts',(20.8509695804609,-18.9640473292392,
0.891795630669776));
#170991=CARTESIAN_POINT('Ctrl Pts',(20.8509116364382,-18.9716710250809,
0.892257712671293));
#170992=CARTESIAN_POINT('Ctrl Pts',(20.8508753307681,-18.9752520943311,
0.892474250698219));
#170993=CARTESIAN_POINT('Ctrl Pts',(20.8507715424075,-18.9834398188553,
0.892968183478084));
#170994=CARTESIAN_POINT('Ctrl Pts',(20.8506981094313,-18.988046350801,0.893245242243488));
#170995=CARTESIAN_POINT('Ctrl Pts',(20.8504631736449,-19.000278450673,0.893978808018579));
#170996=CARTESIAN_POINT('Ctrl Pts',(20.8502754957042,-19.0079035280152,
0.894433888677758));
#170997=CARTESIAN_POINT('Ctrl Pts',(20.848670192472,-19.061374758166,0.897610771588053));
#170998=CARTESIAN_POINT('Ctrl Pts',(20.845804004915,-19.1071688816759,0.900257379866982));
#170999=CARTESIAN_POINT('Ctrl Pts',(20.8378738680996,-19.190382455053,0.904989165875819));
#171000=CARTESIAN_POINT('Ctrl Pts',(20.8332930167474,-19.2278269539272,
0.907089594987942));
#171001=CARTESIAN_POINT('Ctrl Pts',(20.8083554848241,-19.3945691353168,
0.916389495730702));
#171002=CARTESIAN_POINT('Ctrl Pts',(20.7770356154966,-19.5219342647907,
0.923366576445844));
#171003=CARTESIAN_POINT('Ctrl Pts',(20.7052127845892,-19.7290535564578,
0.935466841354512));
#171004=CARTESIAN_POINT('Ctrl Pts',(20.6710793550723,-19.8106111333967,
0.940438850852846));
#171005=CARTESIAN_POINT('Ctrl Pts',(20.6228630275673,-19.9081938682297,
0.946782330883236));
#171006=CARTESIAN_POINT('Ctrl Pts',(20.613504225402,-19.9264609143076,0.94798733709584));
#171007=CARTESIAN_POINT('Ctrl Pts',(20.5997291471433,-19.9524110069799,
0.949725671679413));
#171008=CARTESIAN_POINT('Ctrl Pts',(20.5955277532256,-19.9602072474063,
0.950251395298374));
#171009=CARTESIAN_POINT('Ctrl Pts',(20.5881609057574,-19.9736743667182,
0.951165660908251));
#171010=CARTESIAN_POINT('Ctrl Pts',(20.5850180256244,-19.9793575051611,
0.951553392582516));
#171011=CARTESIAN_POINT('Ctrl Pts',(20.578925774579,-19.9902551592022,0.952300605540826));
#171012=CARTESIAN_POINT('Ctrl Pts',(20.5759803176971,-19.9954717999949,
0.952659943299068));
#171013=CARTESIAN_POINT('Ctrl Pts',(20.5682083838618,-20.0091010696816,
0.953603141133994));
#171014=CARTESIAN_POINT('Ctrl Pts',(20.5633462080697,-20.0174930844778,
0.954188288616566));
#171015=CARTESIAN_POINT('Ctrl Pts',(20.5462827866204,-20.0464830949498,
0.956225129268232));
#171016=CARTESIAN_POINT('Ctrl Pts',(20.5337902835073,-20.0669067249354,
0.957687395725874));
#171017=CARTESIAN_POINT('Ctrl Pts',(20.4376925818721,-20.2181887111039,
0.968729193057548));
#171018=CARTESIAN_POINT('Ctrl Pts',(20.3402766470718,-20.3396818906598,
0.978844831797642));
#171019=CARTESIAN_POINT('Ctrl Pts',(20.1778923763589,-20.5019647485338,
0.994011770681932));
#171020=CARTESIAN_POINT('Ctrl Pts',(20.1225743791027,-20.5517117431381,
0.998935572874766));
#171021=CARTESIAN_POINT('Ctrl Pts',(20.028995869482,-20.6273472817382,1.00677231099476));
#171022=CARTESIAN_POINT('Ctrl Pts',(19.9923045149465,-20.6550775407114,
1.00973306955527));
#171023=CARTESIAN_POINT('Ctrl Pts',(19.9410807103848,-20.6912310236778,
1.01368767342682));
#171024=CARTESIAN_POINT('Ctrl Pts',(19.9273103005608,-20.7007077967887,
1.01473382801114));
#171025=CARTESIAN_POINT('Ctrl Pts',(19.9035320870702,-20.7166602283377,
1.01650952270634));
#171026=CARTESIAN_POINT('Ctrl Pts',(19.8935793755225,-20.7232161672246,
1.01724370883771));
#171027=CARTESIAN_POINT('Ctrl Pts',(19.8793553253973,-20.7324143869249,
1.0182795759814));
#171028=CARTESIAN_POINT('Ctrl Pts',(19.8751293410706,-20.7351259177989,
1.0185856686404));
#171029=CARTESIAN_POINT('Ctrl Pts',(19.8678307178282,-20.7397723813504,
1.01911139810944));
#171030=CARTESIAN_POINT('Ctrl Pts',(19.8647626892435,-20.7417144815897,
1.01933150798476));
#171031=CARTESIAN_POINT('Ctrl Pts',(19.8588028021837,-20.7454657207324,
1.01975735780632));
#171032=CARTESIAN_POINT('Ctrl Pts',(19.8559115711682,-20.7472757621329,
1.01996316072368));
#171033=CARTESIAN_POINT('Ctrl Pts',(19.8481018918748,-20.7521387406616,
1.02051699369924));
#171034=CARTESIAN_POINT('Ctrl Pts',(19.843175233503,-20.7551785308962,1.02086416262428));
#171035=CARTESIAN_POINT('Ctrl Pts',(19.8248594182825,-20.7663760757551,
1.02214689117409));
#171036=CARTESIAN_POINT('Ctrl Pts',(19.811391855142,-20.774405453696,1.02307441286469));
#171037=CARTESIAN_POINT('Ctrl Pts',(19.6817561764723,-20.8497549800986,
1.03186595120302));
#171038=CARTESIAN_POINT('Ctrl Pts',(19.5595042888919,-20.9060389756439,
1.03912865015386));
#171039=CARTESIAN_POINT('Ctrl Pts',(19.2810393565962,-21.0034044001591,
1.05514839286962));
#171040=CARTESIAN_POINT('Ctrl Pts',(19.1238252041838,-21.0389931039599,
1.06389558320799));
#171041=CARTESIAN_POINT('Ctrl Pts',(18.9455568207444,-21.0584854458993,
1.07436835008178));
#171042=CARTESIAN_POINT('Ctrl Pts',(18.9269811212476,-21.0602683595867,
1.07546547260087));
#171043=CARTESIAN_POINT('Ctrl Pts',(18.899884412029,-21.0625080218997,1.07707529684192));
#171044=CARTESIAN_POINT('Ctrl Pts',(18.8913800445507,-21.0631592235043,
1.07758189314329));
#171045=CARTESIAN_POINT('Ctrl Pts',(18.8764405208529,-21.0642124108122,
1.07847428179421));
#171046=CARTESIAN_POINT('Ctrl Pts',(18.8700069918926,-21.0646364256793,
1.07885937747679));
#171047=CARTESIAN_POINT('Ctrl Pts',(18.8574944176068,-21.06540370039,1.07960994174849));
#171048=CARTESIAN_POINT('Ctrl Pts',(18.8514156251003,-21.0657501370267,
1.07997530663645));
#171049=CARTESIAN_POINT('Ctrl Pts',(18.8368538202104,-21.066517020409,1.08085232479858));
#171050=CARTESIAN_POINT('Ctrl Pts',(18.8283696560654,-21.0669126465785,
1.08136475180461));
#171051=CARTESIAN_POINT('Ctrl Pts',(18.7975852189731,-21.0681625528504,
1.08322945501518));
#171052=CARTESIAN_POINT('Ctrl Pts',(18.7752747833154,-21.0687152294586,
1.08459112605128));
#171053=CARTESIAN_POINT('Ctrl Pts',(18.5696370501106,-21.0705570509026,
1.09724050441705));
#171054=CARTESIAN_POINT('Ctrl Pts',(18.3869095213298,-21.0483780083643,
1.10930507026757));
#171055=CARTESIAN_POINT('Ctrl Pts',(18.1303766037215,-20.9827574163749,
1.12678910466413));
#171056=CARTESIAN_POINT('Ctrl Pts',(18.0526132115985,-20.9580036617207,
1.13214925943526));
#171057=CARTESIAN_POINT('Ctrl Pts',(17.9424743182601,-20.9157976743825,
1.13967023168194));
#171058=CARTESIAN_POINT('Ctrl Pts',(17.9088205239887,-20.901895743746,1.14195787695923));
#171059=CARTESIAN_POINT('Ctrl Pts',(17.868691505981,-20.8840937708203,1.14465883255332));
#171060=CARTESIAN_POINT('Ctrl Pts',(17.8618592503056,-20.8810193481767,
1.14511773346991));
#171061=CARTESIAN_POINT('Ctrl Pts',(17.8512529429529,-20.8761787840294,
1.14582846849455));
#171062=CARTESIAN_POINT('Ctrl Pts',(17.8474676197023,-20.874437697042,1.1460817951661));
#171063=CARTESIAN_POINT('Ctrl Pts',(17.8404514818725,-20.8711854436266,
1.14655069120322));
#171064=CARTESIAN_POINT('Ctrl Pts',(17.8372193748333,-20.8696773012933,
1.14676643650128));
#171065=CARTESIAN_POINT('Ctrl Pts',(17.829913226265,-20.8662456483881,1.14725355039617));
#171066=CARTESIAN_POINT('Ctrl Pts',(17.8258415152605,-20.8643173021946,
1.14752461591591));
#171067=CARTESIAN_POINT('Ctrl Pts',(17.8135518609585,-20.8584488665955,
1.14834164637307));
#171068=CARTESIAN_POINT('Ctrl Pts',(17.8053530516742,-20.8544686356715,
1.14888518455738));
#171069=CARTESIAN_POINT('Ctrl Pts',(17.742406533295,-20.823406450517,1.15304834161828));
#171070=CARTESIAN_POINT('Ctrl Pts',(17.6888228907673,-20.794016825117,1.15653478817146));
#171071=CARTESIAN_POINT('Ctrl Pts',(17.4971417817146,-20.6778211700197,
1.16906404356491));
#171072=CARTESIAN_POINT('Ctrl Pts',(17.3679313976352,-20.5774658581177,
1.17766507019037));
#171073=CARTESIAN_POINT('Ctrl Pts',(17.1948923637841,-20.4077225768788,
1.191113614336));
#171074=CARTESIAN_POINT('Ctrl Pts',(17.1414403955231,-20.3490441937331,
1.19560092452114));
#171075=CARTESIAN_POINT('Ctrl Pts',(17.0791845743373,-20.2724735680201,
1.2013595674809));
#171076=CARTESIAN_POINT('Ctrl Pts',(17.0671668213682,-20.2572707207976,
1.20249829610772));
#171077=CARTESIAN_POINT('Ctrl Pts',(17.050084020611,-20.2350397285934,1.20415785262012));
#171078=CARTESIAN_POINT('Ctrl Pts',(17.0448505163626,-20.2281418374624,
1.20467201801049));
#171079=CARTESIAN_POINT('Ctrl Pts',(17.0357829816299,-20.2160370908401,
1.20557306108346));
#171080=CARTESIAN_POINT('Ctrl Pts',(17.0319301924208,-20.2108443816442,
1.2059591978554));
#171081=CARTESIAN_POINT('Ctrl Pts',(17.0245195218137,-20.2007602167472,
1.20670834888397));
#171082=CARTESIAN_POINT('Ctrl Pts',(17.0209586919641,-20.1958709981395,
1.20707124330529));
#171083=CARTESIAN_POINT('Ctrl Pts',(17.0125345191679,-20.1841993553616,
1.20793681684641));
#171084=CARTESIAN_POINT('Ctrl Pts',(17.0076902625268,-20.177403337777,1.20844022578092));
#171085=CARTESIAN_POINT('Ctrl Pts',(16.9905656874668,-20.1530761607897,
1.21024028032476));
#171086=CARTESIAN_POINT('Ctrl Pts',(16.9785115316578,-20.1353880728047,
1.21154550124966));
#171087=CARTESIAN_POINT('Ctrl Pts',(16.8609883990679,-19.9571884619835,
1.22466377252393));
#171088=CARTESIAN_POINT('Ctrl Pts',(16.7775784213282,-19.7832402364215,
1.23734170066882));
#171089=CARTESIAN_POINT('Ctrl Pts',(16.6954799616009,-19.5281125874455,
1.25502391781768));
#171090=CARTESIAN_POINT('Ctrl Pts',(16.6761041766622,-19.4545296219884,
1.26000955504588));
#171091=CARTESIAN_POINT('Ctrl Pts',(16.6536719489235,-19.3458808933151,
1.26707452376771));
#171092=CARTESIAN_POINT('Ctrl Pts',(16.6474610384553,-19.3115308720113,
1.26926547983072));
#171093=CARTESIAN_POINT('Ctrl Pts',(16.6409663500992,-19.2697323453033,
1.27186750610064));
#171094=CARTESIAN_POINT('Ctrl Pts',(16.639869047353,-19.2624178792355,1.27232047861227));
#171095=CARTESIAN_POINT('Ctrl Pts',(16.6382167990403,-19.2509965648377,
1.27302393473657));
#171096=CARTESIAN_POINT('Ctrl Pts',(16.6376355523249,-19.2468936662818,
1.27327586526393));
#171097=CARTESIAN_POINT('Ctrl Pts',(16.6365763775123,-19.2392557606341,
1.2737433840514));
#171098=CARTESIAN_POINT('Ctrl Pts',(16.6360953416556,-19.2357212874404,
1.2739591405538));
#171099=CARTESIAN_POINT('Ctrl Pts',(16.6350235911957,-19.2276946907583,
1.27444778780642));
#171100=CARTESIAN_POINT('Ctrl Pts',(16.6344383637596,-19.2232018874071,
1.27472036628636));
#171101=CARTESIAN_POINT('Ctrl Pts',(16.6327408137607,-19.2098348694521,
1.27552865093633));
#171102=CARTESIAN_POINT('Ctrl Pts',(16.6316702820028,-19.200955319001,1.27606205837468));
#171103=CARTESIAN_POINT('Ctrl Pts',(16.6239226733556,-19.1330753311044,
1.28011460693802));
#171104=CARTESIAN_POINT('Ctrl Pts',(16.6196735818517,-19.0738185473203,
1.28350784889789));
#171105=CARTESIAN_POINT('Ctrl Pts',(16.6173229666981,-18.9941773248179,
1.28796711722882));
#171106=CARTESIAN_POINT('Ctrl Pts',(16.6170159594122,-18.9738905047956,
1.28909419685705));
#171107=CARTESIAN_POINT('Ctrl Pts',(16.6168948152901,-18.813805207517,1.2979391220944));
#171108=CARTESIAN_POINT('Ctrl Pts',(16.6306361033606,-18.674341220692,1.30537418636845));
#171109=CARTESIAN_POINT('Ctrl Pts',(16.6757502479721,-18.4485303115064,
1.31812043025327));
#171110=CARTESIAN_POINT('Ctrl Pts',(16.6991412232676,-18.3610510614871,
1.32323611835779));
#171111=CARTESIAN_POINT('Ctrl Pts',(16.7324404237939,-18.2623358209319,
1.3293438777088));
#171112=CARTESIAN_POINT('Ctrl Pts',(16.7369541499677,-18.2493725904713,
1.33015264909307));
#171113=CARTESIAN_POINT('Ctrl Pts',(16.7428594802954,-18.2329294480821,
1.33118740041875));
#171114=CARTESIAN_POINT('Ctrl Pts',(16.7441347600493,-18.2294078921804,
1.33140952898772));
#171115=CARTESIAN_POINT('Ctrl Pts',(16.7454193692336,-18.2258897639197,
1.33163196665472));
#171116=CARTESIAN_POINT('Origin',(18.734,-18.952,0.));
#171117=CARTESIAN_POINT('',(16.7454193691877,-18.2258897640454,2.35747631421306));
#171118=CARTESIAN_POINT('',(16.7452305870807,-18.2258208582162,2.13351566426921));
#171119=CARTESIAN_POINT('',(16.7454193692319,-18.2258897639242,0.));
#171120=CARTESIAN_POINT('Ctrl Pts',(16.7454193691877,-18.2258897640453,
2.35747631421306));
#171121=CARTESIAN_POINT('Ctrl Pts',(16.742191647268,-18.2347294483981,2.35692305832686));
#171122=CARTESIAN_POINT('Ctrl Pts',(16.7390229051106,-18.2435905499536,
2.35636788652136));
#171123=CARTESIAN_POINT('Ctrl Pts',(16.7330803313949,-18.2605645458309,
2.35530317645736));
#171124=CARTESIAN_POINT('Ctrl Pts',(16.7302965273719,-18.2686736519259,
2.35479398625594));
#171125=CARTESIAN_POINT('Ctrl Pts',(16.7255041834798,-18.2829146638836,
2.35389872613313));
#171126=CARTESIAN_POINT('Ctrl Pts',(16.7234742637549,-18.2890392964446,
2.35351336858945));
#171127=CARTESIAN_POINT('Ctrl Pts',(16.7195884540897,-18.300945475638,2.35276355646451));
#171128=CARTESIAN_POINT('Ctrl Pts',(16.7177293753157,-18.3067259211549,
2.35239921146551));
#171129=CARTESIAN_POINT('Ctrl Pts',(16.7133468272281,-18.3205564735102,
2.35152668444952));
#171130=CARTESIAN_POINT('Ctrl Pts',(16.7108465738788,-18.3286137770769,
2.3510177453064));
#171131=CARTESIAN_POINT('Ctrl Pts',(16.7020108004384,-18.3577010113374,
2.34917806413336));
#171132=CARTESIAN_POINT('Ctrl Pts',(16.6959546544632,-18.3788137235067,
2.3478382462076));
#171133=CARTESIAN_POINT('Ctrl Pts',(16.641457713344,-18.58059376658,2.33498642094185));
#171134=CARTESIAN_POINT('Ctrl Pts',(16.616843652966,-18.7668066908484,2.32266065705822));
#171135=CARTESIAN_POINT('Ctrl Pts',(16.6170536898947,-19.016790561049,2.30615864857607));
#171136=CARTESIAN_POINT('Ctrl Pts',(16.6199199087135,-19.0797716781136,
2.30201615293556));
#171137=CARTESIAN_POINT('Ctrl Pts',(16.6300811392499,-19.1922138793031,
2.29473640421839));
#171138=CARTESIAN_POINT('Ctrl Pts',(16.6363255949835,-19.2417244169326,
2.29157204903625));
#171139=CARTESIAN_POINT('Ctrl Pts',(16.6455655230035,-19.2986864772174,
2.28801329944128));
#171140=CARTESIAN_POINT('Ctrl Pts',(16.6468596252838,-19.3063940444386,
2.28753351543509));
#171141=CARTESIAN_POINT('Ctrl Pts',(16.6489941838878,-19.3186899263177,
2.28677110884327));
#171142=CARTESIAN_POINT('Ctrl Pts',(16.6498071584404,-19.3232828509857,
2.28648699258429));
#171143=CARTESIAN_POINT('Ctrl Pts',(16.6512728103301,-19.3314065698001,
2.28598569190362));
#171144=CARTESIAN_POINT('Ctrl Pts',(16.6519192987852,-19.3349384365235,
2.2857681597343));
#171145=CARTESIAN_POINT('Ctrl Pts',(16.6533073569515,-19.3424141755541,
2.28530860903462));
#171146=CARTESIAN_POINT('Ctrl Pts',(16.6540511539905,-19.3463575812757,
2.28506671893067));
#171147=CARTESIAN_POINT('Ctrl Pts',(16.6560859637875,-19.3569796646717,
2.28441650041225));
#171148=CARTESIAN_POINT('Ctrl Pts',(16.6573979731469,-19.3636543399822,
2.28400935192934));
#171149=CARTESIAN_POINT('Ctrl Pts',(16.6640292710389,-19.3965515595136,
2.28200921964718));
#171150=CARTESIAN_POINT('Ctrl Pts',(16.6698134504046,-19.4226792400825,
2.28044127498456));
#171151=CARTESIAN_POINT('Ctrl Pts',(16.6879077713527,-19.4976482032919,
2.27598365064359));
#171152=CARTESIAN_POINT('Ctrl Pts',(16.7014678574174,-19.5461709650004,
2.27314936331566));
#171153=CARTESIAN_POINT('Ctrl Pts',(16.7568102839577,-19.7200193903671,
2.2630318424694));
#171154=CARTESIAN_POINT('Ctrl Pts',(16.8085639996897,-19.8418492049444,
2.25599589812605));
#171155=CARTESIAN_POINT('Ctrl Pts',(16.9207548644365,-20.0495633359862,
2.24300920133381));
#171156=CARTESIAN_POINT('Ctrl Pts',(16.9768431251024,-20.1372842985294,
2.23716708890243));
#171157=CARTESIAN_POINT('Ctrl Pts',(17.0475681398124,-20.2317789787875,
2.23025034436802));
#171158=CARTESIAN_POINT('Ctrl Pts',(17.0561041215743,-20.2429500612168,
2.2294222526471));
#171159=CARTESIAN_POINT('Ctrl Pts',(17.0699092574628,-20.2606486739674,
2.22809314038657));
#171160=CARTESIAN_POINT('Ctrl Pts',(17.0751071295488,-20.2672314596875,
2.22759494147258));
#171161=CARTESIAN_POINT('Ctrl Pts',(17.0843685933005,-20.278818289363,2.22671109752194));
#171162=CARTESIAN_POINT('Ctrl Pts',(17.0884162008142,-20.283835015832,2.2263260965131));
#171163=CARTESIAN_POINT('Ctrl Pts',(17.0968603459561,-20.2942036825246,
2.22552548768125));
#171164=CARTESIAN_POINT('Ctrl Pts',(17.1012603578281,-20.2995526822103,
2.22510974180079));
#171165=CARTESIAN_POINT('Ctrl Pts',(17.1126754486993,-20.3132917775771,
2.22403476649502));
#171166=CARTESIAN_POINT('Ctrl Pts',(17.1197293707355,-20.3216492006401,
2.22337395481139));
#171167=CARTESIAN_POINT('Ctrl Pts',(17.1499117473638,-20.3568519484336,
2.22056071772465));
#171168=CARTESIAN_POINT('Ctrl Pts',(17.173646434622,-20.3831677406774,2.21838328353239));
#171169=CARTESIAN_POINT('Ctrl Pts',(17.2376865338461,-20.4506846956561,
2.2125935663988));
#171170=CARTESIAN_POINT('Ctrl Pts',(17.2790313529665,-20.4908551302041,
2.20893872119819));
#171171=CARTESIAN_POINT('Ctrl Pts',(17.4217681512704,-20.6186378809442,
2.19659998968109));
#171172=CARTESIAN_POINT('Ctrl Pts',(17.5298270513337,-20.6983094339051,
2.18767358335912));
#171173=CARTESIAN_POINT('Ctrl Pts',(17.7216270867672,-20.8134091984661,
2.17297278913589));
#171174=CARTESIAN_POINT('Ctrl Pts',(17.8014472693961,-20.8546540122369,
2.16715226193123));
#171175=CARTESIAN_POINT('Ctrl Pts',(17.892492001079,-20.894587563985,2.16101026085349));
#171176=CARTESIAN_POINT('Ctrl Pts',(17.9013574906196,-20.8984040216945,
2.16041725927675));
#171177=CARTESIAN_POINT('Ctrl Pts',(17.914496659348,-20.9039540304203,2.15954621082074));
#171178=CARTESIAN_POINT('Ctrl Pts',(17.9187502541619,-20.9057344023827,
2.15926542624076));
#171179=CARTESIAN_POINT('Ctrl Pts',(17.9263117558392,-20.9088703276771,
2.15876846066808));
#171180=CARTESIAN_POINT('Ctrl Pts',(17.9296173089669,-20.9102314128161,
2.1585519476452));
#171181=CARTESIAN_POINT('Ctrl Pts',(17.9367125522005,-20.9131319324304,
2.15808880166515));
#171182=CARTESIAN_POINT('Ctrl Pts',(17.9405032501498,-20.9146687543866,
2.15784232687763));
#171183=CARTESIAN_POINT('Ctrl Pts',(17.9509339896548,-20.918862418058,2.1571666973332));
#171184=CARTESIAN_POINT('Ctrl Pts',(17.9575831481224,-20.921496642183,2.15673888599771));
#171185=CARTESIAN_POINT('Ctrl Pts',(17.993357975345,-20.9354603706962,2.15445185884578));
#171186=CARTESIAN_POINT('Ctrl Pts',(18.0227201246813,-20.9461782326752,
2.15262711556594));
#171187=CARTESIAN_POINT('Ctrl Pts',(18.2073709256909,-21.008982258067,2.14141263178207));
#171188=CARTESIAN_POINT('Ctrl Pts',(18.3680442167472,-21.0435551359027,
2.13275774562994));
#171189=CARTESIAN_POINT('Ctrl Pts',(18.6477495766403,-21.0704853923423,
2.1173762373682));
#171190=CARTESIAN_POINT('Ctrl Pts',(18.7651027779518,-21.0720110415517,
2.11083587710707));
#171191=CARTESIAN_POINT('Ctrl Pts',(18.8962303130863,-21.062823217679,2.10313519787881));
#171192=CARTESIAN_POINT('Ctrl Pts',(18.9104790297499,-21.0616797074229,
2.10229342675773));
#171193=CARTESIAN_POINT('Ctrl Pts',(18.9331364557481,-21.0596302275954,
2.1009465044696));
#171194=CARTESIAN_POINT('Ctrl Pts',(18.9415533581131,-21.0588180046348,
2.10044429687156));
#171195=CARTESIAN_POINT('Ctrl Pts',(18.9563884338819,-21.0572966721817,
2.09955579480158));
#171196=CARTESIAN_POINT('Ctrl Pts',(18.9628086882494,-21.056608580278,2.09917016678875));
#171197=CARTESIAN_POINT('Ctrl Pts',(18.9760805752753,-21.0551247163706,
2.09837067025549));
#171198=CARTESIAN_POINT('Ctrl Pts',(18.9829316599811,-21.054324809453,2.09795667559764));
#171199=CARTESIAN_POINT('Ctrl Pts',(19.0005060015871,-21.0521857850952,
2.09689134106119));
#171200=CARTESIAN_POINT('Ctrl Pts',(19.0112230382498,-21.0507980277006,
2.0962384726535));
#171201=CARTESIAN_POINT('Ctrl Pts',(19.0558971022456,-21.0446650103507,
2.09350326012465));
#171202=CARTESIAN_POINT('Ctrl Pts',(19.0897453953052,-21.0391774212423,
2.09139760274706));
#171203=CARTESIAN_POINT('Ctrl Pts',(19.1775689127627,-21.0227408659694,
2.0858439983357));
#171204=CARTESIAN_POINT('Ctrl Pts',(19.2312739323303,-21.0105040518219,
2.08235768089844));
#171205=CARTESIAN_POINT('Ctrl Pts',(19.3900380388603,-20.9677537327037,
2.07178961959005));
#171206=CARTESIAN_POINT('Ctrl Pts',(19.4932692369694,-20.931180582558,2.06455947997301));
#171207=CARTESIAN_POINT('Ctrl Pts',(19.6343931269209,-20.8685104449588,
2.05435928051722));
#171208=CARTESIAN_POINT('Ctrl Pts',(19.6749881689147,-20.8489084100359,
2.05138765429304));
#171209=CARTESIAN_POINT('Ctrl Pts',(19.7364760283702,-20.8167579220294,
2.04685421020773));
#171210=CARTESIAN_POINT('Ctrl Pts',(19.7578295402099,-20.8051199182004,
2.04527366739353));
#171211=CARTESIAN_POINT('Ctrl Pts',(19.791519323121,-20.7859983160153,2.04277500044323));
#171212=CARTESIAN_POINT('Ctrl Pts',(19.8039875121088,-20.7787522227219,
2.04184916003008));
#171213=CARTESIAN_POINT('Ctrl Pts',(19.8483459158365,-20.7523626212031,
2.03855370498121));
#171214=CARTESIAN_POINT('Ctrl Pts',(19.879806499127,-20.732505614515,2.03621344760067));
#171215=CARTESIAN_POINT('Ctrl Pts',(19.9166872116085,-20.7078449027583,
2.03348122807795));
#171216=CARTESIAN_POINT('Ctrl Pts',(19.9226246903646,-20.7038309598396,
2.03304172238286));
#171217=CARTESIAN_POINT('Ctrl Pts',(19.9322733931313,-20.6972364610481,
2.03232824099036));
#171218=CARTESIAN_POINT('Ctrl Pts',(19.93599688225,-20.6946740732551,2.03205308500801));
#171219=CARTESIAN_POINT('Ctrl Pts',(19.9426437500345,-20.6900684698074,
2.03156226478174));
#171220=CARTESIAN_POINT('Ctrl Pts',(19.945570188268,-20.6880297807783,2.03134629975521));
#171221=CARTESIAN_POINT('Ctrl Pts',(19.9518925993929,-20.6836015298445,
2.03088000667716));
#171222=CARTESIAN_POINT('Ctrl Pts',(19.9552866875967,-20.6812093769105,
2.03062985969465));
#171223=CARTESIAN_POINT('Ctrl Pts',(19.9647377843521,-20.6745065383444,
2.0299337298816));
#171224=CARTESIAN_POINT('Ctrl Pts',(19.9707792256063,-20.670173861779,2.02948922907074));
#171225=CARTESIAN_POINT('Ctrl Pts',(20.0055417194514,-20.6449652521705,
2.02693360519926));
#171226=CARTESIAN_POINT('Ctrl Pts',(20.033758608939,-20.6233998870952,2.02486724857726));
#171227=CARTESIAN_POINT('Ctrl Pts',(20.1223549709297,-20.5520868550003,
2.01835813036604));
#171228=CARTESIAN_POINT('Ctrl Pts',(20.1805283151879,-20.4996967420553,
2.01405024523169));
#171229=CARTESIAN_POINT('Ctrl Pts',(20.3685617440419,-20.3104701293267,
1.99949831309707));
#171230=CARTESIAN_POINT('Ctrl Pts',(20.4829781411939,-20.1596021362546,
1.98942970458877));
#171231=CARTESIAN_POINT('Ctrl Pts',(20.5866552886593,-19.9766134412949,
1.97719372375848));
#171232=CARTESIAN_POINT('Ctrl Pts',(20.5971086305613,-19.9574802341664,
1.9759154173762));
#171233=CARTESIAN_POINT('Ctrl Pts',(20.6111823235174,-19.9307472919201,
1.97412940224031));
#171234=CARTESIAN_POINT('Ctrl Pts',(20.6150558848979,-19.9232818807924,
1.97363064816277));
#171235=CARTESIAN_POINT('Ctrl Pts',(20.6216461219928,-19.9103933982634,
1.97276951079539));
#171236=CARTESIAN_POINT('Ctrl Pts',(20.6243841851611,-19.904981331939,1.97240788381888));
#171237=CARTESIAN_POINT('Ctrl Pts',(20.6299885961669,-19.8937844355218,
1.97165964076125));
#171238=CARTESIAN_POINT('Ctrl Pts',(20.6328518121593,-19.8879981163514,
1.97127291990969));
#171239=CARTESIAN_POINT('Ctrl Pts',(20.6394660743292,-19.8744759900004,
1.97036903943696));
#171240=CARTESIAN_POINT('Ctrl Pts',(20.64319653363,-19.8667302909141,1.9698511696023));
#171241=CARTESIAN_POINT('Ctrl Pts',(20.6550374899063,-19.8417564549656,
1.96818096005817));
#171242=CARTESIAN_POINT('Ctrl Pts',(20.6629625844605,-19.8244419163164,
1.96702224650926));
#171243=CARTESIAN_POINT('Ctrl Pts',(20.7016633657586,-19.7367835081093,
1.96115072129043));
#171244=CARTESIAN_POINT('Ctrl Pts',(20.7288263091356,-19.6649165310286,
1.95631684499926));
#171245=CARTESIAN_POINT('Ctrl Pts',(20.7859350761981,-19.484770034785,1.94416142901015));
#171246=CARTESIAN_POINT('Ctrl Pts',(20.811284678941,-19.3752803138305,1.93673372124309));
#171247=CARTESIAN_POINT('Ctrl Pts',(20.8387416783276,-19.1911976000624,
1.92444377814641));
#171248=CARTESIAN_POINT('Ctrl Pts',(20.8458104712599,-19.1175620615204,
1.91958263215513));
#171249=CARTESIAN_POINT('Ctrl Pts',(20.8508466541166,-19.0014102367269,
1.91212805660246));
#171250=CARTESIAN_POINT('Ctrl Pts',(20.8514115646084,-18.9590675444051,
1.90945536089138));
#171251=CARTESIAN_POINT('Ctrl Pts',(20.8505820385815,-18.9092793911404,
1.90638686384221));
#171252=CARTESIAN_POINT('Ctrl Pts',(20.8504184733629,-18.9018260442319,
1.90592946551947));
#171253=CARTESIAN_POINT('Ctrl Pts',(20.8500901260508,-18.889768140469,1.90519283369693));
#171254=CARTESIAN_POINT('Ctrl Pts',(20.8499496804811,-18.8851630602953,
1.90491229223299));
#171255=CARTESIAN_POINT('Ctrl Pts',(20.8496735777288,-18.8769860764492,
1.90441559481882));
#171256=CARTESIAN_POINT('Ctrl Pts',(20.8495439067984,-18.8734140260176,
1.90419910818447));
#171257=CARTESIAN_POINT('Ctrl Pts',(20.8492463489532,-18.8657524806071,
1.90373583898263));
#171258=CARTESIAN_POINT('Ctrl Pts',(20.8490756501035,-18.8616631506368,
1.90348921552593));
#171259=CARTESIAN_POINT('Ctrl Pts',(20.8485735874786,-18.850418237488,1.90281275807648));
#171260=CARTESIAN_POINT('Ctrl Pts',(20.8482177600928,-18.8432637246195,
1.9023842729894));
#171261=CARTESIAN_POINT('Ctrl Pts',(20.8461060910646,-18.8047466814009,
1.90008709494134));
#171262=CARTESIAN_POINT('Ctrl Pts',(20.8436886072698,-18.7734225730965,
1.89825323777532));
#171263=CARTESIAN_POINT('Ctrl Pts',(20.8243542322785,-18.5793237258596,
1.88703960378519));
#171264=CARTESIAN_POINT('Ctrl Pts',(20.7893060586996,-18.4188980447585,
1.87839183547954));
#171265=CARTESIAN_POINT('Ctrl Pts',(20.6980565429817,-18.1533186682206,
1.86302000638181));
#171266=CARTESIAN_POINT('Ctrl Pts',(20.6508708197679,-18.0459034576789,
1.85648178334411));
#171267=CARTESIAN_POINT('Ctrl Pts',(20.5882363068399,-17.9303831276721,
1.84878351034564));
#171268=CARTESIAN_POINT('Ctrl Pts',(20.5812962745788,-17.9178869624485,
1.84794177047477));
#171269=CARTESIAN_POINT('Ctrl Pts',(20.5700502057172,-17.8981118922739,
1.84659488931344));
#171270=CARTESIAN_POINT('Ctrl Pts',(20.5658261032948,-17.8907867200022,
1.84609269131902));
#171271=CARTESIAN_POINT('Ctrl Pts',(20.5582992308094,-17.8779129414109,
1.84520420099984));
#171272=CARTESIAN_POINT('Ctrl Pts',(20.5550147293013,-17.8723537397822,
1.84481857508423));
#171273=CARTESIAN_POINT('Ctrl Pts',(20.548169063422,-17.8608871792916,1.84401907775769));
#171274=CARTESIAN_POINT('Ctrl Pts',(20.544604361378,-17.854982031597,1.84360508018427));
#171275=CARTESIAN_POINT('Ctrl Pts',(20.5353808316011,-17.8398701128789,
1.84253972732813));
#171276=CARTESIAN_POINT('Ctrl Pts',(20.5296803011461,-17.8306891440899,
1.84188684340652));
#171277=CARTESIAN_POINT('Ctrl Pts',(20.5055998716988,-17.7925610653245,
1.839151474149));
#171278=CARTESIAN_POINT('Ctrl Pts',(20.4865891858849,-17.7640203376469,
1.83704567214399));
#171279=CARTESIAN_POINT('Ctrl Pts',(20.4352615146701,-17.6908771120922,
1.83149159397724));
#171280=CARTESIAN_POINT('Ctrl Pts',(20.4018838923408,-17.6470539543977,
1.82800493913055));
#171281=CARTESIAN_POINT('Ctrl Pts',(20.2972294796716,-17.5202306284797,
1.81743623275423));
#171282=CARTESIAN_POINT('Ctrl Pts',(20.2211934822354,-17.4414034227911,
1.81020578731047));
#171283=CARTESIAN_POINT('Ctrl Pts',(20.0508008596991,-17.2901440020614,
1.79515491381617));
#171284=CARTESIAN_POINT('Ctrl Pts',(19.9557263873125,-17.2190484618821,
1.787362537917));
#171285=CARTESIAN_POINT('Ctrl Pts',(19.8471142469255,-17.1512345095083,
1.77945379048602));
#171286=CARTESIAN_POINT('Ctrl Pts',(19.8390027594011,-17.146245701111,1.77886882479014));
#171287=CARTESIAN_POINT('Ctrl Pts',(19.8269353937759,-17.1389356726576,
1.77800728659057));
#171288=CARTESIAN_POINT('Ctrl Pts',(19.8230053212772,-17.1365723806239,
1.7777280602783));
#171289=CARTESIAN_POINT('Ctrl Pts',(19.8160002025276,-17.1323908873519,
1.77723281004933));
#171290=CARTESIAN_POINT('Ctrl Pts',(19.8129282087537,-17.1305676839048,
1.77701646273488));
#171291=CARTESIAN_POINT('Ctrl Pts',(19.8063147171267,-17.1266652328655,
1.77655250918701));
#171292=CARTESIAN_POINT('Ctrl Pts',(19.8027717902178,-17.124588517665,1.77630506722681));
#171293=CARTESIAN_POINT('Ctrl Pts',(19.7929782376184,-17.1188861718591,
1.77562405119693));
#171294=CARTESIAN_POINT('Ctrl Pts',(19.7867149897119,-17.1152821750386,
1.77519185638822));
#171295=CARTESIAN_POINT('Ctrl Pts',(19.7523472612142,-17.0957398524043,
1.77283781471752));
#171296=CARTESIAN_POINT('Ctrl Pts',(19.7238975418857,-17.080413508965,1.77095287569351));
#171297=CARTESIAN_POINT('Ctrl Pts',(19.5499866865743,-16.9918005114291,
1.75974323446217));
#171298=CARTESIAN_POINT('Ctrl Pts',(19.3968036625889,-16.9348436998903,
1.75113480058229));
#171299=CARTESIAN_POINT('Ctrl Pts',(19.1250576175935,-16.8681504438336,
1.73581694083408));
#171300=CARTESIAN_POINT('Ctrl Pts',(19.0094274171547,-16.8497418085637,
1.7292910629989));
#171301=CARTESIAN_POINT('Ctrl Pts',(18.8786271755125,-16.8398976801939,
1.7216066849587));
#171302=CARTESIAN_POINT('Ctrl Pts',(18.864366372587,-16.8389695167336,1.72076512015129));
#171303=CARTESIAN_POINT('Ctrl Pts',(18.8416552559231,-16.8377221486527,
1.7194184664676));
#171304=CARTESIAN_POINT('Ctrl Pts',(18.8332103846389,-16.8373090572752,
1.71891631930771));
#171305=CARTESIAN_POINT('Ctrl Pts',(18.818312422805,-16.8366697405475,1.71802788782991));
#171306=CARTESIAN_POINT('Ctrl Pts',(18.811860311207,-16.8364224283407,1.71764226963368));
#171307=CARTESIAN_POINT('Ctrl Pts',(18.7985130896356,-16.8359719650985,
1.71684275777739));
#171308=CARTESIAN_POINT('Ctrl Pts',(18.7916179238947,-16.835772990363,1.71642873780404));
#171309=CARTESIAN_POINT('Ctrl Pts',(18.7739166660637,-16.8353487577163,
1.71536326299231));
#171310=CARTESIAN_POINT('Ctrl Pts',(18.763109696509,-16.8351725529758,1.71471027884528));
#171311=CARTESIAN_POINT('Ctrl Pts',(18.7179999081334,-16.8347825527538,
1.71197394267123));
#171312=CARTESIAN_POINT('Ctrl Pts',(18.6836973667649,-16.8353197807208,
1.70986725341227));
#171313=CARTESIAN_POINT('Ctrl Pts',(18.5943673693626,-16.8388914215216,
1.70431027686346));
#171314=CARTESIAN_POINT('Ctrl Pts',(18.539421263544,-16.8432412583345,1.70082156104504));
#171315=CARTESIAN_POINT('Ctrl Pts',(18.3808407993589,-16.8620458663092,
1.69055706253802));
#171316=CARTESIAN_POINT('Ctrl Pts',(18.2780335179298,-16.8820431983753,
1.68365068975032));
#171317=CARTESIAN_POINT('Ctrl Pts',(18.0581328402662,-16.9419983944864,
1.66859016502744));
#171318=CARTESIAN_POINT('Ctrl Pts',(17.9421811055153,-16.98478555336,1.66046097023692));
#171319=CARTESIAN_POINT('Ctrl Pts',(17.8220692052393,-17.0414607256951,
1.65225898559873));
#171320=CARTESIAN_POINT('Ctrl Pts',(17.8135597146947,-17.045545756681,1.65167921893351));
#171321=CARTESIAN_POINT('Ctrl Pts',(17.8009716093122,-17.0516926822473,
1.6508238396777));
#171322=CARTESIAN_POINT('Ctrl Pts',(17.796872024498,-17.0537110235346,1.65054562693728));
#171323=CARTESIAN_POINT('Ctrl Pts',(17.7895805346866,-17.0573302071775,
1.65005148501018));
#171324=CARTESIAN_POINT('Ctrl Pts',(17.7863861209334,-17.0589258632729,
1.64983523806324));
#171325=CARTESIAN_POINT('Ctrl Pts',(17.7795905838122,-17.0623418438325,
1.64937572599234));
#171326=CARTESIAN_POINT('Ctrl Pts',(17.7759906352782,-17.0641643772275,
1.64913260219275));
#171327=CARTESIAN_POINT('Ctrl Pts',(17.766164494739,-17.0691743683178,1.6484697616433));
#171328=CARTESIAN_POINT('Ctrl Pts',(17.7599487897929,-17.072382441142,1.64805131888324));
#171329=CARTESIAN_POINT('Ctrl Pts',(17.7460917540264,-17.0796215838848,
1.64712010829601));
#171330=CARTESIAN_POINT('Ctrl Pts',(17.7384589252216,-17.0836687634402,
1.64660830029875));
#171331=CARTESIAN_POINT('Ctrl Pts',(17.7150040138148,-17.096289888059,1.64503839395978));
#171332=CARTESIAN_POINT('Ctrl Pts',(17.699265914446,-17.1050191512982,1.64398898820383));
#171333=CARTESIAN_POINT('Ctrl Pts',(17.6391124288452,-17.1393940195727,
1.63998604701163));
#171334=CARTESIAN_POINT('Ctrl Pts',(17.5955206089469,-17.1664511719524,
1.63710213117425));
#171335=CARTESIAN_POINT('Ctrl Pts',(17.4396156582002,-17.2712538083259,
1.62669260069816));
#171336=CARTESIAN_POINT('Ctrl Pts',(17.3339153733609,-17.3582296089895,
1.61942629536931));
#171337=CARTESIAN_POINT('Ctrl Pts',(17.1677260897055,-17.5243585953945,
1.60646827782242));
#171338=CARTESIAN_POINT('Ctrl Pts',(17.1030698550247,-17.5986939526255,
1.60092467288424));
#171339=CARTESIAN_POINT('Ctrl Pts',(17.0354279899442,-17.6883796259513,
1.59434072383888));
#171340=CARTESIAN_POINT('Ctrl Pts',(17.0271443287725,-17.699591509611,1.59351954304025));
#171341=CARTESIAN_POINT('Ctrl Pts',(17.0140751751975,-17.7176510349408,
1.59219943388756));
#171342=CARTESIAN_POINT('Ctrl Pts',(17.0092183520962,-17.7244467284401,
1.59170326642351));
#171343=CARTESIAN_POINT('Ctrl Pts',(17.0006880677466,-17.7365329181981,
1.59082177070814));
#171344=CARTESIAN_POINT('Ctrl Pts',(16.9969982740845,-17.7418117980301,
1.59043707512971));
#171345=CARTESIAN_POINT('Ctrl Pts',(16.9893819665393,-17.7528148182868,
1.58963584722513));
#171346=CARTESIAN_POINT('Ctrl Pts',(16.985459406972,-17.7585415903918,1.58921917062955));
#171347=CARTESIAN_POINT('Ctrl Pts',(16.9753908836527,-17.7733974005587,
1.58813909123413));
#171348=CARTESIAN_POINT('Ctrl Pts',(16.9692878714939,-17.7825551710961,
1.58747407750949));
#171349=CARTESIAN_POINT('Ctrl Pts',(16.943496282987,-17.8219179611135,1.58461871293199));
#171350=CARTESIAN_POINT('Ctrl Pts',(16.9245106312976,-17.8525742640169,
1.58240241153226));
#171351=CARTESIAN_POINT('Ctrl Pts',(16.8765273212873,-17.9346655813933,
1.57648341351698));
#171352=CARTESIAN_POINT('Ctrl Pts',(16.8488840145837,-17.9868519295412,
1.57273575394182));
#171353=CARTESIAN_POINT('Ctrl Pts',(16.7944907198973,-18.1008151574872,
1.56459391176849));
#171354=CARTESIAN_POINT('Ctrl Pts',(16.7684520761493,-18.1628105935934,
1.5601895301041));
#171355=CARTESIAN_POINT('Ctrl Pts',(16.7454191832631,-18.2258902732327,
1.55576066005867));
#171356=CARTESIAN_POINT('',(16.62007989375,-18.9528282577771,2.08900081341629));
#171357=CARTESIAN_POINT('Ctrl Pts',(16.7454193692336,-18.2258897639197,
1.33163196665472));
#171358=CARTESIAN_POINT('Ctrl Pts',(16.7469780089451,-18.2216211548481,
1.33190185432591));
#171359=CARTESIAN_POINT('Ctrl Pts',(16.7485503828935,-18.2173575917481,
1.33217219704567));
#171360=CARTESIAN_POINT('Ctrl Pts',(16.752380836381,-18.2070732661986,1.33282619209588));
#171361=CARTESIAN_POINT('Ctrl Pts',(16.7546526300675,-18.2010577012268,
1.33321029920865));
#171362=CARTESIAN_POINT('Ctrl Pts',(16.7594433952834,-18.1885448446607,
1.33401258755428));
#171363=CARTESIAN_POINT('Ctrl Pts',(16.7619671080003,-18.1820494622973,
1.33443092439066));
#171364=CARTESIAN_POINT('Ctrl Pts',(16.7686050699071,-18.1652118088885,
1.33552028607709));
#171365=CARTESIAN_POINT('Ctrl Pts',(16.7727688572223,-18.1548894141375,
1.33619297516802));
#171366=CARTESIAN_POINT('Ctrl Pts',(16.7912114292374,-18.110188050701,1.33912754616079));
#171367=CARTESIAN_POINT('Ctrl Pts',(16.8063135109684,-18.0761579407643,
1.34141720640058));
#171368=CARTESIAN_POINT('Ctrl Pts',(16.8488256589398,-17.9867963777953,
1.34758320257742));
#171369=CARTESIAN_POINT('Ctrl Pts',(16.8777709018602,-17.932238882343,1.35150931092493));
#171370=CARTESIAN_POINT('Ctrl Pts',(16.9832811504378,-17.7527838577309,
1.36495842800826));
#171371=CARTESIAN_POINT('Ctrl Pts',(17.0704045413428,-17.6345855675469,
1.37476374262784));
#171372=CARTESIAN_POINT('Ctrl Pts',(17.1821619049304,-17.5119067325975,
1.38559625226587));
#171373=CARTESIAN_POINT('Ctrl Pts',(17.1955076964967,-17.497657689187,1.38686501323907));
#171374=CARTESIAN_POINT('Ctrl Pts',(17.2456814202752,-17.4455518515892,
1.39153840666011));
#171375=CARTESIAN_POINT('Ctrl Pts',(17.2837281423924,-17.4088892563266,
1.39489463915846));
#171376=CARTESIAN_POINT('Ctrl Pts',(17.3295906039455,-17.3678917919831,
1.3986891918161));
#171377=CARTESIAN_POINT('Ctrl Pts',(17.3361072826765,-17.3621382062489,
1.39922271506066));
#171378=CARTESIAN_POINT('Ctrl Pts',(17.3460336267214,-17.3534824398874,
1.40002662231329));
#171379=CARTESIAN_POINT('Ctrl Pts',(17.3494172706136,-17.3505507470801,
1.40029912782608));
#171380=CARTESIAN_POINT('Ctrl Pts',(17.3555106795293,-17.3453049790022,
1.40078709230336));
#171381=CARTESIAN_POINT('Ctrl Pts',(17.3582169964169,-17.3429870029183,
1.40100283730247));
#171382=CARTESIAN_POINT('Ctrl Pts',(17.3641139356768,-17.337961996103,1.4014708084251));
#171383=CARTESIAN_POINT('Ctrl Pts',(17.3673067243892,-17.3352575967872,
1.40172284187846));
#171384=CARTESIAN_POINT('Ctrl Pts',(17.3763062231306,-17.3276804288929,
1.40242955523647));
#171385=CARTESIAN_POINT('Ctrl Pts',(17.3821311845605,-17.322829299732,1.40288267925102));
#171386=CARTESIAN_POINT('Ctrl Pts',(17.4172897232876,-17.293867063297,1.40559281551996));
#171387=CARTESIAN_POINT('Ctrl Pts',(17.4472435822403,-17.2705158003604,
1.40779849345484));
#171388=CARTESIAN_POINT('Ctrl Pts',(17.5483186251552,-17.1960041054724,
1.41496680558571));
#171389=CARTESIAN_POINT('Ctrl Pts',(17.621989712496,-17.1484486546492,1.41976115841988));
#171390=CARTESIAN_POINT('Ctrl Pts',(17.8507181970275,-17.0201611612989,
1.43402845205778));
#171391=CARTESIAN_POINT('Ctrl Pts',(18.0130018697045,-16.953915166998,1.44342145294553));
#171392=CARTESIAN_POINT('Ctrl Pts',(18.2038295264748,-16.9023317694933,
1.45490743175263));
#171393=CARTESIAN_POINT('Ctrl Pts',(18.2261829698051,-16.8966794924945,
1.45625813314429));
#171394=CARTESIAN_POINT('Ctrl Pts',(18.2579262536769,-16.8892023540638,
1.45818536421926));
#171395=CARTESIAN_POINT('Ctrl Pts',(18.2672434753156,-16.8870741703077,
1.45875214469973));
#171396=CARTESIAN_POINT('Ctrl Pts',(18.2824027876545,-16.8837194126031,
1.45967621774609));
#171397=CARTESIAN_POINT('Ctrl Pts',(18.2882362840617,-16.8824543158388,
1.46003227046598));
#171398=CARTESIAN_POINT('Ctrl Pts',(18.3004560173951,-16.8798583132181,
1.46077910342176));
#171399=CARTESIAN_POINT('Ctrl Pts',(18.3068432030002,-16.8785322225193,
1.46117003357874));
#171400=CARTESIAN_POINT('Ctrl Pts',(18.3220485566541,-16.8754485662721,
1.46210207030448));
#171401=CARTESIAN_POINT('Ctrl Pts',(18.330871940371,-16.8737176293311,1.46264402126151));
#171402=CARTESIAN_POINT('Ctrl Pts',(18.3606155311281,-16.8680791859027,
1.46447480585121));
#171403=CARTESIAN_POINT('Ctrl Pts',(18.3815830380425,-16.8644310420847,
1.4657718505232));
#171404=CARTESIAN_POINT('Ctrl Pts',(18.560027681871,-16.8361483419412,1.47686847813807));
#171405=CARTESIAN_POINT('Ctrl Pts',(18.7197391318618,-16.8290602832147,
1.48724159313066));
#171406=CARTESIAN_POINT('Ctrl Pts',(19.0099955999645,-16.8489463452772,
1.50645979812625));
#171407=CARTESIAN_POINT('Ctrl Pts',(19.1401771170331,-16.8701655909268,
1.5151976290909));
#171408=CARTESIAN_POINT('Ctrl Pts',(19.2827888655724,-16.9073074487044,
1.52439146147466));
#171409=CARTESIAN_POINT('Ctrl Pts',(19.2979796407365,-16.9114452110457,
1.52536556984897));
#171410=CARTESIAN_POINT('Ctrl Pts',(19.3187007994414,-16.9173384558227,
1.52668584074879));
#171411=CARTESIAN_POINT('Ctrl Pts',(19.3242717868769,-16.9189476534882,
1.52703995934182));
#171412=CARTESIAN_POINT('Ctrl Pts',(19.3331111279451,-16.921540321884,1.52760041106523));
#171413=CARTESIAN_POINT('Ctrl Pts',(19.3363837882496,-16.9225088272872,
1.52780760179939));
#171414=CARTESIAN_POINT('Ctrl Pts',(19.3431353839554,-16.924524652782,1.52823438145459));
#171415=CARTESIAN_POINT('Ctrl Pts',(19.3466139669554,-16.9255730145887,
1.52845390213702));
#171416=CARTESIAN_POINT('Ctrl Pts',(19.354892372933,-16.9280911928808,1.52897548174013));
#171417=CARTESIAN_POINT('Ctrl Pts',(19.3596897368803,-16.9295691476233,
1.52927706600975));
#171418=CARTESIAN_POINT('Ctrl Pts',(19.3758337328626,-16.9346056739562,
1.5302898239611));
#171419=CARTESIAN_POINT('Ctrl Pts',(19.3871558638069,-16.9382428548627,
1.53099654512627));
#171420=CARTESIAN_POINT('Ctrl Pts',(19.5221729641012,-16.9828749998802,
1.53938838433947));
#171421=CARTESIAN_POINT('Ctrl Pts',(19.6418773231725,-17.0351174996117,
1.54647743995801));
#171422=CARTESIAN_POINT('Ctrl Pts',(19.8981299046051,-17.1763819220244,
1.56237387340025));
#171423=CARTESIAN_POINT('Ctrl Pts',(20.0307355897197,-17.2707838276206,
1.57115663668387));
#171424=CARTESIAN_POINT('Ctrl Pts',(20.168878505492,-17.3952805290851,1.58195490276796));
#171425=CARTESIAN_POINT('Ctrl Pts',(20.1862331046894,-17.4114576346305,
1.58334411948527));
#171426=CARTESIAN_POINT('Ctrl Pts',(20.2102717720847,-17.4346325027105,
1.58531698577307));
#171427=CARTESIAN_POINT('Ctrl Pts',(20.2171857298994,-17.4413900063892,
1.58589024094843));
#171428=CARTESIAN_POINT('Ctrl Pts',(20.2283073981905,-17.4524099664384,
1.58682198497202));
#171429=CARTESIAN_POINT('Ctrl Pts',(20.2325437818724,-17.4566433864389,
1.5871791920608));
#171430=CARTESIAN_POINT('Ctrl Pts',(20.2413447944384,-17.4655132014424,
1.58792612371419));
#171431=CARTESIAN_POINT('Ctrl Pts',(20.2459061215589,-17.4701527711222,
1.58831598794524));
#171432=CARTESIAN_POINT('Ctrl Pts',(20.2566543663712,-17.4811866721208,
1.58924124341416));
#171433=CARTESIAN_POINT('Ctrl Pts',(20.2628224660245,-17.4875990888769,
1.5897774467552));
#171434=CARTESIAN_POINT('Ctrl Pts',(20.2832287960464,-17.5090831566346,
1.59156906342601));
#171435=CARTESIAN_POINT('Ctrl Pts',(20.2972856713562,-17.5243247073985,
1.59283221785415));
#171436=CARTESIAN_POINT('Ctrl Pts',(20.371130264684,-17.6067910760653,1.59962724714155));
#171437=CARTESIAN_POINT('Ctrl Pts',(20.4268036828167,-17.6775610479136,
1.60532712714341));
#171438=CARTESIAN_POINT('Ctrl Pts',(20.5546065910936,-17.8632259826244,
1.61993455285906));
#171439=CARTESIAN_POINT('Ctrl Pts',(20.6205227926009,-17.9819147995188,
1.62898784864941));
#171440=CARTESIAN_POINT('Ctrl Pts',(20.7047984212395,-18.1752519701093,
1.6427793589995));
#171441=CARTESIAN_POINT('Ctrl Pts',(20.7312360825949,-18.246001089841,1.64763738032002));
#171442=CARTESIAN_POINT('Ctrl Pts',(20.7566829422805,-18.3270737668287,
1.65288547815168));
#171443=CARTESIAN_POINT('Ctrl Pts',(20.7594644044671,-18.3361485277717,
1.6534684931989));
#171444=CARTESIAN_POINT('Ctrl Pts',(20.7634973863682,-18.3496294064328,
1.65432771863036));
#171445=CARTESIAN_POINT('Ctrl Pts',(20.7647957461813,-18.3540212282426,
1.65460656269733));
#171446=CARTESIAN_POINT('Ctrl Pts',(20.7670813031071,-18.3618456375569,
1.65510139107388));
#171447=CARTESIAN_POINT('Ctrl Pts',(20.7680740731972,-18.3652765370669,
1.65531769668012));
#171448=CARTESIAN_POINT('Ctrl Pts',(20.770190773628,-18.3726615575667,1.65578184656254));
#171449=CARTESIAN_POINT('Ctrl Pts',(20.7713118682925,-18.3766164327475,
1.65602952506099));
#171450=CARTESIAN_POINT('Ctrl Pts',(20.7743768450923,-18.3875499934551,
1.65671186958355));
#171451=CARTESIAN_POINT('Ctrl Pts',(20.7762964576538,-18.3945355057206,
1.65714514739522));
#171452=CARTESIAN_POINT('Ctrl Pts',(20.786651167271,-18.4329879646419,1.6595161752194));
#171453=CARTESIAN_POINT('Ctrl Pts',(20.79439540772,-18.4646383948966,1.66141638526182));
#171454=CARTESIAN_POINT('Ctrl Pts',(20.8364045223904,-18.6552897504772,
1.67262496741146));
#171455=CARTESIAN_POINT('Ctrl Pts',(20.85298602281,-18.817642977263,1.68122171408322));
#171456=CARTESIAN_POINT('Ctrl Pts',(20.8492485224996,-19.097127165588,1.69652342599794));
#171457=CARTESIAN_POINT('Ctrl Pts',(20.8380194334806,-19.2136011642474,
1.70304550944014));
#171458=CARTESIAN_POINT('Ctrl Pts',(20.8147014981872,-19.3426078253938,
1.71072561209554));
#171459=CARTESIAN_POINT('Ctrl Pts',(20.8120175439466,-19.356643386154,1.71156711253977));
#171460=CARTESIAN_POINT('Ctrl Pts',(20.8075197981348,-19.3789380834008,
1.7129136784744));
#171461=CARTESIAN_POINT('Ctrl Pts',(20.8057982323896,-19.3872155344412,
1.7134158027586));
#171462=CARTESIAN_POINT('Ctrl Pts',(20.8026745525841,-19.4017958257363,
1.71430420272433));
#171463=CARTESIAN_POINT('Ctrl Pts',(20.8012930918349,-19.408103015102,1.71468981237914));
#171464=CARTESIAN_POINT('Ctrl Pts',(20.7983761098417,-19.4211352259918,
1.71548931529257));
#171465=CARTESIAN_POINT('Ctrl Pts',(20.7968365309985,-19.4278592520668,
1.7159033349055));
#171466=CARTESIAN_POINT('Ctrl Pts',(20.7928002588448,-19.4450997082577,
1.7169688271686));
#171467=CARTESIAN_POINT('Ctrl Pts',(20.7902558605417,-19.4556046637053,
1.71762182929343));
#171468=CARTESIAN_POINT('Ctrl Pts',(20.7793001312434,-19.4993694674615,
1.72035839537104));
#171469=CARTESIAN_POINT('Ctrl Pts',(20.7701617717159,-19.5324403361604,
1.722465302016));
#171470=CARTESIAN_POINT('Ctrl Pts',(20.7442598175371,-19.6180191232367,
1.72802300249671));
#171471=CARTESIAN_POINT('Ctrl Pts',(20.7262429966346,-19.670117697727,1.73151223825882));
#171472=CARTESIAN_POINT('Ctrl Pts',(20.6664533298185,-19.8233674071083,
1.74208589180962));
#171473=CARTESIAN_POINT('Ctrl Pts',(20.6188535389836,-19.9220415974775,
1.74931868870912));
#171474=CARTESIAN_POINT('Ctrl Pts',(20.5394820030683,-20.0584679847767,
1.75974486664127));
#171475=CARTESIAN_POINT('Ctrl Pts',(20.5136850643191,-20.0995007510991,
1.76293918765385));
#171476=CARTESIAN_POINT('Ctrl Pts',(20.4766022627348,-20.15422202012,1.7672515224871));
#171477=CARTESIAN_POINT('Ctrl Pts',(20.4665197717848,-20.1687069065792,
1.76839817538964));
#171478=CARTESIAN_POINT('Ctrl Pts',(20.4252331100915,-20.2264668857623,
1.77298679902957));
#171479=CARTESIAN_POINT('Ctrl Pts',(20.3925765095485,-20.2686853361526,
1.77637829090998));
#171480=CARTESIAN_POINT('Ctrl Pts',(20.3527644317497,-20.3163191551136,
1.78020788443709));
#171481=CARTESIAN_POINT('Ctrl Pts',(20.3471307613491,-20.3229756362923,
1.78074310562718));
#171482=CARTESIAN_POINT('Ctrl Pts',(20.3385386736289,-20.3330013554091,
1.78154907719668));
#171483=CARTESIAN_POINT('Ctrl Pts',(20.3356104994851,-20.3363962249324,
1.78182196459178));
#171484=CARTESIAN_POINT('Ctrl Pts',(20.3303352547835,-20.3424731049659,
1.78231034749108));
#171485=CARTESIAN_POINT('Ctrl Pts',(20.3279921868627,-20.3451585014285,
1.78252613113583));
#171486=CARTESIAN_POINT('Ctrl Pts',(20.3228864021595,-20.3509805113537,
1.78299387618881));
#171487=CARTESIAN_POINT('Ctrl Pts',(20.3201211831963,-20.3541148537207,
1.78324564659638));
#171488=CARTESIAN_POINT('Ctrl Pts',(20.312328381068,-20.3628953455847,1.78395089266421));
#171489=CARTESIAN_POINT('Ctrl Pts',(20.3072797517182,-20.3685228488869,
1.78440282271366));
#171490=CARTESIAN_POINT('Ctrl Pts',(20.2769299784554,-20.4019900913812,
1.78709093366332));
#171491=CARTESIAN_POINT('Ctrl Pts',(20.250918878903,-20.429180317943,1.78927674428094));
#171492=CARTESIAN_POINT('Ctrl Pts',(20.1629639659735,-20.5163473506456,
1.79634826981673));
#171493=CARTESIAN_POINT('Ctrl Pts',(20.0980782206357,-20.5732382943573,
1.80107084203581));
#171494=CARTESIAN_POINT('Ctrl Pts',(19.8902352996053,-20.7341347677382,
1.81537497403396));
#171495=CARTESIAN_POINT('Ctrl Pts',(19.7376084161582,-20.8243375496902,
1.82486496392234));
#171496=CARTESIAN_POINT('Ctrl Pts',(19.5545390772695,-20.9036478593207,
1.83645921108515));
#171497=CARTESIAN_POINT('Ctrl Pts',(19.5333737533294,-20.9124120195365,
1.83780132308227));
#171498=CARTESIAN_POINT('Ctrl Pts',(19.5032057142976,-20.9243342608018,
1.83971837378418));
#171499=CARTESIAN_POINT('Ctrl Pts',(19.4943170104229,-20.9277777978266,
1.84028370387923));
#171500=CARTESIAN_POINT('Ctrl Pts',(19.4798293982838,-20.9332781437326,
1.84120604403086));
#171501=CARTESIAN_POINT('Ctrl Pts',(19.47424445741,-20.935371552768,1.84156182341835));
#171502=CARTESIAN_POINT('Ctrl Pts',(19.4625294868531,-20.9397063131477,
1.84230859847614));
#171503=CARTESIAN_POINT('Ctrl Pts',(19.4563977974758,-20.9419429693494,
1.84269974633753));
#171504=CARTESIAN_POINT('Ctrl Pts',(19.4417751703768,-20.9472003730462,
1.84363325480104));
#171505=CARTESIAN_POINT('Ctrl Pts',(19.4332751454164,-20.950195307642,1.844176467059));
#171506=CARTESIAN_POINT('Ctrl Pts',(19.4045222170771,-20.9601203050596,
1.84601605398008));
#171507=CARTESIAN_POINT('Ctrl Pts',(19.3841839186975,-20.9667972657927,
1.84732074829423));
#171508=CARTESIAN_POINT('Ctrl Pts',(19.2725577184012,-21.0015774263021,
1.85450266061469));
#171509=CARTESIAN_POINT('Ctrl Pts',(19.1795609380738,-21.0237826208264,
1.86057006010431));
#171510=CARTESIAN_POINT('Ctrl Pts',(18.9174225540787,-21.0679061201764,
1.87784605121419));
#171511=CARTESIAN_POINT('Ctrl Pts',(18.7466642970659,-21.0758029789536,
1.88933830324689));
#171512=CARTESIAN_POINT('Ctrl Pts',(18.5401936393751,-21.0604298124125,
1.90255187805656));
#171513=CARTESIAN_POINT('Ctrl Pts',(18.5036519322531,-21.0567511306786,
1.90486141653235));
#171514=CARTESIAN_POINT('Ctrl Pts',(18.4601413497464,-21.0512239957896,
1.90756231597942));
#171515=CARTESIAN_POINT('Ctrl Pts',(18.453065164394,-21.0502887232869,1.90800000670298));
#171516=CARTESIAN_POINT('Ctrl Pts',(18.4415246335658,-21.048703963245,1.9087111374922));
#171517=CARTESIAN_POINT('Ctrl Pts',(18.4370574615614,-21.0480759717136,
1.90898574517932));
#171518=CARTESIAN_POINT('Ctrl Pts',(18.4290627168522,-21.0469260056001,
1.9094759757948));
#171519=CARTESIAN_POINT('Ctrl Pts',(18.4255344373287,-21.0464093947568,
1.90969189644735));
#171520=CARTESIAN_POINT('Ctrl Pts',(18.4178939429926,-21.0452709468414,
1.91015853495268));
#171521=CARTESIAN_POINT('Ctrl Pts',(18.4137822631944,-21.0446459083862,
1.9104090693682));
#171522=CARTESIAN_POINT('Ctrl Pts',(18.4022962796745,-21.0428652172993,
1.91110737182983));
#171523=CARTESIAN_POINT('Ctrl Pts',(18.3949261227597,-21.0416826612019,
1.91155364281015));
#171524=CARTESIAN_POINT('Ctrl Pts',(18.3520512124472,-21.034570492711,1.9141400490475));
#171525=CARTESIAN_POINT('Ctrl Pts',(18.3166937771664,-21.0277746981841,
1.91623414697787));
#171526=CARTESIAN_POINT('Ctrl Pts',(18.203351803317,-21.0029765966068,1.92287097850404));
#171527=CARTESIAN_POINT('Ctrl Pts',(18.1262052594277,-20.9814531437156,
1.92727266053633));
#171528=CARTESIAN_POINT('Ctrl Pts',(17.8746327119347,-20.8956278623516,
1.94176357484675));
#171529=CARTESIAN_POINT('Ctrl Pts',(17.7074882150783,-20.8127710653322,
1.95169893338996));
#171530=CARTESIAN_POINT('Ctrl Pts',(17.5349718850057,-20.6968519498344,
1.96378745058492));
#171531=CARTESIAN_POINT('Ctrl Pts',(17.5168351163464,-20.684248925318,1.96508210270746));
#171532=CARTESIAN_POINT('Ctrl Pts',(17.4920320181413,-20.6664316922833,
1.96688735191551));
#171533=CARTESIAN_POINT('Ctrl Pts',(17.485194405452,-20.6614575394964,1.96738873627143));
#171534=CARTESIAN_POINT('Ctrl Pts',(17.473494033636,-20.6528382169013,1.96825320442167));
#171535=CARTESIAN_POINT('Ctrl Pts',(17.4686168003439,-20.6492127999031,
1.96861551828467));
#171536=CARTESIAN_POINT('Ctrl Pts',(17.45876149504,-20.641820914333,1.9693516682046));
#171537=CARTESIAN_POINT('Ctrl Pts',(17.453784339615,-20.6380533291271,1.96972554583959));
#171538=CARTESIAN_POINT('Ctrl Pts',(17.4422552536449,-20.6292456112844,
1.9705965441672));
#171539=CARTESIAN_POINT('Ctrl Pts',(17.4357160681656,-20.6241890322635,
1.97109431190644));
#171540=CARTESIAN_POINT('Ctrl Pts',(17.4220318999469,-20.6134787742574,
1.97214394385367));
#171541=CARTESIAN_POINT('Ctrl Pts',(17.4148934802356,-20.6078170183652,
1.97269612465169));
#171542=CARTESIAN_POINT('Ctrl Pts',(17.3959861783522,-20.5926210464096,
1.97417117336325));
#171543=CARTESIAN_POINT('Ctrl Pts',(17.3842828553074,-20.5830064424968,
1.97509725650284));
#171544=CARTESIAN_POINT('Ctrl Pts',(17.3489054577014,-20.5533013962361,
1.97793721926199));
#171545=CARTESIAN_POINT('Ctrl Pts',(17.3255701344935,-20.5328156784632,
1.97986693697989));
#171546=CARTESIAN_POINT('Ctrl Pts',(17.178583314136,-20.3979396385281,1.99239379582297));
#171547=CARTESIAN_POINT('Ctrl Pts',(17.0685229075891,-20.2696614622352,
2.00358061034142));
#171548=CARTESIAN_POINT('Ctrl Pts',(16.9197541441153,-20.0474479156722,
2.02119664031841));
#171549=CARTESIAN_POINT('Ctrl Pts',(16.8705007701706,-19.9613906267824,
2.0276487267251));
#171550=CARTESIAN_POINT('Ctrl Pts',(16.8232353237117,-19.8634611010547,
2.03436713444442));
#171551=CARTESIAN_POINT('Ctrl Pts',(16.8190812869546,-19.8547011230302,
2.03496280747162));
#171552=CARTESIAN_POINT('Ctrl Pts',(16.813036907456,-19.8417253150655,2.03583701398545));
#171553=CARTESIAN_POINT('Ctrl Pts',(16.8111000197589,-19.837531482279,2.03611831334073));
#171554=CARTESIAN_POINT('Ctrl Pts',(16.8076882727652,-19.8300802439078,
2.03661584705273));
#171555=CARTESIAN_POINT('Ctrl Pts',(16.8062079246769,-19.8268254112821,
2.03683241629388));
#171556=CARTESIAN_POINT('Ctrl Pts',(16.8030539897002,-19.8198439910867,
2.03729530315268));
#171557=CARTESIAN_POINT('Ctrl Pts',(16.8013829451207,-19.8161163158954,
2.037541464585));
#171558=CARTESIAN_POINT('Ctrl Pts',(16.7968258180321,-19.805871181523,2.03821535303689));
#171559=CARTESIAN_POINT('Ctrl Pts',(16.7939618142904,-19.7993438777717,
2.03864174812156));
#171560=CARTESIAN_POINT('Ctrl Pts',(16.77885106819,-19.7644269782842,2.04090763254381));
#171561=CARTESIAN_POINT('Ctrl Pts',(16.7671937064801,-19.7357845184199,
2.04271339922689));
#171562=CARTESIAN_POINT('Ctrl Pts',(16.7338151908354,-19.6483324993772,
2.048097605773));
#171563=CARTESIAN_POINT('Ctrl Pts',(16.714073417265,-19.5888013575638,2.0515893438376));
#171564=CARTESIAN_POINT('Ctrl Pts',(16.6439835862132,-19.3411372612689,
2.06573526128077));
#171565=CARTESIAN_POINT('Ctrl Pts',(16.6170670028625,-19.147403071309,2.07601658058645));
#171566=CARTESIAN_POINT('Ctrl Pts',(16.6170001249202,-18.9527272634281,
2.08722594301759));
#171567=CARTESIAN_POINT('Ctrl Pts',(16.7452305870807,-18.2258208582162,
2.13351566426921));
#171568=CARTESIAN_POINT('Ctrl Pts',(16.663115235549,-18.4580155040381,2.11869586918697));
#171569=CARTESIAN_POINT('Ctrl Pts',(16.6210475648562,-18.7055595715561,
2.10387607410474));
#171570=CARTESIAN_POINT('Ctrl Pts',(16.6201761380985,-18.9528314139021,
2.0890562790225));
#171571=CARTESIAN_POINT('Origin',(18.734,-18.952,0.));
#171572=CARTESIAN_POINT('',(16.7454192974523,-18.2258899605052,3.15472450021254));
#171573=CARTESIAN_POINT('',(16.7454193844899,-18.2258897221376,2.93545674301194));
#171574=CARTESIAN_POINT('',(16.7454193692319,-18.2258897639242,0.));
#171575=CARTESIAN_POINT('',(16.6170000449368,-18.9524361908011,3.11292713430694));
#171576=CARTESIAN_POINT('Ctrl Pts',(16.7454192974521,-18.225889960506,3.15472450021249));
#171577=CARTESIAN_POINT('Ctrl Pts',(16.6825885674479,-18.3979630216364,
3.14472560045024));
#171578=CARTESIAN_POINT('Ctrl Pts',(16.6422996473866,-18.5776169156608,
3.13494345590111));
#171579=CARTESIAN_POINT('Ctrl Pts',(16.6232302295293,-18.7874467506106,
3.12274999908918));
#171580=CARTESIAN_POINT('Ctrl Pts',(16.6212927654639,-18.8145415057395,
3.12116298812376));
#171581=CARTESIAN_POINT('Ctrl Pts',(16.6193445971276,-18.8518703054087,
3.11895644165119));
#171582=CARTESIAN_POINT('Ctrl Pts',(16.6188859031068,-18.8620790335503,
3.11835093317581));
#171583=CARTESIAN_POINT('Ctrl Pts',(16.6182717244293,-18.8783794128681,
3.1173806802683));
#171584=CARTESIAN_POINT('Ctrl Pts',(16.6180685939011,-18.8844691893339,
3.11701743262623));
#171585=CARTESIAN_POINT('Ctrl Pts',(16.6177137006794,-18.8966923162665,
3.11628677084266));
#171586=CARTESIAN_POINT('Ctrl Pts',(16.6175623043788,-18.9028256174748,
3.11591934881402));
#171587=CARTESIAN_POINT('Ctrl Pts',(16.6172825439101,-18.916583117471,3.11509337943087));
#171588=CARTESIAN_POINT('Ctrl Pts',(16.6171687079755,-18.9242074971486,
3.11463438114429));
#171589=CARTESIAN_POINT('Ctrl Pts',(16.6170306368061,-18.9387001093077,
3.11375948242246));
#171590=CARTESIAN_POINT('Ctrl Pts',(16.6169986298366,-18.945568170754,3.11334383289999));
#171591=CARTESIAN_POINT('Ctrl Pts',(16.6170000449368,-18.9524361908011,
3.11292713430694));
#171592=CARTESIAN_POINT('Ctrl Pts',(16.6170000447699,-18.9524353798984,
3.11292718350627));
#171593=CARTESIAN_POINT('Ctrl Pts',(16.6170022250297,-18.9630367189442,
3.11228397597961));
#171594=CARTESIAN_POINT('Ctrl Pts',(16.6170840379741,-18.9736377765493,
3.11163827929964));
#171595=CARTESIAN_POINT('Ctrl Pts',(16.6175725597191,-19.005714562482,3.10967678155756));
#171596=CARTESIAN_POINT('Ctrl Pts',(16.6182264799695,-19.0271845940186,
3.1083533681113));
#171597=CARTESIAN_POINT('Ctrl Pts',(16.6268700210254,-19.2163322797723,
3.0965992937741));
#171598=CARTESIAN_POINT('Ctrl Pts',(16.6544504544027,-19.3824913203712,
3.08554392257207));
#171599=CARTESIAN_POINT('Ctrl Pts',(16.7246641309952,-19.6237294021958,
3.06894891702627));
#171600=CARTESIAN_POINT('Ctrl Pts',(16.7526994568715,-19.7024005598765,
3.06345845456749));
#171601=CARTESIAN_POINT('Ctrl Pts',(16.7997273686543,-19.8131853824819,
3.05578051716473));
#171602=CARTESIAN_POINT('Ctrl Pts',(16.8150342368137,-19.8467746409251,
3.05346060512787));
#171603=CARTESIAN_POINT('Ctrl Pts',(16.8345081106732,-19.8867064188263,
3.05072704485781));
#171604=CARTESIAN_POINT('Ctrl Pts',(16.8378397184622,-19.8934466090163,
3.05026649507614));
#171605=CARTESIAN_POINT('Ctrl Pts',(16.8430751926107,-19.9038979815383,
3.04955386407448));
#171606=CARTESIAN_POINT('Ctrl Pts',(16.8449541986406,-19.9076214499039,
3.0493002755348));
#171607=CARTESIAN_POINT('Ctrl Pts',(16.8484596150504,-19.9145170981066,
3.048831231323));
#171608=CARTESIAN_POINT('Ctrl Pts',(16.8500830190775,-19.9176906941164,
3.04861559772222));
#171609=CARTESIAN_POINT('Ctrl Pts',(16.8537716962027,-19.9248569945028,
3.04812919544042));
#171610=CARTESIAN_POINT('Ctrl Pts',(16.8558416689543,-19.9288472196476,
3.04785872689899));
#171611=CARTESIAN_POINT('Ctrl Pts',(16.8619902175464,-19.9406078021087,
3.04706254392851));
#171612=CARTESIAN_POINT('Ctrl Pts',(16.8661044749617,-19.9483595362936,
3.04653902685531));
#171613=CARTESIAN_POINT('Ctrl Pts',(16.8962493750174,-20.0043129802856,
3.04276778266457));
#171614=CARTESIAN_POINT('Ctrl Pts',(16.9240964587281,-20.0515181831025,
3.03962703080612));
#171615=CARTESIAN_POINT('Ctrl Pts',(17.0437218103382,-20.2374160980352,
3.02720964487713));
#171616=CARTESIAN_POINT('Ctrl Pts',(17.1498597338429,-20.3661576374113,
3.0184523029206));
#171617=CARTESIAN_POINT('Ctrl Pts',(17.3134437142484,-20.5227737185384,
3.00590896696052));
#171618=CARTESIAN_POINT('Ctrl Pts',(17.3586625469145,-20.5625143033791,
3.00252826190643));
#171619=CARTESIAN_POINT('Ctrl Pts',(17.433970717374,-20.6232118508691,2.99697420538423));
#171620=CARTESIAN_POINT('Ctrl Pts',(17.4630191405319,-20.6454085758499,
2.99484900323994));
#171621=CARTESIAN_POINT('Ctrl Pts',(17.4992593892286,-20.6716428920851,
2.9922114452036));
#171622=CARTESIAN_POINT('Ctrl Pts',(17.5059201137793,-20.6764059389847,
2.99172724205299));
#171623=CARTESIAN_POINT('Ctrl Pts',(17.5188186126926,-20.6855169478644,
2.9907905697513));
#171624=CARTESIAN_POINT('Ctrl Pts',(17.5250525161715,-20.6898701883706,
2.99033831149573));
#171625=CARTESIAN_POINT('Ctrl Pts',(17.5313496175007,-20.6942172826115,
2.98988187391757));
#171626=CARTESIAN_POINT('Ctrl Pts',(17.5313895616197,-20.6942448553101,
2.98987897863404));
#171627=CARTESIAN_POINT('Ctrl Pts',(17.5314710796563,-20.6943011215885,
2.98987306996709));
#171628=CARTESIAN_POINT('Ctrl Pts',(17.5315126534155,-20.6943298148903,
2.98987005659652));
#171629=CARTESIAN_POINT('Ctrl Pts',(17.5315975383756,-20.694388396153,2.98986390395742));
#171630=CARTESIAN_POINT('Ctrl Pts',(17.5316408499326,-20.6944182841724,
2.98986076466458));
#171631=CARTESIAN_POINT('Ctrl Pts',(17.531729329459,-20.6944793363963,2.98985435156234));
#171632=CARTESIAN_POINT('Ctrl Pts',(17.5317744975197,-20.6945105004554,
2.98985107774799));
#171633=CARTESIAN_POINT('Ctrl Pts',(17.5318668207361,-20.6945741942869,
2.98984438613586));
#171634=CARTESIAN_POINT('Ctrl Pts',(17.5319139757756,-20.6946067237464,
2.98984096834838));
#171635=CARTESIAN_POINT('Ctrl Pts',(17.5320104154899,-20.694673245997,2.98983397846438));
#171636=CARTESIAN_POINT('Ctrl Pts',(17.5320597005397,-20.6947072387862,
2.9898304063428));
#171637=CARTESIAN_POINT('Ctrl Pts',(17.5321605587156,-20.6947767961784,
2.98982309631337));
#171638=CARTESIAN_POINT('Ctrl Pts',(17.5322121319455,-20.6948123605603,
2.98981935840036));
#171639=CARTESIAN_POINT('Ctrl Pts',(17.5323177412817,-20.694885180782,2.98981170412615));
#171640=CARTESIAN_POINT('Ctrl Pts',(17.5323717775328,-20.6949224363919,
2.9898077877571));
#171641=CARTESIAN_POINT('Ctrl Pts',(17.5324825070636,-20.6949987719184,
2.98979976250736));
#171642=CARTESIAN_POINT('Ctrl Pts',(17.5325392004475,-20.6950378515339,
2.98979565362213));
#171643=CARTESIAN_POINT('Ctrl Pts',(17.5326554600678,-20.6951179826989,
2.9897872277072));
#171644=CARTESIAN_POINT('Ctrl Pts',(17.5327150265564,-20.6951590339989,
2.98978291066263));
#171645=CARTESIAN_POINT('Ctrl Pts',(17.5328372738104,-20.6952432736158,
2.98977405094231));
#171646=CARTESIAN_POINT('Ctrl Pts',(17.5328999547889,-20.6952864615971,
2.98976950825501));
#171647=CARTESIAN_POINT('Ctrl Pts',(17.5330287015219,-20.6953751594731,
2.9897601776571));
#171648=CARTESIAN_POINT('Ctrl Pts',(17.5330947675712,-20.6954206690185,
2.98975538972957));
#171649=CARTESIAN_POINT('Ctrl Pts',(17.5332305891999,-20.6955142182559,
2.98974554657866));
#171650=CARTESIAN_POINT('Ctrl Pts',(17.5333003450219,-20.6955622574801,
2.98974049134279));
#171651=CARTESIAN_POINT('Ctrl Pts',(17.5334438906292,-20.6956611013263,
2.98973008862948));
#171652=CARTESIAN_POINT('Ctrl Pts',(17.5335176807041,-20.6957119054144,
2.98972474113693));
#171653=CARTESIAN_POINT('Ctrl Pts',(17.5336696860685,-20.695816546106,2.98971372557466));
#171654=CARTESIAN_POINT('Ctrl Pts',(17.5337479017288,-20.6958703821131,
2.98970805748486));
#171655=CARTESIAN_POINT('Ctrl Pts',(17.5339092045359,-20.6959813911893,
2.98969636840872));
#171656=CARTESIAN_POINT('Ctrl Pts',(17.5339922923074,-20.6960385636937,
2.98969034738505));
#171657=CARTESIAN_POINT('Ctrl Pts',(17.5341638523806,-20.696156595721,2.98967791528736));
#171658=CARTESIAN_POINT('Ctrl Pts',(17.5342523251175,-20.6962174543747,
2.98967150419113));
#171659=CARTESIAN_POINT('Ctrl Pts',(17.5344352467908,-20.6963432620896,
2.98965824910214));
#171660=CARTESIAN_POINT('Ctrl Pts',(17.5345296964249,-20.696408210248,2.98965140506984));
#171661=CARTESIAN_POINT('Ctrl Pts',(17.5347252610972,-20.6965426666279,
2.98963723420122));
#171662=CARTESIAN_POINT('Ctrl Pts',(17.534826376884,-20.6966121737155,2.98962990732363));
#171663=CARTESIAN_POINT('Ctrl Pts',(17.5350360728862,-20.696756292104,2.98961471290748));
#171664=CARTESIAN_POINT('Ctrl Pts',(17.5351446575342,-20.6968309044714,
2.98960684506337));
#171665=CARTESIAN_POINT('Ctrl Pts',(17.5353702472038,-20.6969858841434,
2.98959049949621));
#171666=CARTESIAN_POINT('Ctrl Pts',(17.5354872522772,-20.697066249085,2.98958202178857));
#171667=CARTESIAN_POINT('Ctrl Pts',(17.5407538962924,-20.7006828642732,
2.98920042853993));
#171668=CARTESIAN_POINT('Ctrl Pts',(17.5459191088559,-20.7041962842724,
2.98882645005517));
#171669=CARTESIAN_POINT('Ctrl Pts',(17.5578167486092,-20.7122123616813,
2.98796559034042));
#171670=CARTESIAN_POINT('Ctrl Pts',(17.5645595852529,-20.7166993263948,
2.98747812393825));
#171671=CARTESIAN_POINT('Ctrl Pts',(17.5843393157514,-20.7296984352639,
2.98604928024905));
#171672=CARTESIAN_POINT('Ctrl Pts',(17.5974443550221,-20.7381054451487,
2.9851039976049));
#171673=CARTESIAN_POINT('Ctrl Pts',(17.7099515808651,-20.8085403365685,
2.97699895964382));
#171674=CARTESIAN_POINT('Ctrl Pts',(17.8142360536012,-20.8623516958022,
2.96953654984386));
#171675=CARTESIAN_POINT('Ctrl Pts',(18.0737247741335,-20.970059161614,2.95118250552068));
#171676=CARTESIAN_POINT('Ctrl Pts',(18.2318032766922,-21.0150862433738,
2.94014783735797));
#171677=CARTESIAN_POINT('Ctrl Pts',(18.4243168587293,-21.046459545984,2.92776874172154));
#171678=CARTESIAN_POINT('Ctrl Pts',(18.4552515476172,-21.05080060463,2.92581301379045));
#171679=CARTESIAN_POINT('Ctrl Pts',(18.4933740750363,-21.0552924885962,
2.9234529893992));
#171680=CARTESIAN_POINT('Ctrl Pts',(18.5004796703129,-21.0560932458748,
2.92301524173163));
#171681=CARTESIAN_POINT('Ctrl Pts',(18.5116558727195,-21.0572954228324,
2.9223302171848));
#171682=CARTESIAN_POINT('Ctrl Pts',(18.5157237422032,-21.0577210651632,
2.92208161212249));
#171683=CARTESIAN_POINT('Ctrl Pts',(18.5233493923546,-21.0584966416467,
2.92161697124014));
#171684=CARTESIAN_POINT('Ctrl Pts',(18.5269067848668,-21.0588493492011,
2.92140078730138));
#171685=CARTESIAN_POINT('Ctrl Pts',(18.5350553507079,-21.0596364233856,
2.92090688910949));
#171686=CARTESIAN_POINT('Ctrl Pts',(18.5396470532403,-21.0600647996853,
2.92062951419674));
#171687=CARTESIAN_POINT('Ctrl Pts',(18.5538555186243,-21.0613435399777,
2.9197740045458));
#171688=CARTESIAN_POINT('Ctrl Pts',(18.5634768814921,-21.0621431415533,
2.91919864615131));
#171689=CARTESIAN_POINT('Ctrl Pts',(18.679751574077,-21.071005894935,2.91228955166938));
#171690=CARTESIAN_POINT('Ctrl Pts',(18.7868778260515,-21.0710420222558,
2.90636861251406));
#171691=CARTESIAN_POINT('Ctrl Pts',(19.002296397891,-21.0547594131499,2.89457347805691));
#171692=CARTESIAN_POINT('Ctrl Pts',(19.1102328110118,-21.0381516511517,
2.88871625187452));
#171693=CARTESIAN_POINT('Ctrl Pts',(19.2773963386886,-20.9990301871559,
2.87922429213375));
#171694=CARTESIAN_POINT('Ctrl Pts',(19.3377161140119,-20.9820586529281,
2.87571161218853));
#171695=CARTESIAN_POINT('Ctrl Pts',(19.4208385937325,-20.9546387004679,
2.87069003399091));
#171696=CARTESIAN_POINT('Ctrl Pts',(19.4443451908838,-20.9464218849405,
2.8692493709782));
#171697=CARTESIAN_POINT('Ctrl Pts',(19.4852470126977,-20.9313096843253,
2.86670306722439));
#171698=CARTESIAN_POINT('Ctrl Pts',(19.5027061747419,-20.9245946578616,
2.86560335020493));
#171699=CARTESIAN_POINT('Ctrl Pts',(19.5279989910008,-20.9144799255535,
2.86399053128551));
#171700=CARTESIAN_POINT('Ctrl Pts',(19.5359049942336,-20.9112626758244,
2.86348357151803));
#171701=CARTESIAN_POINT('Ctrl Pts',(19.5497473798616,-20.9055318703265,
2.86259088837445));
#171702=CARTESIAN_POINT('Ctrl Pts',(19.5556921762052,-20.9030388315656,
2.86220586459655));
#171703=CARTESIAN_POINT('Ctrl Pts',(19.5672246053783,-20.8981404788841,
2.86145569956698));
#171704=CARTESIAN_POINT('Ctrl Pts',(19.5728134449076,-20.8957381536617,
2.86109066318479));
#171705=CARTESIAN_POINT('Ctrl Pts',(19.5861670492308,-20.8899298779716,
2.86021485588539));
#171706=CARTESIAN_POINT('Ctrl Pts',(19.5939218130015,-20.8865013217834,
2.8597033149281));
#171707=CARTESIAN_POINT('Ctrl Pts',(19.6219376442148,-20.8739131477901,
2.85784445759871));
#171708=CARTESIAN_POINT('Ctrl Pts',(19.6420741322782,-20.8644812989342,
2.85648781670395));
#171709=CARTESIAN_POINT('Ctrl Pts',(19.8277496371534,-20.7739181608982,
2.84378166931708));
#171710=CARTESIAN_POINT('Ctrl Pts',(19.9821459063725,-20.6718194051452,
2.83164504671176));
#171711=CARTESIAN_POINT('Ctrl Pts',(20.182499044718,-20.4979935084846,2.81413070795178));
#171712=CARTESIAN_POINT('Ctrl Pts',(20.2405697501656,-20.4414612253418,
2.80880858474812));
#171713=CARTESIAN_POINT('Ctrl Pts',(20.3197446190823,-20.355002902914,2.80133393154705));
#171714=CARTESIAN_POINT('Ctrl Pts',(20.3435381823394,-20.3276417944048,
2.79905603609559));
#171715=CARTESIAN_POINT('Ctrl Pts',(20.3713803464612,-20.2939130172494,
2.79636523895101));
#171716=CARTESIAN_POINT('Ctrl Pts',(20.3761113533266,-20.2881194751797,
2.79590709477342));
#171717=CARTESIAN_POINT('Ctrl Pts',(20.383427127724,-20.2790631011196,2.79519737228355));
#171718=CARTESIAN_POINT('Ctrl Pts',(20.3860330915894,-20.2758175814692,
2.7949443060006));
#171719=CARTESIAN_POINT('Ctrl Pts',(20.3908536521749,-20.2697775565185,
2.7944757383486));
#171720=CARTESIAN_POINT('Ctrl Pts',(20.3930707401206,-20.2669851682601,
2.79426006213776));
#171721=CARTESIAN_POINT('Ctrl Pts',(20.3980740509156,-20.2606507788525,
2.79377294296695));
#171722=CARTESIAN_POINT('Ctrl Pts',(20.4008560179591,-20.2571054839278,
2.7935018039628));
#171723=CARTESIAN_POINT('Ctrl Pts',(20.4092349650928,-20.2463569919747,
2.79268419818449));
#171724=CARTESIAN_POINT('Ctrl Pts',(20.4147968133262,-20.2391263690934,
2.79214016406456));
#171725=CARTESIAN_POINT('Ctrl Pts',(20.45741557681,-20.1829729355585,2.78795918091646));
#171726=CARTESIAN_POINT('Ctrl Pts',(20.4923796339441,-20.132490647179,2.78445672779228));
#171727=CARTESIAN_POINT('Ctrl Pts',(20.5373985768837,-20.0610421607798,
2.7797373938508));
#171728=CARTESIAN_POINT('Ctrl Pts',(20.5493742954183,-20.0413287633696,
2.7784590303652));
#171729=CARTESIAN_POINT('Ctrl Pts',(20.5786288223331,-19.991349696965,2.77526747690636));
#171730=CARTESIAN_POINT('Ctrl Pts',(20.59548704035,-19.9608455649869,2.77336403134532));
#171731=CARTESIAN_POINT('Ctrl Pts',(20.6620560799351,-19.8330369165261,
2.765518731364));
#171732=CARTESIAN_POINT('Ctrl Pts',(20.7049493611461,-19.7323742801806,
2.75963513570466));
#171733=CARTESIAN_POINT('Ctrl Pts',(20.7574649984156,-19.5767426096472,
2.75050124773808));
#171734=CARTESIAN_POINT('Ctrl Pts',(20.7730110518191,-19.5239678457783,
2.74739971936568));
#171735=CARTESIAN_POINT('Ctrl Pts',(20.7948769375166,-19.4374367387551,
2.74226473750703));
#171736=CARTESIAN_POINT('Ctrl Pts',(20.8024619860172,-19.4040258793036,
2.74027049059516));
#171737=CARTESIAN_POINT('Ctrl Pts',(20.81136813513,-19.3598570084272,2.73761311955608));
#171738=CARTESIAN_POINT('Ctrl Pts',(20.8134223670016,-19.3492509549918,
2.73697344986146));
#171739=CARTESIAN_POINT('Ctrl Pts',(20.8166548922365,-19.3318488741907,
2.73592115569512));
#171740=CARTESIAN_POINT('Ctrl Pts',(20.8178813256869,-19.325061906529,2.73551007013574));
#171741=CARTESIAN_POINT('Ctrl Pts',(20.820191767646,-19.3119091634109,2.73471204373013));
#171742=CARTESIAN_POINT('Ctrl Pts',(20.8212798594306,-19.3055441758585,
2.73432523772691));
#171743=CARTESIAN_POINT('Ctrl Pts',(20.8237258358166,-19.2908310290024,
2.73342963665734));
#171744=CARTESIAN_POINT('Ctrl Pts',(20.8250628390276,-19.2824795532087,
2.73292018443606));
#171745=CARTESIAN_POINT('Ctrl Pts',(20.8285257277111,-19.2599861791992,
2.73154502349755));
#171746=CARTESIAN_POINT('Ctrl Pts',(20.8305583919263,-19.245830570418,2.73067638105955));
#171747=CARTESIAN_POINT('Ctrl Pts',(20.8479958613787,-19.1149853545658,
2.72261623137109));
#171748=CARTESIAN_POINT('Ctrl Pts',(20.8537848986482,-18.9972409174073,
2.71511830076217));
#171749=CARTESIAN_POINT('Ctrl Pts',(20.8441721744735,-18.7161641160448,
2.69674208479173));
#171750=CARTESIAN_POINT('Ctrl Pts',(20.8196541810789,-18.5538892504222,
2.68572495911518));
#171751=CARTESIAN_POINT('Ctrl Pts',(20.7685610741576,-18.3661584555948,
2.67338014168731));
#171752=CARTESIAN_POINT('Ctrl Pts',(20.7597681652363,-18.3364411847877,
2.67144021072281));
#171753=CARTESIAN_POINT('Ctrl Pts',(20.7481520750229,-18.3001324569244,
2.66909654633523));
#171754=CARTESIAN_POINT('Ctrl Pts',(20.7459443127011,-18.2933498948886,
2.6686598971194));
#171755=CARTESIAN_POINT('Ctrl Pts',(20.7424179167721,-18.2826994935451,
2.66797620444898));
#171756=CARTESIAN_POINT('Ctrl Pts',(20.7411223163095,-18.2788241653349,
2.66772784120054));
#171757=CARTESIAN_POINT('Ctrl Pts',(20.7386719872702,-18.2715648393806,
2.66726340508465));
#171758=CARTESIAN_POINT('Ctrl Pts',(20.7375199194272,-18.268180055116,2.66704718556748));
#171759=CARTESIAN_POINT('Ctrl Pts',(20.7348602790374,-18.2604304319294,
2.66655288313381));
#171760=CARTESIAN_POINT('Ctrl Pts',(20.7333469993902,-18.2560676033788,
2.66627514163402));
#171761=CARTESIAN_POINT('Ctrl Pts',(20.7286153688591,-18.2425689962341,
2.66541737359719));
#171762=CARTESIAN_POINT('Ctrl Pts',(20.7253485336115,-18.2334501795088,
2.66484014460777));
#171763=CARTESIAN_POINT('Ctrl Pts',(20.6858951203199,-18.1256585722324,
2.65803970026558));
#171764=CARTESIAN_POINT('Ctrl Pts',(20.6424663477042,-18.0297760990913,
2.65221478087934));
#171765=CARTESIAN_POINT('Ctrl Pts',(20.5855435632494,-17.9255196352191,
2.64572572656275));
#171766=CARTESIAN_POINT('Ctrl Pts',(20.5788832193334,-17.9135966983824,
2.64498128901625));
#171767=CARTESIAN_POINT('Ctrl Pts',(20.5179603780658,-17.8069729576078,
2.63829625911225));
#171768=CARTESIAN_POINT('Ctrl Pts',(20.4565657209145,-17.7165373384018,
2.63241820522035));
#171769=CARTESIAN_POINT('Ctrl Pts',(20.3414486534027,-17.5723335540748,
2.62215631898869));
#171770=CARTESIAN_POINT('Ctrl Pts',(20.2913141260961,-17.5159841003951,
2.61788266432365));
#171771=CARTESIAN_POINT('Ctrl Pts',(20.2250197954931,-17.4490347937054,
2.6123815893783));
#171772=CARTESIAN_POINT('Ctrl Pts',(20.2115762521096,-17.4358163610347,
2.61127332060569));
#171773=CARTESIAN_POINT('Ctrl Pts',(20.1917729641286,-17.4168582132912,
2.60965024706848));
#171774=CARTESIAN_POINT('Ctrl Pts',(20.1855518603284,-17.4109745252804,
2.60914169682538));
#171775=CARTESIAN_POINT('Ctrl Pts',(20.1745819219193,-17.4007249320977,
2.60824717684863));
#171776=CARTESIAN_POINT('Ctrl Pts',(20.1698484793457,-17.3963426620894,
2.60786191582327));
#171777=CARTESIAN_POINT('Ctrl Pts',(20.1606182665033,-17.3878752510172,
2.60711200543058));
#171778=CARTESIAN_POINT('Ctrl Pts',(20.1561237897811,-17.3837876948438,
2.60674746430017));
#171779=CARTESIAN_POINT('Ctrl Pts',(20.1453372274603,-17.3740622298702,
2.60587400540248));
#171780=CARTESIAN_POINT('Ctrl Pts',(20.1390289012606,-17.3684425620132,
2.60536432684467));
#171781=CARTESIAN_POINT('Ctrl Pts',(20.1161426816158,-17.3482991640617,
2.60351923789597));
#171782=CARTESIAN_POINT('Ctrl Pts',(20.0993723088522,-17.3339971680744,
2.60217468194046));
#171783=CARTESIAN_POINT('Ctrl Pts',(19.9387526562964,-17.201294121327,2.58936258085404));
#171784=CARTESIAN_POINT('Ctrl Pts',(19.7801118280689,-17.1021291511251,
2.57708863402808));
#171785=CARTESIAN_POINT('Ctrl Pts',(19.538064799707,-16.9920209717671,2.55953366432519));
#171786=CARTESIAN_POINT('Ctrl Pts',(19.46372609483,-16.9631461789141,2.55429956198979));
#171787=CARTESIAN_POINT('Ctrl Pts',(19.3537842034838,-16.9274394014562,
2.54693163888659));
#171788=CARTESIAN_POINT('Ctrl Pts',(19.319357300205,-16.9172186206141,2.54467610132618));
#171789=CARTESIAN_POINT('Ctrl Pts',(19.2774829604783,-16.9059377080309,
2.54200809273293));
#171790=CARTESIAN_POINT('Ctrl Pts',(19.2702707811739,-16.904035575501,2.5415512507225));
#171791=CARTESIAN_POINT('Ctrl Pts',(19.2590228645242,-16.901132554835,2.54084310303985));
#171792=CARTESIAN_POINT('Ctrl Pts',(19.2549940595747,-16.9001053934266,
2.54059031982601));
#171793=CARTESIAN_POINT('Ctrl Pts',(19.2475041557527,-16.8982192915258,
2.54012200912461));
#171794=CARTESIAN_POINT('Ctrl Pts',(19.2440439456601,-16.89735723537,2.53990630847174));
#171795=CARTESIAN_POINT('Ctrl Pts',(19.2361999560249,-16.8954240670267,
2.53941879458008));
#171796=CARTESIAN_POINT('Ctrl Pts',(19.2318149312573,-16.8943582286996,
2.53914728739158));
#171797=CARTESIAN_POINT('Ctrl Pts',(19.2204802964674,-16.8916415500104,
2.53844805517652));
#171798=CARTESIAN_POINT('Ctrl Pts',(19.2135256145716,-16.8900118308931,
2.53802151593928));
#171799=CARTESIAN_POINT('Ctrl Pts',(19.1706862598238,-16.8802015714935,
2.53540870784108));
#171800=CARTESIAN_POINT('Ctrl Pts',(19.1345991930462,-16.8729222544657,
2.53327055520097));
#171801=CARTESIAN_POINT('Ctrl Pts',(18.9307442695811,-16.8373071686671,
2.5214508932242));
#171802=CARTESIAN_POINT('Ctrl Pts',(18.7602171151967,-16.8283336627272,
2.51249780650082));
#171803=CARTESIAN_POINT('Ctrl Pts',(18.4950785314615,-16.8463548335748,
2.49788073300969));
#171804=CARTESIAN_POINT('Ctrl Pts',(18.4002748024625,-16.8592865843129,
2.49252205204228));
#171805=CARTESIAN_POINT('Ctrl Pts',(18.2857022869779,-16.8828995382233,
2.48571044764722));
#171806=CARTESIAN_POINT('Ctrl Pts',(18.264796443625,-16.887539892951,2.48445395202637));
#171807=CARTESIAN_POINT('Ctrl Pts',(18.2351963409351,-16.8945828923915,
2.48265413975129));
#171808=CARTESIAN_POINT('Ctrl Pts',(18.2264410654274,-16.8967252813588,
2.48211918534306));
#171809=CARTESIAN_POINT('Ctrl Pts',(18.2113698161335,-16.9005153439258,
2.48119373180126));
#171810=CARTESIAN_POINT('Ctrl Pts',(18.2050472433013,-16.9021364477347,
2.48080409521172));
#171811=CARTESIAN_POINT('Ctrl Pts',(18.1929620546896,-16.905294717921,2.48005661293148));
#171812=CARTESIAN_POINT('Ctrl Pts',(18.1871982315017,-16.9068270501516,
2.47969892721987));
#171813=CARTESIAN_POINT('Ctrl Pts',(18.1722406854964,-16.910871315506,2.47876758241382));
#171814=CARTESIAN_POINT('Ctrl Pts',(18.1630573890821,-16.9134209938077,
2.47819270160492));
#171815=CARTESIAN_POINT('Ctrl Pts',(18.1318711139857,-16.9223069000896,
2.47622976533447));
#171816=CARTESIAN_POINT('Ctrl Pts',(18.1099544456703,-16.9289378762109,
2.47483215058254));
#171817=CARTESIAN_POINT('Ctrl Pts',(17.9197966134086,-16.9898548796847,
2.4625428166505));
#171818=CARTESIAN_POINT('Ctrl Pts',(17.7588914191062,-17.064652670673,2.45093563248813));
#171819=CARTESIAN_POINT('Ctrl Pts',(17.5362353967373,-17.2042975253663,
2.43357171418553));
#171820=CARTESIAN_POINT('Ctrl Pts',(17.4661401486803,-17.2544614067884,
2.42789875448704));
#171821=CARTESIAN_POINT('Ctrl Pts',(17.3701109788857,-17.3324602412783,
2.42000164294333));
#171822=CARTESIAN_POINT('Ctrl Pts',(17.3415646015901,-17.3569368801045,
2.41763725416295));
#171823=CARTESIAN_POINT('Ctrl Pts',(17.3080783863316,-17.3872336646701,
2.41485851446678));
#171824=CARTESIAN_POINT('Ctrl Pts',(17.3025004899274,-17.3923348791717,
2.41439547564632));
#171825=CARTESIAN_POINT('Ctrl Pts',(17.2938809665726,-17.4003029815971,
2.41367983629214));
#171826=CARTESIAN_POINT('Ctrl Pts',(17.2908203712559,-17.4031491268571,
2.41342570830669));
#171827=CARTESIAN_POINT('Ctrl Pts',(17.2851655106111,-17.408439076604,2.41295616843403));
#171828=CARTESIAN_POINT('Ctrl Pts',(17.282569010505,-17.4108803469855,2.41274057543805));
#171829=CARTESIAN_POINT('Ctrl Pts',(17.276719833283,-17.4164077302856,2.41225489818765));
#171830=CARTESIAN_POINT('Ctrl Pts',(17.2734707971798,-17.4194976177268,
2.41198511019559));
#171831=CARTESIAN_POINT('Ctrl Pts',(17.2639302636739,-17.4286287227468,
2.41119278340234));
#171832=CARTESIAN_POINT('Ctrl Pts',(17.2576661687805,-17.4346986117645,
2.4106724103148));
#171833=CARTESIAN_POINT('Ctrl Pts',(17.2133345236271,-17.4781903077165,
2.40698703341621));
#171834=CARTESIAN_POINT('Ctrl Pts',(17.17665347041,-17.5170047706333,2.40392354355281));
#171835=CARTESIAN_POINT('Ctrl Pts',(17.1324647402756,-17.5674564393888,
2.40015193226831));
#171836=CARTESIAN_POINT('Ctrl Pts',(17.1235531461743,-17.5778322511852,
2.39938689918319));
#171837=CARTESIAN_POINT('Ctrl Pts',(17.0811122472264,-17.6282263481393,
2.39571809797011));
#171838=CARTESIAN_POINT('Ctrl Pts',(17.04896934407,-17.6693906766026,2.3928615223131));
#171839=CARTESIAN_POINT('Ctrl Pts',(16.9542698348109,-17.8003821168439,
2.38406088976791));
#171840=CARTESIAN_POINT('Ctrl Pts',(16.8971323202139,-17.893898179805,2.37816903274667));
#171841=CARTESIAN_POINT('Ctrl Pts',(16.8130787851647,-18.0589719260448,
2.36786971883574));
#171842=CARTESIAN_POINT('Ctrl Pts',(16.7823335504142,-18.1283290864511,
2.36357208491561));
#171843=CARTESIAN_POINT('Ctrl Pts',(16.751997197966,-18.2080617122727,2.3585915450917));
#171844=CARTESIAN_POINT('Ctrl Pts',(16.7486782220989,-18.2169648219953,
2.35803490618603));
#171845=CARTESIAN_POINT('Ctrl Pts',(16.7454193691877,-18.2258897640453,
2.35747631421306));
#171846=CARTESIAN_POINT('',(16.618038032075,-18.9501158127103,2.8890562790225));
#171847=CARTESIAN_POINT('Ctrl Pts',(16.618038032075,-18.9501158127103,2.8890562790225));
#171848=CARTESIAN_POINT('Ctrl Pts',(16.6223668846964,-19.4559949565256,
2.85866010167885));
#171849=CARTESIAN_POINT('Ctrl Pts',(17.0578065183866,-20.6740880083468,
2.78587198877473));
#171850=CARTESIAN_POINT('Ctrl Pts',(19.0938031538723,-21.4292709570805,
2.67069194031012));
#171851=CARTESIAN_POINT('Ctrl Pts',(21.0117474660562,-19.9903622879567,
2.54351613362868));
#171852=CARTESIAN_POINT('Ctrl Pts',(20.8399998530167,-17.5988206232279,
2.41634032694726));
#171853=CARTESIAN_POINT('Ctrl Pts',(18.7361280842055,-16.4487371345171,
2.28916452026581));
#171854=CARTESIAN_POINT('Ctrl Pts',(17.1750895514748,-17.2986361860363,
2.19488963270647));
#171855=CARTESIAN_POINT('Ctrl Pts',(16.7978195835484,-18.0771168317319,
2.1430066807076));
#171856=CARTESIAN_POINT('Ctrl Pts',(16.7452305870807,-18.2258208582162,
2.13351566426921));
#171857=CARTESIAN_POINT('Ctrl Pts',(16.617000874474,-18.950075806071,2.88845972223463));
#171858=CARTESIAN_POINT('Ctrl Pts',(16.6171407059199,-18.7962331792496,
2.8985386370441));
#171859=CARTESIAN_POINT('Ctrl Pts',(16.6340491292001,-18.6428594303531,
2.90887454244536));
#171860=CARTESIAN_POINT('Ctrl Pts',(16.6744827097124,-18.4609467005497,
2.92071560516971));
#171861=CARTESIAN_POINT('Ctrl Pts',(16.6822627059619,-18.4293919667833,
2.92275211774186));
#171862=CARTESIAN_POINT('Ctrl Pts',(16.6926607588507,-18.3910405538783,
2.92519558983202));
#171863=CARTESIAN_POINT('Ctrl Pts',(16.6945908013807,-18.3840638048843,
2.92563880153013));
#171864=CARTESIAN_POINT('Ctrl Pts',(16.697672606106,-18.3731419582713,2.92633044865512));
#171865=CARTESIAN_POINT('Ctrl Pts',(16.6988001139795,-18.3691901577678,
2.92658025432378));
#171866=CARTESIAN_POINT('Ctrl Pts',(16.7009291430241,-18.361809650113,2.92704592485674));
#171867=CARTESIAN_POINT('Ctrl Pts',(16.7019278235753,-18.358380232291,2.92726194509871));
#171868=CARTESIAN_POINT('Ctrl Pts',(16.7042273459033,-18.3505575968172,
2.92775389547489));
#171869=CARTESIAN_POINT('Ctrl Pts',(16.7055337702709,-18.3461660727402,
2.92802949632064));
#171870=CARTESIAN_POINT('Ctrl Pts',(16.7095931435689,-18.3326808968913,
2.92887412508428));
#171871=CARTESIAN_POINT('Ctrl Pts',(16.7123931058315,-18.3236013646558,
2.92944047766867));
#171872=CARTESIAN_POINT('Ctrl Pts',(16.7246572679426,-18.284762445607,2.93185432508154));
#171873=CARTESIAN_POINT('Ctrl Pts',(16.7347152088544,-18.2552049884584,
2.93366911664583));
#171874=CARTESIAN_POINT('Ctrl Pts',(16.7454193844899,-18.2258897221376,
2.93545674301194));
#171875=CARTESIAN_POINT('Origin',(18.734,-18.952,0.));
#171876=CARTESIAN_POINT('',(16.7454192997072,-18.22588995433,3.95421655704364));
#171877=CARTESIAN_POINT('',(16.7454193692324,-18.225889763923,3.73234496387082));
#171878=CARTESIAN_POINT('',(16.7454193692319,-18.2258897639242,0.));
#171879=CARTESIAN_POINT('Ctrl Pts',(16.7454192997072,-18.22588995433,3.95421655704364));
#171880=CARTESIAN_POINT('Ctrl Pts',(16.7247484957261,-18.2825006046045,
3.95029630227183));
#171881=CARTESIAN_POINT('Ctrl Pts',(16.7064930198954,-18.3399995059724,
3.94643457592769));
#171882=CARTESIAN_POINT('Ctrl Pts',(16.6875909790288,-18.4097441828717,
3.94195339820002));
#171883=CARTESIAN_POINT('Ctrl Pts',(16.6845683665288,-18.4212823282768,
3.94121862404921));
#171884=CARTESIAN_POINT('Ctrl Pts',(16.6804108712761,-18.4377180258621,
3.94018187945989));
#171885=CARTESIAN_POINT('Ctrl Pts',(16.6791957315543,-18.4425947800532,
3.93987549555571));
#171886=CARTESIAN_POINT('Ctrl Pts',(16.6771318961882,-18.451005180075,3.93934929254021));
#171887=CARTESIAN_POINT('Ctrl Pts',(16.6762749150324,-18.4545367535743,
3.93912899956492));
#171888=CARTESIAN_POINT('Ctrl Pts',(16.6746311950524,-18.4613873629827,
3.93870297479797));
#171889=CARTESIAN_POINT('Ctrl Pts',(16.6738433838323,-18.4647060931702,
3.9384971791502));
#171890=CARTESIAN_POINT('Ctrl Pts',(16.6717400398738,-18.4736629064988,
3.93794331645963));
#171891=CARTESIAN_POINT('Ctrl Pts',(16.6704395973768,-18.4793045539916,
3.93759611096546));
#171892=CARTESIAN_POINT('Ctrl Pts',(16.6657019231395,-18.5002499787928,
3.9363129626332));
#171893=CARTESIAN_POINT('Ctrl Pts',(16.6624115605977,-18.5155869082596,
3.93538506602472));
#171894=CARTESIAN_POINT('Ctrl Pts',(16.632554547465,-18.6627095418791,3.92658315316966));
#171895=CARTESIAN_POINT('Ctrl Pts',(16.6184239853392,-18.7967259490059,
3.91931202279268));
#171896=CARTESIAN_POINT('Ctrl Pts',(16.6170404625804,-18.9374793398567,
3.91166809579151));
#171897=CARTESIAN_POINT('Ctrl Pts',(16.6170066729722,-18.94376677829,3.91132666064666));
#171898=CARTESIAN_POINT('Ctrl Pts',(16.6168668544331,-19.0958927648747,
3.90306443006442));
#171899=CARTESIAN_POINT('Ctrl Pts',(16.6318021047659,-19.2413359707292,
3.89510371418586));
#171900=CARTESIAN_POINT('Ctrl Pts',(16.6664676942097,-19.4076057064771,
3.88524445554732));
#171901=CARTESIAN_POINT('Ctrl Pts',(16.6717720440742,-19.4310429873341,
3.88383767302017));
#171902=CARTESIAN_POINT('Ctrl Pts',(16.6797804435962,-19.4638256282852,
3.88184394360458));
#171903=CARTESIAN_POINT('Ctrl Pts',(16.6821518237267,-19.4732509150305,
3.88126769147224));
#171904=CARTESIAN_POINT('Ctrl Pts',(16.6860916184719,-19.4884664418707,
3.88033238345868));
#171905=CARTESIAN_POINT('Ctrl Pts',(16.6876199075509,-19.4942669992487,
3.87997462882876));
#171906=CARTESIAN_POINT('Ctrl Pts',(16.690855325819,-19.5063384146194,3.87922759582056));
#171907=CARTESIAN_POINT('Ctrl Pts',(16.6925667182077,-19.5126080556736,
3.87883818238362));
#171908=CARTESIAN_POINT('Ctrl Pts',(16.696678362728,-19.5274024490659,3.87791588445684));
#171909=CARTESIAN_POINT('Ctrl Pts',(16.6991032784907,-19.5359201667639,
3.87738220201063));
#171910=CARTESIAN_POINT('Ctrl Pts',(16.7073169381373,-19.5640987025324,
3.87560762706832));
#171911=CARTESIAN_POINT('Ctrl Pts',(16.7133376061603,-19.5836901919816,
3.87435919381296));
#171912=CARTESIAN_POINT('Ctrl Pts',(16.7467230010809,-19.6869627894031,
3.86769849643721));
#171913=CARTESIAN_POINT('Ctrl Pts',(16.779000315155,-19.7689534976003,3.86212557703156));
#171914=CARTESIAN_POINT('Ctrl Pts',(16.8711049179755,-19.965934299276,3.84804780837658));
#171915=CARTESIAN_POINT('Ctrl Pts',(16.9365619694566,-20.077901295827,3.8394138807018));
#171916=CARTESIAN_POINT('Ctrl Pts',(17.0275742721489,-20.2052093000958,
3.82914899890504));
#171917=CARTESIAN_POINT('Ctrl Pts',(17.0437446644012,-20.2269350140777,
3.82738096877477));
#171918=CARTESIAN_POINT('Ctrl Pts',(17.0955034772297,-20.2937592648694,
3.82190413977418));
#171919=CARTESIAN_POINT('Ctrl Pts',(17.1325165343988,-20.3377275162307,
3.81824355734129));
#171920=CARTESIAN_POINT('Ctrl Pts',(17.177263699391,-20.3866915617919,3.81415056233225));
#171921=CARTESIAN_POINT('Ctrl Pts',(17.1832929079751,-20.3932061990514,
3.81360565013237));
#171922=CARTESIAN_POINT('Ctrl Pts',(17.1924516927485,-20.4029783653255,
3.81278801143652));
#171923=CARTESIAN_POINT('Ctrl Pts',(17.1955509247917,-20.4062640214547,
3.81251305647396));
#171924=CARTESIAN_POINT('Ctrl Pts',(17.2011160478794,-20.412126195834,3.81202245328679));
#171925=CARTESIAN_POINT('Ctrl Pts',(17.2035779471775,-20.4147064159544,
3.81180650539683));
#171926=CARTESIAN_POINT('Ctrl Pts',(17.2089220783741,-20.4202791268719,
3.81134008865029));
#171927=CARTESIAN_POINT('Ctrl Pts',(17.2118065936837,-20.4232693485176,
3.81108980172376));
#171928=CARTESIAN_POINT('Ctrl Pts',(17.219884606349,-20.4315942026561,3.81039288602945));
#171929=CARTESIAN_POINT('Ctrl Pts',(17.2250975285736,-20.4369100192551,
3.80994774472222));
#171930=CARTESIAN_POINT('Ctrl Pts',(17.2554562683131,-20.4675430353591,
3.80738102866061));
#171931=CARTESIAN_POINT('Ctrl Pts',(17.281212535892,-20.4922503634395,3.80530467626046));
#171932=CARTESIAN_POINT('Ctrl Pts',(17.3658586632785,-20.5694356715784,
3.79874973221874));
#171933=CARTESIAN_POINT('Ctrl Pts',(17.4270632496412,-20.6192813612031,
3.79440821669894));
#171934=CARTESIAN_POINT('Ctrl Pts',(17.5646408986174,-20.7190837759748,
3.78513876655965));
#171935=CARTESIAN_POINT('Ctrl Pts',(17.641744789346,-20.7677544465143,3.78023182358685));
#171936=CARTESIAN_POINT('Ctrl Pts',(17.8150630554438,-20.86211352856,3.76938613693422));
#171937=CARTESIAN_POINT('Ctrl Pts',(17.9120634607094,-20.9058154646793,
3.76342351390248));
#171938=CARTESIAN_POINT('Ctrl Pts',(18.0251856585078,-20.9468609432434,
3.75637196410921));
#171939=CARTESIAN_POINT('Ctrl Pts',(18.038492413508,-20.951539231015,3.7555411909062));
#171940=CARTESIAN_POINT('Ctrl Pts',(18.0597976158504,-20.9587911506411,
3.75420858579345));
#171941=CARTESIAN_POINT('Ctrl Pts',(18.0677664960331,-20.9614507936679,
3.75370959922164));
#171942=CARTESIAN_POINT('Ctrl Pts',(18.0818794258604,-20.9660678576787,
3.75282484182403));
#171943=CARTESIAN_POINT('Ctrl Pts',(18.0880170176879,-20.9680447821648,
3.75243971942586));
#171944=CARTESIAN_POINT('Ctrl Pts',(18.1007603097913,-20.9720852426614,
3.75163933827889));
#171945=CARTESIAN_POINT('Ctrl Pts',(18.1073672806373,-20.9741444869565,
3.75122394384581));
#171946=CARTESIAN_POINT('Ctrl Pts',(18.1244160986399,-20.9793666423947,
3.75015090195569));
#171947=CARTESIAN_POINT('Ctrl Pts',(18.1348724171269,-20.9824812651078,
3.74949168306891));
#171948=CARTESIAN_POINT('Ctrl Pts',(18.179165365773,-20.9953028811977,3.74669426657776));
#171949=CARTESIAN_POINT('Ctrl Pts',(18.2132156897672,-21.0042455029274,
3.74453140916394));
#171950=CARTESIAN_POINT('Ctrl Pts',(18.3030452731752,-21.0254579030511,
3.73878992001805));
#171951=CARTESIAN_POINT('Ctrl Pts',(18.359122873625,-21.0363262425726,3.73516960252828));
#171952=CARTESIAN_POINT('Ctrl Pts',(18.5659612572872,-21.067796271307,3.72170022785271));
#171953=CARTESIAN_POINT('Ctrl Pts',(18.7183789724776,-21.0743996040648,
3.71151257409928));
#171954=CARTESIAN_POINT('Ctrl Pts',(18.8926143489366,-21.0631694621775,
3.70010873248781));
#171955=CARTESIAN_POINT('Ctrl Pts',(18.915038513217,-21.0613648609432,3.69864662224109));
#171956=CARTESIAN_POINT('Ctrl Pts',(18.9885573577788,-21.0542673241109,
3.6938793084805));
#171957=CARTESIAN_POINT('Ctrl Pts',(19.0394927019095,-21.0474719031565,
3.6906179728685));
#171958=CARTESIAN_POINT('Ctrl Pts',(19.0978982595057,-21.0375045163014,
3.68696358198722));
#171959=CARTESIAN_POINT('Ctrl Pts',(19.1056546613206,-21.0361362354488,
3.6864800244708));
#171960=CARTESIAN_POINT('Ctrl Pts',(19.1180095511047,-21.0338855841562,
3.68571277998383));
#171961=CARTESIAN_POINT('Ctrl Pts',(19.1226129739211,-21.0330312055151,
3.6854275700628));
#171962=CARTESIAN_POINT('Ctrl Pts',(19.1307440240269,-21.0314941906244,
3.68492502409105));
#171963=CARTESIAN_POINT('Ctrl Pts',(19.134272795892,-21.0308178369106,3.68470733437687));
#171964=CARTESIAN_POINT('Ctrl Pts',(19.1417296701644,-21.0293688989211,
3.68424819967114));
#171965=CARTESIAN_POINT('Ctrl Pts',(19.1456573008308,-21.0285941571289,
3.68400687929838));
#171966=CARTESIAN_POINT('Ctrl Pts',(19.1562102240672,-21.0264814317415,
3.68335980871724));
#171967=CARTESIAN_POINT('Ctrl Pts',(19.162831410307,-21.0251228396548,3.68295521881514));
#171968=CARTESIAN_POINT('Ctrl Pts',(19.1951348592948,-21.0183331552229,
3.6809876451806));
#171969=CARTESIAN_POINT('Ctrl Pts',(19.2207223335718,-21.0124561581417,
3.67944873086008));
#171970=CARTESIAN_POINT('Ctrl Pts',(19.2937036806347,-20.9942581091047,
3.6750985937067));
#171971=CARTESIAN_POINT('Ctrl Pts',(19.3407901344176,-20.9807663142388,
3.67233961646863));
#171972=CARTESIAN_POINT('Ctrl Pts',(19.4792756662508,-20.9358319654717,
3.66425591350563));
#171973=CARTESIAN_POINT('Ctrl Pts',(19.5690360765545,-20.8997528818413,
3.65905285182928));
#171974=CARTESIAN_POINT('Ctrl Pts',(19.7829857781843,-20.7962373969938,
3.64611983252081));
#171975=CARTESIAN_POINT('Ctrl Pts',(19.9034758404611,-20.7222828772199,
3.63834011682043));
#171976=CARTESIAN_POINT('Ctrl Pts',(20.0270790917159,-20.6282575770136,
3.62924195725224));
#171977=CARTESIAN_POINT('Ctrl Pts',(20.0383587492272,-20.6194954993507,
3.62840085445846));
#171978=CARTESIAN_POINT('Ctrl Pts',(20.0561711612286,-20.6053674329431,
3.62705480177545));
#171979=CARTESIAN_POINT('Ctrl Pts',(20.0627620503884,-20.6000751979773,
3.62655278944008));
#171980=CARTESIAN_POINT('Ctrl Pts',(20.0743310926665,-20.5906711837373,
3.62566451474313));
#171981=CARTESIAN_POINT('Ctrl Pts',(20.0793224881636,-20.5865758128014,
3.6252789177452));
#171982=CARTESIAN_POINT('Ctrl Pts',(20.089608460664,-20.5780572860882,3.62447936951975));
#171983=CARTESIAN_POINT('Ctrl Pts',(20.0949003005306,-20.5736309587965,
3.62406529158296));
#171984=CARTESIAN_POINT('Ctrl Pts',(20.1084301930492,-20.5622010926669,
3.62299949835742));
#171985=CARTESIAN_POINT('Ctrl Pts',(20.1166363212192,-20.5551602261918,
3.62234625199899));
#171986=CARTESIAN_POINT('Ctrl Pts',(20.1506782839383,-20.5254964001308,
3.61960737641389));
#171987=CARTESIAN_POINT('Ctrl Pts',(20.1760144769206,-20.5023103924026,
3.61749835576717));
#171988=CARTESIAN_POINT('Ctrl Pts',(20.2405660387311,-20.440285253731,3.61193376400569));
#171989=CARTESIAN_POINT('Ctrl Pts',(20.2788444740461,-20.4005126690312,
3.60843963293878));
#171990=CARTESIAN_POINT('Ctrl Pts',(20.388288080156,-20.2775193627391,3.59785656492648));
#171991=CARTESIAN_POINT('Ctrl Pts',(20.4545961724365,-20.1902309883408,
3.59061928252106));
#171992=CARTESIAN_POINT('Ctrl Pts',(20.5427363516408,-20.0533662161876,
3.57986596111988));
#171993=CARTESIAN_POINT('Ctrl Pts',(20.5699147097805,-20.0074393632676,
3.57634996540707));
#171994=CARTESIAN_POINT('Ctrl Pts',(20.6013704200902,-19.9493853261275,
3.57205283183505));
#171995=CARTESIAN_POINT('Ctrl Pts',(20.6073108039685,-19.9381827496778,
3.57123023453653));
#171996=CARTESIAN_POINT('Ctrl Pts',(20.6376760878161,-19.8796543547082,
3.56696904540654));
#171997=CARTESIAN_POINT('Ctrl Pts',(20.6604116623662,-19.8314682417883,
3.56358373409534));
#171998=CARTESIAN_POINT('Ctrl Pts',(20.6847259255766,-19.7744556574431,
3.55976032947201));
#171999=CARTESIAN_POINT('Ctrl Pts',(20.6880951091711,-19.7664183540963,
3.55922545513258));
#172000=CARTESIAN_POINT('Ctrl Pts',(20.6931218175638,-19.7542161755697,
3.55841989885514));
#172001=CARTESIAN_POINT('Ctrl Pts',(20.6948158573049,-19.7500665780477,
3.55814708319013));
#172002=CARTESIAN_POINT('Ctrl Pts',(20.6978332232313,-19.7426078498529,
3.55765877552597));
#172003=CARTESIAN_POINT('Ctrl Pts',(20.6991613773727,-19.7393007445581,
3.55744299578883));
#172004=CARTESIAN_POINT('Ctrl Pts',(20.7020294311448,-19.7321068106624,
3.55697519917203));
#172005=CARTESIAN_POINT('Ctrl Pts',(20.7035661655875,-19.7282187822778,
3.55672337361937));
#172006=CARTESIAN_POINT('Ctrl Pts',(20.7078510426248,-19.7172831383104,
3.556017814126));
#172007=CARTESIAN_POINT('Ctrl Pts',(20.710572975948,-19.7102252270398,3.5555656280204));
#172008=CARTESIAN_POINT('Ctrl Pts',(20.7266319304302,-19.6679105329622,
3.55287276722474));
#172009=CARTESIAN_POINT('Ctrl Pts',(20.7390640788338,-19.6323148805782,
3.55068267056642));
#172010=CARTESIAN_POINT('Ctrl Pts',(20.7768715595335,-19.5140035235451,
3.54359032882097));
#172011=CARTESIAN_POINT('Ctrl Pts',(20.7981301497969,-19.4300598925435,
3.53885232704573));
#172012=CARTESIAN_POINT('Ctrl Pts',(20.8469054621098,-19.1719163043558,
3.52455637502355));
#172013=CARTESIAN_POINT('Ctrl Pts',(20.8578743442905,-18.9954024848503,
3.51508742487422));
#172014=CARTESIAN_POINT('Ctrl Pts',(20.8454190730435,-18.7966784798802,
3.50351662147154));
#172015=CARTESIAN_POINT('Ctrl Pts',(20.8436120272572,-18.7738082197345,
3.50217258131649));
#172016=CARTESIAN_POINT('Ctrl Pts',(20.8405280284339,-18.7414777056704,
3.50025325244852));
#172017=CARTESIAN_POINT('Ctrl Pts',(20.8395581804588,-18.7319892839764,
3.49968760404709));
#172018=CARTESIAN_POINT('Ctrl Pts',(20.8378775880425,-18.716577656134,3.49876488897144));
#172019=CARTESIAN_POINT('Ctrl Pts',(20.8372058598235,-18.7106502630181,
3.49840905502558));
#172020=CARTESIAN_POINT('Ctrl Pts',(20.8357468337911,-18.6982445371956,
3.49766228331828));
#172021=CARTESIAN_POINT('Ctrl Pts',(20.8349546158209,-18.6917668563875,
3.49727119388797));
#172022=CARTESIAN_POINT('Ctrl Pts',(20.8329976936481,-18.6763574529723,
3.49633804291479));
#172023=CARTESIAN_POINT('Ctrl Pts',(20.8318059189893,-18.6674293514684,
3.49579513140122));
#172024=CARTESIAN_POINT('Ctrl Pts',(20.8275936394899,-18.6373388477539,
3.49395760483708));
#172025=CARTESIAN_POINT('Ctrl Pts',(20.8243096625917,-18.6162152029563,
3.49265469530736));
#172026=CARTESIAN_POINT('Ctrl Pts',(20.8046466900077,-18.5012359833599,
3.48548961692087));
#172027=CARTESIAN_POINT('Ctrl Pts',(20.7822681291721,-18.4085302677464,
3.47943826093059));
#172028=CARTESIAN_POINT('Ctrl Pts',(20.7026061183242,-18.1548893669231,
3.46216230876742));
#172029=CARTESIAN_POINT('Ctrl Pts',(20.6320015056481,-17.9989089470511,
3.4506509601528));
#172030=CARTESIAN_POINT('Ctrl Pts',(20.5243810106594,-17.8217018303696,
3.43741904338694));
#172031=CARTESIAN_POINT('Ctrl Pts',(20.5044996556448,-17.7908068806401,
3.43510868194865));
#172032=CARTESIAN_POINT('Ctrl Pts',(20.4798052598489,-17.754542714772,3.43240694704327));
#172033=CARTESIAN_POINT('Ctrl Pts',(20.4757575757676,-17.7486627630497,
3.43196921080564));
#172034=CARTESIAN_POINT('Ctrl Pts',(20.4691034195864,-17.7391003856303,
3.43125802286862));
#172035=CARTESIAN_POINT('Ctrl Pts',(20.4665148194733,-17.7354056746906,
3.43098340320532));
#172036=CARTESIAN_POINT('Ctrl Pts',(20.4618589570356,-17.7288053547797,
3.43049316130316));
#172037=CARTESIAN_POINT('Ctrl Pts',(20.4597961532816,-17.7258966791383,
3.43027724126631));
#172038=CARTESIAN_POINT('Ctrl Pts',(20.4553116804107,-17.7196070458605,
3.42981061508776));
#172039=CARTESIAN_POINT('Ctrl Pts',(20.4528874030935,-17.7162280183219,
3.42956009232295));
#172040=CARTESIAN_POINT('Ctrl Pts',(20.4460846258646,-17.7068048603717,
3.42886185382716));
#172041=CARTESIAN_POINT('Ctrl Pts',(20.4416840478306,-17.700776639275,3.42841563472515));
#172042=CARTESIAN_POINT('Ctrl Pts',(20.4158828933032,-17.6658220821281,
3.42583012754213));
#172043=CARTESIAN_POINT('Ctrl Pts',(20.3937781263936,-17.6374199827396,
3.42373683954992));
#172044=CARTESIAN_POINT('Ctrl Pts',(20.3202496593505,-17.5477578381783,
3.41710375865058));
#172045=CARTESIAN_POINT('Ctrl Pts',(20.2660735486265,-17.488840176102,3.41270483440733));
#172046=CARTESIAN_POINT('Ctrl Pts',(20.0753509676859,-17.3036658052757,
3.39821265384092));
#172047=CARTESIAN_POINT('Ctrl Pts',(19.9255630372144,-17.1923410637516,
3.38827387289251));
#172048=CARTESIAN_POINT('Ctrl Pts',(19.7438713173816,-17.0912644980932,
3.37618125019198));
#172049=CARTESIAN_POINT('Ctrl Pts',(19.7244066973028,-17.080831593482,3.37488667870934));
#172050=CARTESIAN_POINT('Ctrl Pts',(19.6972690732012,-17.0668280756215,
3.37308152395338));
#172051=CARTESIAN_POINT('Ctrl Pts',(19.689732116709,-17.0629958682443,3.37258015212272));
#172052=CARTESIAN_POINT('Ctrl Pts',(19.6767390402116,-17.0564871320048,
3.37171569961167));
#172053=CARTESIAN_POINT('Ctrl Pts',(19.6712939426879,-17.0537887381825,
3.37135338879623));
#172054=CARTESIAN_POINT('Ctrl Pts',(19.660046122388,-17.0482749208505,3.37060485610026));
#172055=CARTESIAN_POINT('Ctrl Pts',(19.6542420064951,-17.045462498185,3.37021853444855));
#172056=CARTESIAN_POINT('Ctrl Pts',(19.6407080021807,-17.03898070744,3.36931752284501));
#172057=CARTESIAN_POINT('Ctrl Pts',(19.6329685791368,-17.035331613113,3.36880213631401));
#172058=CARTESIAN_POINT('Ctrl Pts',(19.6081365252051,-17.0238069297383,
3.36714793310628));
#172059=CARTESIAN_POINT('Ctrl Pts',(19.590961280438,-17.0161124751592,3.36600291251167));
#172060=CARTESIAN_POINT('Ctrl Pts',(19.5047183302013,-16.9788485005279,
3.36024747716289));
#172061=CARTESIAN_POINT('Ctrl Pts',(19.434220581151,-16.9527444962991,3.35552131377385));
#172062=CARTESIAN_POINT('Ctrl Pts',(19.2583709749715,-16.8980737815082,
3.3436886695316));
#172063=CARTESIAN_POINT('Ctrl Pts',(19.1519128260614,-16.8737980788603,
3.33648210440557));
#172064=CARTESIAN_POINT('Ctrl Pts',(18.9258875206594,-16.8403321465337,
3.32138759652239));
#172065=CARTESIAN_POINT('Ctrl Pts',(18.8064229707569,-16.8328672804233,
3.31352759279534));
#172066=CARTESIAN_POINT('Ctrl Pts',(18.6774513080357,-16.8357340392992,
3.30555982556304));
#172067=CARTESIAN_POINT('Ctrl Pts',(18.6679486157786,-16.8360093116053,
3.30497586470134));
#172068=CARTESIAN_POINT('Ctrl Pts',(18.6538681276579,-16.8365121404063,
3.30411551617469));
#172069=CARTESIAN_POINT('Ctrl Pts',(18.649288849566,-16.8366905609444,3.30383648511564));
#172070=CARTESIAN_POINT('Ctrl Pts',(18.6411413416848,-16.8370345088922,
3.30334144855333));
#172071=CARTESIAN_POINT('Ctrl Pts',(18.6375729229334,-16.8371941984035,
3.30312512073868));
#172072=CARTESIAN_POINT('Ctrl Pts',(18.6299006553742,-16.8375569980548,
3.30266106082491));
#172073=CARTESIAN_POINT('Ctrl Pts',(18.6257970007285,-16.8377630233025,
3.30241349378027));
#172074=CARTESIAN_POINT('Ctrl Pts',(18.6144685825303,-16.8383648391347,
3.30173178280331));
#172075=CARTESIAN_POINT('Ctrl Pts',(18.6072451298914,-16.8387857280082,
3.30129902277524));
#172076=CARTESIAN_POINT('Ctrl Pts',(18.5676406782732,-16.8412971636477,
3.29893618019018));
#172077=CARTESIAN_POINT('Ctrl Pts',(18.5353069688865,-16.8440950622238,
3.29704333166913));
#172078=CARTESIAN_POINT('Ctrl Pts',(18.3412644645688,-16.8653910016222,
3.28583412540617));
#172079=CARTESIAN_POINT('Ctrl Pts',(18.1820510116922,-16.9017457470014,
3.27723163670283));
#172080=CARTESIAN_POINT('Ctrl Pts',(17.9183983242485,-16.9949269006738,
3.26192319637002));
#172081=CARTESIAN_POINT('Ctrl Pts',(17.8116605124413,-17.0429096882309,
3.25540051232392));
#172082=CARTESIAN_POINT('Ctrl Pts',(17.6958125176361,-17.10698021256,3.24764506512588));
#172083=CARTESIAN_POINT('Ctrl Pts',(17.6822757385203,-17.1146629805324,
3.24672806874611));
#172084=CARTESIAN_POINT('Ctrl Pts',(17.6618266740128,-17.1265688342497,
3.24532580519973));
#172085=CARTESIAN_POINT('Ctrl Pts',(17.654851690941,-17.1306835788032,3.24484445694518));
#172086=CARTESIAN_POINT('Ctrl Pts',(17.6425600849073,-17.138030148823,3.24399071904006));
#172087=CARTESIAN_POINT('Ctrl Pts',(17.6372337498715,-17.1412455990557,
3.24361893042769));
#172088=CARTESIAN_POINT('Ctrl Pts',(17.6259970729934,-17.1480968251368,
3.24283065437021));
#172089=CARTESIAN_POINT('Ctrl Pts',(17.6200902883704,-17.1517382681706,
3.2424139615277));
#172090=CARTESIAN_POINT('Ctrl Pts',(17.6080390813448,-17.1592496717812,
3.24155900558252));
#172091=CARTESIAN_POINT('Ctrl Pts',(17.6018964596143,-17.1631223346866,
3.24112064608034));
#172092=CARTESIAN_POINT('Ctrl Pts',(17.586754859295,-17.1727776958993,3.24003363226849));
#172093=CARTESIAN_POINT('Ctrl Pts',(17.5777796275607,-17.1785970948363,
3.23938361821268));
#172094=CARTESIAN_POINT('Ctrl Pts',(17.4712655729678,-17.2488114344553,
3.23160074071753));
#172095=CARTESIAN_POINT('Ctrl Pts',(17.3791929616813,-17.3210985407488,
3.22416359540188));
#172096=CARTESIAN_POINT('Ctrl Pts',(17.1575742715224,-17.5268658373759,
3.20441839977583));
#172097=CARTESIAN_POINT('Ctrl Pts',(17.0387764816844,-17.6704600483137,
3.19185515152312));
#172098=CARTESIAN_POINT('Ctrl Pts',(16.9326610880885,-17.839763629678,3.17941612942038));
#172099=CARTESIAN_POINT('Ctrl Pts',(16.9252230606113,-17.8519010827888,
3.17853668626084));
#172100=CARTESIAN_POINT('Ctrl Pts',(16.9150488886815,-17.8688855990024,
3.17732406635359));
#172101=CARTESIAN_POINT('Ctrl Pts',(16.9122087663511,-17.8736695063082,
3.17698448413844));
#172102=CARTESIAN_POINT('Ctrl Pts',(16.9076800568673,-17.8813666349358,
3.17644133050573));
#172103=CARTESIAN_POINT('Ctrl Pts',(16.9059795267723,-17.8842727469519,
3.17623699190379));
#172104=CARTESIAN_POINT('Ctrl Pts',(16.9024417716782,-17.8903518007728,
3.17581110315119));
#172105=CARTESIAN_POINT('Ctrl Pts',(16.9006058499074,-17.8935254687615,
3.1755896421561));
#172106=CARTESIAN_POINT('Ctrl Pts',(16.8961844996462,-17.901214456298,3.17505518944349));
#172107=CARTESIAN_POINT('Ctrl Pts',(16.8936074330109,-17.9057346068626,
3.17474273630196));
#172108=CARTESIAN_POINT('Ctrl Pts',(16.8846505067469,-17.9215804623655,
3.1736533007204));
#172109=CARTESIAN_POINT('Ctrl Pts',(16.8783581697579,-17.9329556493819,
3.17288173911637));
#172110=CARTESIAN_POINT('Ctrl Pts',(16.841827006579,-18.0004566431848,3.16836065650515));
#172111=CARTESIAN_POINT('Ctrl Pts',(16.8140283819398,-18.0578725289664,
3.16474736288815));
#172112=CARTESIAN_POINT('Ctrl Pts',(16.7733550786844,-18.1525601282371,
3.1590194040154));
#172113=CARTESIAN_POINT('Ctrl Pts',(16.7588705942293,-18.1890512064045,
3.15686514330449));
#172114=CARTESIAN_POINT('Ctrl Pts',(16.7454192974521,-18.225889960506,3.15472450021249));
#172115=CARTESIAN_POINT('Ctrl Pts',(16.7454193844899,-18.2258897221376,
2.93545674301194));
#172116=CARTESIAN_POINT('Ctrl Pts',(16.7759470815439,-18.1422842582728,
2.94055495122605));
#172117=CARTESIAN_POINT('Ctrl Pts',(16.8117309549823,-18.0606488015625,
2.94543447229376));
#172118=CARTESIAN_POINT('Ctrl Pts',(16.8782378463899,-17.931720516084,2.95332993456547));
#172119=CARTESIAN_POINT('Ctrl Pts',(16.9058676585179,-17.8830025582496,
2.95636023097386));
#172120=CARTESIAN_POINT('Ctrl Pts',(16.9829403244133,-17.7588508291059,
2.96432632192045));
#172121=CARTESIAN_POINT('Ctrl Pts',(17.0353246888041,-17.6853843571324,
2.96929182853531));
#172122=CARTESIAN_POINT('Ctrl Pts',(17.1225828220143,-17.5781967170225,
2.97715510187905));
#172123=CARTESIAN_POINT('Ctrl Pts',(17.1541971425227,-17.5419563147247,
2.97993326331005));
#172124=CARTESIAN_POINT('Ctrl Pts',(17.1951439827439,-17.4981248607339,
2.98346365873175));
#172125=CARTESIAN_POINT('Ctrl Pts',(17.203345040904,-17.4894931966346,2.98416750350011));
#172126=CARTESIAN_POINT('Ctrl Pts',(17.2166778947079,-17.4756952740827,
2.98530684168578));
#172127=CARTESIAN_POINT('Ctrl Pts',(17.221764368589,-17.4704854344176,2.98574036242394));
#172128=CARTESIAN_POINT('Ctrl Pts',(17.2313501507484,-17.4607679617444,
2.98655529820242));
#172129=CARTESIAN_POINT('Ctrl Pts',(17.2358431310879,-17.4562541806395,
2.98693643215704));
#172130=CARTESIAN_POINT('Ctrl Pts',(17.2459428252301,-17.4461988883982,
2.98779135310418));
#172131=CARTESIAN_POINT('Ctrl Pts',(17.2515602398015,-17.4406683031692,
2.98826561433618));
#172132=CARTESIAN_POINT('Ctrl Pts',(17.2658704372284,-17.4267358453692,
2.98947072735871));
#172133=CARTESIAN_POINT('Ctrl Pts',(17.2746044567646,-17.418376906356,2.99020343246399));
#172134=CARTESIAN_POINT('Ctrl Pts',(17.3248503942984,-17.3711066757997,
2.99440318358987));
#172135=CARTESIAN_POINT('Ctrl Pts',(17.3678427366168,-17.3338097525053,
2.99793819039885));
#172136=CARTESIAN_POINT('Ctrl Pts',(17.4333458490969,-17.2814567054356,
3.00324450435915));
#172137=CARTESIAN_POINT('Ctrl Pts',(17.4547288890248,-17.2650259476538,
3.00496480060166));
#172138=CARTESIAN_POINT('Ctrl Pts',(17.6003778284853,-17.1574709138737,
3.01659910237716));
#172139=CARTESIAN_POINT('Ctrl Pts',(17.7339561624323,-17.0797450510681,
3.02691629130477));
#172140=CARTESIAN_POINT('Ctrl Pts',(17.9219735294178,-16.9962468782493,
3.04036301841443));
#172141=CARTESIAN_POINT('Ctrl Pts',(17.9699375952316,-16.977014779409,3.04370271288394));
#172142=CARTESIAN_POINT('Ctrl Pts',(18.0441765915031,-16.9503573062147,
3.04868882247872));
#172143=CARTESIAN_POINT('Ctrl Pts',(18.0699694517278,-16.9416534124646,
3.05038822796867));
#172144=CARTESIAN_POINT('Ctrl Pts',(18.1024471678401,-16.9313870190893,
3.05248095324582));
#172145=CARTESIAN_POINT('Ctrl Pts',(18.108980034542,-16.9293567185075,3.05289953840353));
#172146=CARTESIAN_POINT('Ctrl Pts',(18.1193687795427,-16.9261832177474,
3.05356130598534));
#172147=CARTESIAN_POINT('Ctrl Pts',(18.1232182057589,-16.9250192963761,
3.05380567339267));
#172148=CARTESIAN_POINT('Ctrl Pts',(18.1305088015917,-16.9228375494816,
3.05426686675133));
#172149=CARTESIAN_POINT('Ctrl Pts',(18.1339491990775,-16.9218175171612,
3.0544838147274));
#172150=CARTESIAN_POINT('Ctrl Pts',(18.1418526035801,-16.9194961077351,
3.05498064246653));
#172151=CARTESIAN_POINT('Ctrl Pts',(18.1463173115717,-16.9182006810346,
3.05526017331096));
#172152=CARTESIAN_POINT('Ctrl Pts',(18.1582482856154,-16.9147814997828,
3.0560042297709));
#172153=CARTESIAN_POINT('Ctrl Pts',(18.1657221063818,-16.9126840622291,
3.056467266286));
#172154=CARTESIAN_POINT('Ctrl Pts',(18.2200966986481,-16.8977466260996,
3.05981497436556));
#172155=CARTESIAN_POINT('Ctrl Pts',(18.2674198841836,-16.886483765382,3.0626151490539));
#172156=CARTESIAN_POINT('Ctrl Pts',(18.3418054726836,-16.8714675922194,
3.0669002103813));
#172157=CARTESIAN_POINT('Ctrl Pts',(18.3686206275118,-16.8665912509613,
3.06842165420803));
#172158=CARTESIAN_POINT('Ctrl Pts',(18.5444152053767,-16.8381180255152,
3.07828623215645));
#172159=CARTESIAN_POINT('Ctrl Pts',(18.6954586479851,-16.8299828652455,
3.08628188131668));
#172160=CARTESIAN_POINT('Ctrl Pts',(18.9027629555578,-16.8409744005262,
3.09780984267062));
#172161=CARTESIAN_POINT('Ctrl Pts',(18.9592900578601,-16.84625696929,3.10100617960215));
#172162=CARTESIAN_POINT('Ctrl Pts',(19.0502689829886,-16.8584644307665,
3.10628390994597));
#172163=CARTESIAN_POINT('Ctrl Pts',(19.0848813825118,-16.8639867587772,
3.10832317482897));
#172164=CARTESIAN_POINT('Ctrl Pts',(19.1300503338849,-16.8723481567688,
3.11103198762125));
#172165=CARTESIAN_POINT('Ctrl Pts',(19.1407456792376,-16.8744135152211,
3.11167690606008));
#172166=CARTESIAN_POINT('Ctrl Pts',(19.1582053094646,-16.8779250989166,
3.11273563594417));
#172167=CARTESIAN_POINT('Ctrl Pts',(19.1649793716629,-16.8793221139459,
3.1131478713426));
#172168=CARTESIAN_POINT('Ctrl Pts',(19.1780566089302,-16.8820859135468,
3.11394656887917));
#172169=CARTESIAN_POINT('Ctrl Pts',(19.1843606305514,-16.8834483573636,
3.11433288789866));
#172170=CARTESIAN_POINT('Ctrl Pts',(19.1988703577518,-16.8866537142894,
3.1152251007538));
#172171=CARTESIAN_POINT('Ctrl Pts',(19.2070714636147,-16.8885167515727,
3.11573163611591));
#172172=CARTESIAN_POINT('Ctrl Pts',(19.2290272643409,-16.8936421981323,
3.11709384074838));
#172173=CARTESIAN_POINT('Ctrl Pts',(19.2427605651743,-16.8969935510907,
3.1179523583835));
#172174=CARTESIAN_POINT('Ctrl Pts',(19.3609862861363,-16.9271020355118,
3.12540014510187));
#172175=CARTESIAN_POINT('Ctrl Pts',(19.4633101018816,-16.9616673310542,
3.13224467165334));
#172176=CARTESIAN_POINT('Ctrl Pts',(19.682284609536,-17.0547976318088,3.14773322831267));
#172177=CARTESIAN_POINT('Ctrl Pts',(19.7970691509984,-17.1166520128045,
3.15643004234202));
#172178=CARTESIAN_POINT('Ctrl Pts',(19.9461973452119,-17.2157223211458,
3.16811289623007));
#172179=CARTESIAN_POINT('Ctrl Pts',(19.9860007734155,-17.2442010430706,
3.17127003906701));
#172180=CARTESIAN_POINT('Ctrl Pts',(20.0455788678032,-17.2900318314815,
3.17601653352989));
#172181=CARTESIAN_POINT('Ctrl Pts',(20.0660757446133,-17.3064144881906,
3.17765342343682));
#172182=CARTESIAN_POINT('Ctrl Pts',(20.091463258744,-17.327491407066,3.17968031742504));
#172183=CARTESIAN_POINT('Ctrl Pts',(20.096642081454,-17.3318329629149,3.18009375407533));
#172184=CARTESIAN_POINT('Ctrl Pts',(20.1048553908031,-17.3387856554528,
3.18074926601894));
#172185=CARTESIAN_POINT('Ctrl Pts',(20.1079033629727,-17.3413806862658,
3.18099248895619));
#172186=CARTESIAN_POINT('Ctrl Pts',(20.1136732040162,-17.3463214018786,
3.18145280795395));
#172187=CARTESIAN_POINT('Ctrl Pts',(20.116396427197,-17.3486653410558,3.18167001884687));
#172188=CARTESIAN_POINT('Ctrl Pts',(20.1226548573037,-17.3540799103537,
3.18216911898711));
#172189=CARTESIAN_POINT('Ctrl Pts',(20.1261858521274,-17.3571553430793,
3.18245064823499));
#172190=CARTESIAN_POINT('Ctrl Pts',(20.1356298441975,-17.3654361537914,
3.18320355028272));
#172191=CARTESIAN_POINT('Ctrl Pts',(20.1415241038807,-17.3706629203105,
3.18367337757931));
#172192=CARTESIAN_POINT('Ctrl Pts',(20.185662776115,-17.4102454426791,3.1871922595319));
#172193=CARTESIAN_POINT('Ctrl Pts',(20.2226768681572,-17.4459541722953,
3.19014678140815));
#172194=CARTESIAN_POINT('Ctrl Pts',(20.2681769694972,-17.4931681752255,
3.19384034453995));
#172195=CARTESIAN_POINT('Ctrl Pts',(20.2778947156805,-17.5034564602049,
3.19463299310619));
#172196=CARTESIAN_POINT('Ctrl Pts',(20.3959786432631,-17.6310115394064,
3.20432288012174));
#172197=CARTESIAN_POINT('Ctrl Pts',(20.490847236747,-17.760078821804,3.21275663181213));
#172198=CARTESIAN_POINT('Ctrl Pts',(20.5989632037442,-17.9485469210057,
3.2248143437229));
#172199=CARTESIAN_POINT('Ctrl Pts',(20.6255684271208,-17.9996481757029,
3.22805588697978));
#172200=CARTESIAN_POINT('Ctrl Pts',(20.6651178004025,-18.0838251539264,
3.23340152458345));
#172201=CARTESIAN_POINT('Ctrl Pts',(20.6793718703327,-18.1162538705707,
3.23546205570788));
#172202=CARTESIAN_POINT('Ctrl Pts',(20.6969527322443,-18.1591411608038,
3.23819514244229));
#172203=CARTESIAN_POINT('Ctrl Pts',(20.7010217481454,-18.1692906008916,
3.2388425031233));
#172204=CARTESIAN_POINT('Ctrl Pts',(20.7075392488657,-18.1859191946397,
3.2399042286608));
#172205=CARTESIAN_POINT('Ctrl Pts',(20.7100349199889,-18.1923797261873,
3.2403170000799));
#172206=CARTESIAN_POINT('Ctrl Pts',(20.7147921113036,-18.2048767407529,
3.24111602031924));
#172207=CARTESIAN_POINT('Ctrl Pts',(20.7170578533226,-18.2109115426207,
3.24150212220492));
#172208=CARTESIAN_POINT('Ctrl Pts',(20.7222085224844,-18.2248231049034,
3.24239280256983));
#172209=CARTESIAN_POINT('Ctrl Pts',(20.7250742515243,-18.2327068140211,
3.2428980155042));
#172210=CARTESIAN_POINT('Ctrl Pts',(20.7326183448691,-18.2538514141624,
3.24425436006234));
#172211=CARTESIAN_POINT('Ctrl Pts',(20.7372115032743,-18.267142062521,3.24510830184878));
#172212=CARTESIAN_POINT('Ctrl Pts',(20.7747041130236,-18.3792348470295,
3.25232325247312));
#172213=CARTESIAN_POINT('Ctrl Pts',(20.8003997794936,-18.480280239586,3.25892146285842));
#172214=CARTESIAN_POINT('Ctrl Pts',(20.8415710643165,-18.7127349991036,
3.27426306811785));
#172215=CARTESIAN_POINT('Ctrl Pts',(20.8523843199,-18.8445354215822,3.28308291295183));
#172216=CARTESIAN_POINT('Ctrl Pts',(20.8502762805914,-19.0268220942563,
3.29498917484003));
#172217=CARTESIAN_POINT('Ctrl Pts',(20.8478984436826,-19.0771306817407,
3.29824124810074));
#172218=CARTESIAN_POINT('Ctrl Pts',(20.8415135785747,-19.1539680466944,
3.30311260736189));
#172219=CARTESIAN_POINT('Ctrl Pts',(20.8387931751151,-19.1805835088037,
3.3047822372525));
#172220=CARTESIAN_POINT('Ctrl Pts',(20.8347491290615,-19.2138937958856,
3.30684364110698));
#172221=CARTESIAN_POINT('Ctrl Pts',(20.833896832304,-19.2206420669969,3.30725979942214));
#172222=CARTESIAN_POINT('Ctrl Pts',(20.8324900180221,-19.2313648987244,
3.30791861861039));
#172223=CARTESIAN_POINT('Ctrl Pts',(20.8319567066514,-19.2353421253766,
3.30816244680647));
#172224=CARTESIAN_POINT('Ctrl Pts',(20.8309247712772,-19.2428752240934,
3.30862322491539));
#172225=CARTESIAN_POINT('Ctrl Pts',(20.830428415835,-19.2464312989907,3.30884029347265));
#172226=CARTESIAN_POINT('Ctrl Pts',(20.8292664407998,-19.2546041957732,
3.30933817713624));
#172227=CARTESIAN_POINT('Ctrl Pts',(20.8285946086494,-19.2592200898561,
3.30961863816703));
#172228=CARTESIAN_POINT('Ctrl Pts',(20.8267562266423,-19.271564493191,3.31036680757182));
#172229=CARTESIAN_POINT('Ctrl Pts',(20.8255621107907,-19.2792889097217,
3.310833000746));
#172230=CARTESIAN_POINT('Ctrl Pts',(20.8164287987521,-19.3362776034545,
3.31425907681197));
#172231=CARTESIAN_POINT('Ctrl Pts',(20.8067921061513,-19.3852582527571,
3.31712994017732));
#172232=CARTESIAN_POINT('Ctrl Pts',(20.7897351449627,-19.4582297187077,
3.32135674762059));
#172233=CARTESIAN_POINT('Ctrl Pts',(20.7836059566652,-19.4825007122062,
3.32275412859375));
#172234=CARTESIAN_POINT('Ctrl Pts',(20.7393513635755,-19.6455097222503,
3.33211511171528));
#172235=CARTESIAN_POINT('Ctrl Pts',(20.6875982112282,-19.7801585200771,
3.33975532083144));
#172236=CARTESIAN_POINT('Ctrl Pts',(20.5946491093862,-19.9636802394936,
3.3511356401834));
#172237=CARTESIAN_POINT('Ctrl Pts',(20.564311068918,-20.0175855415329,3.35460516621097));
#172238=CARTESIAN_POINT('Ctrl Pts',(20.5119764095494,-20.1017294375973,
3.36029176480344));
#172239=CARTESIAN_POINT('Ctrl Pts',(20.4914623268213,-20.1328487678449,
3.36245762587111));
#172240=CARTESIAN_POINT('Ctrl Pts',(20.463766235496,-20.1725415919741,3.36531069886447));
#172241=CARTESIAN_POINT('Ctrl Pts',(20.4573221120493,-20.1816234782072,
3.3659698165557));
#172242=CARTESIAN_POINT('Ctrl Pts',(20.4467284701655,-20.1963065423077,
3.3670459714976));
#172243=CARTESIAN_POINT('Ctrl Pts',(20.4426223591354,-20.2019388848348,
3.36746133058823));
#172244=CARTESIAN_POINT('Ctrl Pts',(20.434674560547,-20.2127285173225,3.36826198986839));
#172245=CARTESIAN_POINT('Ctrl Pts',(20.4308370364429,-20.2178887888051,
3.3686471250419));
#172246=CARTESIAN_POINT('Ctrl Pts',(20.4219994872438,-20.2296601415075,
3.36953079444804));
#172247=CARTESIAN_POINT('Ctrl Pts',(20.4169840502601,-20.2362594713105,
3.37002993074997));
#172248=CARTESIAN_POINT('Ctrl Pts',(20.4035631274798,-20.2537051342916,
3.37135945867928));
#172249=CARTESIAN_POINT('Ctrl Pts',(20.3950908262364,-20.2644993509937,
3.37219248885101));
#172250=CARTESIAN_POINT('Ctrl Pts',(20.3301141934909,-20.3456465592972,
3.37853531216837));
#172251=CARTESIAN_POINT('Ctrl Pts',(20.2692759214737,-20.4123956236509,
3.38422123195241));
#172252=CARTESIAN_POINT('Ctrl Pts',(20.1040429515391,-20.5719132815576,
3.3990491691745));
#172253=CARTESIAN_POINT('Ctrl Pts',(19.9943909845992,-20.6586183970893,
3.40836597789303));
#172254=CARTESIAN_POINT('Ctrl Pts',(19.8304355719691,-20.7637896475959,
3.42112380011482));
#172255=CARTESIAN_POINT('Ctrl Pts',(19.7826887939228,-20.7918384016435,
3.42471118619517));
#172256=CARTESIAN_POINT('Ctrl Pts',(19.708770732619,-20.8314476486225,3.43001917987131));
#172257=CARTESIAN_POINT('Ctrl Pts',(19.6833761934619,-20.8444023022816,
3.43180054543422));
#172258=CARTESIAN_POINT('Ctrl Pts',(19.6514772289623,-20.8598712665299,
3.43397918279146));
#172259=CARTESIAN_POINT('Ctrl Pts',(19.6452131115392,-20.862870980407,3.43440422055783));
#172260=CARTESIAN_POINT('Ctrl Pts',(19.635277757715,-20.8675687830322,3.43507382443312));
#172261=CARTESIAN_POINT('Ctrl Pts',(19.6316162868592,-20.8692872401593,
3.4353196229997));
#172262=CARTESIAN_POINT('Ctrl Pts',(19.6247017322823,-20.8725083348189,
3.4357819455412));
#172263=CARTESIAN_POINT('Ctrl Pts',(19.6214497987299,-20.8740131880172,
3.4359986004432));
#172264=CARTESIAN_POINT('Ctrl Pts',(19.6140065032312,-20.87743470274,3.43649274590803));
#172265=CARTESIAN_POINT('Ctrl Pts',(19.6098126979085,-20.8793459366048,
3.43676990072171));
#172266=CARTESIAN_POINT('Ctrl Pts',(19.5986629934554,-20.8843832600036,
3.43750348515486));
#172267=CARTESIAN_POINT('Ctrl Pts',(19.5916963144821,-20.8874855183854,
3.43795849113888));
#172268=CARTESIAN_POINT('Ctrl Pts',(19.5428156064377,-20.9089363175357,
3.44112854378698));
#172269=CARTESIAN_POINT('Ctrl Pts',(19.5003298265819,-20.9259609175579,
3.44376885334204));
#172270=CARTESIAN_POINT('Ctrl Pts',(19.4510875086233,-20.9438630767841,
3.44673522128603));
#172271=CARTESIAN_POINT('Ctrl Pts',(19.4448419538897,-20.9461004813692,
3.44710975171836));
#172272=CARTESIAN_POINT('Ctrl Pts',(19.4352870203563,-20.9494728417585,
3.44768028399848));
#172273=CARTESIAN_POINT('Ctrl Pts',(19.4319852141408,-20.9506289999753,
3.44787699140494));
#172274=CARTESIAN_POINT('Ctrl Pts',(19.2892700983293,-21.0002052354252,
3.45636069395331));
#172275=CARTESIAN_POINT('Ctrl Pts',(19.1451709770689,-21.0339254455784,
3.46418597921613));
#172276=CARTESIAN_POINT('Ctrl Pts',(18.9017618184516,-21.0646042777067,
3.47766679983518));
#172277=CARTESIAN_POINT('Ctrl Pts',(18.8040761841515,-21.0700951211588,
3.48313953588566));
#172278=CARTESIAN_POINT('Ctrl Pts',(18.684700857321,-21.0685368217708,3.4900893661415));
#172279=CARTESIAN_POINT('Ctrl Pts',(18.6630404565635,-21.0679213632152,
3.49136056928072));
#172280=CARTESIAN_POINT('Ctrl Pts',(18.6323461967869,-21.0665773861516,
3.49317781885006));
#172281=CARTESIAN_POINT('Ctrl Pts',(18.6233012462277,-21.0661231751636,
3.49371527734835));
#172282=CARTESIAN_POINT('Ctrl Pts',(18.6077351090038,-21.0652413214848,
3.49464370028917));
#172283=CARTESIAN_POINT('Ctrl Pts',(18.6012124276154,-21.0648414906643,
3.49503378731128));
#172284=CARTESIAN_POINT('Ctrl Pts',(18.5887492848719,-21.0640195776363,
3.49578118851852));
#172285=CARTESIAN_POINT('Ctrl Pts',(18.5828085397848,-21.0636026159759,
3.49613833815913));
#172286=CARTESIAN_POINT('Ctrl Pts',(18.5674132547923,-21.0624567694386,
3.49706622564269));
#172287=CARTESIAN_POINT('Ctrl Pts',(18.5579617882873,-21.0616894233012,
3.49763816723172));
#172288=CARTESIAN_POINT('Ctrl Pts',(18.5259974681395,-21.0588780102242,
3.49958037477924));
#172289=CARTESIAN_POINT('Ctrl Pts',(18.5035129097444,-21.0565369187251,
3.50095992805857));
#172290=CARTESIAN_POINT('Ctrl Pts',(18.3020350626346,-21.0322916299343,
3.51344598259085));
#172291=CARTESIAN_POINT('Ctrl Pts',(18.1265177211764,-20.9879633804279,
3.52530095484291));
#172292=CARTESIAN_POINT('Ctrl Pts',(17.8809191597038,-20.8913151870048,
3.54273408455607));
#172293=CARTESIAN_POINT('Ctrl Pts',(17.8049369818549,-20.8560835191905,
3.54824059949552));
#172294=CARTESIAN_POINT('Ctrl Pts',(17.6986805839837,-20.7989350608254,
3.55593786516203));
#172295=CARTESIAN_POINT('Ctrl Pts',(17.6665872714109,-20.7805748176268,
3.55826173359992));
#172296=CARTESIAN_POINT('Ctrl Pts',(17.6285600993605,-20.7574772796631,
3.56099931633537));
#172297=CARTESIAN_POINT('Ctrl Pts',(17.6221518087216,-20.7535380053606,
3.56146008983523));
#172298=CARTESIAN_POINT('Ctrl Pts',(17.6122225228686,-20.7473611594343,
3.56217299124678));
#172299=CARTESIAN_POINT('Ctrl Pts',(17.6086869895072,-20.7451472416156,
3.56242662828347));
#172300=CARTESIAN_POINT('Ctrl Pts',(17.6021423731771,-20.7410220846892,
3.56289571687127));
#172301=CARTESIAN_POINT('Ctrl Pts',(17.5991316008057,-20.7391137131423,
3.56311134663739));
#172302=CARTESIAN_POINT('Ctrl Pts',(17.5923358765432,-20.7347821588739,
3.56359768294462));
#172303=CARTESIAN_POINT('Ctrl Pts',(17.5885538222792,-20.7323545297463,
3.5638680896978));
#172304=CARTESIAN_POINT('Ctrl Pts',(17.5774135297954,-20.7251535928498,
3.5646639223471));
#172305=CARTESIAN_POINT('Ctrl Pts',(17.5700770883693,-20.7203465126205,
3.56518715377071));
#172306=CARTESIAN_POINT('Ctrl Pts',(17.5172400270725,-20.6852546301564,
3.56895081440199));
#172307=CARTESIAN_POINT('Ctrl Pts',(17.4728933733905,-20.6532605943579,
3.57208475553217));
#172308=CARTESIAN_POINT('Ctrl Pts',(17.2972506856308,-20.5158954866961,
3.58461109173557));
#172309=CARTESIAN_POINT('Ctrl Pts',(17.1775027564072,-20.3967634918128,
3.59346953744706));
#172310=CARTESIAN_POINT('Ctrl Pts',(17.0365790293146,-20.2184613731332,
3.60606881771752));
#172311=CARTESIAN_POINT('Ctrl Pts',(17.0019838239229,-20.1707212819433,
3.60938273522733));
#172312=CARTESIAN_POINT('Ctrl Pts',(16.9495309616789,-20.0915859337807,
3.61483688239362));
#172313=CARTESIAN_POINT('Ctrl Pts',(16.9304052155671,-20.0610678412497,
3.61693119579561));
#172314=CARTESIAN_POINT('Ctrl Pts',(16.9064660217075,-20.0206110442278,
3.6197028083194));
#172315=CARTESIAN_POINT('Ctrl Pts',(16.9009381177284,-20.0111006253011,
3.62035400052919));
#172316=CARTESIAN_POINT('Ctrl Pts',(16.8920438741355,-19.9955203868616,
3.62142042708464));
#172317=CARTESIAN_POINT('Ctrl Pts',(16.8886327781257,-19.9894762561496,
3.62183404056539));
#172318=CARTESIAN_POINT('Ctrl Pts',(16.8821134427118,-19.9777907507361,
3.62263357975897));
#172319=CARTESIAN_POINT('Ctrl Pts',(16.8790011034011,-19.9721517424166,
3.62301935259321));
#172320=CARTESIAN_POINT('Ctrl Pts',(16.8719106576768,-19.9591653735746,
3.62390768280936));
#172321=CARTESIAN_POINT('Ctrl Pts',(16.8679502368883,-19.9518085251618,
3.62441086379798));
#172322=CARTESIAN_POINT('Ctrl Pts',(16.857494875827,-19.9321081894115,3.62575822111199));
#172323=CARTESIAN_POINT('Ctrl Pts',(16.8510782832184,-19.919723792131,3.6266051495001));
#172324=CARTESIAN_POINT('Ctrl Pts',(16.8001375194838,-19.8189801749733,
3.6334951568589));
#172325=CARTESIAN_POINT('Ctrl Pts',(16.7617417033069,-19.7276745962983,
3.6397514818284));
#172326=CARTESIAN_POINT('Ctrl Pts',(16.6860055055724,-19.5051258936198,
3.65499319442853));
#172327=CARTESIAN_POINT('Ctrl Pts',(16.6546777501633,-19.3722916901845,
3.66409684717405));
#172328=CARTESIAN_POINT('Ctrl Pts',(16.6262468690777,-19.1633139088278,
3.67787830905605));
#172329=CARTESIAN_POINT('Ctrl Pts',(16.6200989473124,-19.0887539837339,
3.6826851014469));
#172330=CARTESIAN_POINT('Ctrl Pts',(16.617649085885,-19.0051628103158,3.68784414639839));
#172331=CARTESIAN_POINT('Ctrl Pts',(16.6174451480529,-18.99630621939,3.68838785288456));
#172332=CARTESIAN_POINT('Ctrl Pts',(16.6172222390634,-18.9829958379578,
3.68920035586386));
#172333=CARTESIAN_POINT('Ctrl Pts',(16.6171617202317,-18.978542971068,3.6894713942079));
#172334=CARTESIAN_POINT('Ctrl Pts',(16.6170816555799,-18.9708703404116,
3.68993703635941));
#172335=CARTESIAN_POINT('Ctrl Pts',(16.6170554039629,-18.9676507020389,
3.69013201251977));
#172336=CARTESIAN_POINT('Ctrl Pts',(16.6170125976391,-18.960360878647,3.6905725165307));
#172337=CARTESIAN_POINT('Ctrl Pts',(16.6170004354008,-18.956290708061,3.69081779563898));
#172338=CARTESIAN_POINT('Ctrl Pts',(16.6169992761381,-18.9451601459764,
3.69148678110644));
#172339=CARTESIAN_POINT('Ctrl Pts',(16.6170338608871,-18.9380997307795,
3.69190918767181));
#172340=CARTESIAN_POINT('Ctrl Pts',(16.6174008065129,-18.901040209158,3.69411674773463));
#172341=CARTESIAN_POINT('Ctrl Pts',(16.6183355257536,-18.8710488603327,
3.69587020225227));
#172342=CARTESIAN_POINT('Ctrl Pts',(16.6230423750926,-18.7813334126221,
3.70104314768622));
#172343=CARTESIAN_POINT('Ctrl Pts',(16.6287093235971,-18.721736293826,3.70438373877959));
#172344=CARTESIAN_POINT('Ctrl Pts',(16.6574679273623,-18.5134441951214,
3.7159609037468));
#172345=CARTESIAN_POINT('Ctrl Pts',(16.6938573090406,-18.3671015374049,
3.72394888845156));
#172346=CARTESIAN_POINT('Ctrl Pts',(16.7454193692324,-18.2258897639231,
3.73234496387082));
#172347=CARTESIAN_POINT('Origin',(18.734,-18.952,0.));
#172348=CARTESIAN_POINT('',(16.7454193672347,-18.225889769394,4.75730093103984));
#172349=CARTESIAN_POINT('',(16.7454193964829,-18.2258896892926,4.53222340662745));
#172350=CARTESIAN_POINT('',(16.7454193692319,-18.2258897639242,0.));
#172351=CARTESIAN_POINT('',(16.6170000778093,-18.952573972551,4.70909170728562));
#172352=CARTESIAN_POINT('Ctrl Pts',(16.7454193672347,-18.225889769394,4.75730093103984));
#172353=CARTESIAN_POINT('Ctrl Pts',(16.7303995485604,-18.2670241857187,
4.75455315814197));
#172354=CARTESIAN_POINT('Ctrl Pts',(16.7166594239208,-18.3086153643389,
4.75176655660383));
#172355=CARTESIAN_POINT('Ctrl Pts',(16.646312753438,-18.5460434110503,4.73582624675881));
#172356=CARTESIAN_POINT('Ctrl Pts',(16.6169448256217,-18.7487856962723,
4.72195810323501));
#172357=CARTESIAN_POINT('Ctrl Pts',(16.6170000778093,-18.952573972551,4.70909170728562));
#172358=CARTESIAN_POINT('Ctrl Pts',(16.6170000784466,-18.9525763185082,
4.70909155917109));
#172359=CARTESIAN_POINT('Ctrl Pts',(16.6170043638029,-18.9683177858256,
4.70809770510508));
#172360=CARTESIAN_POINT('Ctrl Pts',(16.6171842235391,-18.9840592810225,
4.70711097584169));
#172361=CARTESIAN_POINT('Ctrl Pts',(16.6177851446519,-19.0106677086203,
4.70545672920642));
#172362=CARTESIAN_POINT('Ctrl Pts',(16.6181143694088,-19.0215357710275,
4.70478491638385));
#172363=CARTESIAN_POINT('Ctrl Pts',(16.6187085002744,-19.0371682452493,
4.70382459956396));
#172364=CARTESIAN_POINT('Ctrl Pts',(16.6189057981575,-19.0419348494304,
4.70353258719135));
#172365=CARTESIAN_POINT('Ctrl Pts',(16.6192791186492,-19.0502719316248,
4.70302329503004));
#172366=CARTESIAN_POINT('Ctrl Pts',(16.6194480742848,-19.0538426848307,
4.70280563353445));
#172367=CARTESIAN_POINT('Ctrl Pts',(16.6197955283407,-19.0608119166624,
4.70238174654777));
#172368=CARTESIAN_POINT('Ctrl Pts',(16.6199731789209,-19.0642104344126,
4.70217547433106));
#172369=CARTESIAN_POINT('Ctrl Pts',(16.6203449448697,-19.0710079765581,
4.70176378523197));
#172370=CARTESIAN_POINT('Ctrl Pts',(16.6205390643402,-19.0744069621433,
4.70155836834217));
#172371=CARTESIAN_POINT('Ctrl Pts',(16.6210263189166,-19.0825917791343,
4.7010647506778));
#172372=CARTESIAN_POINT('Ctrl Pts',(16.6213275167566,-19.087377137277,4.70077699901608));
#172373=CARTESIAN_POINT('Ctrl Pts',(16.6224923816379,-19.1049326605121,
4.69972433448047));
#172374=CARTESIAN_POINT('Ctrl Pts',(16.6234556165371,-19.1176962417628,
4.69896478990194));
#172375=CARTESIAN_POINT('Ctrl Pts',(16.626705176885,-19.1561092997692,4.69669421515918));
#172376=CARTESIAN_POINT('Ctrl Pts',(16.6293438484297,-19.1817274135841,
4.69520056233799));
#172377=CARTESIAN_POINT('Ctrl Pts',(16.6557757821633,-19.3993135917065,
4.68264215644977));
#172378=CARTESIAN_POINT('Ctrl Pts',(16.705310468741,-19.5872492273014,4.67256750562623));
#172379=CARTESIAN_POINT('Ctrl Pts',(16.8017752320132,-19.8188889000282,
4.65864103069371));
#172380=CARTESIAN_POINT('Ctrl Pts',(16.8260072394902,-19.8709950098483,
4.65540741632111));
#172381=CARTESIAN_POINT('Ctrl Pts',(16.868526570959,-19.9534728106902,4.65007368184504));
#172382=CARTESIAN_POINT('Ctrl Pts',(16.8855103020577,-19.9844846377123,
4.64801687137834));
#172383=CARTESIAN_POINT('Ctrl Pts',(16.9087490825874,-20.024505243469,4.64528803022755));
#172384=CARTESIAN_POINT('Ctrl Pts',(16.9143093172387,-20.0339122982393,
4.64464109505808));
#172385=CARTESIAN_POINT('Ctrl Pts',(16.9235113715937,-20.0492091283716,
4.64357989145143));
#172386=CARTESIAN_POINT('Ctrl Pts',(16.9271097445465,-20.0551249013447,
4.64316721341621));
#172387=CARTESIAN_POINT('Ctrl Pts',(16.9341142634616,-20.0665141972177,
4.64236824973311));
#172388=CARTESIAN_POINT('Ctrl Pts',(16.937516520852,-20.0719900303649,4.64198211035626));
#172389=CARTESIAN_POINT('Ctrl Pts',(16.945405197213,-20.0845581927722,4.64109116471016));
#172390=CARTESIAN_POINT('Ctrl Pts',(16.9499088621105,-20.0916395206857,
4.64058572276215));
#172391=CARTESIAN_POINT('Ctrl Pts',(16.9620781834053,-20.1105249993702,
4.63922836415674));
#172392=CARTESIAN_POINT('Ctrl Pts',(16.9698195535821,-20.122279639979,4.6383736307449));
#172393=CARTESIAN_POINT('Ctrl Pts',(17.06429528615,-20.2626654609611,4.62804424042255));
#172394=CARTESIAN_POINT('Ctrl Pts',(17.1647816944768,-20.3814384148935,
4.61801768707867));
#172395=CARTESIAN_POINT('Ctrl Pts',(17.3590117104694,-20.5656208243941,
4.60036158904024));
#172396=CARTESIAN_POINT('Ctrl Pts',(17.4467608782599,-20.636453150459,4.59287092259428));
#172397=CARTESIAN_POINT('Ctrl Pts',(17.5637595002678,-20.7163903003474,
4.58378140617193));
#172398=CARTESIAN_POINT('Ctrl Pts',(17.5881262370498,-20.7323116152937,
4.58193408903708));
#172399=CARTESIAN_POINT('Ctrl Pts',(17.6231389365486,-20.7541722558661,
4.57935189551883));
#172400=CARTESIAN_POINT('Ctrl Pts',(17.6335188495791,-20.7605293458116,
4.57859517006848));
#172401=CARTESIAN_POINT('Ctrl Pts',(17.6495558788656,-20.7701618909621,
4.57744015720231));
#172402=CARTESIAN_POINT('Ctrl Pts',(17.6551741228333,-20.7735011509362,
4.57703815948451));
#172403=CARTESIAN_POINT('Ctrl Pts',(17.6644973636086,-20.778984245074,4.57637552990331));
#172404=CARTESIAN_POINT('Ctrl Pts',(17.6681935141098,-20.781142929451,4.57611398885691));
#172405=CARTESIAN_POINT('Ctrl Pts',(17.6753592979093,-20.7852989092982,
4.57560920505075));
#172406=CARTESIAN_POINT('Ctrl Pts',(17.6788280964909,-20.787297600286,4.57536587445251));
#172407=CARTESIAN_POINT('Ctrl Pts',(17.6853320064863,-20.791020561042,4.57491158035356));
#172408=CARTESIAN_POINT('Ctrl Pts',(17.6883656789565,-20.7927471448914,
4.57470047235492));
#172409=CARTESIAN_POINT('Ctrl Pts',(17.6953670040798,-20.7967089845245,
4.57421506945905));
#172410=CARTESIAN_POINT('Ctrl Pts',(17.6993376008,-20.7989389427837,4.57394111666568));
#172411=CARTESIAN_POINT('Ctrl Pts',(17.711491303497,-20.8057131865469,4.57310652566121));
#172412=CARTESIAN_POINT('Ctrl Pts',(17.7196975057545,-20.8102160988045,
4.57254847128136));
#172413=CARTESIAN_POINT('Ctrl Pts',(17.7893103843811,-20.8478155623358,
4.5678582229013));
#172414=CARTESIAN_POINT('Ctrl Pts',(17.8522951891491,-20.8779163613929,
4.56390018414421));
#172415=CARTESIAN_POINT('Ctrl Pts',(18.0595667820946,-20.9646672314175,
4.55141655729296));
#172416=CARTESIAN_POINT('Ctrl Pts',(18.2086110102818,-21.0086136308057,
4.54321803304844));
#172417=CARTESIAN_POINT('Ctrl Pts',(18.4384407830901,-21.0497376837955,
4.53025828619843));
#172418=CARTESIAN_POINT('Ctrl Pts',(18.516462534563,-21.0592575011268,4.52581277617519));
#172419=CARTESIAN_POINT('Ctrl Pts',(18.6140626697009,-21.0656876860543,
4.5201045287648));
#172420=CARTESIAN_POINT('Ctrl Pts',(18.6333137505489,-21.066692138403,4.51897170862239));
#172421=CARTESIAN_POINT('Ctrl Pts',(18.6612089919008,-21.067765846773,4.51731923100289));
#172422=CARTESIAN_POINT('Ctrl Pts',(18.6698444313525,-21.0680452993421,
4.51680615627028));
#172423=CARTESIAN_POINT('Ctrl Pts',(18.684941803863,-21.0684413672396,4.51590639225528));
#172424=CARTESIAN_POINT('Ctrl Pts',(18.6914030507339,-21.068581268474,4.51552043768356));
#172425=CARTESIAN_POINT('Ctrl Pts',(18.703917197826,-21.0687949044309,4.5147711758953));
#172426=CARTESIAN_POINT('Ctrl Pts',(18.7099699792689,-21.0688722680718,
4.51440798631822));
#172427=CARTESIAN_POINT('Ctrl Pts',(18.7243874261361,-21.0689947018708,
4.51354096797064));
#172428=CARTESIAN_POINT('Ctrl Pts',(18.7327521432728,-21.0690161570091,
4.51303640365485));
#172429=CARTESIAN_POINT('Ctrl Pts',(18.7626368289217,-21.0689156937115,
4.51122812784682));
#172430=CARTESIAN_POINT('Ctrl Pts',(18.7841539744868,-21.0685152131365,
4.50991573833505));
#172431=CARTESIAN_POINT('Ctrl Pts',(18.9965843735425,-21.061320298692,4.49685197832337));
#172432=CARTESIAN_POINT('Ctrl Pts',(19.1857206933902,-21.0290414067206,
4.48424637383756));
#172433=CARTESIAN_POINT('Ctrl Pts',(19.4410388815917,-20.9489123845725,
4.46658973483107));
#172434=CARTESIAN_POINT('Ctrl Pts',(19.512869515398,-20.9220068351225,4.46156254636189));
#172435=CARTESIAN_POINT('Ctrl Pts',(19.6152121508221,-20.8771971407868,
4.45444673571601));
#172436=CARTESIAN_POINT('Ctrl Pts',(19.6469852845929,-20.8623342869692,
4.45224483594233));
#172437=CARTESIAN_POINT('Ctrl Pts',(19.6850057934403,-20.8433835800545,
4.44963159486516));
#172438=CARTESIAN_POINT('Ctrl Pts',(19.6916178345808,-20.8400444784696,
4.44917794123936));
#172439=CARTESIAN_POINT('Ctrl Pts',(19.7019036798692,-20.8347821592329,
4.44847365066999));
#172440=CARTESIAN_POINT('Ctrl Pts',(19.7055895148865,-20.8328827735597,
4.44822156158979));
#172441=CARTESIAN_POINT('Ctrl Pts',(19.7124359161086,-20.8293291887992,
4.44775387671116));
#172442=CARTESIAN_POINT('Ctrl Pts',(19.7155978504593,-20.8276778468827,
4.44753811186874));
#172443=CARTESIAN_POINT('Ctrl Pts',(19.722764064781,-20.8239121582036,4.44704961076768));
#172444=CARTESIAN_POINT('Ctrl Pts',(19.7267657345108,-20.8217929567438,
4.44677718577642));
#172445=CARTESIAN_POINT('Ctrl Pts',(19.7371070772479,-20.8162738375559,
4.4460740175249));
#172446=CARTESIAN_POINT('Ctrl Pts',(19.7434363348632,-20.8128543841525,
4.44564448243856));
#172447=CARTESIAN_POINT('Ctrl Pts',(19.7827708128028,-20.7913437428229,
4.44297945114501));
#172448=CARTESIAN_POINT('Ctrl Pts',(19.8153083216276,-20.7724060884381,
4.44079430449092));
#172449=CARTESIAN_POINT('Ctrl Pts',(19.9918623416976,-20.6632418768566,
4.42894868656502));
#172450=CARTESIAN_POINT('Ctrl Pts',(20.1251254953532,-20.5567890886888,
4.42000617243612));
#172451=CARTESIAN_POINT('Ctrl Pts',(20.3107781992903,-20.3677953346874,
4.40543016990868));
#172452=CARTESIAN_POINT('Ctrl Pts',(20.3726815773034,-20.2956612544309,
4.40010468937925));
#172453=CARTESIAN_POINT('Ctrl Pts',(20.4423084910402,-20.2025304762003,
4.39333330054994));
#172454=CARTESIAN_POINT('Ctrl Pts',(20.4548266656395,-20.1852477084033,
4.39208111542018));
#172455=CARTESIAN_POINT('Ctrl Pts',(20.4722503311395,-20.1604104452995,
4.39028641694498));
#172456=CARTESIAN_POINT('Ctrl Pts',(20.4773724369796,-20.1530089758969,
4.38975220026931));
#172457=CARTESIAN_POINT('Ctrl Pts',(20.486125853098,-20.1401862514727,4.38882762053508));
#172458=CARTESIAN_POINT('Ctrl Pts',(20.4897796137966,-20.1347804190083,
4.38843811564798));
#172459=CARTESIAN_POINT('Ctrl Pts',(20.4967266216542,-20.1243990184244,
4.38769060519103));
#172460=CARTESIAN_POINT('Ctrl Pts',(20.5000239434974,-20.1194262421892,
4.38733275824559));
#172461=CARTESIAN_POINT('Ctrl Pts',(20.5085413668962,-20.1064622324682,
4.38640037710397));
#172462=CARTESIAN_POINT('Ctrl Pts',(20.5137284798246,-20.0984495812965,
4.38582461579452));
#172463=CARTESIAN_POINT('Ctrl Pts',(20.5312210626313,-20.0710235705581,
4.38385544930948));
#172464=CARTESIAN_POINT('Ctrl Pts',(20.5432641432144,-20.0514455394227,
4.3824524023307));
#172465=CARTESIAN_POINT('Ctrl Pts',(20.6445550676644,-19.8806078581306,
4.37022777195926));
#172466=CARTESIAN_POINT('Ctrl Pts',(20.7149615076516,-19.7190079758745,
4.35870127227442));
#172467=CARTESIAN_POINT('Ctrl Pts',(20.789180103058,-19.4672456659107,4.34135943388337));
#172468=CARTESIAN_POINT('Ctrl Pts',(20.8086009619582,-19.3824371213776,
4.33563141146094));
#172469=CARTESIAN_POINT('Ctrl Pts',(20.8289075833434,-19.2593759109716,
4.32766841159355));
#172470=CARTESIAN_POINT('Ctrl Pts',(20.8340621234775,-19.2219207666357,
4.32529081759885));
#172471=CARTESIAN_POINT('Ctrl Pts',(20.839042052748,-19.1768205202957,4.3224986811117));
#172472=CARTESIAN_POINT('Ctrl Pts',(20.8398325609285,-19.1692913700373,
4.32203491438735));
#172473=CARTESIAN_POINT('Ctrl Pts',(20.8409970358603,-19.1575966428738,
4.32131839546422));
#172474=CARTESIAN_POINT('Ctrl Pts',(20.8413990669954,-19.1534340135387,
4.32106410990473));
#172475=CARTESIAN_POINT('Ctrl Pts',(20.8421208487724,-19.1457219329353,
4.32059442465788));
#172476=CARTESIAN_POINT('Ctrl Pts',(20.8424439689266,-19.1421728963991,
4.32037884293414));
#172477=CARTESIAN_POINT('Ctrl Pts',(20.8431530945784,-19.1341600862371,
4.31989337473308));
#172478=CARTESIAN_POINT('Ctrl Pts',(20.8435338914737,-19.1296959058606,
4.3196237833973));
#172479=CARTESIAN_POINT('Ctrl Pts',(20.8444763573567,-19.1182169271714,
4.31893274822383));
#172480=CARTESIAN_POINT('Ctrl Pts',(20.8450172319542,-19.1112004125795,
4.31851244417552));
#172481=CARTESIAN_POINT('Ctrl Pts',(20.848048910714,-19.0691356968986,4.31600450809082));
#172482=CARTESIAN_POINT('Ctrl Pts',(20.8497019886367,-19.0340304003715,
4.31396066853021));
#172483=CARTESIAN_POINT('Ctrl Pts',(20.8508317907905,-18.9830430664197,
4.31104263089572));
#172484=CARTESIAN_POINT('Ctrl Pts',(20.8510049507799,-18.9671843196658,
4.3101421031561));
#172485=CARTESIAN_POINT('Ctrl Pts',(20.8509917276277,-18.9257264327126,
4.30780306630794));
#172486=CARTESIAN_POINT('Ctrl Pts',(20.8505192678903,-18.9001296074882,
4.30637396114873));
#172487=CARTESIAN_POINT('Ctrl Pts',(20.847950390662,-18.8299622870072,4.30248318612837));
#172488=CARTESIAN_POINT('Ctrl Pts',(20.8449090787682,-18.7854390923712,
4.3000438789528));
#172489=CARTESIAN_POINT('Ctrl Pts',(20.829567578654,-18.6322491769349,4.29166191353768));
#172490=CARTESIAN_POINT('Ctrl Pts',(20.8102598944457,-18.5244628304246,
4.28577433985349));
#172491=CARTESIAN_POINT('Ctrl Pts',(20.7636477950918,-18.3454140539896,
4.2754866413596));
#172492=CARTESIAN_POINT('Ctrl Pts',(20.7406691328952,-18.2732556217367,
4.27119645027553));
#172493=CARTESIAN_POINT('Ctrl Pts',(20.7071891610852,-18.1848164968621,
4.26567544465709));
#172494=CARTESIAN_POINT('Ctrl Pts',(20.7002636503135,-18.1672368407426,
4.26456479443249));
#172495=CARTESIAN_POINT('Ctrl Pts',(20.689856181517,-18.1418215957923,4.26293886638913));
#172496=CARTESIAN_POINT('Ctrl Pts',(20.6865603448444,-18.1339104291894,
4.26242987456728));
#172497=CARTESIAN_POINT('Ctrl Pts',(20.6806993452425,-18.1200791597766,
4.26153484398041));
#172498=CARTESIAN_POINT('Ctrl Pts',(20.6781549711503,-18.1141503285822,
4.26114951645581));
#172499=CARTESIAN_POINT('Ctrl Pts',(20.6731630380808,-18.1026634391019,
4.26039967421896));
#172500=CARTESIAN_POINT('Ctrl Pts',(20.6707185834004,-18.0971040943756,
4.26003526867241));
#172501=CARTESIAN_POINT('Ctrl Pts',(20.6648198327366,-18.0838439032243,
4.25916245376206));
#172502=CARTESIAN_POINT('Ctrl Pts',(20.6613433584442,-18.0761530896946,
4.25865328614023));
#172503=CARTESIAN_POINT('Ctrl Pts',(20.6486448480703,-18.0485026074533,
4.25681193685448));
#172504=CARTESIAN_POINT('Ctrl Pts',(20.6391582333856,-18.0286666468042,
4.25547065783859));
#172505=CARTESIAN_POINT('Ctrl Pts',(20.546145041176,-17.8417200226915,4.24263097866432));
#172506=CARTESIAN_POINT('Ctrl Pts',(20.4411650382425,-17.6862390983626,
4.23032107809196));
#172507=CARTESIAN_POINT('Ctrl Pts',(20.2645139983812,-17.4872434911663,
4.21275533868005));
#172508=CARTESIAN_POINT('Ctrl Pts',(20.2085405373111,-17.4309093964385,
4.20754406201707));
#172509=CARTESIAN_POINT('Ctrl Pts',(20.1229033879014,-17.3539014600333,
4.20020386615802));
#172510=CARTESIAN_POINT('Ctrl Pts',(20.0956684954129,-17.3306330380802,
4.19795417072745));
#172511=CARTESIAN_POINT('Ctrl Pts',(20.0620669148646,-17.3033694112692,
4.19529212064689));
#172512=CARTESIAN_POINT('Ctrl Pts',(20.0562544412648,-17.2987039754446,
4.19483562144942));
#172513=CARTESIAN_POINT('Ctrl Pts',(20.0471622419283,-17.2914846576279,
4.19412788839423));
#172514=CARTESIAN_POINT('Ctrl Pts',(20.0438994953154,-17.2889096270083,
4.19387517973555));
#172515=CARTESIAN_POINT('Ctrl Pts',(20.0378233134293,-17.2841431462135,
4.19340693652406));
#172516=CARTESIAN_POINT('Ctrl Pts',(20.035011951709,-17.281949216596,4.19319122924798));
#172517=CARTESIAN_POINT('Ctrl Pts',(20.028629118394,-17.2769940822256,4.1927036105747));
#172518=CARTESIAN_POINT('Ctrl Pts',(20.025054359683,-17.2742371979377,4.19243200578278));
#172519=CARTESIAN_POINT('Ctrl Pts',(20.0144335225311,-17.2661003635453,
4.19162936538449));
#172520=CARTESIAN_POINT('Ctrl Pts',(20.0073623383546,-17.2607531370939,
4.19110058062748));
#172521=CARTESIAN_POINT('Ctrl Pts',(19.9544663864566,-17.2212730640029,
4.18718478482324));
#172522=CARTESIAN_POINT('Ctrl Pts',(19.9073057639961,-17.1889603693999,
4.18391425916349));
#172523=CARTESIAN_POINT('Ctrl Pts',(19.7306463782179,-17.0781530767405,
4.17222267625575));
#172524=CARTESIAN_POINT('Ctrl Pts',(19.5941380576055,-17.0116973506049,
4.16420735934564));
#172525=CARTESIAN_POINT('Ctrl Pts',(19.3644839877892,-16.9289395463648,
4.15076200706893));
#172526=CARTESIAN_POINT('Ctrl Pts',(19.2753058170039,-16.9032763010901,
4.14555622103287));
#172527=CARTESIAN_POINT('Ctrl Pts',(19.164153621561,-16.879055052733,4.13892974352589));
#172528=CARTESIAN_POINT('Ctrl Pts',(19.1435027078165,-16.8748768987773,
4.13769320972292));
#172529=CARTESIAN_POINT('Ctrl Pts',(19.1139907181514,-16.869363150666,4.13591709199079));
#172530=CARTESIAN_POINT('Ctrl Pts',(19.1051777878207,-16.8677744272367,
4.13538556879195));
#172531=CARTESIAN_POINT('Ctrl Pts',(19.0899347952602,-16.8651262887952,
4.13446417536122));
#172532=CARTESIAN_POINT('Ctrl Pts',(19.0835093862001,-16.8640405529589,
4.134075147376));
#172533=CARTESIAN_POINT('Ctrl Pts',(19.0711817164841,-16.8620159791263,
4.13332751709865));
#172534=CARTESIAN_POINT('Ctrl Pts',(19.065280284217,-16.8610724332035,4.13296906844586));
#172535=CARTESIAN_POINT('Ctrl Pts',(19.0498903628258,-16.8586786168554,
4.13203283314908));
#172536=CARTESIAN_POINT('Ctrl Pts',(19.0403959443273,-16.8572678798925,
4.13145379925986));
#172537=CARTESIAN_POINT('Ctrl Pts',(19.0078133147692,-16.8526528162177,
4.12946155524423));
#172538=CARTESIAN_POINT('Ctrl Pts',(18.9846825953532,-16.8497653561907,
4.12803839513612));
#172539=CARTESIAN_POINT('Ctrl Pts',(18.7917166869458,-16.8289069079813,
4.11608809178876));
#172540=CARTESIAN_POINT('Ctrl Pts',(18.6203570807412,-16.8311701841246,
4.10489910512723));
#172541=CARTESIAN_POINT('Ctrl Pts',(18.3616263041957,-16.866049274014,4.08764702233133));
#172542=CARTESIAN_POINT('Ctrl Pts',(18.2729426564417,-16.8838412239402,
4.08168385502502));
#172543=CARTESIAN_POINT('Ctrl Pts',(18.14832615013,-16.9172593734167,4.07344069870718));
#172544=CARTESIAN_POINT('Ctrl Pts',(18.1112679246029,-16.9282933824863,
4.07100780009328));
#172545=CARTESIAN_POINT('Ctrl Pts',(18.0672905502075,-16.9427101867487,
4.06815963979157));
#172546=CARTESIAN_POINT('Ctrl Pts',(18.0600637077912,-16.9451225941346,
4.06769287816026));
#172547=CARTESIAN_POINT('Ctrl Pts',(18.0488804313078,-16.9489229288312,
4.06697274127613));
#172548=CARTESIAN_POINT('Ctrl Pts',(18.0449149172585,-16.9502836549867,
4.0667178082477));
#172549=CARTESIAN_POINT('Ctrl Pts',(18.0375868535028,-16.9528225632225,
4.06624752257099));
#172550=CARTESIAN_POINT('Ctrl Pts',(18.0342232636899,-16.9539974439549,
4.06603198408222));
#172551=CARTESIAN_POINT('Ctrl Pts',(18.0266492713103,-16.9566644643807,
4.06554736103049));
#172552=CARTESIAN_POINT('Ctrl Pts',(18.022440628305,-16.9581614372078,4.06527856706043));
#172553=CARTESIAN_POINT('Ctrl Pts',(18.0101012168159,-16.9625944906925,
4.06449185677364));
#172554=CARTESIAN_POINT('Ctrl Pts',(18.0019835443578,-16.9655671057874,
4.06397606049243));
#172555=CARTESIAN_POINT('Ctrl Pts',(17.9455379723991,-16.9866299471171,
4.06040026212017));
#172556=CARTESIAN_POINT('Ctrl Pts',(17.8978632353713,-17.0064337440309,
4.05743505602116));
#172557=CARTESIAN_POINT('Ctrl Pts',(17.8310742020106,-17.0370868022155,
4.05329619037604));
#172558=CARTESIAN_POINT('Ctrl Pts',(17.8113344771107,-17.0465195014372,
4.05207490024794));
#172559=CARTESIAN_POINT('Ctrl Pts',(17.6684450276636,-17.1175409486336,
4.04322468535368));
#172560=CARTESIAN_POINT('Ctrl Pts',(17.5514166600587,-17.1907087962064,
4.03590132363251));
#172561=CARTESIAN_POINT('Ctrl Pts',(17.3704325636644,-17.3300859112174,
4.02330710303858));
#172562=CARTESIAN_POINT('Ctrl Pts',(17.3021868055151,-17.390004575054,4.01820660161727));
#172563=CARTESIAN_POINT('Ctrl Pts',(17.2232621157577,-17.4688297945207,
4.01170749855595));
#172564=CARTESIAN_POINT('Ctrl Pts',(17.2087435020694,-17.4837645341443,
4.01048487776013));
#172565=CARTESIAN_POINT('Ctrl Pts',(17.1883296413621,-17.5053930741443,
4.008725293793));
#172566=CARTESIAN_POINT('Ctrl Pts',(17.1822523792232,-17.5119139702028,
4.00819618446423));
#172567=CARTESIAN_POINT('Ctrl Pts',(17.1718088678202,-17.5232627128226,
4.00727764100022));
#172568=CARTESIAN_POINT('Ctrl Pts',(17.1674233376777,-17.5280727094266,
4.00688903489124));
#172569=CARTESIAN_POINT('Ctrl Pts',(17.1590478582533,-17.5373443611202,
4.00614127375467));
#172570=CARTESIAN_POINT('Ctrl Pts',(17.1550545057865,-17.5418028681897,
4.00578226784526));
#172571=CARTESIAN_POINT('Ctrl Pts',(17.1446737338493,-17.5534921869244,
4.00484248117269));
#172572=CARTESIAN_POINT('Ctrl Pts',(17.1383167963132,-17.5607497737066,
4.00426043453881));
#172573=CARTESIAN_POINT('Ctrl Pts',(17.1165780864919,-17.5859134085734,
4.00224711048491));
#172574=CARTESIAN_POINT('Ctrl Pts',(17.1014467666773,-17.604032607531,4.00080559830235));
#172575=CARTESIAN_POINT('Ctrl Pts',(16.9829321781835,-17.7508725516009,
3.98918379304907));
#172576=CARTESIAN_POINT('Ctrl Pts',(16.8946451434888,-17.8910100374429,
3.97838997399393));
#172577=CARTESIAN_POINT('Ctrl Pts',(16.7945495092901,-18.1006775466402,
3.9630363229136));
#172578=CARTESIAN_POINT('Ctrl Pts',(16.7684811701782,-18.1627309458507,
3.9585902818317));
#172579=CARTESIAN_POINT('Ctrl Pts',(16.7454192997072,-18.22588995433,3.95421655704364));
#172580=CARTESIAN_POINT('',(16.6170007560322,-18.9537891450234,4.48828854762057));
#172581=CARTESIAN_POINT('Ctrl Pts',(16.7454193692323,-18.2258897639231,
3.73234496387082));
#172582=CARTESIAN_POINT('Ctrl Pts',(16.7511301832802,-18.2102496949126,
3.73327488065988));
#172583=CARTESIAN_POINT('Ctrl Pts',(16.7570271353207,-18.1946725451317,
3.73420935406355));
#172584=CARTESIAN_POINT('Ctrl Pts',(16.7847361158326,-18.1240091654445,
3.73849006986507));
#172585=CARTESIAN_POINT('Ctrl Pts',(16.8086666864644,-18.0697929867798,
3.74189144374715));
#172586=CARTESIAN_POINT('Ctrl Pts',(16.8402460970562,-18.0056728844381,
3.74609042332773));
#172587=CARTESIAN_POINT('Ctrl Pts',(16.845749776351,-17.9947383126766,3.74681280679622));
#172588=CARTESIAN_POINT('Ctrl Pts',(16.8549744676129,-17.9768000542255,
3.7480086185687));
#172589=CARTESIAN_POINT('Ctrl Pts',(16.8586405983915,-17.9697683583884,
3.74848011584894));
#172590=CARTESIAN_POINT('Ctrl Pts',(16.8653238732181,-17.9571235546143,
3.74933302844374));
#172591=CARTESIAN_POINT('Ctrl Pts',(16.868327031592,-17.9515031324552,3.74971394448125));
#172592=CARTESIAN_POINT('Ctrl Pts',(16.8748001940854,-17.9395190777573,
3.75053006324578));
#172593=CARTESIAN_POINT('Ctrl Pts',(16.8782775882242,-17.9331595489891,
3.75096552618938));
#172594=CARTESIAN_POINT('Ctrl Pts',(16.8877881918118,-17.9159765906649,
3.7521486376987));
#172595=CARTESIAN_POINT('Ctrl Pts',(16.8938838125168,-17.9051881966121,
3.75289851812423));
#172596=CARTESIAN_POINT('Ctrl Pts',(16.9256758914823,-17.8500564706596,
3.75676757293195));
#172597=CARTESIAN_POINT('Ctrl Pts',(16.952879941276,-17.8066065098667,3.75994114551695));
#172598=CARTESIAN_POINT('Ctrl Pts',(17.0774339360714,-17.6228529769686,
3.77392295900185));
#172599=CARTESIAN_POINT('Ctrl Pts',(17.1899738781833,-17.4936414503088,
3.78529468825417));
#172600=CARTESIAN_POINT('Ctrl Pts',(17.3851490490077,-17.3177536136922,
3.80257302147171));
#172601=CARTESIAN_POINT('Ctrl Pts',(17.4574748256261,-17.2606550911788,
3.80854929244341));
#172602=CARTESIAN_POINT('Ctrl Pts',(17.5412586053927,-17.2029572777869,
3.81483427635308));
#172603=CARTESIAN_POINT('Ctrl Pts',(17.5492591618462,-17.1975281042186,
3.81542831630398));
#172604=CARTESIAN_POINT('Ctrl Pts',(17.5611326745739,-17.189589001078,3.81630059267153));
#172605=CARTESIAN_POINT('Ctrl Pts',(17.5649769617597,-17.1870367059999,
3.81658157771615));
#172606=CARTESIAN_POINT('Ctrl Pts',(17.5718145078082,-17.1825292703079,
3.81707876465126));
#172607=CARTESIAN_POINT('Ctrl Pts',(17.5748044015588,-17.1805691244846,
3.817295299682));
#172608=CARTESIAN_POINT('Ctrl Pts',(17.5812240080072,-17.1763837052268,
3.81775834497569));
#172609=CARTESIAN_POINT('Ctrl Pts',(17.5846551956961,-17.1741607959522,
3.81800469784223));
#172610=CARTESIAN_POINT('Ctrl Pts',(17.594098473366,-17.168081693519,3.81867964902525));
#172611=CARTESIAN_POINT('Ctrl Pts',(17.6001237367296,-17.1642459236454,
3.81910690840493));
#172612=CARTESIAN_POINT('Ctrl Pts',(17.6325052722027,-17.1438609337127,
3.82138566269506));
#172613=CARTESIAN_POINT('Ctrl Pts',(17.6592061315552,-17.1278629739202,
3.82320297959581));
#172614=CARTESIAN_POINT('Ctrl Pts',(17.828669100441,-17.0313418722698,3.83441818884811));
#172615=CARTESIAN_POINT('Ctrl Pts',(17.9800398963943,-16.967029414782,3.84307889885775));
#172616=CARTESIAN_POINT('Ctrl Pts',(18.2497877708956,-16.8877893531268,
3.8584682837578));
#172617=CARTESIAN_POINT('Ctrl Pts',(18.3647796710668,-16.8641546683099,
3.86501034560311));
#172618=CARTESIAN_POINT('Ctrl Pts',(18.495320101572,-16.8484493710478,3.87271293993901));
#172619=CARTESIAN_POINT('Ctrl Pts',(18.5095292598403,-16.8468857004034,
3.87355473483307));
#172620=CARTESIAN_POINT('Ctrl Pts',(18.5321672437503,-16.8446262683625,
3.87490168806475));
#172621=CARTESIAN_POINT('Ctrl Pts',(18.5405864386676,-16.8438368902243,
3.87540390262013));
#172622=CARTESIAN_POINT('Ctrl Pts',(18.5554424095455,-16.8425337450981,
3.87629241280931));
#172623=CARTESIAN_POINT('Ctrl Pts',(18.5618772661354,-16.8419989439007,
3.87667804194531));
#172624=CARTESIAN_POINT('Ctrl Pts',(18.575190856144,-16.840953758748,3.87747753669457));
#172625=CARTESIAN_POINT('Ctrl Pts',(18.5820698310345,-16.840447538212,3.87789152842497));
#172626=CARTESIAN_POINT('Ctrl Pts',(18.5997319976758,-16.8392345422098,
3.87895684676922));
#172627=CARTESIAN_POINT('Ctrl Pts',(18.6105182517222,-16.8385767042211,
3.87960970182205));
#172628=CARTESIAN_POINT('Ctrl Pts',(18.6555452815088,-16.8361764448126,
3.88234478481104));
#172629=CARTESIAN_POINT('Ctrl Pts',(18.6898192372429,-16.8351834505981,
3.88445032323934));
#172630=CARTESIAN_POINT('Ctrl Pts',(18.779160516857,-16.834765676957,3.890003538934));
#172631=CARTESIAN_POINT('Ctrl Pts',(18.8342053173157,-16.8366563573999,
3.89348957990565));
#172632=CARTESIAN_POINT('Ctrl Pts',(18.9981747663941,-16.8487026022327,
3.90405710903076));
#172633=CARTESIAN_POINT('Ctrl Pts',(19.1064469602738,-16.8651535644466,
3.91128699468513));
#172634=CARTESIAN_POINT('Ctrl Pts',(19.2565081710211,-16.9000074364045,
3.92146357345564));
#172635=CARTESIAN_POINT('Ctrl Pts',(19.2997315668984,-16.9115009825276,
3.92441189601922));
#172636=CARTESIAN_POINT('Ctrl Pts',(19.3667225176066,-16.9316070516135,
3.92898244550899));
#172637=CARTESIAN_POINT('Ctrl Pts',(19.3907547813336,-16.9392907119383,
3.93062222124833));
#172638=CARTESIAN_POINT('Ctrl Pts',(19.4618700859977,-16.9634373263618,
3.93546477987658));
#172639=CARTESIAN_POINT('Ctrl Pts',(19.5085184738595,-16.9811376585107,
3.9386285377538));
#172640=CARTESIAN_POINT('Ctrl Pts',(19.5617057801968,-17.0034997527569,
3.94218669676189));
#172641=CARTESIAN_POINT('Ctrl Pts',(19.5688931112473,-17.0065685390691,
3.94266645645164));
#172642=CARTESIAN_POINT('Ctrl Pts',(19.5803427049956,-17.0115323295886,
3.94342883181288));
#172643=CARTESIAN_POINT('Ctrl Pts',(19.5846159046973,-17.0134017079738,
3.94371294097046));
#172644=CARTESIAN_POINT('Ctrl Pts',(19.5921676674785,-17.0167351224768,
3.94421423354226));
#172645=CARTESIAN_POINT('Ctrl Pts',(19.5954487270417,-17.0181933956315,
3.94443176466584));
#172646=CARTESIAN_POINT('Ctrl Pts',(19.6023890469679,-17.0212992031604,
3.94489131804331));
#172647=CARTESIAN_POINT('Ctrl Pts',(19.6060473302649,-17.0229487932651,
3.94513321184596));
#172648=CARTESIAN_POINT('Ctrl Pts',(19.6158942044524,-17.0274226732447,
3.94578345080099));
#172649=CARTESIAN_POINT('Ctrl Pts',(19.62207397044,-17.0302664335541,3.94619061589417));
#172650=CARTESIAN_POINT('Ctrl Pts',(19.6524952180077,-17.0444435473644,
3.94819096148223));
#172651=CARTESIAN_POINT('Ctrl Pts',(19.6765352025799,-17.0562065966464,
3.94975909642348));
#172652=CARTESIAN_POINT('Ctrl Pts',(19.7451645107943,-17.0914160505706,
3.95421742905699));
#172653=CARTESIAN_POINT('Ctrl Pts',(19.7891502712375,-17.1160030276241,
3.95705221333874));
#172654=CARTESIAN_POINT('Ctrl Pts',(19.9451769745112,-17.2106796028815,
3.96717298649608));
#172655=CARTESIAN_POINT('Ctrl Pts',(20.0514718891016,-17.2896472539463,
3.97421153969132));
#172656=CARTESIAN_POINT('Ctrl Pts',(20.2269864681888,-17.4475127764653,
3.9871979813182));
#172657=CARTESIAN_POINT('Ctrl Pts',(20.2990259401707,-17.5226014672619,
3.9930368106686));
#172658=CARTESIAN_POINT('Ctrl Pts',(20.3742161951422,-17.6135017929218,
3.99994988500642));
#172659=CARTESIAN_POINT('Ctrl Pts',(20.3830679487324,-17.6244226939959,
4.00077790143366));
#172660=CARTESIAN_POINT('Ctrl Pts',(20.3970261455375,-17.6419987083217,
4.00210691562647));
#172661=CARTESIAN_POINT('Ctrl Pts',(20.4022030298426,-17.6485975321968,
4.00260509243156));
#172662=CARTESIAN_POINT('Ctrl Pts',(20.4112889860191,-17.660321941206,4.00348891078108));
#172663=CARTESIAN_POINT('Ctrl Pts',(20.4152141380485,-17.6654349721844,
4.0038739084213));
#172664=CARTESIAN_POINT('Ctrl Pts',(20.4233084165637,-17.6760791371702,
4.00467452378859));
#172665=CARTESIAN_POINT('Ctrl Pts',(20.4274738667817,-17.6816129584921,
4.00509027964009));
#172666=CARTESIAN_POINT('Ctrl Pts',(20.4381465875191,-17.6959374901244,
4.00616530969077));
#172667=CARTESIAN_POINT('Ctrl Pts',(20.4446129652035,-17.7047582845677,
4.00682616645467));
#172668=CARTESIAN_POINT('Ctrl Pts',(20.4717423031179,-17.7423733032411,
4.00963985230717));
#172669=CARTESIAN_POINT('Ctrl Pts',(20.4917478456482,-17.7716325443616,
4.01181770011623));
#172670=CARTESIAN_POINT('Ctrl Pts',(20.5423376118021,-17.8497629084138,
4.01760878776335));
#172671=CARTESIAN_POINT('Ctrl Pts',(20.5716749686063,-17.8994025921407,
4.02126461491021));
#172672=CARTESIAN_POINT('Ctrl Pts',(20.6748482200605,-18.091464709783,4.03530648712856));
#172673=CARTESIAN_POINT('Ctrl Pts',(20.7344376960959,-18.2409061446823,
4.04607429360625));
#172674=CARTESIAN_POINT('Ctrl Pts',(20.7803435580114,-18.4094395685974,
4.0574348272326));
#172675=CARTESIAN_POINT('Ctrl Pts',(20.7839643612777,-18.4232846601414,
4.05836215204823));
#172676=CARTESIAN_POINT('Ctrl Pts',(20.7900696933786,-18.4476361054248,
4.05998165332226));
#172677=CARTESIAN_POINT('Ctrl Pts',(20.7926147433524,-18.4581266683209,
4.06067560310594));
#172678=CARTESIAN_POINT('Ctrl Pts',(20.8043550495345,-18.5081877484977,
4.06396805562113));
#172679=CARTESIAN_POINT('Ctrl Pts',(20.8124909508737,-18.5480009789565,
4.06652999704423));
#172680=CARTESIAN_POINT('Ctrl Pts',(20.8207425767955,-18.5952807202378,
4.0694869495392));
#172681=CARTESIAN_POINT('Ctrl Pts',(20.8219707990689,-18.6025416015748,
4.06993868969426));
#172682=CARTESIAN_POINT('Ctrl Pts',(20.8239013892064,-18.6143283296685,
4.0706680086335));
#172683=CARTESIAN_POINT('Ctrl Pts',(20.8246269892519,-18.6188502344688,
4.07094685440025));
#172684=CARTESIAN_POINT('Ctrl Pts',(20.8258923568697,-18.6269029003023,
4.07144168781869));
#172685=CARTESIAN_POINT('Ctrl Pts',(20.8264378675351,-18.6304327004786,
4.07165799675415));
#172686=CARTESIAN_POINT('Ctrl Pts',(20.8275920133439,-18.6380280584882,
4.07212215647192));
#172687=CARTESIAN_POINT('Ctrl Pts',(20.8281977392569,-18.6420940014357,
4.07236984145998));
#172688=CARTESIAN_POINT('Ctrl Pts',(20.8298382348117,-18.65333032011,4.0730522100572));
#172689=CARTESIAN_POINT('Ctrl Pts',(20.8308480583633,-18.6605043606289,
4.07348550535171));
#172690=CARTESIAN_POINT('Ctrl Pts',(20.8361967042274,-18.6999691975279,
4.07585673303363));
#172691=CARTESIAN_POINT('Ctrl Pts',(20.8398267298088,-18.7323535666501,
4.07775711901633));
#172692=CARTESIAN_POINT('Ctrl Pts',(20.8570892017347,-18.92681727768,4.08896587802496));
#172693=CARTESIAN_POINT('Ctrl Pts',(20.8527546651832,-19.0899580453236,
4.09756266631738));
#172694=CARTESIAN_POINT('Ctrl Pts',(20.8132771506168,-19.3666607797021,
4.1128641864491));
#172695=CARTESIAN_POINT('Ctrl Pts',(20.7872343545411,-19.4807347696848,
4.11938601378332));
#172696=CARTESIAN_POINT('Ctrl Pts',(20.7475989285466,-19.6056914830379,
4.12706583117076));
#172697=CARTESIAN_POINT('Ctrl Pts',(20.7431406986708,-19.6192681905171,
4.12790733665854));
#172698=CARTESIAN_POINT('Ctrl Pts',(20.7358265267352,-19.6408040641056,
4.12925391330786));
#172699=CARTESIAN_POINT('Ctrl Pts',(20.7330597085465,-19.6487931977078,
4.12975604329215));
#172700=CARTESIAN_POINT('Ctrl Pts',(20.7280956111988,-19.6628539822056,
4.130644454966));
#172701=CARTESIAN_POINT('Ctrl Pts',(20.7259182590846,-19.6689325898016,
4.13103007063195));
#172702=CARTESIAN_POINT('Ctrl Pts',(20.7213572721845,-19.6814845150261,
4.131829587642));
#172703=CARTESIAN_POINT('Ctrl Pts',(20.7189697402013,-19.6879563259464,
4.1322436153506));
#172704=CARTESIAN_POINT('Ctrl Pts',(20.7127600158151,-19.7045387921159,
4.13330913198197));
#172705=CARTESIAN_POINT('Ctrl Pts',(20.7088919767256,-19.7146319605857,
4.1339621504423));
#172706=CARTESIAN_POINT('Ctrl Pts',(20.6924245296528,-19.7566362010405,
4.13669881683496));
#172707=CARTESIAN_POINT('Ctrl Pts',(20.6791282008865,-19.7882667756943,
4.13880580902997));
#172708=CARTESIAN_POINT('Ctrl Pts',(20.6424846364209,-19.8698304339781,
4.14436377314599));
#172709=CARTESIAN_POINT('Ctrl Pts',(20.6179467356701,-19.9191970786531,
4.14785319061943));
#172710=CARTESIAN_POINT('Ctrl Pts',(20.5390317512022,-20.0635385596571,
4.15842720592655));
#172711=CARTESIAN_POINT('Ctrl Pts',(20.4791925194379,-20.15531093108,4.16566017969358));
#172712=CARTESIAN_POINT('Ctrl Pts',(20.3828537962609,-20.2806620365107,
4.176103493032));
#172713=CARTESIAN_POINT('Ctrl Pts',(20.3518464901503,-20.3182483759927,
4.17931472136264));
#172714=CARTESIAN_POINT('Ctrl Pts',(20.3080707575026,-20.3677299911857,
4.18362416080086));
#172715=CARTESIAN_POINT('Ctrl Pts',(20.2964123899318,-20.3805859108204,
4.18475165787128));
#172716=CARTESIAN_POINT('Ctrl Pts',(20.2482575777891,-20.4323925099416,
4.18932303072838));
#172717=CARTESIAN_POINT('Ctrl Pts',(20.2104490714907,-20.4701031496099,
4.19271619582484));
#172718=CARTESIAN_POINT('Ctrl Pts',(20.1648482747888,-20.5122686586665,
4.19654748053733));
#172719=CARTESIAN_POINT('Ctrl Pts',(20.1584077585188,-20.5181505726358,
4.19708280915994));
#172720=CARTESIAN_POINT('Ctrl Pts',(20.1486016335192,-20.5269956574417,
4.1978889126663));
#172721=CARTESIAN_POINT('Ctrl Pts',(20.1452627515513,-20.5299881334962,
4.19816182552491));
#172722=CARTESIAN_POINT('Ctrl Pts',(20.1392528137062,-20.5353402133521,
4.19865023694286));
#172723=CARTESIAN_POINT('Ctrl Pts',(20.1365852956949,-20.5377036893859,
4.19886602378302));
#172724=CARTESIAN_POINT('Ctrl Pts',(20.1307765613152,-20.5428242220714,
4.19933375530113));
#172725=CARTESIAN_POINT('Ctrl Pts',(20.1276331552509,-20.5455787075157,
4.19958550908801));
#172726=CARTESIAN_POINT('Ctrl Pts',(20.1187818434445,-20.5532886629269,
4.20029066479879));
#172727=CARTESIAN_POINT('Ctrl Pts',(20.1130554585783,-20.5582229552659,
4.20074252173185));
#172728=CARTESIAN_POINT('Ctrl Pts',(20.0786891501913,-20.5875163356939,
4.20342930969765));
#172729=CARTESIAN_POINT('Ctrl Pts',(20.0494289484576,-20.6111412445241,
4.20561392778844));
#172730=CARTESIAN_POINT('Ctrl Pts',(19.9511263783463,-20.6862750047007,
4.21267968183811));
#172731=CARTESIAN_POINT('Ctrl Pts',(19.8795663476027,-20.7343542018459,
4.21739797804719));
#172732=CARTESIAN_POINT('Ctrl Pts',(19.652829988649,-20.8673792323252,4.23170432042636));
#172733=CARTESIAN_POINT('Ctrl Pts',(19.4898086759238,-20.9373646409992,
4.24120007847877));
#172734=CARTESIAN_POINT('Ctrl Pts',(19.2979887004385,-20.9926200220358,
4.25280076814476));
#172735=CARTESIAN_POINT('Ctrl Pts',(19.2758844677203,-20.9986007163114,
4.25414235637142));
#172736=CARTESIAN_POINT('Ctrl Pts',(19.2444489369933,-21.0065611990252,
4.25605878434435));
#172737=CARTESIAN_POINT('Ctrl Pts',(19.2351941095054,-21.0088384228955,
4.25662402395593));
#172738=CARTESIAN_POINT('Ctrl Pts',(19.2201234937752,-21.0124389142055,
4.25754625447383));
#172739=CARTESIAN_POINT('Ctrl Pts',(19.2143168695668,-21.0138002507666,
4.25790201526899));
#172740=CARTESIAN_POINT('Ctrl Pts',(19.2021436046721,-21.0166000019803,
4.25864878230591));
#172741=CARTESIAN_POINT('Ctrl Pts',(19.1957759178932,-21.0180335435189,
4.25903994087415));
#172742=CARTESIAN_POINT('Ctrl Pts',(19.1805993514443,-21.0213765392341,
4.25997353223949));
#172743=CARTESIAN_POINT('Ctrl Pts',(19.1717847600478,-21.0232592164636,
4.26051681712549));
#172744=CARTESIAN_POINT('Ctrl Pts',(19.1419896847806,-21.029424351108,4.26235692391388));
#172745=CARTESIAN_POINT('Ctrl Pts',(19.1209568613373,-21.0334446550569,
4.26366207199765));
#172746=CARTESIAN_POINT('Ctrl Pts',(19.0707415851066,-21.0422556128637,
4.26679375978029));
#172747=CARTESIAN_POINT('Ctrl Pts',(19.0415132385426,-21.0467550916538,
4.26862915598807));
#172748=CARTESIAN_POINT('Ctrl Pts',(18.843318555189,-21.0730283001473,4.28116187296321));
#172749=CARTESIAN_POINT('Ctrl Pts',(18.6723714835105,-21.0749450630205,
4.29247109123198));
#172750=CARTESIAN_POINT('Ctrl Pts',(18.4039127858904,-21.0454860698564,
4.3102647913417));
#172751=CARTESIAN_POINT('Ctrl Pts',(18.3056266028396,-21.0276065267998,
4.31676753280609));
#172752=CARTESIAN_POINT('Ctrl Pts',(18.19956691186,-21.0004541132151,4.3235317165698));
#172753=CARTESIAN_POINT('Ctrl Pts',(18.1901919011292,-20.9979852735181,
4.32412736630247));
#172754=CARTESIAN_POINT('Ctrl Pts',(18.1763750908517,-20.9942450389934,
4.32500154581603));
#172755=CARTESIAN_POINT('Ctrl Pts',(18.1719201170092,-20.9930234062026,
4.32528284120623));
#172756=CARTESIAN_POINT('Ctrl Pts',(18.1640238970266,-20.9908303086036,
4.3257803710753));
#172757=CARTESIAN_POINT('Ctrl Pts',(18.1605810812025,-20.989864698523,4.32599694041291));
#172758=CARTESIAN_POINT('Ctrl Pts',(18.1532101339695,-20.9877772028319,
4.32645983097572));
#172759=CARTESIAN_POINT('Ctrl Pts',(18.14928280938,-20.9866526720047,4.32670599599692));
#172760=CARTESIAN_POINT('Ctrl Pts',(18.1385117459141,-20.983534776636,4.32737990272118));
#172761=CARTESIAN_POINT('Ctrl Pts',(18.1316747085127,-20.9815181832054,
4.32780631237714));
#172762=CARTESIAN_POINT('Ctrl Pts',(18.0952340843999,-20.9705696040853,
4.33007240364837));
#172763=CARTESIAN_POINT('Ctrl Pts',(18.0658170093122,-20.9610238573582,
4.33187835544342));
#172764=CARTESIAN_POINT('Ctrl Pts',(17.9774236090361,-20.9301839300038,
4.33726331477463));
#172765=CARTESIAN_POINT('Ctrl Pts',(17.9191714013096,-20.9069104837852,
4.34075559236385));
#172766=CARTESIAN_POINT('Ctrl Pts',(17.7219706492996,-20.8177737363914,
4.35264919877123));
#172767=CARTESIAN_POINT('Ctrl Pts',(17.5892223540265,-20.7394002591372,
4.36081661047618));
#172768=CARTESIAN_POINT('Ctrl Pts',(17.4622379180975,-20.6444342844427,
4.36970909216085));
#172769=CARTESIAN_POINT('Ctrl Pts',(17.4583575640986,-20.6415114605778,
4.36998191255556));
#172770=CARTESIAN_POINT('Ctrl Pts',(17.4040558575116,-20.6003157184154,
4.37381531857891));
#172771=CARTESIAN_POINT('Ctrl Pts',(17.3553698866704,-20.5598165391312,
4.3774424392865));
#172772=CARTESIAN_POINT('Ctrl Pts',(17.2993257549232,-20.5087772114836,
4.38189394341832));
#172773=CARTESIAN_POINT('Ctrl Pts',(17.2901522188873,-20.500272925101,4.38263190214923));
#172774=CARTESIAN_POINT('Ctrl Pts',(17.2752274191951,-20.4861889565102,
4.3838482227587));
#172775=CARTESIAN_POINT('Ctrl Pts',(17.2694314319325,-20.4806569607065,
4.38432453625511));
#172776=CARTESIAN_POINT('Ctrl Pts',(17.2590770460138,-20.4706612465413,
4.38518268437635));
#172777=CARTESIAN_POINT('Ctrl Pts',(17.2545071364174,-20.4662095519354,
4.38556399268506));
#172778=CARTESIAN_POINT('Ctrl Pts',(17.2456932590751,-20.4575456811477,
4.38630443929746));
#172779=CARTESIAN_POINT('Ctrl Pts',(17.2414468729001,-20.4533360432453,
4.38666346397012));
#172780=CARTESIAN_POINT('Ctrl Pts',(17.2299422995142,-20.4418339820608,
4.38764244842814));
#172781=CARTESIAN_POINT('Ctrl Pts',(17.2227194195755,-20.434506614445,4.38826395895046));
#172782=CARTESIAN_POINT('Ctrl Pts',(17.1934248661666,-20.404351715827,4.39081324186662));
#172783=CARTESIAN_POINT('Ctrl Pts',(17.1718156123648,-20.3810825786974,
4.39276089049446));
#172784=CARTESIAN_POINT('Ctrl Pts',(17.1176145239884,-20.3200193095613,
4.39782554201291));
#172785=CARTESIAN_POINT('Ctrl Pts',(17.0858223367537,-20.2815445116243,
4.40097335656107));
#172786=CARTESIAN_POINT('Ctrl Pts',(17.0102400644393,-20.1831938779723,
4.40891138223178));
#172787=CARTESIAN_POINT('Ctrl Pts',(16.9681822759228,-20.1220739429574,
4.41375216312812));
#172788=CARTESIAN_POINT('Ctrl Pts',(16.8493472984656,-19.9283332935157,
4.42872202418659));
#172789=CARTESIAN_POINT('Ctrl Pts',(16.7836721142417,-19.7894782272955,
4.43897491950335));
#172790=CARTESIAN_POINT('Ctrl Pts',(16.7284957728217,-19.6301449193315,
4.44949009207163));
#172791=CARTESIAN_POINT('Ctrl Pts',(16.7235995346047,-19.6154890635135,
4.45044585903614));
#172792=CARTESIAN_POINT('Ctrl Pts',(16.7171006642882,-19.5953033326114,
4.4517453404905));
#172793=CARTESIAN_POINT('Ctrl Pts',(16.7153596043772,-19.5898189892765,
4.45209669915286));
#172794=CARTESIAN_POINT('Ctrl Pts',(16.7126241720105,-19.5810789688052,
4.45265385178579));
#172795=CARTESIAN_POINT('Ctrl Pts',(16.7116152688895,-19.5778279210169,
4.45286048602846));
#172796=CARTESIAN_POINT('Ctrl Pts',(16.7095441627949,-19.5710967633095,
4.45328702903049));
#172797=CARTESIAN_POINT('Ctrl Pts',(16.7084830894302,-19.5676163450457,
4.4535068657369));
#172798=CARTESIAN_POINT('Ctrl Pts',(16.7059703329421,-19.5592974456252,
4.45403065433402));
#172799=CARTESIAN_POINT('Ctrl Pts',(16.7045269733107,-19.5544564325111,
4.45433412059053));
#172800=CARTESIAN_POINT('Ctrl Pts',(16.6996912606082,-19.5380229049513,
4.45535988124939));
#172801=CARTESIAN_POINT('Ctrl Pts',(16.696380723361,-19.5264062944156,4.45607756586052));
#172802=CARTESIAN_POINT('Ctrl Pts',(16.6886498163706,-19.4983705029819,
4.45779325489078));
#172803=CARTESIAN_POINT('Ctrl Pts',(16.6843274150554,-19.4819249306869,
4.45878621140754));
#172804=CARTESIAN_POINT('Ctrl Pts',(16.6687721240632,-19.4197012718665,
4.46249872608696));
#172805=CARTESIAN_POINT('Ctrl Pts',(16.6588703556768,-19.3736019354585,
4.46515906019934));
#172806=CARTESIAN_POINT('Ctrl Pts',(16.6283221911304,-19.2039715288572,
4.47474467089376));
#172807=CARTESIAN_POINT('Ctrl Pts',(16.6171065839709,-19.0790096628014,
4.48142927135385));
#172808=CARTESIAN_POINT('Ctrl Pts',(16.6170007560322,-18.9537891450234,
4.48828854762057));
#172809=CARTESIAN_POINT('Ctrl Pts',(16.6170007544017,-18.9537872147055,
4.48828865335871));
#172810=CARTESIAN_POINT('Ctrl Pts',(16.6169304739052,-18.8705382588802,
4.49284883024313));
#172811=CARTESIAN_POINT('Ctrl Pts',(16.6217706707422,-18.7873622863883,
4.49747291987405));
#172812=CARTESIAN_POINT('Ctrl Pts',(16.6354867574308,-18.6707551618226,
4.5041975533329));
#172813=CARTESIAN_POINT('Ctrl Pts',(16.6402991570916,-18.6369236936205,
4.50617710222748));
#172814=CARTESIAN_POINT('Ctrl Pts',(16.6476157990064,-18.5931199034441,
4.50878346471332));
#172815=CARTESIAN_POINT('Ctrl Pts',(16.6493769494046,-18.5830275223217,
4.50938696765868));
#172816=CARTESIAN_POINT('Ctrl Pts',(16.6524781169082,-18.5659874210792,
4.51041117473668));
#172817=CARTESIAN_POINT('Ctrl Pts',(16.6537798486759,-18.5590328499048,
4.51083066560809));
#172818=CARTESIAN_POINT('Ctrl Pts',(16.6564245881202,-18.5452846648746,
4.51166293212674));
#172819=CARTESIAN_POINT('Ctrl Pts',(16.6577661161461,-18.5384908542017,
4.51207565605965));
#172820=CARTESIAN_POINT('Ctrl Pts',(16.6604207784662,-18.5253856910209,
4.51287464746878));
#172821=CARTESIAN_POINT('Ctrl Pts',(16.6617294562935,-18.5190735063975,
4.51326076834749));
#172822=CARTESIAN_POINT('Ctrl Pts',(16.6648077475785,-18.5045597021983,
4.51415158331865));
#172823=CARTESIAN_POINT('Ctrl Pts',(16.6665973215928,-18.4963624689217,
4.51465691248745));
#172824=CARTESIAN_POINT('Ctrl Pts',(16.6715178729829,-18.4744495882456,
4.51601377176292));
#172825=CARTESIAN_POINT('Ctrl Pts',(16.6747368802982,-18.4607543294126,
4.51686811537757));
#172826=CARTESIAN_POINT('Ctrl Pts',(16.6964948318064,-18.3721592143423,
4.52243687221738));
#172827=CARTESIAN_POINT('Ctrl Pts',(16.7189735909982,-18.2983161719576,
4.52727680159809));
#172828=CARTESIAN_POINT('Ctrl Pts',(16.7454193964829,-18.2258896892926,
4.53222340662745));
#172829=CARTESIAN_POINT('Origin',(18.734,-18.952,0.));
#172830=CARTESIAN_POINT('',(16.7454193466937,-18.2258898256491,5.55626851740655));
#172831=CARTESIAN_POINT('',(16.7454193844609,-18.2258897222169,5.33540091855302));
#172832=CARTESIAN_POINT('',(16.7454193692319,-18.2258897639242,0.));
#172833=CARTESIAN_POINT('Ctrl Pts',(16.7454193466937,-18.2258898256491,
5.55626851740655));
#172834=CARTESIAN_POINT('Ctrl Pts',(16.7359008843311,-18.2519578119853,
5.55474535788985));
#172835=CARTESIAN_POINT('Ctrl Pts',(16.7268931576281,-18.2782180124468,
5.55321402945697));
#172836=CARTESIAN_POINT('Ctrl Pts',(16.6925866539401,-18.3850361381322,
5.54697988874858));
#172837=CARTESIAN_POINT('Ctrl Pts',(16.6716050349134,-18.4668803814372,
5.54218747913845));
#172838=CARTESIAN_POINT('Ctrl Pts',(16.6528673380296,-18.5636990438631,
5.53639853261415));
#172839=CARTESIAN_POINT('Ctrl Pts',(16.6503087149706,-18.5776720646127,
5.53556032075485));
#172840=CARTESIAN_POINT('Ctrl Pts',(16.6465902594023,-18.5991998131029,
5.53426430419031));
#172841=CARTESIAN_POINT('Ctrl Pts',(16.645330360663,-18.6067370098265,5.53380968308545));
#172842=CARTESIAN_POINT('Ctrl Pts',(16.643106864088,-18.6204965478617,5.53297810679902));
#172843=CARTESIAN_POINT('Ctrl Pts',(16.642130161454,-18.6267167052547,5.53260157251945));
#172844=CARTESIAN_POINT('Ctrl Pts',(16.6400580228059,-18.6403085853967,
5.53177742293717));
#172845=CARTESIAN_POINT('Ctrl Pts',(16.6389737391432,-18.6476819001443,
5.53132945929608));
#172846=CARTESIAN_POINT('Ctrl Pts',(16.6361094454989,-18.6679007286344,
5.530098589618));
#172847=CARTESIAN_POINT('Ctrl Pts',(16.6344085221732,-18.6807569555613,
5.52931319511429));
#172848=CARTESIAN_POINT('Ctrl Pts',(16.6263685192506,-18.7461410985298,
5.52530435191713));
#172849=CARTESIAN_POINT('Ctrl Pts',(16.6218825840024,-18.7988739559501,
5.52202307361011));
#172850=CARTESIAN_POINT('Ctrl Pts',(16.6177663610352,-18.885670091598,5.51653981045079));
#172851=CARTESIAN_POINT('Ctrl Pts',(16.6169742107339,-18.91965658388,5.51437225302693));
#172852=CARTESIAN_POINT('Ctrl Pts',(16.6171022078418,-19.0842687455959,
5.5037810395224));
#172853=CARTESIAN_POINT('Ctrl Pts',(16.6292932821579,-19.2145944755365,
5.49508949971731));
#172854=CARTESIAN_POINT('Ctrl Pts',(16.6709615190644,-19.4363469018122,
5.48023959087602));
#172855=CARTESIAN_POINT('Ctrl Pts',(16.6947819163944,-19.5284664524788,
5.47405980222472));
#172856=CARTESIAN_POINT('Ctrl Pts',(16.727765752138,-19.6278749492191,5.46758873518461));
#172857=CARTESIAN_POINT('Ctrl Pts',(16.7308789343071,-19.6370465740627,
5.46699364833627));
#172858=CARTESIAN_POINT('Ctrl Pts',(16.7355692047997,-19.6505590019216,
5.46612013419701));
#172859=CARTESIAN_POINT('Ctrl Pts',(16.7370976766823,-19.6549163779793,
5.46583894724034));
#172860=CARTESIAN_POINT('Ctrl Pts',(16.7398349366883,-19.6626387860223,
5.46534153720036));
#172861=CARTESIAN_POINT('Ctrl Pts',(16.7410380035872,-19.6660057881174,
5.465124979859));
#172862=CARTESIAN_POINT('Ctrl Pts',(16.7436342810792,-19.6732142552974,
5.46466203532028));
#172863=CARTESIAN_POINT('Ctrl Pts',(16.7450300811399,-19.6770547287055,
5.46441580474307));
#172864=CARTESIAN_POINT('Ctrl Pts',(16.7488929553554,-19.6875881335771,
5.46374153367509));
#172865=CARTESIAN_POINT('Ctrl Pts',(16.7513827766128,-19.6942727462213,
5.46331482763278));
#172866=CARTESIAN_POINT('Ctrl Pts',(16.7648702439157,-19.7299315152197,
5.46104432982681));
#172867=CARTESIAN_POINT('Ctrl Pts',(16.7764699573688,-19.758675770873,5.45923442348496));
#172868=CARTESIAN_POINT('Ctrl Pts',(16.8532264206235,-19.9374620610696,
5.44804383693206));
#172869=CARTESIAN_POINT('Ctrl Pts',(16.9349648030108,-20.07979849345,5.4393986993646));
#172870=CARTESIAN_POINT('Ctrl Pts',(17.1022876526277,-20.3059020269329,
5.42400418916545));
#172871=CARTESIAN_POINT('Ctrl Pts',(17.1800410560598,-20.3944777785986,
5.41743777573114));
#172872=CARTESIAN_POINT('Ctrl Pts',(17.2750386715052,-20.486055197147,5.40970777271542));
#172873=CARTESIAN_POINT('Ctrl Pts',(17.2854344387419,-20.4958754178144,
5.40886564583278));
#172874=CARTESIAN_POINT('Ctrl Pts',(17.3021355842578,-20.5113347393207,
5.40751826057675));
#172875=CARTESIAN_POINT('Ctrl Pts',(17.3083767585881,-20.5170427804698,
5.40701594897468));
#172876=CARTESIAN_POINT('Ctrl Pts',(17.3194429387323,-20.527042544702,5.4061273256713));
#172877=CARTESIAN_POINT('Ctrl Pts',(17.324253717047,-20.531349902168,5.40574168101176));
#172878=CARTESIAN_POINT('Ctrl Pts',(17.3342433771475,-20.5402121912422,
5.40494221158013));
#172879=CARTESIAN_POINT('Ctrl Pts',(17.339424956335,-20.5447639540953,5.4045282609742));
#172880=CARTESIAN_POINT('Ctrl Pts',(17.3527797536973,-20.5563803605167,
5.40346316950663));
#172881=CARTESIAN_POINT('Ctrl Pts',(17.3609849003692,-20.5634078439113,
5.40281050146319));
#172882=CARTESIAN_POINT('Ctrl Pts',(17.3954326820626,-20.5924573056214,
5.40007723009742));
#172883=CARTESIAN_POINT('Ctrl Pts',(17.4221529410106,-20.613902438357,5.39797335489242));
#172884=CARTESIAN_POINT('Ctrl Pts',(17.4930984155857,-20.6680645208865,
5.39242557024259));
#172885=CARTESIAN_POINT('Ctrl Pts',(17.5380970725674,-20.6997212459683,
5.38894339058952));
#172886=CARTESIAN_POINT('Ctrl Pts',(17.6611867388643,-20.7793343759979,
5.37952162449786));
#172887=CARTESIAN_POINT('Ctrl Pts',(17.7412415107427,-20.8240330014683,
5.37349486871033));
#172888=CARTESIAN_POINT('Ctrl Pts',(17.8723921801402,-20.8864770904454,
5.36389706536462));
#172889=CARTESIAN_POINT('Ctrl Pts',(17.921712036845,-20.9076988725713,5.36034702183442));
#172890=CARTESIAN_POINT('Ctrl Pts',(18.0061637171794,-20.9402910298159,
5.35441155329808));
#172891=CARTESIAN_POINT('Ctrl Pts',(18.0408836779819,-20.9526591030056,
5.35201099068368));
#172892=CARTESIAN_POINT('Ctrl Pts',(18.1208910951545,-20.9788266329332,
5.34659306904659));
#172893=CARTESIAN_POINT('Ctrl Pts',(18.1663567646846,-20.9920271172026,
5.34359566530302));
#172894=CARTESIAN_POINT('Ctrl Pts',(18.2196964179984,-21.0055920172991,
5.34020231494323));
#172895=CARTESIAN_POINT('Ctrl Pts',(18.2271729697419,-21.0074500026783,
5.33972945975241));
#172896=CARTESIAN_POINT('Ctrl Pts',(18.2391605365535,-21.0103596277329,
5.33897594524377));
#172897=CARTESIAN_POINT('Ctrl Pts',(18.2436650691388,-21.011437328054,5.33869384535696));
#172898=CARTESIAN_POINT('Ctrl Pts',(18.2516635997707,-21.0133232297586,
5.33819483045165));
#172899=CARTESIAN_POINT('Ctrl Pts',(18.2551561565076,-21.0141373462514,
5.33797757859747));
#172900=CARTESIAN_POINT('Ctrl Pts',(18.262579167711,-21.015847777812,5.33751721362111));
#172901=CARTESIAN_POINT('Ctrl Pts',(18.2665101097136,-21.0167417403152,
5.3372742361178));
#172902=CARTESIAN_POINT('Ctrl Pts',(18.2771614480846,-21.0191320566201,
5.33661800488184));
#172903=CARTESIAN_POINT('Ctrl Pts',(18.2838866969936,-21.020606878905,5.33620596894611));
#172904=CARTESIAN_POINT('Ctrl Pts',(18.3177561661862,-21.0278613330994,
5.3341419411297));
#172905=CARTESIAN_POINT('Ctrl Pts',(18.3450063639415,-21.0331399092261,
5.33251695090472));
#172906=CARTESIAN_POINT('Ctrl Pts',(18.4247475690468,-21.0469652849544,
5.32784471454025));
#172907=CARTESIAN_POINT('Ctrl Pts',(18.4774685848287,-21.0540725528601,
5.3248594438555));
#172908=CARTESIAN_POINT('Ctrl Pts',(18.6705343316279,-21.0727264684781,
5.31412794462035));
#172909=CARTESIAN_POINT('Ctrl Pts',(18.8116660994787,-21.0722544315329,
5.30664406807786));
#172910=CARTESIAN_POINT('Ctrl Pts',(19.0430844231071,-21.0483287866107,
5.29377488274038));
#172911=CARTESIAN_POINT('Ctrl Pts',(19.1337369952539,-21.0329456755309,
5.28858388886549));
#172912=CARTESIAN_POINT('Ctrl Pts',(19.2364887274002,-21.0085465017107,
5.28239265087972));
#172913=CARTESIAN_POINT('Ctrl Pts',(19.2498483281825,-21.00523620751,5.28158172383808));
#172914=CARTESIAN_POINT('Ctrl Pts',(19.2712120751727,-20.9997209514359,
5.28027498800694));
#172915=CARTESIAN_POINT('Ctrl Pts',(19.2792373173305,-20.9975987322678,
5.27978185124187));
#172916=CARTESIAN_POINT('Ctrl Pts',(19.2934588752124,-20.9937483061839,
5.27890385386484));
#172917=CARTESIAN_POINT('Ctrl Pts',(19.2996602182366,-20.9920389444697,
5.27851960907695));
#172918=CARTESIAN_POINT('Ctrl Pts',(19.3125592840503,-20.9884200598194,
5.27771741969674));
#172919=CARTESIAN_POINT('Ctrl Pts',(19.3192555582502,-20.9865056979348,
5.27729932140178));
#172920=CARTESIAN_POINT('Ctrl Pts',(19.3366093753671,-20.9814517437655,
5.27621142450831));
#172921=CARTESIAN_POINT('Ctrl Pts',(19.3472517637493,-20.9782612631248,
5.2755399706083));
#172922=CARTESIAN_POINT('Ctrl Pts',(19.3932524252594,-20.9640751335714,
5.27261871195812));
#172923=CARTESIAN_POINT('Ctrl Pts',(19.4283421815413,-20.9522371776136,
5.27034144501515));
#172924=CARTESIAN_POINT('Ctrl Pts',(19.5206273164225,-20.9183827158465,
5.26421754509036));
#172925=CARTESIAN_POINT('Ctrl Pts',(19.5772047983738,-20.8947938863392,
5.26032198678025));
#172926=CARTESIAN_POINT('Ctrl Pts',(19.7734805152882,-20.8027709938382,
5.24632186742231));
#172927=CARTESIAN_POINT('Ctrl Pts',(19.9065686253226,-20.7214490469248,
5.23588573570889));
#172928=CARTESIAN_POINT('Ctrl Pts',(20.04189546632,-20.6167349084246,5.22476105877163));
#172929=CARTESIAN_POINT('Ctrl Pts',(20.0541401252136,-20.6070416715196,
5.22374985132899));
#172930=CARTESIAN_POINT('Ctrl Pts',(20.1040988825323,-20.566585597837,5.21960830584544));
#172931=CARTESIAN_POINT('Ctrl Pts',(20.1408570825245,-20.5346596479578,
5.21652329509552));
#172932=CARTESIAN_POINT('Ctrl Pts',(20.1821676888973,-20.4962019386202,
5.21304298154817));
#172933=CARTESIAN_POINT('Ctrl Pts',(20.1878214614105,-20.4908802568677,
5.21256637217816));
#172934=CARTESIAN_POINT('Ctrl Pts',(20.1968138283211,-20.4823222927788,
5.21180803834416));
#172935=CARTESIAN_POINT('Ctrl Pts',(20.2001711992745,-20.479105966026,5.21152484464288));
#172936=CARTESIAN_POINT('Ctrl Pts',(20.2061010862889,-20.4733876130133,
5.21102459145544));
#172937=CARTESIAN_POINT('Ctrl Pts',(20.2086778691496,-20.4708900751069,
5.21080718921328));
#172938=CARTESIAN_POINT('Ctrl Pts',(20.2141286873532,-20.4655799413635,
5.21034727370704));
#172939=CARTESIAN_POINT('Ctrl Pts',(20.2170010572892,-20.4627657113937,
5.21010489213194));
#172940=CARTESIAN_POINT('Ctrl Pts',(20.2247372779883,-20.4551427570659,
5.20945195697488));
#172941=CARTESIAN_POINT('Ctrl Pts',(20.2295859203568,-20.4503185702149,
5.20904260037014));
#172942=CARTESIAN_POINT('Ctrl Pts',(20.253601038531,-20.426191851873,5.20701388280868));
#172943=CARTESIAN_POINT('Ctrl Pts',(20.2724185746045,-20.4065437015529,
5.20542042921281));
#172944=CARTESIAN_POINT('Ctrl Pts',(20.3258253031997,-20.3485832464852,
5.2008674013323));
#172945=CARTESIAN_POINT('Ctrl Pts',(20.3594002848401,-20.3093603769208,
5.1979660963545));
#172946=CARTESIAN_POINT('Ctrl Pts',(20.477228516741,-20.1610617134911,5.18747332338905));
#172947=CARTESIAN_POINT('Ctrl Pts',(20.5522105038521,-20.0450639829885,
5.18014387401597));
#172948=CARTESIAN_POINT('Ctrl Pts',(20.6300376601681,-19.8942053634468,
5.17077621990492));
#172949=CARTESIAN_POINT('Ctrl Pts',(20.6440406809721,-19.8654846740376,
5.1690008260937));
#172950=CARTESIAN_POINT('Ctrl Pts',(20.6853895917279,-19.7755652799806,
5.16344810184575));
#172951=CARTESIAN_POINT('Ctrl Pts',(20.7104811944482,-19.7133815672481,
5.15961475188325));
#172952=CARTESIAN_POINT('Ctrl Pts',(20.7367727534823,-19.6381136565477,
5.15493406682916));
#172953=CARTESIAN_POINT('Ctrl Pts',(20.7408572017516,-19.6260732994402,
5.1541841638845));
#172954=CARTESIAN_POINT('Ctrl Pts',(20.7473579955751,-19.6063269735402,
5.15295213084223));
#172955=CARTESIAN_POINT('Ctrl Pts',(20.749839177489,-19.598642570813,5.15247214119126));
#172956=CARTESIAN_POINT('Ctrl Pts',(20.7542037330234,-19.5848559546031,
5.15160995480767));
#172957=CARTESIAN_POINT('Ctrl Pts',(20.7561035826163,-19.5787590302404,
5.15122830503331));
#172958=CARTESIAN_POINT('Ctrl Pts',(20.7600734600284,-19.5658131049891,
5.15041712365904));
#172959=CARTESIAN_POINT('Ctrl Pts',(20.7621364064564,-19.5589620318744,
5.14998736548389));
#172960=CARTESIAN_POINT('Ctrl Pts',(20.7675575871534,-19.5406219616332,
5.14883558624048));
#172961=CARTESIAN_POINT('Ctrl Pts',(20.7708531414546,-19.5291148455117,
5.1481115306973));
#172962=CARTESIAN_POINT('Ctrl Pts',(20.7863447022556,-19.4732367385839,
5.14458835558003));
#172963=CARTESIAN_POINT('Ctrl Pts',(20.7971886090947,-19.4285068308974,
5.14174580910474));
#172964=CARTESIAN_POINT('Ctrl Pts',(20.8410865586169,-19.2176390033274,
5.12823209825699));
#172965=CARTESIAN_POINT('Ctrl Pts',(20.8555768467132,-19.0482924557364,
5.11698566285067));
#172966=CARTESIAN_POINT('Ctrl Pts',(20.8463190488305,-18.7797321213914,
5.09928230616555));
#172967=CARTESIAN_POINT('Ctrl Pts',(20.8359029716536,-18.680749975873,5.092804795141));
#172968=CARTESIAN_POINT('Ctrl Pts',(20.816877115971,-18.5733102788523,5.08606340077225));
#172969=CARTESIAN_POINT('Ctrl Pts',(20.8151210687593,-18.5637757213809,
5.0854677334217));
#172970=CARTESIAN_POINT('Ctrl Pts',(20.8124316394239,-18.5497161955159,
5.08459353305305));
#172971=CARTESIAN_POINT('Ctrl Pts',(20.8115488734488,-18.5451818361064,
5.08431223423984));
#172972=CARTESIAN_POINT('Ctrl Pts',(20.8099564858598,-18.5371428509674,
5.08381470055339));
#172973=CARTESIAN_POINT('Ctrl Pts',(20.8092528208595,-18.5336371007351,
5.08359813080258));
#172974=CARTESIAN_POINT('Ctrl Pts',(20.8077262056343,-18.5261299354911,
5.08313524182846));
#172975=CARTESIAN_POINT('Ctrl Pts',(20.806900557178,-18.522129125807,5.08288907879628));
#172976=CARTESIAN_POINT('Ctrl Pts',(20.8046024912724,-18.5111540741109,
5.08221518325148));
#172977=CARTESIAN_POINT('Ctrl Pts',(20.8031064076511,-18.5041847653949,
5.08178878271177));
#172978=CARTESIAN_POINT('Ctrl Pts',(20.7949329799469,-18.4670255047476,
5.07952282752548));
#172979=CARTESIAN_POINT('Ctrl Pts',(20.7876296646545,-18.4369753051609,
5.07771699789486));
#172980=CARTESIAN_POINT('Ctrl Pts',(20.7635348963703,-18.3465194026107,
5.07233253738531));
#172981=CARTESIAN_POINT('Ctrl Pts',(20.7447157619216,-18.2866865983345,
5.06884061755312));
#172982=CARTESIAN_POINT('Ctrl Pts',(20.6772851160064,-18.1014716602466,
5.05800781631651));
#172983=CARTESIAN_POINT('Ctrl Pts',(20.6193796952157,-17.9798376645672,
5.05083994676616));
#172984=CARTESIAN_POINT('Ctrl Pts',(20.529375547633,-17.829511712847,5.04111629893205));
#172985=CARTESIAN_POINT('Ctrl Pts',(20.5074124473629,-17.7951243117778,
5.03882943063877));
#172986=CARTESIAN_POINT('Ctrl Pts',(20.4571198046639,-17.7211823126013,
5.03374715354906));
#172987=CARTESIAN_POINT('Ctrl Pts',(20.4283934804564,-17.6819274665458,
5.03093987799765));
#172988=CARTESIAN_POINT('Ctrl Pts',(20.3905520674963,-17.6337878923138,
5.02733863546636));
#172989=CARTESIAN_POINT('Ctrl Pts',(20.3826733027,-17.6239471984142,5.02659380992691));
#172990=CARTESIAN_POINT('Ctrl Pts',(20.370050220488,-17.6084662327259,5.02540797910422));
#172991=CARTESIAN_POINT('Ctrl Pts',(20.3653634508192,-17.6027792630595,
5.0249692980654));
#172992=CARTESIAN_POINT('Ctrl Pts',(20.3565758268546,-17.5922290069864,
5.02414968284782));
#172993=CARTESIAN_POINT('Ctrl Pts',(20.3524825493749,-17.5873594966676,
5.02376906056121));
#172994=CARTESIAN_POINT('Ctrl Pts',(20.3433430414357,-17.5765857719689,
5.02292171363795));
#172995=CARTESIAN_POINT('Ctrl Pts',(20.3382861592764,-17.5706907513758,
5.02245455300102));
#172996=CARTESIAN_POINT('Ctrl Pts',(20.3235001590823,-17.553644808404,5.02109335634916));
#172997=CARTESIAN_POINT('Ctrl Pts',(20.3136865635017,-17.5425680785398,
5.02019581449633));
#172998=CARTESIAN_POINT('Ctrl Pts',(20.2348710413583,-17.4554652346242,
5.01303236958278));
#172999=CARTESIAN_POINT('Ctrl Pts',(20.1605477075074,-17.3844584812322,
5.00653638429608));
#173000=CARTESIAN_POINT('Ctrl Pts',(19.9622878213766,-17.2208625695326,
4.98985208558333));
#173001=CARTESIAN_POINT('Ctrl Pts',(19.832814885006,-17.1359245894896,4.9794792746869));
#173002=CARTESIAN_POINT('Ctrl Pts',(19.6471547041593,-17.0413056519028,
4.96600612213582));
#173003=CARTESIAN_POINT('Ctrl Pts',(19.5981223985087,-17.0186355862422,
4.96257237536748));
#173004=CARTESIAN_POINT('Ctrl Pts',(19.540200848538,-16.9945001511946,4.95870136918187));
#173005=CARTESIAN_POINT('Ctrl Pts',(19.5321081526108,-16.9911866868436,
4.95816464068569));
#173006=CARTESIAN_POINT('Ctrl Pts',(19.519830793032,-16.9862484615939,4.95735685104349));
#173007=CARTESIAN_POINT('Ctrl Pts',(19.5156612260621,-16.9845867555206,
4.95708363880995));
#173008=CARTESIAN_POINT('Ctrl Pts',(19.508171175597,-16.9816293001501,4.95659490736115));
#173009=CARTESIAN_POINT('Ctrl Pts',(19.5048526906678,-16.9803286699272,
4.95637909819435));
#173010=CARTESIAN_POINT('Ctrl Pts',(19.4976392279169,-16.9775224573611,
4.95591156531599));
#173011=CARTESIAN_POINT('Ctrl Pts',(19.4937430880841,-16.976020020952,4.95566003115926));
#173012=CARTESIAN_POINT('Ctrl Pts',(19.4827977870243,-16.9718364328974,
4.95495611122427));
#173013=CARTESIAN_POINT('Ctrl Pts',(19.4757386255172,-16.9691813765175,
4.95450526174506));
#173014=CARTESIAN_POINT('Ctrl Pts',(19.4336808862023,-16.9536188689361,
4.95183695137688));
#173015=CARTESIAN_POINT('Ctrl Pts',(19.3983579757969,-16.9415997036103,
4.94966900134766));
#173016=CARTESIAN_POINT('Ctrl Pts',(19.2815937019356,-16.9052829473468,
4.9426836851965));
#173017=CARTESIAN_POINT('Ctrl Pts',(19.1990013073988,-16.8849524392151,
4.93802495004452));
#173018=CARTESIAN_POINT('Ctrl Pts',(18.9399197219225,-16.8374990788314,
4.92368659589947));
#173019=CARTESIAN_POINT('Ctrl Pts',(18.7610973104413,-16.8276703962925,
4.91410957790419));
#173020=CARTESIAN_POINT('Ctrl Pts',(18.5604566308968,-16.8420023720653,
4.90241830992957));
#173021=CARTESIAN_POINT('Ctrl Pts',(18.5377768143958,-16.8439905851481,
4.90108435087472));
#173022=CARTESIAN_POINT('Ctrl Pts',(18.5056759114268,-16.8473272144179,
4.89917694942165));
#173023=CARTESIAN_POINT('Ctrl Pts',(18.4962245754309,-16.8483740192756,
4.89861298266469));
#173024=CARTESIAN_POINT('Ctrl Pts',(18.4808613441585,-16.8501804681498,
4.89769226024643));
#173025=CARTESIAN_POINT('Ctrl Pts',(18.4749449729642,-16.8509014741339,
4.89733672655739));
#173026=CARTESIAN_POINT('Ctrl Pts',(18.4625525391915,-16.8524648313052,
4.89658997074541));
#173027=CARTESIAN_POINT('Ctrl Pts',(18.456077180921,-16.8533121828825,4.89619859423836));
#173028=CARTESIAN_POINT('Ctrl Pts',(18.4406551583803,-16.8554029018133,
4.89526361932241));
#173029=CARTESIAN_POINT('Ctrl Pts',(18.4317123822986,-16.8566735861777,
4.89471916216865));
#173030=CARTESIAN_POINT('Ctrl Pts',(18.4014850482065,-16.8611661431394,
4.8928709386469));
#173031=CARTESIAN_POINT('Ctrl Pts',(18.3802421343791,-16.8646553401602,
4.89155874596095));
#173032=CARTESIAN_POINT('Ctrl Pts',(18.1813146057088,-16.9004534618432,
4.87914154751217));
#173033=CARTESIAN_POINT('Ctrl Pts',(18.0084285223842,-16.9550461715309,
4.86728210648543));
#173034=CARTESIAN_POINT('Ctrl Pts',(17.7363591800773,-17.0810027225583,
4.84747615314401));
#173035=CARTESIAN_POINT('Ctrl Pts',(17.6325274989788,-17.1401824166858,
4.83962887022806));
#173036=CARTESIAN_POINT('Ctrl Pts',(17.5263848639483,-17.2131943061605,
4.83167172260674));
#173037=CARTESIAN_POINT('Ctrl Pts',(17.5185807529136,-17.2186403664178,
4.83108715121268));
#173038=CARTESIAN_POINT('Ctrl Pts',(17.5070715754884,-17.2267879377201,
4.83022607957612));
#173039=CARTESIAN_POINT('Ctrl Pts',(17.503338259817,-17.2294490716168,4.82994692961862));
#173040=CARTESIAN_POINT('Ctrl Pts',(17.4967965708902,-17.2341441567271,
4.82945811851666));
#173041=CARTESIAN_POINT('Ctrl Pts',(17.4939845240037,-17.2361728982267,
4.82924810448511));
#173042=CARTESIAN_POINT('Ctrl Pts',(17.491164892823,-17.2382176635852,4.82903763801035));
#173043=CARTESIAN_POINT('Ctrl Pts',(17.4911523728596,-17.2382267431335,
4.82903670348161));
#173044=CARTESIAN_POINT('Ctrl Pts',(17.4911275513973,-17.2382447442137,
4.82903485073532));
#173045=CARTESIAN_POINT('Ctrl Pts',(17.4911152499266,-17.2382536657177,
4.82903393251981));
#173046=CARTESIAN_POINT('Ctrl Pts',(17.4910908606305,-17.2382713541827,
4.82903211204004));
#173047=CARTESIAN_POINT('Ctrl Pts',(17.4910787727824,-17.2382801211532,
4.82903120977402));
#173048=CARTESIAN_POINT('Ctrl Pts',(17.4910548064742,-17.2382975036179,
4.82902942087523));
#173049=CARTESIAN_POINT('Ctrl Pts',(17.4910429278426,-17.2383061192298,
4.8290285342296));
#173050=CARTESIAN_POINT('Ctrl Pts',(17.4910193741398,-17.2383232031844,
4.82902677613641));
#173051=CARTESIAN_POINT('Ctrl Pts',(17.491007699632,-17.238331671112,4.82902590473084));
#173052=CARTESIAN_POINT('Ctrl Pts',(17.4909845508505,-17.2383484620914,
4.82902417686927));
#173053=CARTESIAN_POINT('Ctrl Pts',(17.4909730763056,-17.2383567853337,
4.82902332039297));
#173054=CARTESIAN_POINT('Ctrl Pts',(17.4909503232398,-17.2383732899781,
4.82902162207552));
#173055=CARTESIAN_POINT('Ctrl Pts',(17.4909390444557,-17.2383814715651,
4.82902078021466));
#173056=CARTESIAN_POINT('Ctrl Pts',(17.4909166782863,-17.2383976962361,
4.82901911078267));
#173057=CARTESIAN_POINT('Ctrl Pts',(17.4909055909967,-17.238405739245,4.82901828321862));
#173058=CARTESIAN_POINT('Ctrl Pts',(17.4908836033598,-17.2384216899757,
4.82901664204743));
#173059=CARTESIAN_POINT('Ctrl Pts',(17.4908727032694,-17.2384295975056,
4.82901582845942));
#173060=CARTESIAN_POINT('Ctrl Pts',(17.4908510867112,-17.2384452796703,
4.82901421499234));
#173061=CARTESIAN_POINT('Ctrl Pts',(17.4908403700331,-17.2384530544523,
4.82901341509752));
#173062=CARTESIAN_POINT('Ctrl Pts',(17.490819116412,-17.2384684739256,4.82901182872651));
#173063=CARTESIAN_POINT('Ctrl Pts',(17.4908085793549,-17.2384761186946,
4.82901104224176));
#173064=CARTESIAN_POINT('Ctrl Pts',(17.4907876807863,-17.2384912811663,
4.82900948237801));
#173065=CARTESIAN_POINT('Ctrl Pts',(17.4907773194862,-17.2384987987107,
4.82900870901474));
#173066=CARTESIAN_POINT('Ctrl Pts',(17.4907572863614,-17.2385133338344,
4.82900721375325));
#173067=CARTESIAN_POINT('Ctrl Pts',(17.4907476147675,-17.2385203512278,
4.82900649187207));
#173068=CARTESIAN_POINT('Ctrl Pts',(17.4907283082907,-17.2385343596279,
4.82900505085238));
#173069=CARTESIAN_POINT('Ctrl Pts',(17.4907186731607,-17.2385413508128,
4.82900433169542));
#173070=CARTESIAN_POINT('Ctrl Pts',(17.4906994389801,-17.2385553072514,
4.82900289607701));
#173071=CARTESIAN_POINT('Ctrl Pts',(17.4906898399113,-17.2385622725173,
4.82900217961419));
#173072=CARTESIAN_POINT('Ctrl Pts',(17.4906706776621,-17.2385761772538,
4.82900074936975));
#173073=CARTESIAN_POINT('Ctrl Pts',(17.4906611144548,-17.2385831167428,
4.82900003558613));
#173074=CARTESIAN_POINT('Ctrl Pts',(17.4873595633594,-17.2409789114267,
4.82875361314171));
#173075=CARTESIAN_POINT('Ctrl Pts',(17.4840744353518,-17.2433772718097,
4.82850856674509));
#173076=CARTESIAN_POINT('Ctrl Pts',(17.4772837403103,-17.2483649933542,
4.82800229636659));
#173077=CARTESIAN_POINT('Ctrl Pts',(17.4737792121438,-17.2509557442992,
4.82774116884939));
#173078=CARTESIAN_POINT('Ctrl Pts',(17.4648886357129,-17.25757073086,4.82707902482906));
#173079=CARTESIAN_POINT('Ctrl Pts',(17.4595136673081,-17.2616098694312,
4.82667899986179));
#173080=CARTESIAN_POINT('Ctrl Pts',(17.4440675041607,-17.2733327843016,
4.82552997832671));
#173081=CARTESIAN_POINT('Ctrl Pts',(17.4340457362834,-17.2810815718692,
4.82478513649517));
#173082=CARTESIAN_POINT('Ctrl Pts',(17.3998992444123,-17.307976670175,4.82224727187036));
#173083=CARTESIAN_POINT('Ctrl Pts',(17.3761221193629,-17.3275599775156,
4.82048004543612));
#173084=CARTESIAN_POINT('Ctrl Pts',(17.2576046163725,-17.4295947020338,
4.81162244029538));
#173085=CARTESIAN_POINT('Ctrl Pts',(17.1699023948968,-17.5198460840967,
4.80489273819077));
#173086=CARTESIAN_POINT('Ctrl Pts',(17.0703323498763,-17.6424412566836,
4.79629573249236));
#173087=CARTESIAN_POINT('Ctrl Pts',(17.0505285847102,-17.6679991863497,
4.79453089435811));
#173088=CARTESIAN_POINT('Ctrl Pts',(16.9677514087738,-17.7800367236019,
4.78687724020415));
#173089=CARTESIAN_POINT('Ctrl Pts',(16.9108049776667,-17.8707564587531,
4.78087640088961));
#173090=CARTESIAN_POINT('Ctrl Pts',(16.8543804800283,-17.9778753612386,
4.77378206341766));
#173091=CARTESIAN_POINT('Ctrl Pts',(16.8479255629668,-17.9904327609149,
4.77295047080033));
#173092=CARTESIAN_POINT('Ctrl Pts',(16.8378292523889,-18.0105669742307,
4.77161679850807));
#173093=CARTESIAN_POINT('Ctrl Pts',(16.8341064723427,-18.0181026680824,
4.7711175714359));
#173094=CARTESIAN_POINT('Ctrl Pts',(16.8276068936708,-18.0314589030616,
4.77023253496533));
#173095=CARTESIAN_POINT('Ctrl Pts',(16.8248116151471,-18.0372703695984,
4.76984737533886));
#173096=CARTESIAN_POINT('Ctrl Pts',(16.819072493442,-18.0493430809861,4.76904706285574));
#173097=CARTESIAN_POINT('Ctrl Pts',(16.8161327079192,-18.0556061596514,
4.76863177503638));
#173098=CARTESIAN_POINT('Ctrl Pts',(16.8086396505514,-18.0717753764283,
4.76755931972236));
#173099=CARTESIAN_POINT('Ctrl Pts',(16.8041321485649,-18.0817023887174,
4.7669005840777));
#173100=CARTESIAN_POINT('Ctrl Pts',(16.7854245684037,-18.1237627314918,
4.76410794969152));
#173101=CARTESIAN_POINT('Ctrl Pts',(16.7719494902557,-18.1562106116635,
4.76194949610491));
#173102=CARTESIAN_POINT('Ctrl Pts',(16.7545505706728,-18.2012392122745,
4.75894686365453));
#173103=CARTESIAN_POINT('Ctrl Pts',(16.7499273310879,-18.2135439171612,
4.75812563213439));
#173104=CARTESIAN_POINT('Ctrl Pts',(16.7454193672347,-18.225889769394,4.75730093103984));
#173105=CARTESIAN_POINT('Ctrl Pts',(16.7454193964829,-18.2258896892926,
4.53222340662745));
#173106=CARTESIAN_POINT('Ctrl Pts',(16.754772318456,-18.200275069933,4.53397284136854));
#173107=CARTESIAN_POINT('Ctrl Pts',(16.7646214421699,-18.1748376104556,
4.53573525615426));
#173108=CARTESIAN_POINT('Ctrl Pts',(16.8069131799647,-18.0715845407491,
4.54298738003099));
#173109=CARTESIAN_POINT('Ctrl Pts',(16.8434938433157,-17.9955585372352,
4.54856233763303));
#173110=CARTESIAN_POINT('Ctrl Pts',(16.9297103717033,-17.8407581583082,
4.5602682192208));
#173111=CARTESIAN_POINT('Ctrl Pts',(16.9802103467348,-17.7626540023637,
4.56638569977088));
#173112=CARTESIAN_POINT('Ctrl Pts',(17.0541238084425,-17.6633343328212,
4.5742404025468));
#173113=CARTESIAN_POINT('Ctrl Pts',(17.0731072755806,-17.6389581837111,
4.57617427513876));
#173114=CARTESIAN_POINT('Ctrl Pts',(17.0971189102555,-17.6094799534252,
4.57851166140639));
#173115=CARTESIAN_POINT('Ctrl Pts',(17.1016471801378,-17.6039777256158,
4.57894788660996));
#173116=CARTESIAN_POINT('Ctrl Pts',(17.1088147078132,-17.5953576558042,
4.5796310650876));
#173117=CARTESIAN_POINT('Ctrl Pts',(17.111435305927,-17.5922244677135,4.57987933492333));
#173118=CARTESIAN_POINT('Ctrl Pts',(17.1163670238579,-17.5863626613758,
4.58034369213323));
#173119=CARTESIAN_POINT('Ctrl Pts',(17.1186759616822,-17.5836323456073,
4.58055992558959));
#173120=CARTESIAN_POINT('Ctrl Pts',(17.1239841426583,-17.5773875873574,
4.58105438511289));
#173121=CARTESIAN_POINT('Ctrl Pts',(17.1269879753649,-17.5738771101644,
4.58133226895676));
#173122=CARTESIAN_POINT('Ctrl Pts',(17.1348968945598,-17.5646952456248,
4.58205897836552));
#173123=CARTESIAN_POINT('Ctrl Pts',(17.1398207111901,-17.5590399782331,
4.58250645781604));
#173124=CARTESIAN_POINT('Ctrl Pts',(17.1732971584306,-17.5210004842219,
4.58551655451351));
#173125=CARTESIAN_POINT('Ctrl Pts',(17.2028067799057,-17.4894676521047,
4.5880127018827));
#173126=CARTESIAN_POINT('Ctrl Pts',(17.2841891408324,-17.4076713448506,
4.59456112287321));
#173127=CARTESIAN_POINT('Ctrl Pts',(17.3377047382897,-17.3591210282201,
4.59852801774289));
#173128=CARTESIAN_POINT('Ctrl Pts',(17.4624292677644,-17.2570945701982,
4.60731084102632));
#173129=CARTESIAN_POINT('Ctrl Pts',(17.5347367473087,-17.2051846040635,
4.61210402565903));
#173130=CARTESIAN_POINT('Ctrl Pts',(17.6710014414909,-17.1198185781199,
4.62094191479838));
#173131=CARTESIAN_POINT('Ctrl Pts',(17.7338083413045,-17.0847908206052,
4.62494721111515));
#173132=CARTESIAN_POINT('Ctrl Pts',(17.8227977656424,-17.0409408466135,
4.63062111952317));
#173133=CARTESIAN_POINT('Ctrl Pts',(17.8475550973671,-17.0293320778753,
4.6321992403569));
#173134=CARTESIAN_POINT('Ctrl Pts',(17.8907948774613,-17.0100695295552,
4.63495923152697));
#173135=CARTESIAN_POINT('Ctrl Pts',(17.9091740820108,-17.0021920619488,
4.63613350538952));
#173136=CARTESIAN_POINT('Ctrl Pts',(17.9357442339642,-16.99124679124,4.63783385888435));
#173137=CARTESIAN_POINT('Ctrl Pts',(17.9438472553281,-16.9879674009152,
4.63835277178358));
#173138=CARTESIAN_POINT('Ctrl Pts',(17.9580199490438,-16.9823334437839,
4.63926110786267));
#173139=CARTESIAN_POINT('Ctrl Pts',(17.9640806427731,-16.9799565004632,
4.63964977092109));
#173140=CARTESIAN_POINT('Ctrl Pts',(17.9757332274125,-16.9754483785895,
4.64039751280649));
#173141=CARTESIAN_POINT('Ctrl Pts',(17.9813233875882,-16.9733128780688,
4.64075644189779));
#173142=CARTESIAN_POINT('Ctrl Pts',(17.9959434004303,-16.9677987983539,
4.64169574023316));
#173143=CARTESIAN_POINT('Ctrl Pts',(18.0049873357343,-16.9644581807389,
4.64227737278311));
#173144=CARTESIAN_POINT('Ctrl Pts',(18.0362140946776,-16.9531655549944,
4.64428780762626));
#173145=CARTESIAN_POINT('Ctrl Pts',(18.0585060534235,-16.9455224481869,
4.64572680546249));
#173146=CARTESIAN_POINT('Ctrl Pts',(18.2397818338403,-16.8867327617592,
4.65746335188572));
#173147=CARTESIAN_POINT('Ctrl Pts',(18.4041534451225,-16.8542008464835,
4.66839028012184));
#173148=CARTESIAN_POINT('Ctrl Pts',(18.6959290106786,-16.8316130817408,
4.68772987662371));
#173149=CARTESIAN_POINT('Ctrl Pts',(18.8218850191862,-16.8330915692602,
4.69603740526457));
#173150=CARTESIAN_POINT('Ctrl Pts',(18.9588884424978,-16.8469447636106,
4.70457748661341));
#173151=CARTESIAN_POINT('Ctrl Pts',(18.9707908796195,-16.8482503822106,
4.70531515341339));
#173152=CARTESIAN_POINT('Ctrl Pts',(18.9876807360557,-16.8502482491841,
4.70635523972687));
#173153=CARTESIAN_POINT('Ctrl Pts',(18.9926774971707,-16.8508573842878,
4.70666211073343));
#173154=CARTESIAN_POINT('Ctrl Pts',(19.0012791776244,-16.851937130166,4.70718888456338));
#173155=CARTESIAN_POINT('Ctrl Pts',(19.0048851290856,-16.8523992132633,
4.70740926396949));
#173156=CARTESIAN_POINT('Ctrl Pts',(19.0118699263502,-16.8533125712208,
4.70783524715647));
#173157=CARTESIAN_POINT('Ctrl Pts',(19.0152488725661,-16.8537627179592,
4.70804091578542));
#173158=CARTESIAN_POINT('Ctrl Pts',(19.0243527712292,-16.8549979353352,
4.70859399576695));
#173159=CARTESIAN_POINT('Ctrl Pts',(19.0300756695645,-16.8557982943802,
4.70894054992581));
#173160=CARTESIAN_POINT('Ctrl Pts',(19.0512482991217,-16.8588477681515,
4.71021875029902));
#173161=CARTESIAN_POINT('Ctrl Pts',(19.0666767188995,-16.8612443993234,
4.71114243008841));
#173162=CARTESIAN_POINT('Ctrl Pts',(19.2162964974428,-16.8861843472443,
4.7200369313936));
#173163=CARTESIAN_POINT('Ctrl Pts',(19.3480651140697,-16.9214487168096,
4.72738951779247));
#173164=CARTESIAN_POINT('Ctrl Pts',(19.6208322890261,-17.0234574446481,
4.74320404432964));
#173165=CARTESIAN_POINT('Ctrl Pts',(19.7596839715869,-17.093583251869,4.75165261966882));
#173166=CARTESIAN_POINT('Ctrl Pts',(19.9074470798247,-17.1898526076665,
4.76192312841269));
#173167=CARTESIAN_POINT('Ctrl Pts',(19.9250932814396,-17.2017319554377,
4.7631713912118));
#173168=CARTESIAN_POINT('Ctrl Pts',(19.9499376985908,-17.2190068308189,
4.76496143502447));
#173169=CARTESIAN_POINT('Ctrl Pts',(19.957285523834,-17.2241856770287,4.765494978814));
#173170=CARTESIAN_POINT('Ctrl Pts',(19.9699075633757,-17.2332027342146,
4.76641876189396));
#173171=CARTESIAN_POINT('Ctrl Pts',(19.9751974716944,-17.2370188394995,
4.76680814699667));
#173172=CARTESIAN_POINT('Ctrl Pts',(19.9852943241552,-17.2443738277718,
4.76755568472128));
#173173=CARTESIAN_POINT('Ctrl Pts',(19.9901041092418,-17.247908718597,4.76791367995835));
#173174=CARTESIAN_POINT('Ctrl Pts',(20.0025768327709,-17.2571568859452,
4.76884701316293));
#173175=CARTESIAN_POINT('Ctrl Pts',(20.010216078317,-17.2629017557701,4.76942358320949));
#173176=CARTESIAN_POINT('Ctrl Pts',(20.0361560695647,-17.2826855967837,
4.77139846845714));
#173177=CARTESIAN_POINT('Ctrl Pts',(20.0542656587715,-17.2969714411774,
4.77280650147324));
#173178=CARTESIAN_POINT('Ctrl Pts',(20.207352452308,-17.4218464405586,4.78496745277203));
#173179=CARTESIAN_POINT('Ctrl Pts',(20.3283874709806,-17.5484178328147,
4.79641507488717));
#173180=CARTESIAN_POINT('Ctrl Pts',(20.4848581117967,-17.7587363930967,
4.81373567188046));
#173181=CARTESIAN_POINT('Ctrl Pts',(20.532791902547,-17.8322983480734,4.81951805212073));
#173182=CARTESIAN_POINT('Ctrl Pts',(20.5947541019857,-17.9416895947832,
4.82754598929554));
#173183=CARTESIAN_POINT('Ctrl Pts',(20.6125899992041,-17.9752538849689,
4.82993652355876));
#173184=CARTESIAN_POINT('Ctrl Pts',(20.6328900403606,-18.0160709973614,
4.83274178051278));
#173185=CARTESIAN_POINT('Ctrl Pts',(20.6362298347509,-18.0228777566229,
4.8332062556453));
#173186=CARTESIAN_POINT('Ctrl Pts',(20.6413560446168,-18.0334688745061,
4.83392363046653));
#173187=CARTESIAN_POINT('Ctrl Pts',(20.6431678902856,-18.0372407547124,
4.83417806927643));
#173188=CARTESIAN_POINT('Ctrl Pts',(20.6465020140673,-18.044234752239,4.83464789617231));
#173189=CARTESIAN_POINT('Ctrl Pts',(20.6480273271511,-18.0474553133902,
4.83486346719623));
#173190=CARTESIAN_POINT('Ctrl Pts',(20.6514506883045,-18.054730863922,4.83534873327727));
#173191=CARTESIAN_POINT('Ctrl Pts',(20.6533440037885,-18.0587880203415,
4.83561813427794));
#173192=CARTESIAN_POINT('Ctrl Pts',(20.6588751268934,-18.0707393707925,
4.83640827253624));
#173193=CARTESIAN_POINT('Ctrl Pts',(20.6624772549224,-18.0786501080127,
4.83692686193532));
#173194=CARTESIAN_POINT('Ctrl Pts',(20.6875902756344,-18.1347145519584,
4.84057262004026));
#173195=CARTESIAN_POINT('Ctrl Pts',(20.7073457422561,-18.1836393823493,
4.84360071800973));
#173196=CARTESIAN_POINT('Ctrl Pts',(20.7306225801284,-18.2481269597652,
4.84745835617574));
#173197=CARTESIAN_POINT('Ctrl Pts',(20.735823873816,-18.2630586525973,4.84834244346051));
#173198=CARTESIAN_POINT('Ctrl Pts',(20.7570349475525,-18.3262197808785,
4.85204911562008));
#173199=CARTESIAN_POINT('Ctrl Pts',(20.7714732402945,-18.374960639018,4.8548291864931));
#173200=CARTESIAN_POINT('Ctrl Pts',(20.811422380871,-18.5301286100413,4.86355297288325));
#173201=CARTESIAN_POINT('Ctrl Pts',(20.8304458149371,-18.6380361702916,
4.86944393682973));
#173202=CARTESIAN_POINT('Ctrl Pts',(20.846389206078,-18.8018475032445,4.87859495474299));
#173203=CARTESIAN_POINT('Ctrl Pts',(20.8495848950305,-18.8569535131039,
4.88170630147725));
#173204=CARTESIAN_POINT('Ctrl Pts',(20.8512712239753,-18.9464523135157,
4.8868560873045));
#173205=CARTESIAN_POINT('Ctrl Pts',(20.8510826304748,-18.9807949876418,
4.88885502266212));
#173206=CARTESIAN_POINT('Ctrl Pts',(20.8497365406336,-19.0259243042199,
4.89151775477155));
#173207=CARTESIAN_POINT('Ctrl Pts',(20.8493313807709,-19.0367293047743,
4.89215797610226));
#173208=CARTESIAN_POINT('Ctrl Pts',(20.8485321517945,-19.0544225315507,
4.89321094644742));
#173209=CARTESIAN_POINT('Ctrl Pts',(20.8481871471625,-19.0613128582669,
4.89362215266174));
#173210=CARTESIAN_POINT('Ctrl Pts',(20.84745407647,-19.0746480865406,4.8944202480048));
#173211=CARTESIAN_POINT('Ctrl Pts',(20.8470701938352,-19.0810931484332,
4.8948070014158));
#173212=CARTESIAN_POINT('Ctrl Pts',(20.846115669035,-19.0959716965935,4.89570223994669));
#173213=CARTESIAN_POINT('Ctrl Pts',(20.8455239908086,-19.1044036804215,
4.89621138054998));
#173214=CARTESIAN_POINT('Ctrl Pts',(20.8437967267627,-19.1270736393192,
4.89758515543206));
#173215=CARTESIAN_POINT('Ctrl Pts',(20.8425675337751,-19.1413038490304,
4.89845271424219));
#173216=CARTESIAN_POINT('Ctrl Pts',(20.8276339788592,-19.2959218893946,
4.90793753224795));
#173217=CARTESIAN_POINT('Ctrl Pts',(20.8000780806493,-19.4345904264661,
4.91700446926346));
#173218=CARTESIAN_POINT('Ctrl Pts',(20.7307657611253,-19.6618965447862,
4.9326383499417));
#173219=CARTESIAN_POINT('Ctrl Pts',(20.6962859582462,-19.7522878394038,
4.93906620081814));
#173220=CARTESIAN_POINT('Ctrl Pts',(20.6352154251679,-19.8844515525025,
4.94856682673797));
#173221=CARTESIAN_POINT('Ctrl Pts',(20.6131418038496,-19.9281724769969,
4.9517262946967));
#173222=CARTESIAN_POINT('Ctrl Pts',(20.5769349017628,-19.9940983322026,
4.95647585431921));
#173223=CARTESIAN_POINT('Ctrl Pts',(20.5638717655726,-20.0168696888842,
4.95811355220475));
#173224=CARTESIAN_POINT('Ctrl Pts',(20.5469161354676,-20.0451924660992,
4.96014129875251));
#173225=CARTESIAN_POINT('Ctrl Pts',(20.5434166529492,-20.0509750047458,
4.96055480325799));
#173226=CARTESIAN_POINT('Ctrl Pts',(20.5378004231564,-20.0601557017502,
4.96121039766653));
#173227=CARTESIAN_POINT('Ctrl Pts',(20.5357016616382,-20.0635647299935,
4.96145363570265));
#173228=CARTESIAN_POINT('Ctrl Pts',(20.5317008673729,-20.070022138123,4.96191396606396));
#173229=CARTESIAN_POINT('Ctrl Pts',(20.5298007682063,-20.0730715904659,
4.96213117331686));
#173230=CARTESIAN_POINT('Ctrl Pts',(20.5254067434013,-20.0800836853035,
4.96263024271057));
#173231=CARTESIAN_POINT('Ctrl Pts',(20.5229074300434,-20.0840429007112,
4.96291174500148));
#173232=CARTESIAN_POINT('Ctrl Pts',(20.5161685919782,-20.0946399885494,
4.96366452749176));
#173233=CARTESIAN_POINT('Ctrl Pts',(20.5119050780741,-20.1012626207208,
4.96413426295707));
#173234=CARTESIAN_POINT('Ctrl Pts',(20.4795573094514,-20.1508984604032,
4.96765070155067));
#173235=CARTESIAN_POINT('Ctrl Pts',(20.4499503115872,-20.1929042217322,
4.97060301945223));
#173236=CARTESIAN_POINT('Ctrl Pts',(20.405322651057,-20.2515645953815,4.97475506271402));
#173237=CARTESIAN_POINT('Ctrl Pts',(20.3915229145882,-20.2691201075979,
4.97600158804748));
#173238=CARTESIAN_POINT('Ctrl Pts',(20.34849985572,-20.3221051671264,4.97978668947714));
#173239=CARTESIAN_POINT('Ctrl Pts',(20.31839877085,-20.3568055840512,4.98229787485677));
#173240=CARTESIAN_POINT('Ctrl Pts',(20.2128871884547,-20.4707296129182,
4.99075189091243));
#173241=CARTESIAN_POINT('Ctrl Pts',(20.1324783320613,-20.54508016895,4.99664011080124));
#173242=CARTESIAN_POINT('Ctrl Pts',(20.0034506055505,-20.6470580023039,
5.00578474865274));
#173243=CARTESIAN_POINT('Ctrl Pts',(19.9588963512765,-20.6795285104071,
5.00889243798102));
#173244=CARTESIAN_POINT('Ctrl Pts',(19.8846336888657,-20.729331771879,5.01403670977699));
#173245=CARTESIAN_POINT('Ctrl Pts',(19.8556800796864,-20.7477448915421,
5.01603389934779));
#173246=CARTESIAN_POINT('Ctrl Pts',(19.8170338156994,-20.7710227019625,
5.01869463528502));
#173247=CARTESIAN_POINT('Ctrl Pts',(19.8077321939334,-20.7765287077368,
5.01933465131812));
#173248=CARTESIAN_POINT('Ctrl Pts',(19.7924260374679,-20.7854314572724,
5.02038736999084));
#173249=CARTESIAN_POINT('Ctrl Pts',(19.7864462707031,-20.7888705536475,
5.02079853127742));
#173250=CARTESIAN_POINT('Ctrl Pts',(19.7748370293323,-20.7954719875448,
5.02159660086907));
#173251=CARTESIAN_POINT('Ctrl Pts',(19.769209679183,-20.7986379204339,5.0219833737817));
#173252=CARTESIAN_POINT('Ctrl Pts',(19.7561805473098,-20.8058898051277,
5.02287874696172));
#173253=CARTESIAN_POINT('Ctrl Pts',(19.7487686329828,-20.8099572382404,
5.02338800333369));
#173254=CARTESIAN_POINT('Ctrl Pts',(19.7287643514983,-20.8207795694781,
5.02476229315683));
#173255=CARTESIAN_POINT('Ctrl Pts',(19.7161277950838,-20.8274514583743,
5.02563025455207));
#173256=CARTESIAN_POINT('Ctrl Pts',(19.5995666347805,-20.8874926935597,
5.03363619915195));
#173257=CARTESIAN_POINT('Ctrl Pts',(19.4914754346517,-20.9322930917346,
5.04107584411056));
#173258=CARTESIAN_POINT('Ctrl Pts',(19.2253670958755,-21.0176000717807,
5.05932905993716));
#173259=CARTESIAN_POINT('Ctrl Pts',(19.0652754111759,-21.0492367399968,
5.07028251195642));
#173260=CARTESIAN_POINT('Ctrl Pts',(18.8706544515756,-21.0648361836614,
5.08268978694441));
#173261=CARTESIAN_POINT('Ctrl Pts',(18.8381096402168,-21.0666897246284,
5.08473256954471));
#173262=CARTESIAN_POINT('Ctrl Pts',(18.7982918666113,-21.0680359283952,
5.08718250355468));
#173263=CARTESIAN_POINT('Ctrl Pts',(18.7910493736998,-21.0682435745509,
5.08762612892618));
#173264=CARTESIAN_POINT('Ctrl Pts',(18.7796960555114,-21.068510753617,5.08831827726249));
#173265=CARTESIAN_POINT('Ctrl Pts',(18.7755859595699,-21.0685954994511,
5.08856817367552));
#173266=CARTESIAN_POINT('Ctrl Pts',(18.7679044559218,-21.0687315004401,
5.08903392288986));
#173267=CARTESIAN_POINT('Ctrl Pts',(18.7643332045736,-21.0687856892039,
5.08924993161544));
#173268=CARTESIAN_POINT('Ctrl Pts',(18.7561826605718,-21.0688887313678,
5.08974173868459));
#173269=CARTESIAN_POINT('Ctrl Pts',(18.7516033448229,-21.0689317642705,
5.09001720848254));
#173270=CARTESIAN_POINT('Ctrl Pts',(18.737534159529,-21.0690183201493,5.09086103663999));
#173271=CARTESIAN_POINT('Ctrl Pts',(18.7280439575885,-21.0690128935072,
5.09142672702305));
#173272=CARTESIAN_POINT('Ctrl Pts',(18.6431563082706,-21.0683935185377,
5.09645789482124));
#173273=CARTESIAN_POINT('Ctrl Pts',(18.5678330642437,-21.0638156197783,
5.10071966128931));
#173274=CARTESIAN_POINT('Ctrl Pts',(18.450068703757,-21.0503162925105,5.10728216443256));
#173275=CARTESIAN_POINT('Ctrl Pts',(18.4073891580195,-21.0440979409608,
5.10963935816056));
#173276=CARTESIAN_POINT('Ctrl Pts',(18.2572776141251,-21.0175209278849,
5.11793903805176));
#173277=CARTESIAN_POINT('Ctrl Pts',(18.1512660832122,-20.9901514252831,
5.12382591142329));
#173278=CARTESIAN_POINT('Ctrl Pts',(17.9957399364974,-20.9368664675411,
5.13296741886644));
#173279=CARTESIAN_POINT('Ctrl Pts',(17.9443529688159,-20.9169884826622,
5.13607331392347));
#173280=CARTESIAN_POINT('Ctrl Pts',(17.8623244915629,-20.8815198603959,
5.14121488036626));
#173281=CARTESIAN_POINT('Ctrl Pts',(17.8311837891009,-20.8671469334335,
5.14321121316726));
#173282=CARTESIAN_POINT('Ctrl Pts',(17.7907074600633,-20.8472585530818,
5.1458709694105));
#173283=CARTESIAN_POINT('Ctrl Pts',(17.7810445492673,-20.8424183931852,
5.14651088463052));
#173284=CARTESIAN_POINT('Ctrl Pts',(17.7652757072066,-20.8343681426957,
5.14756347971931));
#173285=CARTESIAN_POINT('Ctrl Pts',(17.7591475806824,-20.8312017823808,
5.14797461894549));
#173286=CARTESIAN_POINT('Ctrl Pts',(17.7473131699517,-20.8250135589137,
5.14877267590951));
#173287=CARTESIAN_POINT('Ctrl Pts',(17.7416050148993,-20.8219954236787,
5.14915945841463));
#173288=CARTESIAN_POINT('Ctrl Pts',(17.7284539648584,-20.8149647521691,
5.15005489779027));
#173289=CARTESIAN_POINT('Ctrl Pts',(17.7210211612614,-20.8109336635934,
5.15056421107067));
#173290=CARTESIAN_POINT('Ctrl Pts',(17.7010897608731,-20.7999690809423,
5.15193875404837));
#173291=CARTESIAN_POINT('Ctrl Pts',(17.6886370695332,-20.7929534524509,
5.15280691336821));
#173292=CARTESIAN_POINT('Ctrl Pts',(17.5748446652883,-20.7273179688134,
5.16082807579894));
#173293=CARTESIAN_POINT('Ctrl Pts',(17.4784763014697,-20.6605219849814,
5.16828407250825));
#173294=CARTESIAN_POINT('Ctrl Pts',(17.2619802702192,-20.4822146764628,
5.1866057889009));
#173295=CARTESIAN_POINT('Ctrl Pts',(17.1482855190796,-20.3640583589844,
5.19761341248368));
#173296=CARTESIAN_POINT('Ctrl Pts',(17.0301312372366,-20.20879106028,5.21000148021404));
#173297=CARTESIAN_POINT('Ctrl Pts',(17.0115145700478,-20.1831525995034,
5.21198579601905));
#173298=CARTESIAN_POINT('Ctrl Pts',(16.9893908703803,-20.151199552754,5.21437539162412));
#173299=CARTESIAN_POINT('Ctrl Pts',(16.9853324635605,-20.1452738298009,
5.21481510182035));
#173300=CARTESIAN_POINT('Ctrl Pts',(16.9790064012734,-20.1359354939914,
5.21550250549595));
#173301=CARTESIAN_POINT('Ctrl Pts',(16.97671840577,-20.1325368205786,5.21575154220205));
#173302=CARTESIAN_POINT('Ctrl Pts',(16.9724531169237,-20.1261611263267,
5.21621655077545));
#173303=CARTESIAN_POINT('Ctrl Pts',(16.9704735177931,-20.1231857746006,
5.21643267337742));
#173304=CARTESIAN_POINT('Ctrl Pts',(16.9659626667949,-20.1163685647674,
5.21692585995881));
#173305=CARTESIAN_POINT('Ctrl Pts',(16.963436402639,-20.1125234658731,5.21720258826067));
#173306=CARTESIAN_POINT('Ctrl Pts',(16.9568612413429,-20.1024443004704,
5.21792429528379));
#173307=CARTESIAN_POINT('Ctrl Pts',(16.9528325684129,-20.0961970286344,
5.21836795778722));
#173308=CARTESIAN_POINT('Ctrl Pts',(16.9263026459696,-20.0545773327195,
5.22130031036703));
#173309=CARTESIAN_POINT('Ctrl Pts',(16.9048218062812,-20.0185618413852,
5.22372636744759));
#173310=CARTESIAN_POINT('Ctrl Pts',(16.8738470304827,-19.9629364588946,
5.22734407529229));
#173311=CARTESIAN_POINT('Ctrl Pts',(16.8635636945988,-19.9437810610351,
5.22856737227146));
#173312=CARTESIAN_POINT('Ctrl Pts',(16.8457316295034,-19.9092999763928,
5.23073541025197));
#173313=CARTESIAN_POINT('Ctrl Pts',(16.8380700257995,-19.8940351563942,
5.23168355136719));
#173314=CARTESIAN_POINT('Ctrl Pts',(16.7722507223706,-19.7588417841076,
5.23999251737901));
#173315=CARTESIAN_POINT('Ctrl Pts',(16.725354489134,-19.6337616411367,5.24709266585253));
#173316=CARTESIAN_POINT('Ctrl Pts',(16.6648838059536,-19.4103478525176,
5.25986483766746));
#173317=CARTESIAN_POINT('Ctrl Pts',(16.6458617350985,-19.3139386783995,
5.26540003836287));
#173318=CARTESIAN_POINT('Ctrl Pts',(16.6317631833846,-19.20200921222,5.27201864577449));
#173319=CARTESIAN_POINT('Ctrl Pts',(16.6300811152558,-19.1874348095121,
5.27288398235805));
#173320=CARTESIAN_POINT('Ctrl Pts',(16.6277432511404,-19.1651464696357,
5.27421314451305));
#173321=CARTESIAN_POINT('Ctrl Pts',(16.6269780363118,-19.1574442789052,
5.27467352219713));
#173322=CARTESIAN_POINT('Ctrl Pts',(16.6257184970612,-19.144018505712,5.27547791919846));
#173323=CARTESIAN_POINT('Ctrl Pts',(16.625205197021,-19.1382967527706,5.27582133732469));
#173324=CARTESIAN_POINT('Ctrl Pts',(16.624103385343,-19.125426421594,5.27659519695625));
#173325=CARTESIAN_POINT('Ctrl Pts',(16.6235279050008,-19.1182768249215,
5.27702604414088));
#173326=CARTESIAN_POINT('Ctrl Pts',(16.6220830311269,-19.0991085335299,
5.27818379609974));
#173327=CARTESIAN_POINT('Ctrl Pts',(16.6212799116607,-19.0870852433443,
5.27891277238418));
#173328=CARTESIAN_POINT('Ctrl Pts',(16.6181723376117,-19.0337143086554,
5.28216140712792));
#173329=CARTESIAN_POINT('Ctrl Pts',(16.6169788915316,-18.9923134308124,
5.28471557896899));
#173330=CARTESIAN_POINT('Ctrl Pts',(16.617087834612,-18.7814276676958,5.29790820125772));
#173331=CARTESIAN_POINT('Ctrl Pts',(16.6375272207331,-18.6125948183922,
5.30913937462206));
#173332=CARTESIAN_POINT('Ctrl Pts',(16.6963015742312,-18.3727973722924,
5.32541879940326));
#173333=CARTESIAN_POINT('Ctrl Pts',(16.7188568526094,-18.2986358842749,
5.3304889857474));
#173334=CARTESIAN_POINT('Ctrl Pts',(16.7454193844609,-18.2258897222169,
5.33540091855303));
#173335=CARTESIAN_POINT('Origin',(18.734,-18.952,0.));
#173336=CARTESIAN_POINT('',(16.7454193692319,-18.2258897639242,6.35350369657411));
#173337=CARTESIAN_POINT('',(16.7454193692319,-18.2258897639242,6.13370787796071));
#173338=CARTESIAN_POINT('',(16.7454193692319,-18.2258897639242,0.));
#173339=CARTESIAN_POINT('',(16.6170008387226,-18.9506676920045,6.31236769265572));
#173340=CARTESIAN_POINT('Ctrl Pts',(16.7454193692319,-18.2258897639243,
6.3535036965741));
#173341=CARTESIAN_POINT('Ctrl Pts',(16.7445879657081,-18.2281667087484,
6.35335894716062));
#173342=CARTESIAN_POINT('Ctrl Pts',(16.7437604676845,-18.2304450957259,
6.35321441845044));
#173343=CARTESIAN_POINT('Ctrl Pts',(16.7316385710274,-18.2640003541916,
6.35109037726281));
#173344=CARTESIAN_POINT('Ctrl Pts',(16.7210780199771,-18.2955396540834,
6.34915175896324));
#173345=CARTESIAN_POINT('Ctrl Pts',(16.6634370111024,-18.4821822421839,
6.33794484181155));
#173346=CARTESIAN_POINT('Ctrl Pts',(16.6335480199623,-18.6420437528863,
6.32937665650607));
#173347=CARTESIAN_POINT('Ctrl Pts',(16.618764144361,-18.8526586204593,6.31781740961247));
#173348=CARTESIAN_POINT('Ctrl Pts',(16.6170313257821,-18.9016549965022,
6.31511280070357));
#173349=CARTESIAN_POINT('Ctrl Pts',(16.6170004208958,-18.9506650571224,
6.3123685677428));
#173350=CARTESIAN_POINT('Ctrl Pts',(16.6170004192105,-18.950667732362,6.31236841794738));
#173351=CARTESIAN_POINT('Ctrl Pts',(16.6169589235782,-19.0166051114148,
6.30867636740193));
#173352=CARTESIAN_POINT('Ctrl Pts',(16.6199979904649,-19.0825044489203,
6.30491530142379));
#173353=CARTESIAN_POINT('Ctrl Pts',(16.6271997938263,-19.1598966693579,
6.30036722445836));
#173354=CARTESIAN_POINT('Ctrl Pts',(16.6283908363858,-19.1716319094263,
6.29967406401305));
#173355=CARTESIAN_POINT('Ctrl Pts',(16.6305234250977,-19.1910290350328,
6.29852224835313));
#173356=CARTESIAN_POINT('Ctrl Pts',(16.6314089287677,-19.1986969102738,
6.29806534581304));
#173357=CARTESIAN_POINT('Ctrl Pts',(16.6330729561629,-19.212446045737,6.29724317617807));
#173358=CARTESIAN_POINT('Ctrl Pts',(16.6338360029738,-19.2185291178272,
6.29687839895436));
#173359=CARTESIAN_POINT('Ctrl Pts',(16.6354355559125,-19.2308473608446,
6.29613761458187));
#173360=CARTESIAN_POINT('Ctrl Pts',(16.6362734530907,-19.2370822858573,
6.29576156702282));
#173361=CARTESIAN_POINT('Ctrl Pts',(16.6381348447124,-19.2504805029742,
6.29495108088364));
#173362=CARTESIAN_POINT('Ctrl Pts',(16.6391672979084,-19.2576424512848,
6.2945163629894));
#173363=CARTESIAN_POINT('Ctrl Pts',(16.642059177247,-19.2769996537484,6.29333735088658));
#173364=CARTESIAN_POINT('Ctrl Pts',(16.6439884938243,-19.2891840369773,
6.2925908510825));
#173365=CARTESIAN_POINT('Ctrl Pts',(16.6533161529773,-19.3449329706041,
6.28915476773769));
#173366=CARTESIAN_POINT('Ctrl Pts',(16.6619704192879,-19.3882734790275,
6.28642560721673));
#173367=CARTESIAN_POINT('Ctrl Pts',(16.681085743994,-19.4705091403054,6.28113243164965));
#173368=CARTESIAN_POINT('Ctrl Pts',(16.6913131117228,-19.5094393553305,
6.27857651366147));
#173369=CARTESIAN_POINT('Ctrl Pts',(16.7452404049068,-19.693224414201,6.26627806706897));
#173370=CARTESIAN_POINT('Ctrl Pts',(16.8032757919129,-19.833405046162,6.25616035700209));
#173371=CARTESIAN_POINT('Ctrl Pts',(16.9019242599444,-20.0141554369697,
6.24267850398749));
#173372=CARTESIAN_POINT('Ctrl Pts',(16.929955191671,-20.0610982082332,6.23913809436873));
#173373=CARTESIAN_POINT('Ctrl Pts',(16.9751922023063,-20.1305936367556,
6.23389087200403));
#173374=CARTESIAN_POINT('Ctrl Pts',(16.991084804231,-20.1539711440418,6.23212480632293));
#173375=CARTESIAN_POINT('Ctrl Pts',(17.0114495429772,-20.182673349827,6.22996217357871));
#173376=CARTESIAN_POINT('Ctrl Pts',(17.0154851701229,-20.1883024522825,
6.22953831573068));
#173377=CARTESIAN_POINT('Ctrl Pts',(17.0219186703776,-20.1971838601842,
6.22887014442115));
#173378=CARTESIAN_POINT('Ctrl Pts',(17.0242983117426,-20.2004492231188,
6.22862460723963));
#173379=CARTESIAN_POINT('Ctrl Pts',(17.0288065179394,-20.2065983561217,
6.22816249371857));
#173380=CARTESIAN_POINT('Ctrl Pts',(17.0309330312536,-20.2094834975402,
6.22794578807074));
#173381=CARTESIAN_POINT('Ctrl Pts',(17.0358149821053,-20.2160719723384,
6.22745116515522));
#173382=CARTESIAN_POINT('Ctrl Pts',(17.0385752081386,-20.2197716996052,
6.22717358598846));
#173383=CARTESIAN_POINT('Ctrl Pts',(17.0459422768841,-20.2295792148904,
6.22643813489804));
#173384=CARTESIAN_POINT('Ctrl Pts',(17.0505702126507,-20.2356711736097,
6.22598169817505));
#173385=CARTESIAN_POINT('Ctrl Pts',(17.0834118429753,-20.2784190071789,
6.22278055155043));
#173386=CARTESIAN_POINT('Ctrl Pts',(17.112789510265,-20.3141695511646,6.22011224294324));
#173387=CARTESIAN_POINT('Ctrl Pts',(17.1681251004714,-20.377180061586,6.21536677188298));
#173388=CARTESIAN_POINT('Ctrl Pts',(17.1936820139472,-20.4047639650173,
6.21327339968138));
#173389=CARTESIAN_POINT('Ctrl Pts',(17.2454134775468,-20.4576976075686,
6.20919107428181));
#173390=CARTESIAN_POINT('Ctrl Pts',(17.271534277295,-20.4830810677156,6.20720160430701));
#173391=CARTESIAN_POINT('Ctrl Pts',(17.3785990815193,-20.5818825497916,
6.1992701886771));
#173392=CARTESIAN_POINT('Ctrl Pts',(17.4645168941252,-20.649657364387,6.19338603766223));
#173393=CARTESIAN_POINT('Ctrl Pts',(17.6009752904639,-20.7411256077791,
6.18425085872232));
#173394=CARTESIAN_POINT('Ctrl Pts',(17.6478458904249,-20.7699615069063,
6.18114859054433));
#173395=CARTESIAN_POINT('Ctrl Pts',(17.7156177725683,-20.8080992950845,
6.17667442661243));
#173396=CARTESIAN_POINT('Ctrl Pts',(17.7356297280632,-20.8189396610462,
6.17535475344012));
#173397=CARTESIAN_POINT('Ctrl Pts',(17.7711481074409,-20.8374453782201,
6.17301265653074));
#173398=CARTESIAN_POINT('Ctrl Pts',(17.7865811598294,-20.8452473573717,
6.17199504449517));
#173399=CARTESIAN_POINT('Ctrl Pts',(17.8094981274425,-20.8564823529428,
6.17048330742093));
#173400=CARTESIAN_POINT('Ctrl Pts',(17.8169095110432,-20.8600623095636,
6.16999431049844));
#173401=CARTESIAN_POINT('Ctrl Pts',(17.8298642262263,-20.8662269744544,
6.16913931828668));
#173402=CARTESIAN_POINT('Ctrl Pts',(17.8353982661557,-20.868831064509,6.16877400061096));
#173403=CARTESIAN_POINT('Ctrl Pts',(17.8464424480703,-20.8739696607753,
6.16804475200748));
#173404=CARTESIAN_POINT('Ctrl Pts',(17.8519523521697,-20.8765045416145,
6.1676808383766));
#173405=CARTESIAN_POINT('Ctrl Pts',(17.8651280114369,-20.8824976535387,
6.16681036374622));
#173406=CARTESIAN_POINT('Ctrl Pts',(17.8728035858138,-20.8859339326431,
6.16630305367577));
#173407=CARTESIAN_POINT('Ctrl Pts',(17.900446064772,-20.8981120038595,6.16447517593854));
#173408=CARTESIAN_POINT('Ctrl Pts',(17.920526696827,-20.9065908072475,6.16314568322973));
#173409=CARTESIAN_POINT('Ctrl Pts',(18.1155344023314,-20.9854048941387,
6.15021472296584));
#173410=CARTESIAN_POINT('Ctrl Pts',(18.2989582507223,-21.032371339003,6.13778451101057));
#173411=CARTESIAN_POINT('Ctrl Pts',(18.5638257376764,-21.0635992777619,
6.12018172853438));
#173412=CARTESIAN_POINT('Ctrl Pts',(18.641983042084,-21.0684463904165,6.11504564636913));
#173413=CARTESIAN_POINT('Ctrl Pts',(18.7557447730535,-21.0691861622347,
6.10779693945435));
#173414=CARTESIAN_POINT('Ctrl Pts',(18.7912584058533,-21.0685235410227,
6.10556662027387));
#173415=CARTESIAN_POINT('Ctrl Pts',(18.8341683241406,-21.0666419508439,
6.10292434407441));
#173416=CARTESIAN_POINT('Ctrl Pts',(18.8415941572181,-21.0662771281299,
6.10246898963634));
#173417=CARTESIAN_POINT('Ctrl Pts',(18.8531643015383,-21.0656475845377,
6.10176264131586));
#173418=CARTESIAN_POINT('Ctrl Pts',(18.8573099317897,-21.0654097813223,
6.10151018176803));
#173419=CARTESIAN_POINT('Ctrl Pts',(18.8650149715528,-21.0649450531459,
6.10104216361974));
#173420=CARTESIAN_POINT('Ctrl Pts',(18.8685744727273,-21.0647213332441,
6.10082643377388));
#173421=CARTESIAN_POINT('Ctrl Pts',(18.8766436548562,-21.0641936976585,
6.10033846292882));
#173422=CARTESIAN_POINT('Ctrl Pts',(18.8811529268464,-21.0638843353011,
6.10006653039827));
#173423=CARTESIAN_POINT('Ctrl Pts',(18.8928092632662,-21.0630471278457,
6.09936547486492));
#173424=CARTESIAN_POINT('Ctrl Pts',(18.899954767083,-21.0624974239907,6.09893754799677));
#173425=CARTESIAN_POINT('Ctrl Pts',(18.9441612624284,-21.0588707163678,
6.09630070388491));
#173426=CARTESIAN_POINT('Ctrl Pts',(18.9811410832951,-21.0548536884396,
6.09414092412532));
#173427=CARTESIAN_POINT('Ctrl Pts',(19.1867552431878,-21.0270186771987,
6.08229475508146));
#173428=CARTESIAN_POINT('Ctrl Pts',(19.3521537696724,-20.9838926253637,
6.07333414141544));
#173429=CARTESIAN_POINT('Ctrl Pts',(19.5990582330958,-20.8865291080759,
6.05873241540789));
#173430=CARTESIAN_POINT('Ctrl Pts',(19.6850469190682,-20.8457358116979,
6.05340058994421));
#173431=CARTESIAN_POINT('Ctrl Pts',(19.7866309135426,-20.7888759189048,
6.04662151622879));
#173432=CARTESIAN_POINT('Ctrl Pts',(19.8051048928457,-20.7781651735305,
6.04536850629302));
#173433=CARTESIAN_POINT('Ctrl Pts',(19.8311329972267,-20.762543909398,6.04357282918225));
#173434=CARTESIAN_POINT('Ctrl Pts',(19.838823056954,-20.7578615867422,6.04303847120485));
#173435=CARTESIAN_POINT('Ctrl Pts',(19.8520345748599,-20.7497013846639,
6.04211372413928));
#173436=CARTESIAN_POINT('Ctrl Pts',(19.8575702922207,-20.7462467433365,
6.04172419405976));
#173437=CARTESIAN_POINT('Ctrl Pts',(19.8681366691222,-20.7395845744625,
6.04097668914648));
#173438=CARTESIAN_POINT('Ctrl Pts',(19.8731699215115,-20.7363812608003,
6.04061887319687));
#173439=CARTESIAN_POINT('Ctrl Pts',(19.8862180549583,-20.7279993271395,
6.03968669117099));
#173440=CARTESIAN_POINT('Ctrl Pts',(19.8942115166272,-20.7227877592174,
6.03911109901927));
#173441=CARTESIAN_POINT('Ctrl Pts',(19.9213240105203,-20.7048486013623,
6.03714312929067));
#173442=CARTESIAN_POINT('Ctrl Pts',(19.9402705076473,-20.6918643402368,
6.03574112578493));
#173443=CARTESIAN_POINT('Ctrl Pts',(20.1024104767653,-20.5768263487607,
6.02350465632215));
#173444=CARTESIAN_POINT('Ctrl Pts',(20.2325583640737,-20.4576251699998,
6.01196334054752));
#173445=CARTESIAN_POINT('Ctrl Pts',(20.402675028537,-20.2576574616752,5.99461738879427));
#173446=CARTESIAN_POINT('Ctrl Pts',(20.4547854833156,-20.1881702913624,
5.98889944139805));
#173447=CARTESIAN_POINT('Ctrl Pts',(20.5232432545789,-20.0841322743137,
5.98094848913989));
#173448=CARTESIAN_POINT('Ctrl Pts',(20.5431537418779,-20.0520354799077,
5.97857330402471));
#173449=CARTESIAN_POINT('Ctrl Pts',(20.5660122068564,-20.0128852679587,
5.97578361078896));
#173450=CARTESIAN_POINT('Ctrl Pts',(20.5697931969881,-20.0063289902624,
5.97531997647551));
#173451=CARTESIAN_POINT('Ctrl Pts',(20.5756085244748,-19.9961190197423,
5.97460361754594));
#173452=CARTESIAN_POINT('Ctrl Pts',(20.5776672888977,-19.9924794151507,
5.97434936064464));
#173453=CARTESIAN_POINT('Ctrl Pts',(20.5814606986839,-19.9857265922021,
5.97387970186458));
#173454=CARTESIAN_POINT('Ctrl Pts',(20.5831982516336,-19.982615120722,5.97366411811812));
#173455=CARTESIAN_POINT('Ctrl Pts',(20.5871028301655,-19.9755814474733,
5.97317861201329));
#173456=CARTESIAN_POINT('Ctrl Pts',(20.5892652587948,-19.971656755549,5.97290898499985));
#173457=CARTESIAN_POINT('Ctrl Pts',(20.5955940859986,-19.9600834872905,
5.97211756886456));
#173458=CARTESIAN_POINT('Ctrl Pts',(20.5997258220393,-19.9524159241269,
5.97159793801832));
#173459=CARTESIAN_POINT('Ctrl Pts',(20.6287422339887,-19.8977630282585,
5.96792583736771));
#173460=CARTESIAN_POINT('Ctrl Pts',(20.6518986191712,-19.8498762364502,
5.96487407255763));
#173461=CARTESIAN_POINT('Ctrl Pts',(20.6798587385253,-19.7860239503508,
5.96095337059357));
#173462=CARTESIAN_POINT('Ctrl Pts',(20.6863110483281,-19.7708063083639,
5.96002974072647));
#173463=CARTESIAN_POINT('Ctrl Pts',(20.7492249714697,-19.617452190958,5.95081513922359));
#173464=CARTESIAN_POINT('Ctrl Pts',(20.7911099715278,-19.4737858125974,
5.94290576256185));
#173465=CARTESIAN_POINT('Ctrl Pts',(20.828449987223,-19.2662674724425,5.93123962701694));
#173466=CARTESIAN_POINT('Ctrl Pts',(20.8367077414126,-19.2051878649734,
5.92778193483492));
#173467=CARTESIAN_POINT('Ctrl Pts',(20.8456586459258,-19.1068179851342,
5.92211297374943));
#173468=CARTESIAN_POINT('Ctrl Pts',(20.8480513818264,-19.0697172561207,
5.91995250223802));
#173469=CARTESIAN_POINT('Ctrl Pts',(20.8498895438205,-19.0214566160792,
5.9171055593353));
#173470=CARTESIAN_POINT('Ctrl Pts',(20.8502253424791,-19.010335888353,5.9164470298258));
#173471=CARTESIAN_POINT('Ctrl Pts',(20.8506288613221,-18.9922469400273,
5.9153715970044));
#173472=CARTESIAN_POINT('Ctrl Pts',(20.8507498648743,-18.9852800320589,
5.91495636757392));
#173473=CARTESIAN_POINT('Ctrl Pts',(20.8509164090886,-18.9718816868263,
5.91415579336967));
#173474=CARTESIAN_POINT('Ctrl Pts',(20.8509670404518,-18.9654503815805,
5.91377061271823));
#173475=CARTESIAN_POINT('Ctrl Pts',(20.8510158622387,-18.9507253274372,
5.91288660615498));
#173476=CARTESIAN_POINT('Ctrl Pts',(20.8509946219938,-18.9424316588326,
5.912387176615));
#173477=CARTESIAN_POINT('Ctrl Pts',(20.850808734445,-18.9204005765702,5.91105635887353));
#173478=CARTESIAN_POINT('Ctrl Pts',(20.8505590980706,-18.9066644489074,
5.91022232399389));
#173479=CARTESIAN_POINT('Ctrl Pts',(20.8476401951111,-18.8020916013823,
5.90383923571801));
#173480=CARTESIAN_POINT('Ctrl Pts',(20.8392585059012,-18.7115208313588,
5.89811144914314));
#173481=CARTESIAN_POINT('Ctrl Pts',(20.8031525277393,-18.4828845147944,
5.8831624275689));
#173482=CARTESIAN_POINT('Ctrl Pts',(20.7674349599478,-18.3465259255292,
5.87376393638202));
#173483=CARTESIAN_POINT('Ctrl Pts',(20.6996503153591,-18.1640735105363,
5.86102482119008));
#173484=CARTESIAN_POINT('Ctrl Pts',(20.6788961788204,-18.1141521829133,
5.85752537179799));
#173485=CARTESIAN_POINT('Ctrl Pts',(20.644500042845,-18.0396044967632,5.85233124189623));
#173486=CARTESIAN_POINT('Ctrl Pts',(20.6322413511948,-18.0143668533074,
5.85057860870479));
#173487=CARTESIAN_POINT('Ctrl Pts',(20.6163422646763,-17.9832253430069,
5.84843003952564));
#173488=CARTESIAN_POINT('Ctrl Pts',(20.613170413408,-17.977087030637,5.84800722677176));
#173489=CARTESIAN_POINT('Ctrl Pts',(20.60809789318,-17.9673871921274,5.84734032449112));
#173490=CARTESIAN_POINT('Ctrl Pts',(20.6062170239817,-17.9638154472006,
5.84709501896253));
#173491=CARTESIAN_POINT('Ctrl Pts',(20.6026464636024,-17.9570817891174,
5.84663308968833));
#173492=CARTESIAN_POINT('Ctrl Pts',(20.6009589780553,-17.9539188275942,
5.8464163380719));
#173493=CARTESIAN_POINT('Ctrl Pts',(20.5970773163752,-17.9466874721828,
5.84592128754615));
#173494=CARTESIAN_POINT('Ctrl Pts',(20.5948778473299,-17.9426219718941,
5.84564332884129));
#173495=CARTESIAN_POINT('Ctrl Pts',(20.5889923492203,-17.9318278358562,
5.84490620685704));
#173496=CARTESIAN_POINT('Ctrl Pts',(20.5852829899473,-17.9251119071071,
5.84444848916911));
#173497=CARTESIAN_POINT('Ctrl Pts',(20.558735100005,-17.8776573982688,5.84121965665632));
#173498=CARTESIAN_POINT('Ctrl Pts',(20.5345886285815,-17.8376609530344,
5.83852643934218));
#173499=CARTESIAN_POINT('Ctrl Pts',(20.5067023993536,-17.7947467154586,
5.83563149080974));
#173500=CARTESIAN_POINT('Ctrl Pts',(20.5042561239897,-17.7910080890895,
5.83537924307333));
#173501=CARTESIAN_POINT('Ctrl Pts',(20.4889651681,-17.7677997155497,5.83381290499945));
#173502=CARTESIAN_POINT('Ctrl Pts',(20.4758109573607,-17.7485351274904,
5.83251073514876));
#173503=CARTESIAN_POINT('Ctrl Pts',(20.4360626303147,-17.6923403059282,
5.82869450340581));
#173504=CARTESIAN_POINT('Ctrl Pts',(20.4085927281712,-17.6560450739698,
5.82620627250336));
#173505=CARTESIAN_POINT('Ctrl Pts',(20.3112069239627,-17.5356439945393,
5.81777526838908));
#173506=CARTESIAN_POINT('Ctrl Pts',(20.2359569921626,-17.4560821128771,
5.81188725839029));
#173507=CARTESIAN_POINT('Ctrl Pts',(20.1140504529712,-17.3457040596506,
5.80274310867441));
#173508=CARTESIAN_POINT('Ctrl Pts',(20.0717732879441,-17.3103277167841,
5.79963569920776));
#173509=CARTESIAN_POINT('Ctrl Pts',(20.0010165637319,-17.2556701441101,
5.79449184930673));
#173510=CARTESIAN_POINT('Ctrl Pts',(19.9733622396418,-17.235361716865,5.79249479329015));
#173511=CARTESIAN_POINT('Ctrl Pts',(19.9363629060227,-17.2095507833398,
5.78983420999984));
#173512=CARTESIAN_POINT('Ctrl Pts',(19.9274509160678,-17.2034346638465,
5.78919420960976));
#173513=CARTESIAN_POINT('Ctrl Pts',(19.912775273546,-17.1935275268055,5.78814151006629));
#173514=CARTESIAN_POINT('Ctrl Pts',(19.9070391663069,-17.1896959124247,
5.78773035215526));
#173515=CARTESIAN_POINT('Ctrl Pts',(19.8958978645778,-17.1823322223919,
5.78693228439748));
#173516=CARTESIAN_POINT('Ctrl Pts',(19.8904950300019,-17.1787967023032,
5.78654550991818));
#173517=CARTESIAN_POINT('Ctrl Pts',(19.8779803887895,-17.1706888667593,
5.78565012623694));
#173518=CARTESIAN_POINT('Ctrl Pts',(19.8708572318772,-17.166134351517,5.7851408608827));
#173519=CARTESIAN_POINT('Ctrl Pts',(19.8516216673883,-17.1539969362302,
5.78376653125884));
#173520=CARTESIAN_POINT('Ctrl Pts',(19.8394596088827,-17.1464939085806,
5.78289853878201));
#173521=CARTESIAN_POINT('Ctrl Pts',(19.7271457697577,-17.0787653843559,
5.77489023814325));
#173522=CARTESIAN_POINT('Ctrl Pts',(19.6222601056303,-17.0268162113851,
5.76744806231527));
#173523=CARTESIAN_POINT('Ctrl Pts',(19.3623098138836,-16.9238457041456,
5.74918452666127));
#173524=CARTESIAN_POINT('Ctrl Pts',(19.2045757370591,-16.8815552105659,
5.73822299193626));
#173525=CARTESIAN_POINT('Ctrl Pts',(19.0114504404594,-16.8530089384606,
5.72581868616253));
#173526=CARTESIAN_POINT('Ctrl Pts',(18.9792388897572,-16.8490020500259,
5.72378472823888));
#173527=CARTESIAN_POINT('Ctrl Pts',(18.9397467944933,-16.84500934631,5.72134388951952));
#173528=CARTESIAN_POINT('Ctrl Pts',(18.932543794116,-16.8443184008294,5.72090084672935));
#173529=CARTESIAN_POINT('Ctrl Pts',(18.9212452374452,-16.8432930256369,
5.72020940423208));
#173530=CARTESIAN_POINT('Ctrl Pts',(18.9171520881604,-16.8429335724214,
5.71995963559178));
#173531=CARTESIAN_POINT('Ctrl Pts',(18.9094986752622,-16.8422839114739,
5.71949399708822));
#173532=CARTESIAN_POINT('Ctrl Pts',(18.9059387629808,-16.8419908006791,
5.71927797207067));
#173533=CARTESIAN_POINT('Ctrl Pts',(18.8978099901034,-16.8413422145912,
5.71878596290514));
#173534=CARTESIAN_POINT('Ctrl Pts',(18.8932407152944,-16.8409925638542,
5.71851030834989));
#173535=CARTESIAN_POINT('Ctrl Pts',(18.8791899348779,-16.8399632478783,
5.71766535145905));
#173536=CARTESIAN_POINT('Ctrl Pts',(18.8697048075751,-16.8393325930649,
5.71709872747489));
#173537=CARTESIAN_POINT('Ctrl Pts',(18.7843129931441,-16.8342324600796,
5.7120289470986));
#173538=CARTESIAN_POINT('Ctrl Pts',(18.7082123316671,-16.8337912368566,
5.70773298215973));
#173539=CARTESIAN_POINT('Ctrl Pts',(18.5898209498408,-16.8394883700714,
5.70117337088389));
#173540=CARTESIAN_POINT('Ctrl Pts',(18.547466633118,-16.8428062037057,5.69885161600951));
#173541=CARTESIAN_POINT('Ctrl Pts',(18.3965609963475,-16.859208907409,5.69058744196724));
#173542=CARTESIAN_POINT('Ctrl Pts',(18.288961472109,-16.8794220256274,5.68470085914685));
#173543=CARTESIAN_POINT('Ctrl Pts',(18.1302307474953,-16.9221761859047,
5.6755600273208));
#173544=CARTESIAN_POINT('Ctrl Pts',(18.0776354836409,-16.9385683513123,
5.6724545195517));
#173545=CARTESIAN_POINT('Ctrl Pts',(17.9934267966454,-16.9684637154784,
5.66731353701058));
#173546=CARTESIAN_POINT('Ctrl Pts',(17.9613969278722,-16.9807189043255,
5.66531738910068));
#173547=CARTESIAN_POINT('Ctrl Pts',(17.919683474215,-16.9978520049024,5.66265784421248));
#173548=CARTESIAN_POINT('Ctrl Pts',(17.909718596724,-17.0020343714392,5.66201795068399));
#173549=CARTESIAN_POINT('Ctrl Pts',(17.8934466830099,-17.0090108851905,
5.66096538213877));
#173550=CARTESIAN_POINT('Ctrl Pts',(17.8871204303578,-17.0117599190403,
5.66055424761143));
#173551=CARTESIAN_POINT('Ctrl Pts',(17.8748983876208,-17.0171420950068,
5.65975619323664));
#173552=CARTESIAN_POINT('Ctrl Pts',(17.8690009808611,-17.0197713933484,
5.6593694085872));
#173553=CARTESIAN_POINT('Ctrl Pts',(17.8554086029071,-17.0259061141775,
5.65847395472911));
#173554=CARTESIAN_POINT('Ctrl Pts',(17.8477224595356,-17.0294307247653,
5.65796462904438));
#173555=CARTESIAN_POINT('Ctrl Pts',(17.8271010189593,-17.0390369725575,
5.65659003103985));
#173556=CARTESIAN_POINT('Ctrl Pts',(17.8142060315361,-17.0452036432742,
5.65572182873334));
#173557=CARTESIAN_POINT('Ctrl Pts',(17.696226356622,-17.1030993784689,5.64769731498152));
#173558=CARTESIAN_POINT('Ctrl Pts',(17.5955588130439,-17.1633269032491,
5.64023771614866));
#173559=CARTESIAN_POINT('Ctrl Pts',(17.3674343851142,-17.3268979014458,
5.62190024953151));
#173560=CARTESIAN_POINT('Ctrl Pts',(17.2459727153523,-17.4373272888777,
5.61087998701859));
#173561=CARTESIAN_POINT('Ctrl Pts',(17.1177578285452,-17.5843594953859,
5.59849616104893));
#173562=CARTESIAN_POINT('Ctrl Pts',(17.0976054366513,-17.6085371665684,
5.59652525315303));
#173563=CARTESIAN_POINT('Ctrl Pts',(17.073533379214,-17.6387631700887,5.59414952095432));
#173564=CARTESIAN_POINT('Ctrl Pts',(17.0690967400017,-17.6443924486247,
5.59371072714514));
#173565=CARTESIAN_POINT('Ctrl Pts',(17.0621710439961,-17.6532722761588,
5.59302443430166));
#173566=CARTESIAN_POINT('Ctrl Pts',(17.0596627288536,-17.6565076372618,
5.59277559907393));
#173567=CARTESIAN_POINT('Ctrl Pts',(17.0549819911819,-17.662581409482,5.59231076245265));
#173568=CARTESIAN_POINT('Ctrl Pts',(17.0528073968767,-17.665418013911,5.59209461154477));
#173569=CARTESIAN_POINT('Ctrl Pts',(17.0478470428556,-17.6719224953121,
5.59160109431123));
#173570=CARTESIAN_POINT('Ctrl Pts',(17.0450660668932,-17.6755939582505,
5.59132406536616));
#173571=CARTESIAN_POINT('Ctrl Pts',(17.0378180122053,-17.6852280509601,
5.59060105794398));
#173572=CARTESIAN_POINT('Ctrl Pts',(17.0333703441385,-17.6912052966883,
5.59015640342551));
#173573=CARTESIAN_POINT('Ctrl Pts',(17.0039154241879,-17.7312293850776,
5.58720407982091));
#173574=CARTESIAN_POINT('Ctrl Pts',(16.9798986668736,-17.7659972236289,
5.58476001796528));
#173575=CARTESIAN_POINT('Ctrl Pts',(16.9164817125184,-17.8639479554217,
5.57813172056542));
#173576=CARTESIAN_POINT('Ctrl Pts',(16.8793476037037,-17.928527502961,5.57404405300756));
#173577=CARTESIAN_POINT('Ctrl Pts',(16.8077026002861,-18.0698842851205,
5.56540885297391));
#173578=CARTESIAN_POINT('Ctrl Pts',(16.7742225791892,-18.1470070983212,
5.56087765657378));
#173579=CARTESIAN_POINT('Ctrl Pts',(16.7454193466937,-18.2258898256491,
5.55626851740655));
#173580=CARTESIAN_POINT('',(16.6170004656572,-18.950595866038,6.0890562790225));
#173581=CARTESIAN_POINT('Ctrl Pts',(16.7454193844609,-18.2258897222169,
5.33540091855303));
#173582=CARTESIAN_POINT('Ctrl Pts',(16.754433949033,-18.2012017527527,5.33706788824166));
#173583=CARTESIAN_POINT('Ctrl Pts',(16.7639100417315,-18.1766767755762,
5.33871640463477));
#173584=CARTESIAN_POINT('Ctrl Pts',(16.7775028833961,-18.1433580018566,
5.34093968279766));
#173585=CARTESIAN_POINT('Ctrl Pts',(16.7812238464402,-18.1344132151779,
5.34153491144854));
#173586=CARTESIAN_POINT('Ctrl Pts',(16.7868091135376,-18.1212425274892,
5.34240859319378));
#173587=CARTESIAN_POINT('Ctrl Pts',(16.788625993279,-18.1169968255376,5.34268980745089));
#173588=CARTESIAN_POINT('Ctrl Pts',(16.7918742109987,-18.1094745084244,
5.34318724763144));
#173589=CARTESIAN_POINT('Ctrl Pts',(16.7932999700237,-18.1061955435284,
5.34340380796438));
#173590=CARTESIAN_POINT('Ctrl Pts',(16.7963728336157,-18.0991772406288,
5.3438667388128));
#173591=CARTESIAN_POINT('Ctrl Pts',(16.7980224537718,-18.0954390646537,
5.34411295281316));
#173592=CARTESIAN_POINT('Ctrl Pts',(16.802581091417,-18.0851892579945,5.34478713183788));
#173593=CARTESIAN_POINT('Ctrl Pts',(16.8055122379532,-18.0786874455159,
5.34521376302037));
#173594=CARTESIAN_POINT('Ctrl Pts',(16.8213484050857,-18.0440285090467,
5.34748314738849));
#173595=CARTESIAN_POINT('Ctrl Pts',(16.8348380680208,-18.0161407498361,
5.34929205450183));
#173596=CARTESIAN_POINT('Ctrl Pts',(16.9233519448441,-17.8429551722759,
5.36047870226354));
#173597=CARTESIAN_POINT('Ctrl Pts',(17.0143947010761,-17.7064492099266,
5.36912121828694));
#173598=CARTESIAN_POINT('Ctrl Pts',(17.1964660723114,-17.4920196930226,
5.38451635750169));
#173599=CARTESIAN_POINT('Ctrl Pts',(17.2800215745483,-17.408790855096,5.39108660895357));
#173600=CARTESIAN_POINT('Ctrl Pts',(17.3809923330986,-17.323729818445,5.39882093143983));
#173601=CARTESIAN_POINT('Ctrl Pts',(17.3920227743658,-17.3146269081943,
5.39966310887849));
#173602=CARTESIAN_POINT('Ctrl Pts',(17.4097221163854,-17.3003194541485,
5.40101055987238));
#173603=CARTESIAN_POINT('Ctrl Pts',(17.41633156251,-17.2950418157808,5.40151288620035));
#173604=CARTESIAN_POINT('Ctrl Pts',(17.4280424976652,-17.2858050234679,
5.40240152660719));
#173605=CARTESIAN_POINT('Ctrl Pts',(17.4331308359691,-17.2818293157964,
5.40278717356146));
#173606=CARTESIAN_POINT('Ctrl Pts',(17.4436912485878,-17.2736556097667,
5.40358663896818));
#173607=CARTESIAN_POINT('Ctrl Pts',(17.449165801305,-17.2694609525151,5.40400058321099));
#173608=CARTESIAN_POINT('Ctrl Pts',(17.4632677460002,-17.2587648602399,
5.40506563981983));
#173609=CARTESIAN_POINT('Ctrl Pts',(17.4719245038197,-17.2523026342785,
5.40571827917524));
#173610=CARTESIAN_POINT('Ctrl Pts',(17.5082358074039,-17.2256267779826,
5.40845127344328));
#173611=CARTESIAN_POINT('Ctrl Pts',(17.5363281837713,-17.2060205147779,
5.4105548943404));
#173612=CARTESIAN_POINT('Ctrl Pts',(17.6107287412886,-17.1567354307796,
5.41610184893497));
#173613=CARTESIAN_POINT('Ctrl Pts',(17.6577374024471,-17.1281657972743,
5.41958343856949));
#173614=CARTESIAN_POINT('Ctrl Pts',(17.8013463570321,-17.0483736930509,
5.43014241484471));
#173615=CARTESIAN_POINT('Ctrl Pts',(17.900852237189,-17.0027700825176,5.43736822709063));
#173616=CARTESIAN_POINT('Ctrl Pts',(18.0393905078837,-16.9518312356504,
5.44711888988099));
#173617=CARTESIAN_POINT('Ctrl Pts',(18.0757095445325,-16.9395857263662,
5.44964641887755));
#173618=CARTESIAN_POINT('Ctrl Pts',(18.1433564257909,-16.9188050095241,
5.45428269774576));
#173619=CARTESIAN_POINT('Ctrl Pts',(18.1745873804996,-16.9099913405522,
5.45639562427383));
#173620=CARTESIAN_POINT('Ctrl Pts',(18.2118426580303,-16.900396482765,5.45887513073604));
#173621=CARTESIAN_POINT('Ctrl Pts',(18.2176821772654,-16.8989190983179,
5.45926259046659));
#173622=CARTESIAN_POINT('Ctrl Pts',(18.2659510721549,-16.8869261459276,
5.46245510065301));
#173623=CARTESIAN_POINT('Ctrl Pts',(18.3086939618794,-16.8777012746337,
5.46521733624854));
#173624=CARTESIAN_POINT('Ctrl Pts',(18.359096822264,-16.8684469671571,5.46837568582161));
#173625=CARTESIAN_POINT('Ctrl Pts',(18.3665059278418,-16.8671274033791,
5.46883746635955));
#173626=CARTESIAN_POINT('Ctrl Pts',(18.378482948755,-16.8650601235504,5.46957975652983));
#173627=CARTESIAN_POINT('Ctrl Pts',(18.3830464792807,-16.8642878433857,
5.46986160625586));
#173628=CARTESIAN_POINT('Ctrl Pts',(18.3911409504078,-16.8629453180559,
5.47035974958842));
#173629=CARTESIAN_POINT('Ctrl Pts',(18.3946708375065,-16.8623690488016,
5.47057638112279));
#173630=CARTESIAN_POINT('Ctrl Pts',(18.4022300915659,-16.8611546278822,
5.47103899954019));
#173631=CARTESIAN_POINT('Ctrl Pts',(18.4062598365983,-16.8605191781447,
5.47128483233343));
#173632=CARTESIAN_POINT('Ctrl Pts',(18.4173105656312,-16.8588093135312,
5.47195689265315));
#173633=CARTESIAN_POINT('Ctrl Pts',(18.424335233447,-16.8577585661216,5.472381800274));
#173634=CARTESIAN_POINT('Ctrl Pts',(18.4616235699675,-16.8523727111395,
5.47462571418014));
#173635=CARTESIAN_POINT('Ctrl Pts',(18.4919748908451,-16.8486579597797,
5.47641176801372));
#173636=CARTESIAN_POINT('Ctrl Pts',(18.5836894513795,-16.8394445994394,
5.48171583979441));
#173637=CARTESIAN_POINT('Ctrl Pts',(18.6452253183669,-16.8359650902674,
5.48515016186904));
#173638=CARTESIAN_POINT('Ctrl Pts',(18.8537589470336,-16.8332884446971,
5.49661962330192));
#173639=CARTESIAN_POINT('Ctrl Pts',(19.0004825832405,-16.8467046089495,
5.504434456642));
#173640=CARTESIAN_POINT('Ctrl Pts',(19.2184209579186,-16.889796715592,5.51683517791733));
#173641=CARTESIAN_POINT('Ctrl Pts',(19.2913689040297,-16.9083062428076,
5.52111972714955));
#173642=CARTESIAN_POINT('Ctrl Pts',(19.3757170650484,-16.9345608256659,
5.52630296666846));
#173643=CARTESIAN_POINT('Ctrl Pts',(19.3882248313633,-16.9385821417002,
5.5270775392275));
#173644=CARTESIAN_POINT('Ctrl Pts',(19.4084805652702,-16.9453031444008,
5.52834198027179));
#173645=CARTESIAN_POINT('Ctrl Pts',(19.4162518112928,-16.9479319456934,
5.52882951243624));
#173646=CARTESIAN_POINT('Ctrl Pts',(19.4300586123929,-16.9526920256414,
5.52970008530443));
#173647=CARTESIAN_POINT('Ctrl Pts',(19.4361001817187,-16.9548056424922,
5.53008253662895));
#173648=CARTESIAN_POINT('Ctrl Pts',(19.448805687718,-16.9593153842814,5.53089005612648));
#173649=CARTESIAN_POINT('Ctrl Pts',(19.4554673613867,-16.9617176096161,
5.53131532358104));
#173650=CARTESIAN_POINT('Ctrl Pts',(19.4730455196085,-16.9681562104988,
5.53244250022741));
#173651=CARTESIAN_POINT('Ctrl Pts',(19.4839408719425,-16.9722492224249,
5.53314629423618));
#173652=CARTESIAN_POINT('Ctrl Pts',(19.5342904522513,-16.9916391118871,
5.53642298330857));
#173653=CARTESIAN_POINT('Ctrl Pts',(19.5733118863955,-17.0080260359025,
5.53903229286097));
#173654=CARTESIAN_POINT('Ctrl Pts',(19.6793107226783,-17.0563264046731,
5.54631991827515));
#173655=CARTESIAN_POINT('Ctrl Pts',(19.7451380104212,-17.0906056811991,
5.55107341881012));
#173656=CARTESIAN_POINT('Ctrl Pts',(19.9379616752512,-17.2042682654032,
5.56565146896423));
#173657=CARTESIAN_POINT('Ctrl Pts',(20.0584676519581,-17.2937258247171,
5.57570072226783));
#173658=CARTESIAN_POINT('Ctrl Pts',(20.173022375557,-17.3992795133665,5.58575053870765));
#173659=CARTESIAN_POINT('Ctrl Pts',(20.1774963120218,-17.403437858724,5.58614384153748));
#173660=CARTESIAN_POINT('Ctrl Pts',(20.2148437594107,-17.4384533105634,
5.58943341140839));
#173661=CARTESIAN_POINT('Ctrl Pts',(20.2467445178454,-17.4703365751843,
5.59228496083212));
#173662=CARTESIAN_POINT('Ctrl Pts',(20.2828016943608,-17.5087536683832,
5.59553267444668));
#173663=CARTESIAN_POINT('Ctrl Pts',(20.2879686611691,-17.5143185101511,
5.59599868237962));
#173664=CARTESIAN_POINT('Ctrl Pts',(20.296216851927,-17.5232982607529,5.59674339828276));
#173665=CARTESIAN_POINT('Ctrl Pts',(20.2993170303833,-17.5266955597187,
5.59702349517267));
#173666=CARTESIAN_POINT('Ctrl Pts',(20.3048120623795,-17.5327567876314,
5.59752025325519));
#173667=CARTESIAN_POINT('Ctrl Pts',(20.3072112524501,-17.5354167207515,
5.59773724043542));
#173668=CARTESIAN_POINT('Ctrl Pts',(20.3123089119801,-17.5410973159954,
5.59819847817065));
#173669=CARTESIAN_POINT('Ctrl Pts',(20.3150054607718,-17.5441196290131,
5.59844258572847));
#173670=CARTESIAN_POINT('Ctrl Pts',(20.3223193026342,-17.5523645520587,
5.59910507398887));
#173671=CARTESIAN_POINT('Ctrl Pts',(20.3269195478702,-17.5576023123404,
5.59952219695394));
#173672=CARTESIAN_POINT('Ctrl Pts',(20.3504126588416,-17.5846191550521,
5.60165522550219));
#173673=CARTESIAN_POINT('Ctrl Pts',(20.3688860507686,-17.606760970648,5.60334192128337));
#173674=CARTESIAN_POINT('Ctrl Pts',(20.4220893071256,-17.6732447468011,
5.60825156091645));
#173675=CARTESIAN_POINT('Ctrl Pts',(20.4555102709456,-17.7186047743925,
5.61140477888345));
#173676=CARTESIAN_POINT('Ctrl Pts',(20.5660785849803,-17.8819374465208,
5.62229126072365));
#173677=CARTESIAN_POINT('Ctrl Pts',(20.6332246192037,-18.0062234101449,
5.62978562537011));
#173678=CARTESIAN_POINT('Ctrl Pts',(20.7212603367996,-18.2170508220902,
5.64245085297522));
#173679=CARTESIAN_POINT('Ctrl Pts',(20.7499480236224,-18.2998459864583,
5.6474083154387));
#173680=CARTESIAN_POINT('Ctrl Pts',(20.7770887500541,-18.39732553729,5.65334122507995));
#173681=CARTESIAN_POINT('Ctrl Pts',(20.7806233643868,-18.4105129812296,
5.65414571868845));
#173682=CARTESIAN_POINT('Ctrl Pts',(20.7860934147498,-18.4317404625099,
5.65544405944733));
#173683=CARTESIAN_POINT('Ctrl Pts',(20.7881097644217,-18.439759390564,5.65593528966799));
#173684=CARTESIAN_POINT('Ctrl Pts',(20.7916099818974,-18.454032652851,5.65681109604792));
#173685=CARTESIAN_POINT('Ctrl Pts',(20.7931124471362,-18.4602823522873,
5.65719506697261));
#173686=CARTESIAN_POINT('Ctrl Pts',(20.7961869752037,-18.4733324787294,
5.65799790573463));
#173687=CARTESIAN_POINT('Ctrl Pts',(20.7977539131636,-18.4801340225174,
5.65841693335104));
#173688=CARTESIAN_POINT('Ctrl Pts',(20.8017429340734,-18.4978490036616,
5.65950992845358));
#173689=CARTESIAN_POINT('Ctrl Pts',(20.8041122353658,-18.5087739917771,
5.66018558039105));
#173690=CARTESIAN_POINT('Ctrl Pts',(20.8140881492265,-18.5565992267383,
5.66315059981171));
#173691=CARTESIAN_POINT('Ctrl Pts',(20.8207950690573,-18.5936781700032,
5.66546845862681));
#173692=CARTESIAN_POINT('Ctrl Pts',(20.8360316170003,-18.6929745094115,
5.67173021859019));
#173693=CARTESIAN_POINT('Ctrl Pts',(20.8427880694131,-18.7554222245571,
5.67572581940703));
#173694=CARTESIAN_POINT('Ctrl Pts',(20.8529257464839,-18.9153491949447,
5.68608641475998));
#173695=CARTESIAN_POINT('Ctrl Pts',(20.8523661267429,-19.0129295550779,
5.69253289499523));
#173696=CARTESIAN_POINT('Ctrl Pts',(20.8362349370176,-19.2283033897917,
5.706799865447));
#173697=CARTESIAN_POINT('Ctrl Pts',(20.8174727821903,-19.3455517733947,
5.71459383377768));
#173698=CARTESIAN_POINT('Ctrl Pts',(20.7867036120705,-19.4698682939201,
5.7225040375181));
#173699=CARTESIAN_POINT('Ctrl Pts',(20.7843532286604,-19.4790970824845,
5.7230890371202));
#173700=CARTESIAN_POINT('Ctrl Pts',(20.780778814449,-19.4927462582499,5.72395061584839));
#173701=CARTESIAN_POINT('Ctrl Pts',(20.7796026042249,-19.497178885863,5.72422984912721));
#173702=CARTESIAN_POINT('Ctrl Pts',(20.7774845626374,-19.5050575046963,
5.72472510748545));
#173703=CARTESIAN_POINT('Ctrl Pts',(20.7765484055392,-19.508504962176,5.72494145599792));
#173704=CARTESIAN_POINT('Ctrl Pts',(20.7745173001035,-19.5159104647103,
5.72540540750867));
#173705=CARTESIAN_POINT('Ctrl Pts',(20.7734195633255,-19.5198676867155,
5.72565284625754));
#173706=CARTESIAN_POINT('Ctrl Pts',(20.7703585804263,-19.530778837324,5.72633384232184));
#173707=CARTESIAN_POINT('Ctrl Pts',(20.7683712149744,-19.5377260227424,
5.72676602051922));
#173708=CARTESIAN_POINT('Ctrl Pts',(20.7573044102899,-19.5756760907432,
5.72911979156386));
#173709=CARTESIAN_POINT('Ctrl Pts',(20.7475512793176,-19.6064800265913,
5.73100448674677));
#173710=CARTESIAN_POINT('Ctrl Pts',(20.6843902247641,-19.7911637499992,
5.7422142041314));
#173711=CARTESIAN_POINT('Ctrl Pts',(20.6140695368678,-19.9386956435286,
5.75082287827826));
#173712=CARTESIAN_POINT('Ctrl Pts',(20.4654105553701,-20.1757533414089,
5.76614094015221));
#173713=CARTESIAN_POINT('Ctrl Pts',(20.3952159709305,-20.2694638448558,
5.77266675538923));
#173714=CARTESIAN_POINT('Ctrl Pts',(20.3081688603013,-20.36758667267,5.78035106190394));
#173715=CARTESIAN_POINT('Ctrl Pts',(20.2985772493002,-20.378180649372,5.7811926253937));
#173716=CARTESIAN_POINT('Ctrl Pts',(20.2831414126377,-20.3948864717692,
5.78253927751728));
#173717=CARTESIAN_POINT('Ctrl Pts',(20.277366453126,-20.4010619293064,5.7830414244519));
#173718=CARTESIAN_POINT('Ctrl Pts',(20.2671163332905,-20.411892119244,5.78392985587015));
#173719=CARTESIAN_POINT('Ctrl Pts',(20.2626565553318,-20.4165613082586,
5.7843154742351));
#173720=CARTESIAN_POINT('Ctrl Pts',(20.253388225888,-20.4261763810269,5.78511498677931));
#173721=CARTESIAN_POINT('Ctrl Pts',(20.2485767269903,-20.4311193054153,
5.78552900727363));
#173722=CARTESIAN_POINT('Ctrl Pts',(20.236164377411,-20.443746629118,5.78659448414575));
#173723=CARTESIAN_POINT('Ctrl Pts',(20.2285287481798,-20.4513964240075,
5.78724746984077));
#173724=CARTESIAN_POINT('Ctrl Pts',(20.1964159784567,-20.483079762904,5.78998381866931));
#173725=CARTESIAN_POINT('Ctrl Pts',(20.1714162057145,-20.5065739511842,
5.79209051929034));
#173726=CARTESIAN_POINT('Ctrl Pts',(20.1047997625853,-20.5661973818843,
5.797647530931));
#173727=CARTESIAN_POINT('Ctrl Pts',(20.0623257470958,-20.6013256396556,
5.80113627107753));
#173728=CARTESIAN_POINT('Ctrl Pts',(19.9315791246987,-20.7011312010865,
5.81170898535592));
#173729=CARTESIAN_POINT('Ctrl Pts',(19.8396173858778,-20.7606631661658,
5.81894133976479));
#173730=CARTESIAN_POINT('Ctrl Pts',(19.6394019071724,-20.8692781744089,
5.83398783200305));
#173731=CARTESIAN_POINT('Ctrl Pts',(19.5307613354876,-20.9169137672831,
5.84177392127846));
#173732=CARTESIAN_POINT('Ctrl Pts',(19.4096763468073,-20.9583004109624,
5.84967776298821));
#173733=CARTESIAN_POINT('Ctrl Pts',(19.4006354689389,-20.9613225286211,
5.85026333632698));
#173734=CARTESIAN_POINT('Ctrl Pts',(19.3872134520778,-20.9657085771535,
5.85112559446481));
#173735=CARTESIAN_POINT('Ctrl Pts',(19.3828479412285,-20.9671194499969,
5.85140493936761));
#173736=CARTESIAN_POINT('Ctrl Pts',(19.3750749369647,-20.9696036993622,
5.85190032024666));
#173737=CARTESIAN_POINT('Ctrl Pts',(19.3716692852213,-20.9706826510944,
5.85211668027456));
#173738=CARTESIAN_POINT('Ctrl Pts',(19.3643440103366,-20.9729829992078,
5.85258057234032));
#173739=CARTESIAN_POINT('Ctrl Pts',(19.360423572214,-20.9742016129177,5.85282794057178));
#173740=CARTESIAN_POINT('Ctrl Pts',(19.3495985006389,-20.9775319346873,
5.85350854369729));
#173741=CARTESIAN_POINT('Ctrl Pts',(19.3426864959403,-20.9796197586094,
5.85394040210108));
#173742=CARTESIAN_POINT('Ctrl Pts',(19.3048668542628,-20.9908326492226,
5.85628920499539));
#173743=CARTESIAN_POINT('Ctrl Pts',(19.2737628175131,-20.9992869590498,
5.8581694353563));
#173744=CARTESIAN_POINT('Ctrl Pts',(19.0843025193898,-21.0461651548016,
5.86937944722153));
#173745=CARTESIAN_POINT('Ctrl Pts',(18.9221230792634,-21.0669139971618,
5.87799151927304));
#173746=CARTESIAN_POINT('Ctrl Pts',(18.6422408361077,-21.0702398331054,
5.89331429267761));
#173747=CARTESIAN_POINT('Ctrl Pts',(18.5254286432224,-21.0619413391152,
5.89984122875645));
#173748=CARTESIAN_POINT('Ctrl Pts',(18.395784578589,-21.0418573073978,5.90752679697457));
#173749=CARTESIAN_POINT('Ctrl Pts',(18.38168468691,-21.0395265607444,5.90836837668167));
#173750=CARTESIAN_POINT('Ctrl Pts',(18.3592822524734,-21.0355899543386,
5.90971504990787));
#173751=CARTESIAN_POINT('Ctrl Pts',(18.350963713911,-21.0340767729619,5.91021720158176));
#173752=CARTESIAN_POINT('Ctrl Pts',(18.3363089495164,-21.0313202061658,
5.91110563852035));
#173753=CARTESIAN_POINT('Ctrl Pts',(18.3299688939879,-21.0300975808063,
5.91149125763992));
#173754=CARTESIAN_POINT('Ctrl Pts',(18.3168673872367,-21.0275088451415,
5.91229076893606));
#173755=CARTESIAN_POINT('Ctrl Pts',(18.3101068289092,-21.0261386551149,
5.91270478741361));
#173756=CARTESIAN_POINT('Ctrl Pts',(18.2927708565883,-21.0225368052788,
5.91377025317083));
#173757=CARTESIAN_POINT('Ctrl Pts',(18.2822057140478,-21.0202571734208,
5.91442322970615));
#173758=CARTESIAN_POINT('Ctrl Pts',(18.2381844207426,-21.0104053430644,
5.91715948976383));
#173759=CARTESIAN_POINT('Ctrl Pts',(18.2048988775109,-21.002101809893,5.91926610888014));
#173760=CARTESIAN_POINT('Ctrl Pts',(18.1187107711583,-20.978362263788,5.9248228542819));
#173761=CARTESIAN_POINT('Ctrl Pts',(18.0661857632456,-20.9616636991741,
5.92831140510364));
#173762=CARTESIAN_POINT('Ctrl Pts',(17.8184621070226,-20.8721238884677,
5.94524253490021));
#173763=CARTESIAN_POINT('Ctrl Pts',(17.6341001355082,-20.7727945402005,
5.95943300876748));
#173764=CARTESIAN_POINT('Ctrl Pts',(17.4635919722165,-20.6454500092709,
5.9728494765435));
#173765=CARTESIAN_POINT('Ctrl Pts',(17.4599738122632,-20.6427296545023,
5.97313425606137));
#173766=CARTESIAN_POINT('Ctrl Pts',(17.4399959671345,-20.6276085398481,
5.97470702139216));
#173767=CARTESIAN_POINT('Ctrl Pts',(17.4238079167231,-20.6149814169334,
5.97598271146736));
#173768=CARTESIAN_POINT('Ctrl Pts',(17.4027810313994,-20.5980821997696,
5.97763860701494));
#173769=CARTESIAN_POINT('Ctrl Pts',(17.3977750251302,-20.5940211234255,
5.97803275146324));
#173770=CARTESIAN_POINT('Ctrl Pts',(17.3897442118159,-20.5874451529167,
5.9786648050546));
#173771=CARTESIAN_POINT('Ctrl Pts',(17.386707774317,-20.5849446198398,5.97890372616249));
#173772=CARTESIAN_POINT('Ctrl Pts',(17.3810359180814,-20.5802472061477,
5.97934987773984));
#173773=CARTESIAN_POINT('Ctrl Pts',(17.3783988701044,-20.5780523817002,
5.97955725067337));
#173774=CARTESIAN_POINT('Ctrl Pts',(17.3721624888226,-20.5728361043561,
5.98004755412945));
#173775=CARTESIAN_POINT('Ctrl Pts',(17.3685678362495,-20.5698090404011,
5.98033007578921));
#173776=CARTESIAN_POINT('Ctrl Pts',(17.3573349183623,-20.5602856700686,
5.98121275390682));
#173777=CARTESIAN_POINT('Ctrl Pts',(17.3497325798042,-20.5537469406319,
5.98180989073701));
#173778=CARTESIAN_POINT('Ctrl Pts',(17.3319067413098,-20.5381933260096,
5.98321024073961));
#173779=CARTESIAN_POINT('Ctrl Pts',(17.3217231634268,-20.5291331365875,
5.9840103878859));
#173780=CARTESIAN_POINT('Ctrl Pts',(17.2863073425746,-20.4970060368439,
5.98679657699121));
#173781=CARTESIAN_POINT('Ctrl Pts',(17.2615458532658,-20.4734258841379,
5.98875091460641));
#173782=CARTESIAN_POINT('Ctrl Pts',(17.1836732754796,-20.3955855636051,
5.99496002785008));
#173783=CARTESIAN_POINT('Ctrl Pts',(17.1329039463589,-20.3390634504074,
5.99910803211691));
#173784=CARTESIAN_POINT('Ctrl Pts',(16.9773656441819,-20.1459517987438,
6.01259282574975));
#173785=CARTESIAN_POINT('Ctrl Pts',(16.8861986189146,-19.9993339378304,
6.02185803999852));
#173786=CARTESIAN_POINT('Ctrl Pts',(16.8039951982117,-19.8222356839923,
6.03320082167258));
#173787=CARTESIAN_POINT('Ctrl Pts',(16.7945621925219,-19.8010050699168,
6.03456160741386));
#173788=CARTESIAN_POINT('Ctrl Pts',(16.7817332890366,-19.7708013035738,
6.03650075742275));
#173789=CARTESIAN_POINT('Ctrl Pts',(16.7780458554122,-19.7619532487414,
6.03706920488626));
#173790=CARTESIAN_POINT('Ctrl Pts',(16.7721580869368,-19.747550750926,6.03799523947808));
#173791=CARTESIAN_POINT('Ctrl Pts',(16.7699209237878,-19.7420114368851,
6.03835157590773));
#173792=CARTESIAN_POINT('Ctrl Pts',(16.7652917997094,-19.7304083201676,
6.03909838999349));
#173793=CARTESIAN_POINT('Ctrl Pts',(16.7629043425996,-19.7243427986974,
6.03948901484956));
#173794=CARTESIAN_POINT('Ctrl Pts',(16.7572996268597,-19.7099083219375,
6.04041919415483));
#173795=CARTESIAN_POINT('Ctrl Pts',(16.7541074665883,-19.7015298138903,
6.04095958430167));
#173796=CARTESIAN_POINT('Ctrl Pts',(16.7435701496583,-19.6733353125818,
6.04277975751818));
#173797=CARTESIAN_POINT('Ctrl Pts',(16.736468697918,-19.6534301595239,6.04406762352146));
#173798=CARTESIAN_POINT('Ctrl Pts',(16.6996529282216,-19.5451404165116,
6.05109143606473));
#173799=CARTESIAN_POINT('Ctrl Pts',(16.6755085000078,-19.4549834205257,
6.05700831957264));
#173800=CARTESIAN_POINT('Ctrl Pts',(16.6304385570067,-19.2275615688264,
6.07205887777749));
#173801=CARTESIAN_POINT('Ctrl Pts',(16.6169140925337,-19.0892811970425,
6.08133516793109));
#173802=CARTESIAN_POINT('Ctrl Pts',(16.6170004105532,-18.9506815606685,
6.09037076557823));
#173803=CARTESIAN_POINT('Ctrl Pts',(16.7454193692319,-18.2258897639242,
6.13370787796071));
#173804=CARTESIAN_POINT('Ctrl Pts',(16.7204253525143,-18.2943402760645,
6.12932687904854));
#173805=CARTESIAN_POINT('Ctrl Pts',(16.6989959006628,-18.3640109059891,
6.12494588013637));
#173806=CARTESIAN_POINT('Ctrl Pts',(16.6812266680874,-18.4344957509464,
6.1205648812242));
#173807=CARTESIAN_POINT('Ctrl Pts',(16.6634283619283,-18.505095921483,6.11617671422876));
#173808=CARTESIAN_POINT('Ctrl Pts',(16.6493023130958,-18.5765124923157,
6.11178854723333));
#173809=CARTESIAN_POINT('Ctrl Pts',(16.6388927520737,-18.6483313982534,
6.1074003802379));
#173810=CARTESIAN_POINT('Ctrl Pts',(16.6365508801238,-18.6644887252465,
6.10641316039488));
#173811=CARTESIAN_POINT('Ctrl Pts',(16.6343969017635,-18.6806664075672,
6.10542594055187));
#173812=CARTESIAN_POINT('Ctrl Pts',(16.6324309574259,-18.6968597262404,
6.10443872070885));
#173813=CARTESIAN_POINT('Ctrl Pts',(16.6222201199426,-18.7809655384568,
6.09931124014674));
#173814=CARTESIAN_POINT('Ctrl Pts',(16.6170567766291,-18.8656963446802,
6.09418375958462));
#173815=CARTESIAN_POINT('Ctrl Pts',(16.6170004656572,-18.950595866038,6.0890562790225));
#173816=CARTESIAN_POINT('Origin',(18.734,-18.952,0.));
#173817=CARTESIAN_POINT('',(16.7454193236514,-18.2258898887545,7.15616137122352));
#173818=CARTESIAN_POINT('',(16.7486737197731,-18.2270709325543,6.93361858681016));
#173819=CARTESIAN_POINT('',(16.7454193692319,-18.2258897639242,0.));
#173820=CARTESIAN_POINT('Ctrl Pts',(16.7454193236514,-18.2258898887546,
7.15616137122351));
#173821=CARTESIAN_POINT('Ctrl Pts',(16.7205840422062,-18.2939056896761,
7.15141136591347));
#173822=CARTESIAN_POINT('Ctrl Pts',(16.6992294961428,-18.3632196084634,
7.14660725207261));
#173823=CARTESIAN_POINT('Ctrl Pts',(16.6631797913716,-18.5059445142713,
7.13689819598514));
#173824=CARTESIAN_POINT('Ctrl Pts',(16.6487382377985,-18.5792443860931,
7.13200642664211));
#173825=CARTESIAN_POINT('Ctrl Pts',(16.6333272121045,-18.6873232098812,
7.12505656814692));
#173826=CARTESIAN_POINT('Ctrl Pts',(16.629291438054,-18.7216043578968,7.12289061591573));
#173827=CARTESIAN_POINT('Ctrl Pts',(16.6254128245581,-18.7633111888787,
7.12031415742816));
#173828=CARTESIAN_POINT('Ctrl Pts',(16.62476854426,-18.770654987178,7.11986269306851));
#173829=CARTESIAN_POINT('Ctrl Pts',(16.6238224665487,-18.7821267945445,
7.11916105190624));
#173830=CARTESIAN_POINT('Ctrl Pts',(16.6234943985693,-18.7862524943738,
7.11890944030274));
#173831=CARTESIAN_POINT('Ctrl Pts',(16.6229060239731,-18.7939368614968,
7.11844218237915));
#173832=CARTESIAN_POINT('Ctrl Pts',(16.6226426179124,-18.7974951886471,
7.11822636985866));
#173833=CARTESIAN_POINT('Ctrl Pts',(16.6220645668247,-18.8055816665784,
7.11773717361678));
#173834=CARTESIAN_POINT('Ctrl Pts',(16.6217554882698,-18.8101101631181,
7.11746410481957));
#173835=CARTESIAN_POINT('Ctrl Pts',(16.6209918950824,-18.8218538767062,
7.11675817189079));
#173836=CARTESIAN_POINT('Ctrl Pts',(16.6205597664585,-18.8290705588811,
7.11632653177196));
#173837=CARTESIAN_POINT('Ctrl Pts',(16.6180743367141,-18.8744751346457,
7.11362364774395));
#173838=CARTESIAN_POINT('Ctrl Pts',(16.6170190194692,-18.9127131790533,
7.11140440706729));
#173839=CARTESIAN_POINT('Ctrl Pts',(16.6169207094652,-19.1130991496786,
7.09997625594565));
#173840=CARTESIAN_POINT('Ctrl Pts',(16.6354677196798,-19.2747232329275,
7.09141461483807));
#173841=CARTESIAN_POINT('Ctrl Pts',(16.697373122891,-19.5402575685224,7.07645434330741));
#173842=CARTESIAN_POINT('Ctrl Pts',(16.7308397027785,-19.6457147643738,
7.07026707766899));
#173843=CARTESIAN_POINT('Ctrl Pts',(16.777712666695,-19.7612157292806,7.06296367776398));
#173844=CARTESIAN_POINT('Ctrl Pts',(16.7831788076353,-19.7743058359248,
7.06212823659863));
#173845=CARTESIAN_POINT('Ctrl Pts',(16.7921001452617,-19.7950806157054,
7.06078955305786));
#173846=CARTESIAN_POINT('Ctrl Pts',(16.7954704367952,-19.802801445616,7.06028919752226));
#173847=CARTESIAN_POINT('Ctrl Pts',(16.8015031073668,-19.8163994371424,
7.05940285044233));
#173848=CARTESIAN_POINT('Ctrl Pts',(16.8041464536137,-19.822284961979,7.05901751498165));
#173849=CARTESIAN_POINT('Ctrl Pts',(16.8096767357639,-19.8344492800026,
7.05821751895034));
#173850=CARTESIAN_POINT('Ctrl Pts',(16.8125675911792,-19.8407261972221,
7.05780272678382));
#173851=CARTESIAN_POINT('Ctrl Pts',(16.82008271323,-19.8568357214004,7.05673299948148));
#173852=CARTESIAN_POINT('Ctrl Pts',(16.8247519979579,-19.8666469937216,
7.05607651141696));
#173853=CARTESIAN_POINT('Ctrl Pts',(16.8446948516566,-19.907733471956,7.05330601284697));
#173854=CARTESIAN_POINT('Ctrl Pts',(16.8606622755661,-19.9386640549607,
7.05116793022875));
#173855=CARTESIAN_POINT('Ctrl Pts',(16.9043949478943,-20.01848702026,7.04550808426069));
#173856=CARTESIAN_POINT('Ctrl Pts',(16.9333567099543,-20.0666892324598,
7.04194609514396));
#173857=CARTESIAN_POINT('Ctrl Pts',(17.033235571777,-20.2188531399357,7.03023623095629));
#173858=CARTESIAN_POINT('Ctrl Pts',(17.1115049696023,-20.3176579849348,
7.02187674911319));
#173859=CARTESIAN_POINT('Ctrl Pts',(17.2668984461352,-20.4814782138005,
7.00699926012126));
#173860=CARTESIAN_POINT('Ctrl Pts',(17.340787624772,-20.5490768939823,7.00047971996934));
#173861=CARTESIAN_POINT('Ctrl Pts',(17.4267853739081,-20.6172245780694,
6.9937003735011));
#173862=CARTESIAN_POINT('Ctrl Pts',(17.434424519406,-20.6231931523665,6.99310474164512));
#173863=CARTESIAN_POINT('Ctrl Pts',(17.4457640290431,-20.6319281000143,
6.99223058323371));
#173864=CARTESIAN_POINT('Ctrl Pts',(17.449432755844,-20.6347350754828,6.99194929125815));
#173865=CARTESIAN_POINT('Ctrl Pts',(17.4559575628414,-20.6396934893593,
6.99145176513152));
#173866=CARTESIAN_POINT('Ctrl Pts',(17.4588099326086,-20.6418497205106,
6.99123519614061));
#173867=CARTESIAN_POINT('Ctrl Pts',(17.464932836444,-20.6464539600509,6.99077230377625));
#173868=CARTESIAN_POINT('Ctrl Pts',(17.4682049880638,-20.6488997250145,
6.99052613662012));
#173869=CARTESIAN_POINT('Ctrl Pts',(17.4772061326084,-20.6555870939352,
6.98985221814885));
#173870=CARTESIAN_POINT('Ctrl Pts',(17.482949561784,-20.6598093031912,6.98942579895779));
#173871=CARTESIAN_POINT('Ctrl Pts',(17.5137221168821,-20.6821928119932,
6.98715956675343));
#173872=CARTESIAN_POINT('Ctrl Pts',(17.5391269999282,-20.6998340938013,
6.98535348852625));
#173873=CARTESIAN_POINT('Ctrl Pts',(17.6171834267134,-20.7515391392161,
6.97996801335136));
#173874=CARTESIAN_POINT('Ctrl Pts',(17.6709725792072,-20.7838281096898,
6.97647536587213));
#173875=CARTESIAN_POINT('Ctrl Pts',(17.8443351482861,-20.8776833556854,
6.96564099390635));
#173876=CARTESIAN_POINT('Ctrl Pts',(17.9683763451223,-20.9302772946545,
6.9584722452433));
#173877=CARTESIAN_POINT('Ctrl Pts',(18.1354765441738,-20.9830399900457,
6.94874720043832));
#173878=CARTESIAN_POINT('Ctrl Pts',(18.17473005089,-20.9941975043606,6.94645996765171));
#173879=CARTESIAN_POINT('Ctrl Pts',(18.2613895347852,-21.0161438868505,
6.94137922699533));
#173880=CARTESIAN_POINT('Ctrl Pts',(18.3088928558736,-21.0264478833089,
6.93857392112183));
#173881=CARTESIAN_POINT('Ctrl Pts',(18.3691073382889,-21.03735397004,6.93497490416398));
#173882=CARTESIAN_POINT('Ctrl Pts',(18.381528146417,-21.0394892615366,6.93423025968309));
#173883=CARTESIAN_POINT('Ctrl Pts',(18.4012400734647,-21.0426970436934,
6.93304465328028));
#173884=CARTESIAN_POINT('Ctrl Pts',(18.4085191234941,-21.0438426074014,
6.93260601410387));
#173885=CARTESIAN_POINT('Ctrl Pts',(18.4220931084109,-21.0459062918154,
6.93178643766937));
#173886=CARTESIAN_POINT('Ctrl Pts',(18.4283865045984,-21.0468340884151,
6.93140581205598));
#173887=CARTESIAN_POINT('Ctrl Pts',(18.4423736272109,-21.0488317520093,
6.93055840763253));
#173888=CARTESIAN_POINT('Ctrl Pts',(18.450069225143,-21.0498876638469,6.93009119252828));
#173889=CARTESIAN_POINT('Ctrl Pts',(18.4724466614918,-21.0528326861058,
6.92872968181976));
#173890=CARTESIAN_POINT('Ctrl Pts',(18.4871424945694,-21.0546101584567,
6.92783187789438));
#173891=CARTESIAN_POINT('Ctrl Pts',(18.6040636645042,-21.0675092078417,
6.92065849927563));
#173892=CARTESIAN_POINT('Ctrl Pts',(18.7069422908414,-21.0713218500874,
6.91415210350628));
#173893=CARTESIAN_POINT('Ctrl Pts',(18.9653712327339,-21.0620776316681,
6.89736585629444));
#173894=CARTESIAN_POINT('Ctrl Pts',(19.1199622063566,-21.0393403449755,
6.88689550539218));
#173895=CARTESIAN_POINT('Ctrl Pts',(19.3214687454626,-20.9865340776092,
6.87343963271799));
#173896=CARTESIAN_POINT('Ctrl Pts',(19.3717748098951,-20.9713297716734,
6.87010191625839));
#173897=CARTESIAN_POINT('Ctrl Pts',(19.4296851682674,-20.9514465840586,
6.86632509219423));
#173898=CARTESIAN_POINT('Ctrl Pts',(19.4378858215163,-20.9485743792971,
6.86579182172744));
#173899=CARTESIAN_POINT('Ctrl Pts',(19.4502843393181,-20.9441460247169,
6.86498819790692));
#173900=CARTESIAN_POINT('Ctrl Pts',(19.4544952188937,-20.9426269562505,
6.86471572579251));
#173901=CARTESIAN_POINT('Ctrl Pts',(19.4620494704452,-20.9398746607746,
6.86422778459499));
#173902=CARTESIAN_POINT('Ctrl Pts',(19.4653945595866,-20.9386463442574,
6.86401202969258));
#173903=CARTESIAN_POINT('Ctrl Pts',(19.472661434878,-20.9359571060101,6.86354400158541));
#173904=CARTESIAN_POINT('Ctrl Pts',(19.4765819827785,-20.9344930046314,
6.86329192125436));
#173905=CARTESIAN_POINT('Ctrl Pts',(19.4875952542926,-20.9303429209852,
6.86258492723344));
#173906=CARTESIAN_POINT('Ctrl Pts',(19.4946780054251,-20.9276304047851,
6.86213157150478));
#173907=CARTESIAN_POINT('Ctrl Pts',(19.537198546351,-20.911083537179,6.85941698078505));
#173908=CARTESIAN_POINT('Ctrl Pts',(19.5722751497765,-20.8963331477928,
6.8572072784303));
#173909=CARTESIAN_POINT('Ctrl Pts',(19.6869983762708,-20.8444074489981,
6.85001917294139));
#173910=CARTESIAN_POINT('Ctrl Pts',(19.7647318453029,-20.8032174828116,
6.84521011970471));
#173911=CARTESIAN_POINT('Ctrl Pts',(19.9882640263207,-20.6663125020235,
6.83095045532758));
#173912=CARTESIAN_POINT('Ctrl Pts',(20.1250238164415,-20.5573322364003,
6.82157749679089));
#173913=CARTESIAN_POINT('Ctrl Pts',(20.2630317539919,-20.4163373137427,
6.81011396583166));
#173914=CARTESIAN_POINT('Ctrl Pts',(20.27890756625,-20.3995781233629,6.80876165751377));
#173915=CARTESIAN_POINT('Ctrl Pts',(20.3009668565588,-20.3755151181416,
6.80683254484499));
#173916=CARTESIAN_POINT('Ctrl Pts',(20.307380096146,-20.36842348527,6.80626551687288));
#173917=CARTESIAN_POINT('Ctrl Pts',(20.317718983374,-20.356834089197,6.80534116612256));
#173918=CARTESIAN_POINT('Ctrl Pts',(20.3216740787798,-20.3523626869192,
6.80498508491906));
#173919=CARTESIAN_POINT('Ctrl Pts',(20.3299107197553,-20.3429710688386,
6.8042382947326));
#173920=CARTESIAN_POINT('Ctrl Pts',(20.3341885394292,-20.3380476819278,
6.8038474362912));
#173921=CARTESIAN_POINT('Ctrl Pts',(20.3443064028859,-20.3262936556785,
6.80291575976586));
#173922=CARTESIAN_POINT('Ctrl Pts',(20.350125802035,-20.3194454838558,6.80237409879659));
#173923=CARTESIAN_POINT('Ctrl Pts',(20.3695621385229,-20.2962757539406,
6.80054519409433));
#173924=CARTESIAN_POINT('Ctrl Pts',(20.3829764782285,-20.2797866297497,
6.79924976134771));
#173925=CARTESIAN_POINT('Ctrl Pts',(20.4545180199004,-20.18909014491,6.792155086083));
#173926=CARTESIAN_POINT('Ctrl Pts',(20.5078803601392,-20.1112750502559,
6.78617079350107));
#173927=CARTESIAN_POINT('Ctrl Pts',(20.6403889128631,-19.8873645819508,
6.76927208601287));
#173928=CARTESIAN_POINT('Ctrl Pts',(20.7078127914036,-19.7351252486921,
6.7580895347162));
#173929=CARTESIAN_POINT('Ctrl Pts',(20.7691591445091,-19.5364487520998,
6.74476058614701));
#173930=CARTESIAN_POINT('Ctrl Pts',(20.7803546805778,-19.4959541821624,
6.74210945345194));
#173931=CARTESIAN_POINT('Ctrl Pts',(20.7921063628785,-19.4479259183983,
6.73906263745244));
#173932=CARTESIAN_POINT('Ctrl Pts',(20.793836006481,-19.4406920785126,6.73860631930271));
#173933=CARTESIAN_POINT('Ctrl Pts',(20.7965740907663,-19.4289678162969,
6.73787108305089));
#173934=CARTESIAN_POINT('Ctrl Pts',(20.7976060584196,-19.4244830306595,
6.73759086485057));
#173935=CARTESIAN_POINT('Ctrl Pts',(20.7994134599979,-19.4165094312379,
6.73709452363717));
#173936=CARTESIAN_POINT('Ctrl Pts',(20.8001946905246,-19.413021988593,6.73687807173217));
#173937=CARTESIAN_POINT('Ctrl Pts',(20.8018523888711,-19.4055331043866,
6.73641463657394));
#173938=CARTESIAN_POINT('Ctrl Pts',(20.8027260732621,-19.4015311039228,
6.73616781369144));
#173939=CARTESIAN_POINT('Ctrl Pts',(20.8050988636786,-19.3905088677092,
6.73549024767434));
#173940=CARTESIAN_POINT('Ctrl Pts',(20.8065739032446,-19.3834834285796,
6.73506086079326));
#173941=CARTESIAN_POINT('Ctrl Pts',(20.8143542752058,-19.3454658179259,
6.73275002415719));
#173942=CARTESIAN_POINT('Ctrl Pts',(20.8200005951603,-19.3143410260219,
6.7309039019925));
#173943=CARTESIAN_POINT('Ctrl Pts',(20.8505124673408,-19.1216535872645,
6.71969131597434));
#173944=CARTESIAN_POINT('Ctrl Pts',(20.8572960747971,-18.9577730278763,
6.71105305100452));
#173945=CARTESIAN_POINT('Ctrl Pts',(20.8364523718367,-18.6779727513606,
6.69569421656281));
#173946=CARTESIAN_POINT('Ctrl Pts',(20.8180853133802,-18.5621538371215,
6.68915892571303));
#173947=CARTESIAN_POINT('Ctrl Pts',(20.7868423666665,-18.4345722145591,
6.68146395285269));
#173948=CARTESIAN_POINT('Ctrl Pts',(20.7833021713075,-18.4207242794161,
6.68062225334265));
#173949=CARTESIAN_POINT('Ctrl Pts',(20.7774449141534,-18.3987429340034,
6.67927542418178));
#173950=CARTESIAN_POINT('Ctrl Pts',(20.7752188365562,-18.3905855751958,
6.678773237454));
#173951=CARTESIAN_POINT('Ctrl Pts',(20.7712067839709,-18.3762229493748,
6.67788475962816));
#173952=CARTESIAN_POINT('Ctrl Pts',(20.7694411667829,-18.3700120724419,
6.67749913487164));
#173953=CARTESIAN_POINT('Ctrl Pts',(20.7657306842343,-18.3571832161886,
6.67669963263889));
#173954=CARTESIAN_POINT('Ctrl Pts',(20.7637818346387,-18.3505664778366,
6.6762856289637));
#173955=CARTESIAN_POINT('Ctrl Pts',(20.7586966829697,-18.3336076187836,
6.67522024500074));
#173956=CARTESIAN_POINT('Ctrl Pts',(20.7555134890168,-18.3232798698026,
6.67456733591104));
#173957=CARTESIAN_POINT('Ctrl Pts',(20.7419000613083,-18.280284040829,6.67183173002492));
#173958=CARTESIAN_POINT('Ctrl Pts',(20.7307563860413,-18.2478489474932,
6.66972571159078));
#173959=CARTESIAN_POINT('Ctrl Pts',(20.6996742767553,-18.1640614509794,
6.66417092838132));
#173960=CARTESIAN_POINT('Ctrl Pts',(20.6785117126121,-18.1131937654685,
6.66068377289905));
#173961=CARTESIAN_POINT('Ctrl Pts',(20.6094732597096,-17.9639456559883,
6.65011410260269));
#173962=CARTESIAN_POINT('Ctrl Pts',(20.5559344158356,-17.8683935896613,
6.64288319739068));
#173963=CARTESIAN_POINT('Ctrl Pts',(20.4696791982319,-17.7390563388693,
6.63261382664497));
#173964=CARTESIAN_POINT('Ctrl Pts',(20.4428521125348,-17.7015443793991,
6.62957398240444));
#173965=CARTESIAN_POINT('Ctrl Pts',(20.4015497055692,-17.6476060843514,
6.62513733129959));
#173966=CARTESIAN_POINT('Ctrl Pts',(20.3880107982308,-17.6304804833595,
6.62371849968117));
#173967=CARTESIAN_POINT('Ctrl Pts',(20.3415181457843,-17.5735051469832,
6.61897095617013));
#173968=CARTESIAN_POINT('Ctrl Pts',(20.3073673279748,-17.5346507648916,
6.61568719385093));
#173969=CARTESIAN_POINT('Ctrl Pts',(20.2658808040086,-17.4908001476466,
6.61196388803746));
#173970=CARTESIAN_POINT('Ctrl Pts',(20.2598981389262,-17.4845536869499,
6.61143308847346));
#173971=CARTESIAN_POINT('Ctrl Pts',(20.2507671430933,-17.4751362976341,
6.6106324427902));
#173972=CARTESIAN_POINT('Ctrl Pts',(20.247646863015,-17.4719384686219,6.61036050087401));
#173973=CARTESIAN_POINT('Ctrl Pts',(20.2420201170573,-17.466208284743,6.60987312401625));
#173974=CARTESIAN_POINT('Ctrl Pts',(20.2395173736773,-17.46367237051,6.60965740621838));
#173975=CARTESIAN_POINT('Ctrl Pts',(20.2340562793087,-17.4581667666818,
6.60918901528118));
#173976=CARTESIAN_POINT('Ctrl Pts',(20.2310955165991,-17.4551995507292,
6.60893653742389));
#173977=CARTESIAN_POINT('Ctrl Pts',(20.2227310843156,-17.4468665344498,
6.60822730324664));
#173978=CARTESIAN_POINT('Ctrl Pts',(20.2173071842674,-17.4415210058994,
6.60777212076156));
#173979=CARTESIAN_POINT('Ctrl Pts',(20.1842216388275,-17.4092636006333,
6.60502312005463));
#173980=CARTESIAN_POINT('Ctrl Pts',(20.1558552863375,-17.3830811471696,
6.60278236541031));
#173981=CARTESIAN_POINT('Ctrl Pts',(20.0589373025155,-17.2984138843316,
6.59544057029809));
#173982=CARTESIAN_POINT('Ctrl Pts',(19.9873673987102,-17.2435273955039,
6.59051724223738));
#173983=CARTESIAN_POINT('Ctrl Pts',(19.7703568644642,-17.0981022828827,
6.57631246218393));
#173984=CARTESIAN_POINT('Ctrl Pts',(19.6171936690868,-17.0204373233737,
6.56709203842127));
#173985=CARTESIAN_POINT('Ctrl Pts',(19.4344700030725,-16.9541078506304,
6.55579962952865));
#173986=CARTESIAN_POINT('Ctrl Pts',(19.4124520303893,-16.9465239854499,
6.55443563902311));
#173987=CARTESIAN_POINT('Ctrl Pts',(19.3811919096339,-16.9363304601114,
6.55249269243209));
#173988=CARTESIAN_POINT('Ctrl Pts',(19.3720497605427,-16.9334179332026,
6.55192370647252));
#173989=CARTESIAN_POINT('Ctrl Pts',(19.3571822849514,-16.9287925096709,
6.55099703281094));
#173990=CARTESIAN_POINT('Ctrl Pts',(19.3514688840056,-16.9270415102135,
6.55064059927417));
#173991=CARTESIAN_POINT('Ctrl Pts',(19.339509129042,-16.9234314980434,6.54989377463234));
#173992=CARTESIAN_POINT('Ctrl Pts',(19.3332614593487,-16.9215770947044,
6.54950323717956));
#173993=CARTESIAN_POINT('Ctrl Pts',(19.3184058056801,-16.9172422493727,
6.54857362021242));
#173994=CARTESIAN_POINT('Ctrl Pts',(19.309790495537,-16.9147875538265,6.54803370769934));
#173995=CARTESIAN_POINT('Ctrl Pts',(19.2808432814633,-16.9067381316301,
6.54621680888953));
#173996=CARTESIAN_POINT('Ctrl Pts',(19.2604439218395,-16.9013926676821,
6.54493177925463));
#173997=CARTESIAN_POINT('Ctrl Pts',(19.1497950947463,-16.8741580112182,
6.53793443075258));
#173998=CARTESIAN_POINT('Ctrl Pts',(19.0582706834185,-16.8579232403246,
6.53204269793041));
#173999=CARTESIAN_POINT('Ctrl Pts',(18.8139405565176,-16.8309867181146,
6.51608860539451));
#174000=CARTESIAN_POINT('Ctrl Pts',(18.6605373395818,-16.8307533524097,
6.50581585662054));
#174001=CARTESIAN_POINT('Ctrl Pts',(18.5040735368982,-16.8475185378853,
6.4956318624244));
#174002=CARTESIAN_POINT('Ctrl Pts',(18.499695196508,-16.848001506107,6.49534715683458));
#174003=CARTESIAN_POINT('Ctrl Pts',(18.4442788129399,-16.8542895312967,
6.49174736493));
#174004=CARTESIAN_POINT('Ctrl Pts',(18.3934622119089,-16.8619371949286,
6.48848588507889));
#174005=CARTESIAN_POINT('Ctrl Pts',(18.3352295037965,-16.8728816475476,
6.48483135229389));
#174006=CARTESIAN_POINT('Ctrl Pts',(18.3274970175734,-16.874379639628,6.48434778940366));
#174007=CARTESIAN_POINT('Ctrl Pts',(18.3151814396582,-16.8768368896382,
6.48358053802955));
#174008=CARTESIAN_POINT('Ctrl Pts',(18.3105929449135,-16.8777682415491,
6.48329532655325));
#174009=CARTESIAN_POINT('Ctrl Pts',(18.3024887454088,-16.87944120792,6.48279277880801));
#174010=CARTESIAN_POINT('Ctrl Pts',(18.298971790993,-16.8801765597469,6.48257508886703));
#174011=CARTESIAN_POINT('Ctrl Pts',(18.29154023578,-16.8817501640925,6.48211595474024));
#174012=CARTESIAN_POINT('Ctrl Pts',(18.2876261427665,-16.882590565833,6.48187463516785));
#174013=CARTESIAN_POINT('Ctrl Pts',(18.2771101511795,-16.8848796964931,
6.48122756900835));
#174014=CARTESIAN_POINT('Ctrl Pts',(18.2705127033572,-16.8863489617572,
6.48082298269991));
#174015=CARTESIAN_POINT('Ctrl Pts',(18.2383282279912,-16.8936784691655,
6.47885545437729));
#174016=CARTESIAN_POINT('Ctrl Pts',(18.2128434368267,-16.8999829412734,
6.47731658043968));
#174017=CARTESIAN_POINT('Ctrl Pts',(18.1401795898599,-16.9193998116499,
6.47296659201194));
#174018=CARTESIAN_POINT('Ctrl Pts',(18.0933274841723,-16.9336775373401,
6.47020771883184));
#174019=CARTESIAN_POINT('Ctrl Pts',(17.9175621553092,-16.9939787413755,
6.45989040273254));
#174020=CARTESIAN_POINT('Ctrl Pts',(17.7927230343377,-17.0508375930593,
6.45261020107232));
#174021=CARTESIAN_POINT('Ctrl Pts',(17.5865916267845,-17.170036300437,6.43949642027855));
#174022=CARTESIAN_POINT('Ctrl Pts',(17.5027007508073,-17.2269379826017,
6.43380098422931));
#174023=CARTESIAN_POINT('Ctrl Pts',(17.4121866698885,-17.2983085155314,
6.42704597803946));
#174024=CARTESIAN_POINT('Ctrl Pts',(17.4012518620529,-17.3071083950231,
6.42621922657819));
#174025=CARTESIAN_POINT('Ctrl Pts',(17.3839289808812,-17.3213352638226,
6.424891860317));
#174026=CARTESIAN_POINT('Ctrl Pts',(17.3774841170513,-17.3266926768445,
6.42439405532392));
#174027=CARTESIAN_POINT('Ctrl Pts',(17.3661396864615,-17.3362374246486,
6.42351066773136));
#174028=CARTESIAN_POINT('Ctrl Pts',(17.3612270845954,-17.3404091528636,
6.42312572695975));
#174029=CARTESIAN_POINT('Ctrl Pts',(17.3561424637417,-17.3447670756299,
6.42272478562491));
#174030=CARTESIAN_POINT('Ctrl Pts',(17.3559513063226,-17.3449309718437,
6.42270970843043));
#174031=CARTESIAN_POINT('Ctrl Pts',(17.3556444990268,-17.3451941199501,
6.42268550358961));
#174032=CARTESIAN_POINT('Ctrl Pts',(17.355528832093,-17.3452933489667,6.42267637695556));
#174033=CARTESIAN_POINT('Ctrl Pts',(17.3553013834243,-17.3454885165824,
6.42265842756588));
#174034=CARTESIAN_POINT('Ctrl Pts',(17.355189600013,-17.3455844551966,6.42264960476726));
#174035=CARTESIAN_POINT('Ctrl Pts',(17.3549764819806,-17.3457674033349,
6.42263278143891));
#174036=CARTESIAN_POINT('Ctrl Pts',(17.354875142966,-17.3458544130278,6.42262478078877));
#174037=CARTESIAN_POINT('Ctrl Pts',(17.3546817820773,-17.3460204645072,
6.42260951307112));
#174038=CARTESIAN_POINT('Ctrl Pts',(17.3545897579858,-17.3460995052803,
6.42260224601196));
#174039=CARTESIAN_POINT('Ctrl Pts',(17.3544140446979,-17.3462504541158,
6.42258836844169));
#174040=CARTESIAN_POINT('Ctrl Pts',(17.3543303532612,-17.346322361729,6.42258175790306));
#174041=CARTESIAN_POINT('Ctrl Pts',(17.3541704369891,-17.346459783393,6.42256912522274));
#174042=CARTESIAN_POINT('Ctrl Pts',(17.3540942146795,-17.3465252933352,
6.42256310340266));
#174043=CARTESIAN_POINT('Ctrl Pts',(17.353948485064,-17.3466505599948,6.422551589135));
#174044=CARTESIAN_POINT('Ctrl Pts',(17.3538789770043,-17.3467103157724,
6.42254609672779));
#174045=CARTESIAN_POINT('Ctrl Pts',(17.3537460096147,-17.3468246422803,
6.42253558892838));
#174046=CARTESIAN_POINT('Ctrl Pts',(17.3536825496168,-17.3468792122795,
6.42253057356556));
#174047=CARTESIAN_POINT('Ctrl Pts',(17.3535610892799,-17.3469836699825,
6.42252097353842));
#174048=CARTESIAN_POINT('Ctrl Pts',(17.3535030883777,-17.3470335570941,
6.42251638889736));
#174049=CARTESIAN_POINT('Ctrl Pts',(17.3533920237486,-17.3471290952818,
6.42250760921151));
#174050=CARTESIAN_POINT('Ctrl Pts',(17.3533389595992,-17.3471747458308,
6.42250341418939));
#174051=CARTESIAN_POINT('Ctrl Pts',(17.3532373039123,-17.3472622079599,
6.42249537717822));
#174052=CARTESIAN_POINT('Ctrl Pts',(17.3531887120005,-17.3473040191231,
6.42249153520608));
#174053=CARTESIAN_POINT('Ctrl Pts',(17.3530955863933,-17.3473841568981,
6.42248417166563));
#174054=CARTESIAN_POINT('Ctrl Pts',(17.3530510524237,-17.3474224831314,
6.42248065011431));
#174055=CARTESIAN_POINT('Ctrl Pts',(17.3529656723011,-17.3474959680257,
6.42247389823852));
#174056=CARTESIAN_POINT('Ctrl Pts',(17.3529248258877,-17.3475311263988,
6.42247066792569));
#174057=CARTESIAN_POINT('Ctrl Pts',(17.3528265963618,-17.3476156835672,
6.42246289909446));
#174058=CARTESIAN_POINT('Ctrl Pts',(17.3527692145124,-17.3476650839204,
6.42245836050928));
#174059=CARTESIAN_POINT('Ctrl Pts',(17.352655536496,-17.3477629605741,6.4224493685421));
#174060=CARTESIAN_POINT('Ctrl Pts',(17.3525992344936,-17.3478114417002,
6.42244491471103));
#174061=CARTESIAN_POINT('Ctrl Pts',(17.3524876634027,-17.3479075247515,
6.42243608811409));
#174062=CARTESIAN_POINT('Ctrl Pts',(17.3524324000683,-17.3479551215323,
6.42243171581548));
#174063=CARTESIAN_POINT('Ctrl Pts',(17.3523228802671,-17.3480494577653,
6.42242305025827));
#174064=CARTESIAN_POINT('Ctrl Pts',(17.3522686236564,-17.3480961971627,
6.42241875699954));
#174065=CARTESIAN_POINT('Ctrl Pts',(17.3521610845664,-17.3481888462976,
6.42241024696516));
#174066=CARTESIAN_POINT('Ctrl Pts',(17.3521078020635,-17.3482347558857,
6.42240603019835));
#174067=CARTESIAN_POINT('Ctrl Pts',(17.3520021798921,-17.348325771863,6.42239767070273));
#174068=CARTESIAN_POINT('Ctrl Pts',(17.3519498401874,-17.3483708781218,
6.42239352798124));
#174069=CARTESIAN_POINT('Ctrl Pts',(17.3518460738484,-17.3484603126104,
6.42238531425069));
#174070=CARTESIAN_POINT('Ctrl Pts',(17.3517946470405,-17.3485046408362,
6.42238124323756));
#174071=CARTESIAN_POINT('Ctrl Pts',(17.3516926772692,-17.3485925439932,
6.42237317063892));
#174072=CARTESIAN_POINT('Ctrl Pts',(17.3516421343707,-17.3486361187222,
6.42236916906777));
#174073=CARTESIAN_POINT('Ctrl Pts',(17.3459070467533,-17.3535810029808,
6.42191508219764));
#174074=CARTESIAN_POINT('Ctrl Pts',(17.3402486644273,-17.3585124571519,
6.4214637476894));
#174075=CARTESIAN_POINT('Ctrl Pts',(17.3243532093297,-17.3725152701771,
6.42018637321097));
#174076=CARTESIAN_POINT('Ctrl Pts',(17.3141777963635,-17.3816557758,6.41935744412653));
#174077=CARTESIAN_POINT('Ctrl Pts',(17.2915006215952,-17.4024271254078,
6.41748432679498));
#174078=CARTESIAN_POINT('Ctrl Pts',(17.2790496789871,-17.4141118093299,
6.41643788148387));
#174079=CARTESIAN_POINT('Ctrl Pts',(17.2402933392558,-17.4513749364202,
6.41312271720485));
#174080=CARTESIAN_POINT('Ctrl Pts',(17.2145118654067,-17.4774862759698,
6.41083142260862));
#174081=CARTESIAN_POINT('Ctrl Pts',(17.1336459612229,-17.5637607586575,
6.40335973354851));
#174082=CARTESIAN_POINT('Ctrl Pts',(17.0813595156129,-17.6264365499411,
6.39807659050608));
#174083=CARTESIAN_POINT('Ctrl Pts',(17.00200945163,-17.7335674757035,6.38932606776703));
#174084=CARTESIAN_POINT('Ctrl Pts',(16.9727332252932,-17.7762839414903,
6.38590397144071));
#174085=CARTESIAN_POINT('Ctrl Pts',(16.878437326321,-17.9253076325162,6.37425085273708));
#174086=CARTESIAN_POINT('Ctrl Pts',(16.8212373151914,-18.0362729447741,
6.36603542867206));
#174087=CARTESIAN_POINT('Ctrl Pts',(16.7705660899994,-18.1603530211319,
6.35775868565974));
#174088=CARTESIAN_POINT('Ctrl Pts',(16.7670644075452,-18.1690938493287,
6.35718035341813));
#174089=CARTESIAN_POINT('Ctrl Pts',(16.761951806765,-18.1821066556356,6.35632667497136));
#174090=CARTESIAN_POINT('Ctrl Pts',(16.7602962549954,-18.186360812135,6.35604874332209));
#174091=CARTESIAN_POINT('Ctrl Pts',(16.757370392281,-18.193951755447,6.35555490977215));
#174092=CARTESIAN_POINT('Ctrl Pts',(16.7560947526008,-18.197286425101,6.35533869165968));
#174093=CARTESIAN_POINT('Ctrl Pts',(16.7533649789617,-18.2044768272441,
6.35487402918853));
#174094=CARTESIAN_POINT('Ctrl Pts',(16.7519136689214,-18.2083335712921,
6.35462575431155));
#174095=CARTESIAN_POINT('Ctrl Pts',(16.7487731480944,-18.2167537661666,
6.35408574701506));
#174096=CARTESIAN_POINT('Ctrl Pts',(16.7470883891837,-18.2213188591448,
6.35379427708308));
#174097=CARTESIAN_POINT('Ctrl Pts',(16.7454193692319,-18.2258897639243,
6.3535036965741));
#174098=CARTESIAN_POINT('',(16.6170007251258,-18.9537521935254,6.8890562790225));
#174099=CARTESIAN_POINT('Ctrl Pts',(16.6170007251258,-18.9537521935254,
6.8890562790225));
#174100=CARTESIAN_POINT('Ctrl Pts',(16.6170993834536,-19.0729511321297,
6.88186870628082));
#174101=CARTESIAN_POINT('Ctrl Pts',(16.6272689227094,-19.1917453566806,
6.87468113353914));
#174102=CARTESIAN_POINT('Ctrl Pts',(16.6472858251195,-19.3088094062,6.86749356079746));
#174103=CARTESIAN_POINT('Ctrl Pts',(16.6595066892529,-19.3802801969733,
6.86310535186656));
#174104=CARTESIAN_POINT('Ctrl Pts',(16.6754275106646,-19.4512619171913,
6.85871714293566));
#174105=CARTESIAN_POINT('Ctrl Pts',(16.6949957094314,-19.5213421669286,
6.85432893400477));
#174106=CARTESIAN_POINT('Ctrl Pts',(16.7145348657469,-19.5913184059559,
6.8499472379035));
#174107=CARTESIAN_POINT('Ctrl Pts',(16.7377105245955,-19.6603953697142,
6.84556554180223));
#174108=CARTESIAN_POINT('Ctrl Pts',(16.7644188550042,-19.7281695132361,
6.84118384570096));
#174109=CARTESIAN_POINT('Ctrl Pts',(16.7910958009992,-19.7958640167457,
6.83680729844132));
#174110=CARTESIAN_POINT('Ctrl Pts',(16.8212969962484,-19.8622582946367,
6.83243075118168));
#174111=CARTESIAN_POINT('Ctrl Pts',(16.8548689277714,-19.9269643139033,
6.82805420392204));
#174112=CARTESIAN_POINT('Ctrl Pts',(16.8884195684633,-19.9916292975528,
6.82368043220506));
#174113=CARTESIAN_POINT('Ctrl Pts',(16.9253364824028,-20.0546077198004,
6.81930666048808));
#174114=CARTESIAN_POINT('Ctrl Pts',(16.9654187837192,-20.1155331887913,
6.81493288877111));
#174115=CARTESIAN_POINT('Ctrl Pts',(17.0054888878568,-20.1764401179574,
6.81056044800755));
#174116=CARTESIAN_POINT('Ctrl Pts',(17.0487222020848,-20.2352949313846,
6.806188007244));
#174117=CARTESIAN_POINT('Ctrl Pts',(17.0948736736053,-20.2917588910397,
6.80181556648045));
#174118=CARTESIAN_POINT('Ctrl Pts',(17.1410263252241,-20.3482242944845,
6.7974430139131));
#174119=CARTESIAN_POINT('Ctrl Pts',(17.1900969754572,-20.4022983505563,
6.79307046134575));
#174120=CARTESIAN_POINT('Ctrl Pts',(17.2418003884899,-20.4536755040318,
6.78869790877841));
#174121=CARTESIAN_POINT('Ctrl Pts',(17.2935574612748,-20.5051059786551,
6.78432081821108));
#174122=CARTESIAN_POINT('Ctrl Pts',(17.3479524093387,-20.5538336216567,
6.77994372764375));
#174123=CARTESIAN_POINT('Ctrl Pts',(17.4046638348791,-20.5995904709914,
6.77556663707642));
#174124=CARTESIAN_POINT('Ctrl Pts',(17.4614062326338,-20.6453723098397,
6.77118715601747));
#174125=CARTESIAN_POINT('Ctrl Pts',(17.5204672358496,-20.6881798414323,
6.76680767495852));
#174126=CARTESIAN_POINT('Ctrl Pts',(17.5814953303094,-20.7277877086919,
6.76242819389958));
#174127=CARTESIAN_POINT('Ctrl Pts',(17.6426315966569,-20.7674657806304,
6.75804095023986));
#174128=CARTESIAN_POINT('Ctrl Pts',(17.7057414989265,-20.8039326211616,
6.75365370658013));
#174129=CARTESIAN_POINT('Ctrl Pts',(17.7704482580137,-20.8370084987912,
6.74926646292041));
#174130=CARTESIAN_POINT('Ctrl Pts',(17.8144426190642,-20.8594969083952,
6.74628355998562));
#174131=CARTESIAN_POINT('Ctrl Pts',(17.8591746727794,-20.8804187619501,
6.74330065705082));
#174132=CARTESIAN_POINT('Ctrl Pts',(17.9045214391031,-20.8997305555473,
6.74031775411602));
#174133=CARTESIAN_POINT('Ctrl Pts',(17.9712319856139,-20.9281405262995,
6.73592954518513));
#174134=CARTESIAN_POINT('Ctrl Pts',(18.0395340178843,-20.9531746938961,
6.73154133625423));
#174135=CARTESIAN_POINT('Ctrl Pts',(18.1090523123257,-20.9746540454735,
6.72715312732333));
#174136=CARTESIAN_POINT('Ctrl Pts',(18.1784674300917,-20.9961015181319,
6.72277143122207));
#174137=CARTESIAN_POINT('Ctrl Pts',(18.2490947695194,-21.0140045070018,
6.71838973512081));
#174138=CARTESIAN_POINT('Ctrl Pts',(18.3205388114172,-21.0282318862631,
6.71400803901954));
#174139=CARTESIAN_POINT('Ctrl Pts',(18.39189890088,-21.0424425472215,6.70963149175991));
#174140=CARTESIAN_POINT('Ctrl Pts',(18.4640733156415,-21.0529860848151,
6.70525494450027));
#174141=CARTESIAN_POINT('Ctrl Pts',(18.5366526876864,-21.0597815442599,
6.70087839724063));
#174142=CARTESIAN_POINT('Ctrl Pts',(18.6091860309483,-21.066572694123,6.69650462552366));
#174143=CARTESIAN_POINT('Ctrl Pts',(18.6821233428378,-21.0696204372107,
6.69213085380669));
#174144=CARTESIAN_POINT('Ctrl Pts',(18.7550478100763,-21.0688953657871,
6.68775708208972));
#174145=CARTESIAN_POINT('Ctrl Pts',(18.8279500861544,-21.0681705150053,
6.68338464132617));
#174146=CARTESIAN_POINT('Ctrl Pts',(18.9008390432775,-21.0636751337982,
6.67901220056262));
#174147=CARTESIAN_POINT('Ctrl Pts',(18.9732972139342,-21.0554319203158,
6.67463975979907));
#174148=CARTESIAN_POINT('Ctrl Pts',(19.0457572373544,-21.0471884960535,
6.67026720723173));
#174149=CARTESIAN_POINT('Ctrl Pts',(19.1177859733785,-21.0351971057623,
6.66589465466438));
#174150=CARTESIAN_POINT('Ctrl Pts',(19.1889721056824,-21.0195321963759,
6.66152210209704));
#174151=CARTESIAN_POINT('Ctrl Pts',(19.2602321176395,-21.0038510293557,
6.65714501152972));
#174152=CARTESIAN_POINT('Ctrl Pts',(19.3306473077923,-20.9844888351851,
6.65276792096239));
#174153=CARTESIAN_POINT('Ctrl Pts',(19.399818395932,-20.9615708157809,6.64839083039507));
#174154=CARTESIAN_POINT('Ctrl Pts',(19.4690272609703,-20.9386402799958,
6.64401134933613));
#174155=CARTESIAN_POINT('Ctrl Pts',(19.5369902214611,-20.9121502278397,
6.63963186827719));
#174156=CARTESIAN_POINT('Ctrl Pts',(19.6033275197872,-20.8822742456295,
6.63525238721825));
#174157=CARTESIAN_POINT('Ctrl Pts',(19.6697824005294,-20.8523453084414,
6.63086514355853));
#174158=CARTESIAN_POINT('Ctrl Pts',(19.734605435538,-20.8190186771225,6.62647789989881));
#174159=CARTESIAN_POINT('Ctrl Pts',(19.7974415556865,-20.7825138780242,
6.62209065623909));
#174160=CARTESIAN_POINT('Ctrl Pts',(19.8401640625136,-20.7576941322312,
6.61910775330426));
#174161=CARTESIAN_POINT('Ctrl Pts',(19.8819686426644,-20.7314061565723,
6.61612485036943));
#174162=CARTESIAN_POINT('Ctrl Pts',(19.922752149464,-20.7037298099721,6.61314194743459));
#174163=CARTESIAN_POINT('Ctrl Pts',(19.982749592452,-20.6630145758598,6.6087537385037));
#174164=CARTESIAN_POINT('Ctrl Pts',(20.0407699602754,-20.6191338958608,
6.6043655295728));
#174165=CARTESIAN_POINT('Ctrl Pts',(20.0964596300333,-20.572306377365,6.5999773206419));
#174166=CARTESIAN_POINT('Ctrl Pts',(20.1520666470878,-20.5255483586707,
6.59559562454063));
#174167=CARTESIAN_POINT('Ctrl Pts',(20.2053494667968,-20.475852491549,6.59121392843937));
#174168=CARTESIAN_POINT('Ctrl Pts',(20.2559837460598,-20.4234803691282,
6.5868322323381));
#174169=CARTESIAN_POINT('Ctrl Pts',(20.3065585260151,-20.3711697881192,
6.58245568507846));
#174170=CARTESIAN_POINT('Ctrl Pts',(20.3544906143947,-20.3161895440789,
6.57807913781882));
#174171=CARTESIAN_POINT('Ctrl Pts',(20.3994903578942,-20.2588400314351,
6.57370259055918));
#174172=CARTESIAN_POINT('Ctrl Pts',(20.4444615632104,-20.2015268890188,
6.5693288188422));
#174173=CARTESIAN_POINT('Ctrl Pts',(20.4865038163916,-20.1418478378278,
6.56495504712523));
#174174=CARTESIAN_POINT('Ctrl Pts',(20.5253667770637,-20.0801374340179,
6.56058127540825));
#174175=CARTESIAN_POINT('Ctrl Pts',(20.5642179116064,-20.0184458088911,
6.5562088346447));
#174176=CARTESIAN_POINT('Ctrl Pts',(20.599891417463,-19.9547244662924,6.55183639388115));
#174177=CARTESIAN_POINT('Ctrl Pts',(20.6321804129397,-19.889336716411,6.54746395311759));
#174178=CARTESIAN_POINT('Ctrl Pts',(20.6644702340495,-19.8239472945576,
6.54309140055025));
#174179=CARTESIAN_POINT('Ctrl Pts',(20.6933751611701,-19.756891814226,6.5387188479829));
#174180=CARTESIAN_POINT('Ctrl Pts',(20.7187351546661,-19.6885564240657,
6.53434629541556));
#174181=CARTESIAN_POINT('Ctrl Pts',(20.7441214677199,-19.62015011286,6.52996920484823));
#174182=CARTESIAN_POINT('Ctrl Pts',(20.7659553334561,-19.5504616929154,
6.5255921142809));
#174183=CARTESIAN_POINT('Ctrl Pts',(20.784125904069,-19.479894665123,6.52121502371357));
#174184=CARTESIAN_POINT('Ctrl Pts',(20.8023063983049,-19.4092890980576,
6.51683554265463));
#174185=CARTESIAN_POINT('Ctrl Pts',(20.8168195180774,-19.337804440848,6.51245606159569));
#174186=CARTESIAN_POINT('Ctrl Pts',(20.8276056664129,-19.2658539685332,
6.50807658053674));
#174187=CARTESIAN_POINT('Ctrl Pts',(20.8384109331238,-19.1937759644891,
6.50368933687702));
#174188=CARTESIAN_POINT('Ctrl Pts',(20.8454759896224,-19.1212309770712,
6.4993020932173));
#174189=CARTESIAN_POINT('Ctrl Pts',(20.8487932306455,-19.0486363886742,
6.49491484955758));
#174190=CARTESIAN_POINT('Ctrl Pts',(20.8510486348926,-18.9992790637622,
6.49193194662277));
#174191=CARTESIAN_POINT('Ctrl Pts',(20.8515726338748,-18.9498988449408,
6.48894904368796));
#174192=CARTESIAN_POINT('Ctrl Pts',(20.8503765449711,-18.9006256883613,
6.48596614075315));
#174193=CARTESIAN_POINT('Ctrl Pts',(20.8486169543561,-18.8281389496101,
6.48157793182225));
#174194=CARTESIAN_POINT('Ctrl Pts',(20.8431255714046,-18.7556012223724,
6.47718972289135));
#174195=CARTESIAN_POINT('Ctrl Pts',(20.8338948009668,-18.6834281755797,
6.47280151396046));
#174196=CARTESIAN_POINT('Ctrl Pts',(20.8246777305229,-18.6113622455548,
6.46841981785919));
#174197=CARTESIAN_POINT('Ctrl Pts',(20.811732350535,-18.5396603960523,6.46403812175792));
#174198=CARTESIAN_POINT('Ctrl Pts',(20.7951030586572,-18.46873694369,6.45965642565666));
#174199=CARTESIAN_POINT('Ctrl Pts',(20.7784933075207,-18.3978968320285,
6.45527987839702));
#174200=CARTESIAN_POINT('Ctrl Pts',(20.758208353431,-18.3278337678025,6.45090333113738));
#174201=CARTESIAN_POINT('Ctrl Pts',(20.7343439967234,-18.2589539014087,
6.44652678387774));
#174202=CARTESIAN_POINT('Ctrl Pts',(20.710494774444,-18.1901177176251,6.44215301216076));
#174203=CARTESIAN_POINT('Ctrl Pts',(20.6830708110596,-18.1224636975236,
6.43777924044379));
#174204=CARTESIAN_POINT('Ctrl Pts',(20.652217910856,-18.0563834266433,6.43340546872682));
#174205=CARTESIAN_POINT('Ctrl Pts',(20.6213743992936,-17.9903232642113,
6.42903302796327));
#174206=CARTESIAN_POINT('Ctrl Pts',(20.5871042264079,-17.9258363370628,
6.42466058719971));
#174207=CARTESIAN_POINT('Ctrl Pts',(20.5496008974357,-17.8632932528772,
6.42028814643616));
#174208=CARTESIAN_POINT('Ctrl Pts',(20.5120966094992,-17.800748569458,6.41591559386882));
#174209=CARTESIAN_POINT('Ctrl Pts',(20.4713592511252,-17.7401482403578,
6.41154304130147));
#174210=CARTESIAN_POINT('Ctrl Pts',(20.4276268857995,-17.681835848523,6.40717048873413));
#174211=CARTESIAN_POINT('Ctrl Pts',(20.3838491333754,-17.6234629378886,
6.4027933981668));
#174212=CARTESIAN_POINT('Ctrl Pts',(20.3370704580446,-17.567383092118,6.39841630759947));
#174213=CARTESIAN_POINT('Ctrl Pts',(20.2875701403861,-17.5139079240533,
6.39403921703215));
#174214=CARTESIAN_POINT('Ctrl Pts',(20.2380427887669,-17.4604035512145,
6.38965973597321));
#174215=CARTESIAN_POINT('Ctrl Pts',(20.1857911812157,-17.409507025103,6.38528025491427));
#174216=CARTESIAN_POINT('Ctrl Pts',(20.1311305579265,-17.3614921552825,
6.38090077385533));
#174217=CARTESIAN_POINT('Ctrl Pts',(20.0763730490495,-17.3133921794275,
6.37651353019561));
#174218=CARTESIAN_POINT('Ctrl Pts',(20.0191983762075,-17.2681843592168,
6.37212628653589));
#174219=CARTESIAN_POINT('Ctrl Pts',(19.9599533753576,-17.2261010106471,
6.36773904287617));
#174220=CARTESIAN_POINT('Ctrl Pts',(19.9196724836144,-17.1974883887616,
6.36475613994135));
#174221=CARTESIAN_POINT('Ctrl Pts',(19.8784351648852,-17.170319212664,6.36177323700653));
#174222=CARTESIAN_POINT('Ctrl Pts',(19.8363568176099,-17.1446543090297,
6.35879033407171));
#174223=CARTESIAN_POINT('Ctrl Pts',(19.7744545085686,-17.1068981494093,
6.35440212514082));
#174224=CARTESIAN_POINT('Ctrl Pts',(19.7104893778666,-17.0722522374744,
6.35001391620992));
#174225=CARTESIAN_POINT('Ctrl Pts',(19.6448068261837,-17.0409479532526,
6.34562570727902));
#174226=CARTESIAN_POINT('Ctrl Pts',(19.5792217582977,-17.009690129779,6.34124401117776));
#174227=CARTESIAN_POINT('Ctrl Pts',(19.5119247612709,-16.9817642944955,
6.33686231507649));
#174228=CARTESIAN_POINT('Ctrl Pts',(19.4432882414199,-16.9573573777282,
6.33248061897523));
#174229=CARTESIAN_POINT('Ctrl Pts',(19.374732374942,-16.9329791410304,6.32810407171559));
#174230=CARTESIAN_POINT('Ctrl Pts',(19.3048405647341,-16.9121117694419,
6.32372752445595));
#174231=CARTESIAN_POINT('Ctrl Pts',(19.2340061739096,-16.8948945515477,
6.31935097719632));
#174232=CARTESIAN_POINT('Ctrl Pts',(19.1632167052263,-16.8776882525628,
6.31497720547934));
#174233=CARTESIAN_POINT('Ctrl Pts',(19.0914863095583,-16.8641276279119,
6.31060343376237));
#174234=CARTESIAN_POINT('Ctrl Pts',(19.019223169469,-16.8543020370897,6.3062296620454));
#174235=CARTESIAN_POINT('Ctrl Pts',(18.9469820192958,-16.8444794362278,
6.30185722128185));
#174236=CARTESIAN_POINT('Ctrl Pts',(18.8742089242435,-16.838389677678,6.2974847805183));
#174237=CARTESIAN_POINT('Ctrl Pts',(18.8013202474354,-16.8360706570669,
6.29311233975475));
#174238=CARTESIAN_POINT('Ctrl Pts',(18.7284297068557,-16.8337515771582,
6.2887397871874));
#174239=CARTESIAN_POINT('Ctrl Pts',(18.6554240608497,-16.8352034399581,
6.28436723462006));
#174240=CARTESIAN_POINT('Ctrl Pts',(18.5827210675518,-16.8404120466821,
6.27999468205272));
#174241=CARTESIAN_POINT('Ctrl Pts',(18.5099426203453,-16.8456260590946,
6.27561759148539));
#174242=CARTESIAN_POINT('Ctrl Pts',(18.4374679351514,-16.8546045652847,
6.27124050091807));
#174243=CARTESIAN_POINT('Ctrl Pts',(18.365710198337,-16.8672814046037,6.26686341035074));
#174244=CARTESIAN_POINT('Ctrl Pts',(18.2939132719592,-16.8799651672152,
6.2624839292918));
#174245=CARTESIAN_POINT('Ctrl Pts',(18.222834543912,-16.8963511759144,6.25810444823286));
#174246=CARTESIAN_POINT('Ctrl Pts',(18.1528748782451,-16.9163225715096,
6.25372496717392));
#174247=CARTESIAN_POINT('Ctrl Pts',(18.0827912095404,-16.9363293662694,
6.2493377235142));
#174248=CARTESIAN_POINT('Ctrl Pts',(18.0138310210299,-16.9599340823954,
6.24495047985448));
#174249=CARTESIAN_POINT('Ctrl Pts',(17.9463773894275,-16.9869708339786,
6.24056323619476));
#174250=CARTESIAN_POINT('Ctrl Pts',(17.9005154197541,-17.0053532198,6.23758033325993));
#174251=CARTESIAN_POINT('Ctrl Pts',(17.8553494637707,-17.0253211191867,
6.23459743032511));
#174252=CARTESIAN_POINT('Ctrl Pts',(17.810993130072,-17.0468104246386,6.23161452739028));
#174253=CARTESIAN_POINT('Ctrl Pts',(17.7457580547156,-17.0784148505146,
6.22722755755964));
#174254=CARTESIAN_POINT('Ctrl Pts',(17.6820207921123,-17.1134353687213,
6.22284058772901));
#174255=CARTESIAN_POINT('Ctrl Pts',(17.6201625345959,-17.1517069403394,
6.21845361789837));
#174256=CARTESIAN_POINT('Ctrl Pts',(17.5583882674463,-17.1899265472972,
6.21407260464039));
#174257=CARTESIAN_POINT('Ctrl Pts',(17.4984883504377,-17.231388199258,6.20969159138242));
#174258=CARTESIAN_POINT('Ctrl Pts',(17.4408213800094,-17.2758800589459,
6.20531057812444));
#174259=CARTESIAN_POINT('Ctrl Pts',(17.3832136794369,-17.3203261900983,
6.20093406765239));
#174260=CARTESIAN_POINT('Ctrl Pts',(17.3278347507031,-17.3677960551435,
6.19655755718035));
#174261=CARTESIAN_POINT('Ctrl Pts',(17.2750146386688,-17.4180343173913,
6.19218104670831));
#174262=CARTESIAN_POINT('Ctrl Pts',(17.2222313878218,-17.4682375202285,
6.1878075904398));
#174263=CARTESIAN_POINT('Ctrl Pts',(17.1720037564618,-17.5212049524845,
6.18343413417128));
#174264=CARTESIAN_POINT('Ctrl Pts',(17.1246277766843,-17.5766418478011,
6.17906067790277));
#174265=CARTESIAN_POINT('Ctrl Pts',(17.0772569743065,-17.6320726847952,
6.17468769957965));
#174266=CARTESIAN_POINT('Ctrl Pts',(17.0327375273207,-17.6899720904902,
6.17031472125653));
#174267=CARTESIAN_POINT('Ctrl Pts',(16.9913267830639,-17.7500103748477,
6.16594174293342));
#174268=CARTESIAN_POINT('Ctrl Pts',(16.9499189762258,-17.8100444004656,
6.16156907480197));
#174269=CARTESIAN_POINT('Ctrl Pts',(16.9116197015766,-17.8722166017246,
6.15719640667052));
#174270=CARTESIAN_POINT('Ctrl Pts',(16.8766431790062,-17.9361680062591,
6.15282373853907));
#174271=CARTESIAN_POINT('Ctrl Pts',(16.8416426205708,-18.0001633581963,
6.14844806551025));
#174272=CARTESIAN_POINT('Ctrl Pts',(16.8099695961693,-18.0659399263405,
6.14407239248142));
#174273=CARTESIAN_POINT('Ctrl Pts',(16.7817919876685,-18.1331148575113,
6.1396967194526));
#174274=CARTESIAN_POINT('Ctrl Pts',(16.768936728617,-18.1637615726841,6.1377004389553));
#174275=CARTESIAN_POINT('Ctrl Pts',(16.7568083399034,-18.194699064005,6.13570415845801));
#174276=CARTESIAN_POINT('Ctrl Pts',(16.7454193692319,-18.2258897639242,
6.13370787796071));
#174277=CARTESIAN_POINT('Ctrl Pts',(16.7486737197731,-18.2270709325543,
6.93361858681016));
#174278=CARTESIAN_POINT('Ctrl Pts',(16.6638908378346,-18.4600474814419,
6.9187647400854));
#174279=CARTESIAN_POINT('Ctrl Pts',(16.617844373311,-18.7072442534351,6.90391089336065));
#174280=CARTESIAN_POINT('Ctrl Pts',(16.6156461116265,-18.9537405764282,
6.88905704663589));
#174281=CARTESIAN_POINT('Origin',(18.734,-18.952,0.));
#174282=CARTESIAN_POINT('',(16.7454193380512,-18.2258898493182,7.95734463868439));
#174283=CARTESIAN_POINT('',(16.7454193803187,-18.2258897335611,7.73405220804246));
#174284=CARTESIAN_POINT('',(16.7454193692319,-18.2258897639242,0.));
#174285=CARTESIAN_POINT('',(16.6170007998212,-18.953910682177,7.9107295246413));
#174286=CARTESIAN_POINT('Ctrl Pts',(16.7454193380512,-18.2258898493182,
7.95734463868439));
#174287=CARTESIAN_POINT('Ctrl Pts',(16.7388878433806,-18.243777498986,7.9562441231521));
#174288=CARTESIAN_POINT('Ctrl Pts',(16.7325959958868,-18.2617579488697,
7.95513588188335));
#174289=CARTESIAN_POINT('Ctrl Pts',(16.7220479742774,-18.2932597408547,
7.95318937778389));
#174290=CARTESIAN_POINT('Ctrl Pts',(16.7176850471954,-18.3067375112457,
7.95235505144709));
#174291=CARTESIAN_POINT('Ctrl Pts',(16.7109455013963,-18.3282930398624,
7.95101781937374));
#174292=CARTESIAN_POINT('Ctrl Pts',(16.708481192049,-18.3363430890846,7.95051779053978));
#174293=CARTESIAN_POINT('Ctrl Pts',(16.7042135147882,-18.350587130326,7.94963182308968));
#174294=CARTESIAN_POINT('Ctrl Pts',(16.7023903094468,-18.3567751020104,
7.94924653872907));
#174295=CARTESIAN_POINT('Ctrl Pts',(16.698671982321,-18.3696112555395,7.94844645204706));
#174296=CARTESIAN_POINT('Ctrl Pts',(16.696781087097,-18.3762605725066,7.94803151715826));
#174297=CARTESIAN_POINT('Ctrl Pts',(16.6919991061119,-18.3933949133956,
7.94696100415976));
#174298=CARTESIAN_POINT('Ctrl Pts',(16.6891562199663,-18.4038930745159,
7.94630386874284));
#174299=CARTESIAN_POINT('Ctrl Pts',(16.6831809228324,-18.4266522578334,
7.94487642810954));
#174300=CARTESIAN_POINT('Ctrl Pts',(16.6800773158945,-18.4389203431502,
7.94410521854318));
#174301=CARTESIAN_POINT('Ctrl Pts',(16.6713662558257,-18.4747000300723,
7.94185062425237));
#174302=CARTESIAN_POINT('Ctrl Pts',(16.6660513913002,-18.4982801519989,
7.94035801902177));
#174303=CARTESIAN_POINT('Ctrl Pts',(16.6316558078731,-18.6640664717024,
7.92981461318329));
#174304=CARTESIAN_POINT('Ctrl Pts',(16.6168699505192,-18.8088166883431,
7.92031687728472));
#174305=CARTESIAN_POINT('Ctrl Pts',(16.6170008616855,-18.9539100721132,
7.91072945673524));
#174306=CARTESIAN_POINT('Ctrl Pts',(16.6170008622295,-18.9539106750009,
7.91072941689788));
#174307=CARTESIAN_POINT('Ctrl Pts',(16.6171115217675,-19.076519777243,7.90262770333203));
#174308=CARTESIAN_POINT('Ctrl Pts',(16.6278735763027,-19.1989019504627,
7.89450601028431));
#174309=CARTESIAN_POINT('Ctrl Pts',(16.651355511568,-19.3320510967405,7.88604139066189));
#174310=CARTESIAN_POINT('Ctrl Pts',(16.653648122358,-19.3444066550615,7.88525964948426));
#174311=CARTESIAN_POINT('Ctrl Pts',(16.6573287548186,-19.3633030864107,
7.88407054302234));
#174312=CARTESIAN_POINT('Ctrl Pts',(16.6586379310683,-19.3698587978723,
7.88365920698068));
#174313=CARTESIAN_POINT('Ctrl Pts',(16.6608486751434,-19.3806623838382,
7.88298344279256));
#174314=CARTESIAN_POINT('Ctrl Pts',(16.6617322871274,-19.3849138274746,
7.88271805353515));
#174315=CARTESIAN_POINT('Ctrl Pts',(16.6634789752581,-19.3931900145513,
7.88220251642844));
#174316=CARTESIAN_POINT('Ctrl Pts',(16.66434072061,-19.3972150163006,7.88195229568187));
#174317=CARTESIAN_POINT('Ctrl Pts',(16.6659719860138,-19.4047271642203,
7.88148626424512));
#174318=CARTESIAN_POINT('Ctrl Pts',(16.6667385814108,-19.4082148389771,
7.88127029567999));
#174319=CARTESIAN_POINT('Ctrl Pts',(16.6685067296305,-19.4161631714684,
7.88077899629613));
#174320=CARTESIAN_POINT('Ctrl Pts',(16.6695139068702,-19.4206225259872,
7.88050399138715));
#174321=CARTESIAN_POINT('Ctrl Pts',(16.6726472979753,-19.434289685709,7.87966300011892));
#174322=CARTESIAN_POINT('Ctrl Pts',(16.6748207597528,-19.4434866906781,
7.87909965574805));
#174323=CARTESIAN_POINT('Ctrl Pts',(16.7060513529335,-19.5717941851,7.87127264400984));
#174324=CARTESIAN_POINT('Ctrl Pts',(16.7453452201725,-19.6881939778768,
7.86455350603832));
#174325=CARTESIAN_POINT('Ctrl Pts',(16.8230773612645,-19.8658632020382,
7.85400319292143));
#174326=CARTESIAN_POINT('Ctrl Pts',(16.8549331345859,-19.9296905752479,
7.85014915513843));
#174327=CARTESIAN_POINT('Ctrl Pts',(16.9337301852796,-20.06943621804,7.84135924496039));
#174328=CARTESIAN_POINT('Ctrl Pts',(16.9823692282751,-20.1442342433673,
7.83640088446753));
#174329=CARTESIAN_POINT('Ctrl Pts',(17.0559431208771,-20.243115176939,7.8293099492823));
#174330=CARTESIAN_POINT('Ctrl Pts',(17.0769699627459,-20.2699926221172,
7.82732374507707));
#174331=CARTESIAN_POINT('Ctrl Pts',(17.1055477671658,-20.3047567339904,
7.82466995656501));
#174332=CARTESIAN_POINT('Ctrl Pts',(17.1125238594664,-20.3131107871754,
7.82402557515981));
#174333=CARTESIAN_POINT('Ctrl Pts',(17.1240367787783,-20.3266836866202,
7.82296750386227));
#174334=CARTESIAN_POINT('Ctrl Pts',(17.1285353613239,-20.3319348188096,
7.82255538620189));
#174335=CARTESIAN_POINT('Ctrl Pts',(17.1372800548251,-20.3420417345859,
7.82175675862704));
#174336=CARTESIAN_POINT('Ctrl Pts',(17.1415227966835,-20.3469003414935,
7.82137039098903));
#174337=CARTESIAN_POINT('Ctrl Pts',(17.1513514831502,-20.3580524465649,
7.82047783722391));
#174338=CARTESIAN_POINT('Ctrl Pts',(17.1569528523282,-20.3643321497455,
7.81997100799802));
#174339=CARTESIAN_POINT('Ctrl Pts',(17.1720750619579,-20.3810835485491,
7.81860750014261));
#174340=CARTESIAN_POINT('Ctrl Pts',(17.1816635957588,-20.3914933044688,
7.8177479646193));
#174341=CARTESIAN_POINT('Ctrl Pts',(17.265823056454,-20.4810419237264,7.81024568946596));
#174342=CARTESIAN_POINT('Ctrl Pts',(17.3462728239971,-20.5544105810415,
7.80334335793242));
#174343=CARTESIAN_POINT('Ctrl Pts',(17.5090247580217,-20.6813552124303,
7.7899035908775));
#174344=CARTESIAN_POINT('Ctrl Pts',(17.5901246453396,-20.7360351827152,
7.78341836997606));
#174345=CARTESIAN_POINT('Ctrl Pts',(17.7369467988554,-20.8208878484442,
7.77224124367338));
#174346=CARTESIAN_POINT('Ctrl Pts',(17.8009843717867,-20.8536677278415,
7.76753719849889));
#174347=CARTESIAN_POINT('Ctrl Pts',(17.8972767156947,-20.8969206459371,
7.76082211149693));
#174348=CARTESIAN_POINT('Ctrl Pts',(17.9283104656962,-20.9099802971092,
7.75871046801823));
#174349=CARTESIAN_POINT('Ctrl Pts',(17.9664249726907,-20.924959871533,7.75619159313983));
#174350=CARTESIAN_POINT('Ctrl Pts',(17.9732193413863,-20.9275897525189,
7.75574541884126));
#174351=CARTESIAN_POINT('Ctrl Pts',(17.9839074333896,-20.9316634523034,
7.755048162355));
#174352=CARTESIAN_POINT('Ctrl Pts',(17.987791984554,-20.9331309500479,7.75479569918502));
#174353=CARTESIAN_POINT('Ctrl Pts',(17.9950209767194,-20.9358376252837,
7.75432767776961));
#174354=CARTESIAN_POINT('Ctrl Pts',(17.9983641988263,-20.9370797688359,
7.75411194825751));
#174355=CARTESIAN_POINT('Ctrl Pts',(18.0059513417284,-20.9398769024159,
7.75362398255835));
#174356=CARTESIAN_POINT('Ctrl Pts',(18.0101971021762,-20.9414267500821,
7.75335205481275));
#174357=CARTESIAN_POINT('Ctrl Pts',(18.0228091197682,-20.9459848480949,
7.75254757455099));
#174358=CARTESIAN_POINT('Ctrl Pts',(18.0311895194472,-20.948954049858,7.75201728824248));
#174359=CARTESIAN_POINT('Ctrl Pts',(18.0942291797181,-20.9708431992103,
7.74805857365614));
#174360=CARTESIAN_POINT('Ctrl Pts',(18.1496297674981,-20.9875705011626,
7.74474953633496));
#174361=CARTESIAN_POINT('Ctrl Pts',(18.3636968877658,-21.0427420527988,
7.73236241282067));
#174362=CARTESIAN_POINT('Ctrl Pts',(18.5259285032051,-21.0650639754516,
7.72375592421126));
#174363=CARTESIAN_POINT('Ctrl Pts',(18.7491574877104,-21.0697972336905,
7.71138810956231));
#174364=CARTESIAN_POINT('Ctrl Pts',(18.8092159985676,-21.0685152079866,
7.70801427462215));
#174365=CARTESIAN_POINT('Ctrl Pts',(18.8932732959909,-21.0631385600472,
7.70317746656741));
#174366=CARTESIAN_POINT('Ctrl Pts',(18.9173818273774,-21.0611811303556,
7.70177705748212));
#174367=CARTESIAN_POINT('Ctrl Pts',(18.9594296016217,-21.0570408223668,
7.69930862404411));
#174368=CARTESIAN_POINT('Ctrl Pts',(18.9773845148172,-21.0550404934509,
7.69824627062485));
#174369=CARTESIAN_POINT('Ctrl Pts',(19.0037818369706,-21.051757038755,7.69667131928106));
#174370=CARTESIAN_POINT('Ctrl Pts',(19.0122459006903,-21.0506522048338,
7.6961643408173));
#174371=CARTESIAN_POINT('Ctrl Pts',(19.027090020576,-21.0486231889878,7.69527163609937));
#174372=CARTESIAN_POINT('Ctrl Pts',(19.0334730069536,-21.0477209913177,
7.69488660955054));
#174373=CARTESIAN_POINT('Ctrl Pts',(19.0458711036871,-21.0459107956361,
7.69413644759044));
#174374=CARTESIAN_POINT('Ctrl Pts',(19.0518866226705,-21.0450059960072,
7.69377141708849));
#174375=CARTESIAN_POINT('Ctrl Pts',(19.0662768248414,-21.0427780841774,
7.69289563764516));
#174376=CARTESIAN_POINT('Ctrl Pts',(19.0746475740017,-21.0414305713898,
7.69238411877348));
#174377=CARTESIAN_POINT('Ctrl Pts',(19.1049386345306,-21.0363674899412,
7.69052542608143));
#174378=CARTESIAN_POINT('Ctrl Pts',(19.1268075698795,-21.0323570505082,
7.68916892989207));
#174379=CARTESIAN_POINT('Ctrl Pts',(19.3293697769554,-20.9919023681982,
7.67646415885305));
#174380=CARTESIAN_POINT('Ctrl Pts',(19.5046095698364,-20.9323536748864,
7.66432894762078));
#174381=CARTESIAN_POINT('Ctrl Pts',(19.7425292966968,-20.8150933724153,
7.64681469631331));
#174382=CARTESIAN_POINT('Ctrl Pts',(19.8130652399463,-20.7751478843502,
7.64149137483685));
#174383=CARTESIAN_POINT('Ctrl Pts',(19.9116141894632,-20.7116102705018,
7.63401527075843));
#174384=CARTESIAN_POINT('Ctrl Pts',(19.9415782464914,-20.6911833216775,
7.63173707279578));
#174385=CARTESIAN_POINT('Ctrl Pts',(19.9770748889911,-20.6656247458028,
7.62904596747366));
#174386=CARTESIAN_POINT('Ctrl Pts',(19.9831219110962,-20.6612218709477,
7.62858780578386));
#174387=CARTESIAN_POINT('Ctrl Pts',(19.9924973882524,-20.6543191969485,
7.62787806211732));
#174388=CARTESIAN_POINT('Ctrl Pts',(19.9958419518017,-20.6518415261133,
7.62762499202941));
#174389=CARTESIAN_POINT('Ctrl Pts',(20.0020379817709,-20.6472231091899,
7.62715642092181));
#174390=CARTESIAN_POINT('Ctrl Pts',(20.0048913206027,-20.6450850435348,
7.6269407450377));
#174391=CARTESIAN_POINT('Ctrl Pts',(20.0113387267232,-20.6402283863224,
7.62645363115794));
#174392=CARTESIAN_POINT('Ctrl Pts',(20.0149295140985,-20.637505528898,7.62618249709004));
#174393=CARTESIAN_POINT('Ctrl Pts',(20.0257622304005,-20.6292365794639,
7.62536492091644));
#174394=CARTESIAN_POINT('Ctrl Pts',(20.0329771437777,-20.6236550451822,
7.62482091120557));
#174395=CARTESIAN_POINT('Ctrl Pts',(20.0884445674614,-20.5801688919378,
7.62064071834189));
#174396=CARTESIAN_POINT('Ctrl Pts',(20.1350693845819,-20.5402254539061,
7.61713897371162));
#174397=CARTESIAN_POINT('Ctrl Pts',(20.2871671507481,-20.3980043852527,
7.60550202522887));
#174398=CARTESIAN_POINT('Ctrl Pts',(20.3837128764582,-20.2868066810572,
7.59771463143669));
#174399=CARTESIAN_POINT('Ctrl Pts',(20.5211894319472,-20.090528536099,7.58451611416308));
#174400=CARTESIAN_POINT('Ctrl Pts',(20.5693480780316,-20.0111448654155,
7.57930756107859));
#174401=CARTESIAN_POINT('Ctrl Pts',(20.6218684703958,-19.9101679373517,
7.57267773484364));
#174402=CARTESIAN_POINT('Ctrl Pts',(20.631313294231,-19.8913270857248,7.57144083723901));
#174403=CARTESIAN_POINT('Ctrl Pts',(20.6443685992348,-19.8642834134045,
7.56966428738855));
#174404=CARTESIAN_POINT('Ctrl Pts',(20.6482109146407,-19.8561934427054,
7.56913270131874));
#174405=CARTESIAN_POINT('Ctrl Pts',(20.6547601154102,-19.8421752897911,
7.56821123358712));
#174406=CARTESIAN_POINT('Ctrl Pts',(20.6574911942651,-19.8362584981922,
7.56782219454299));
#174407=CARTESIAN_POINT('Ctrl Pts',(20.6626743627559,-19.8248916983921,
7.5670745673735));
#174408=CARTESIAN_POINT('Ctrl Pts',(20.6651307823195,-19.819443724465,7.56671613300442));
#174409=CARTESIAN_POINT('Ctrl Pts',(20.6714718854522,-19.8052196687878,
7.56577998895957));
#174410=CARTESIAN_POINT('Ctrl Pts',(20.6753199833069,-19.7964275148245,
7.56520103251628));
#174411=CARTESIAN_POINT('Ctrl Pts',(20.6883056550384,-19.7661998401453,
7.56320933242042));
#174412=CARTESIAN_POINT('Ctrl Pts',(20.6971487798813,-19.7446403806079,
7.56178664609279));
#174413=CARTESIAN_POINT('Ctrl Pts',(20.7678888704943,-19.5637267355981,
7.54982644524309));
#174414=CARTESIAN_POINT('Ctrl Pts',(20.8106183403783,-19.3975873328279,
7.53862561343313));
#174415=CARTESIAN_POINT('Ctrl Pts',(20.8446804915029,-19.1387026609447,
7.52137064430835));
#174416=CARTESIAN_POINT('Ctrl Pts',(20.850720204172,-19.0485794585914,7.51541603746372));
#174417=CARTESIAN_POINT('Ctrl Pts',(20.8511061996304,-18.9197162415058,
7.50718304618558));
#174418=CARTESIAN_POINT('Ctrl Pts',(20.8501647981973,-18.8810924327384,
7.50475213048953));
#174419=CARTESIAN_POINT('Ctrl Pts',(20.8477729663797,-18.8349065986079,
7.50190597659676));
#174420=CARTESIAN_POINT('Ctrl Pts',(20.8473379761702,-18.8273018822425,
7.50143932087353));
#174421=CARTESIAN_POINT('Ctrl Pts',(20.8465999633302,-18.8155156848552,
7.50071931190345));
#174422=CARTESIAN_POINT('Ctrl Pts',(20.8463255543148,-18.8113325672559,
7.50046440174732));
#174423=CARTESIAN_POINT('Ctrl Pts',(20.8457949348328,-18.8035956612786,
7.49999413736087));
#174424=CARTESIAN_POINT('Ctrl Pts',(20.8455421805573,-18.8000417341095,
7.49977859742441));
#174425=CARTESIAN_POINT('Ctrl Pts',(20.8449522838862,-18.7920330895462,
7.49929394487906));
#174426=CARTESIAN_POINT('Ctrl Pts',(20.844610013377,-18.7875788044112,7.49902512302226));
#174427=CARTESIAN_POINT('Ctrl Pts',(20.8435638848998,-18.7745063891234,
7.49823825540963));
#174428=CARTESIAN_POINT('Ctrl Pts',(20.8428213141118,-18.7658913292997,
7.49772233096261));
#174429=CARTESIAN_POINT('Ctrl Pts',(20.8372749449805,-18.7058464243521,
7.49414339381277));
#174430=CARTESIAN_POINT('Ctrl Pts',(20.8306426326194,-18.6545984492913,
7.49117536667984));
#174431=CARTESIAN_POINT('Ctrl Pts',(20.8185581711124,-18.582161657239,7.48703946443716));
#174432=CARTESIAN_POINT('Ctrl Pts',(20.8146436848486,-18.5607391274452,
7.48582377721568));
#174433=CARTESIAN_POINT('Ctrl Pts',(20.80140135268,-18.4941005975533,7.48205535319941));
#174434=CARTESIAN_POINT('Ctrl Pts',(20.7909244439018,-18.4491259666275,
7.47953088872672));
#174435=CARTESIAN_POINT('Ctrl Pts',(20.7507051679,-18.2988937538901,7.47106355920194));
#174436=CARTESIAN_POINT('Ctrl Pts',(20.7142829501654,-18.1956098512443,
7.46517521627707));
#174437=CARTESIAN_POINT('Ctrl Pts',(20.647750716248,-18.0452006831621,7.45603029254469));
#174438=CARTESIAN_POINT('Ctrl Pts',(20.6234958509789,-17.9956885504537,
7.45292243941184));
#174439=CARTESIAN_POINT('Ctrl Pts',(20.581052886092,-17.9169822014336,7.44777792058188));
#174440=CARTESIAN_POINT('Ctrl Pts',(20.5640366625488,-17.8871846054571,
7.44578065273709));
#174441=CARTESIAN_POINT('Ctrl Pts',(20.540717737575,-17.8485613490703,7.44311982723011));
#174442=CARTESIAN_POINT('Ctrl Pts',(20.5350602037008,-17.8393509197776,
7.44247980191957));
#174443=CARTESIAN_POINT('Ctrl Pts',(20.5256770234057,-17.8243342562632,
7.44142707182663));
#174444=CARTESIAN_POINT('Ctrl Pts',(20.5219930481673,-17.8185021200854,
7.44101590846227));
#174445=CARTESIAN_POINT('Ctrl Pts',(20.5148057904764,-17.8072461282298,
7.44021783758158));
#174446=CARTESIAN_POINT('Ctrl Pts',(20.5113060651323,-17.801820083753,7.43983106547224));
#174447=CARTESIAN_POINT('Ctrl Pts',(20.5031665829805,-17.7893263221723,
7.43893569814861));
#174448=CARTESIAN_POINT('Ctrl Pts',(20.4985092235669,-17.7822702550774,
7.43842644685737));
#174449=CARTESIAN_POINT('Ctrl Pts',(20.4858668730179,-17.7633639559323,
7.43705217979012));
#174450=CARTESIAN_POINT('Ctrl Pts',(20.4778040672908,-17.7515665177865,
7.43618423622166));
#174451=CARTESIAN_POINT('Ctrl Pts',(20.40274250566,-17.6440891103439,7.42817965058385));
#174452=CARTESIAN_POINT('Ctrl Pts',(20.3280628868999,-17.5540414314203,
7.4207414655405));
#174453=CARTESIAN_POINT('Ctrl Pts',(20.1325800273237,-17.3544713805741,
7.40249414441274));
#174454=CARTESIAN_POINT('Ctrl Pts',(20.005810433897,-17.251817052567,7.39154529268232));
#174455=CARTESIAN_POINT('Ctrl Pts',(19.8409604834936,-17.1471745792833,
7.37913630684207));
#174456=CARTESIAN_POINT('Ctrl Pts',(19.8129750486933,-17.1303058906809,
7.37708848181603));
#174457=CARTESIAN_POINT('Ctrl Pts',(19.7783138750587,-17.1104924376088,
7.37463335252583));
#174458=CARTESIAN_POINT('Ctrl Pts',(19.7720005474634,-17.1069264407745,
7.37418939548587));
#174459=CARTESIAN_POINT('Ctrl Pts',(19.7620781525388,-17.1013889599327,
7.3734968452897));
#174460=CARTESIAN_POINT('Ctrl Pts',(19.7584815194936,-17.0993954749522,
7.37324687611266));
#174461=CARTESIAN_POINT('Ctrl Pts',(19.7517502349969,-17.0956901618897,
7.37278106367706));
#174462=CARTESIAN_POINT('Ctrl Pts',(19.7486170944442,-17.0939758053795,
7.37256506405661));
#174463=CARTESIAN_POINT('Ctrl Pts',(19.741458172694,-17.090082175408,7.37207337135263));
#174464=CARTESIAN_POINT('Ctrl Pts',(19.7374296600905,-17.0879080297863,
7.37179800622117));
#174465=CARTESIAN_POINT('Ctrl Pts',(19.725036134151,-17.0812711932295,7.37095481735169));
#174466=CARTESIAN_POINT('Ctrl Pts',(19.7166480362049,-17.0768515439621,
7.37038965572208));
#174467=CARTESIAN_POINT('Ctrl Pts',(19.6008142323478,-17.0168099874429,
7.36265695354855));
#174468=CARTESIAN_POINT('Ctrl Pts',(19.4888059357739,-16.9704339864077,
7.35601945711191));
#174469=CARTESIAN_POINT('Ctrl Pts',(19.2028079839835,-16.8798165665215,
7.33969350389045));
#174470=CARTESIAN_POINT('Ctrl Pts',(19.0260364714918,-16.8476158197381,
7.33007481375237));
#174471=CARTESIAN_POINT('Ctrl Pts',(18.8258763910339,-16.8368855460631,
7.31840384695642));
#174472=CARTESIAN_POINT('Ctrl Pts',(18.8044107491275,-16.8360622171434,
7.31714349183365));
#174473=CARTESIAN_POINT('Ctrl Pts',(18.7739144147734,-16.8353570713255,
7.315339102029));
#174474=CARTESIAN_POINT('Ctrl Pts',(18.7648908377787,-16.8352061507281,
7.31480348852575));
#174475=CARTESIAN_POINT('Ctrl Pts',(18.7493378582586,-16.8350454940832,
7.31387725390126));
#174476=CARTESIAN_POINT('Ctrl Pts',(18.7428088200906,-16.8350082585817,
7.31348749923424));
#174477=CARTESIAN_POINT('Ctrl Pts',(18.7303180279547,-16.834994807401,7.31274004039551));
#174478=CARTESIAN_POINT('Ctrl Pts',(18.7243563334241,-16.8350135709045,
7.31238249740935));
#174479=CARTESIAN_POINT('Ctrl Pts',(18.7088771926739,-16.8351276762229,
7.31145207142552));
#174480=CARTESIAN_POINT('Ctrl Pts',(18.6993602462997,-16.8352620205945,
7.31087797149548));
#174481=CARTESIAN_POINT('Ctrl Pts',(18.6670303152539,-16.8359364892103,
7.30892055874067));
#174482=CARTESIAN_POINT('Ctrl Pts',(18.6442259049728,-16.8367812717643,
7.30752775950298));
#174483=CARTESIAN_POINT('Ctrl Pts',(18.4439242482592,-16.8474462853925,
7.2951834561723));
#174484=CARTESIAN_POINT('Ctrl Pts',(18.268337319563,-16.8792182421591,7.28350740653347));
#174485=CARTESIAN_POINT('Ctrl Pts',(18.0173334357542,-16.9581655260814,
7.26612446145114));
#174486=CARTESIAN_POINT('Ctrl Pts',(17.9374624013684,-16.9887077134318,
7.26049815820106));
#174487=CARTESIAN_POINT('Ctrl Pts',(17.8255729342821,-17.0394494914775,
7.25265696252434));
#174488=CARTESIAN_POINT('Ctrl Pts',(17.7919077540756,-17.0558059752339,
7.250303840077));
#174489=CARTESIAN_POINT('Ctrl Pts',(17.7519919183697,-17.076525098068,7.24753653630727));
#174490=CARTESIAN_POINT('Ctrl Pts',(17.7453107276195,-17.0800385936707,
7.24707412250526));
#174491=CARTESIAN_POINT('Ctrl Pts',(17.7349616587644,-17.085551811115,7.24635923847559));
#174492=CARTESIAN_POINT('Ctrl Pts',(17.7312807434474,-17.087526738651,7.24610524586216));
#174493=CARTESIAN_POINT('Ctrl Pts',(17.7244699970279,-17.0912069227537,
7.24563583071761));
#174494=CARTESIAN_POINT('Ctrl Pts',(17.7213386544485,-17.0929091730773,
7.24542022787485));
#174495=CARTESIAN_POINT('Ctrl Pts',(17.7142752475803,-17.0967721007728,
7.24493437020623));
#174496=CARTESIAN_POINT('Ctrl Pts',(17.7103457550295,-17.0989373684697,
7.24466441260949));
#174497=CARTESIAN_POINT('Ctrl Pts',(17.6987856658911,-17.1053553150359,
7.24387112546098));
#174498=CARTESIAN_POINT('Ctrl Pts',(17.6911743668109,-17.1096428102119,
7.24334996948272));
#174499=CARTESIAN_POINT('Ctrl Pts',(17.6369037156688,-17.1406579084608,
7.23964068144928));
#174500=CARTESIAN_POINT('Ctrl Pts',(17.591246918417,-17.1691099680363,7.23655557857932));
#174501=CARTESIAN_POINT('Ctrl Pts',(17.4071719508445,-17.293800556916,7.22405649839376));
#174502=CARTESIAN_POINT('Ctrl Pts',(17.2794064967081,-17.4046591977115,
7.21518662745224));
#174503=CARTESIAN_POINT('Ctrl Pts',(17.111546472248,-17.5896734100594,7.20134224817517));
#174504=CARTESIAN_POINT('Ctrl Pts',(17.0604711081228,-17.6529279660675,
7.19675114253332));
#174505=CARTESIAN_POINT('Ctrl Pts',(17.0017259821591,-17.7349128743434,
7.19086729246939));
#174506=CARTESIAN_POINT('Ctrl Pts',(16.9905151964005,-17.7510274584236,
7.18971400672685));
#174507=CARTESIAN_POINT('Ctrl Pts',(16.974659743329,-17.7745083382265,7.1880370588382));
#174508=CARTESIAN_POINT('Ctrl Pts',(16.9698336762098,-17.7817513380291,
7.18752025935566));
#174509=CARTESIAN_POINT('Ctrl Pts',(16.9614964374229,-17.7944327137419,
7.18661615870344));
#174510=CARTESIAN_POINT('Ctrl Pts',(16.9579652679746,-17.7998578513191,
7.18622961375325));
#174511=CARTESIAN_POINT('Ctrl Pts',(16.9511894724408,-17.8103730650232,
7.18548080646452));
#174512=CARTESIAN_POINT('Ctrl Pts',(16.947941622299,-17.8154609966607,7.18511866932175));
#174513=CARTESIAN_POINT('Ctrl Pts',(16.9402801559074,-17.8275770391311,
7.18425670132761));
#174514=CARTESIAN_POINT('Ctrl Pts',(16.9358860442713,-17.8346173112282,
7.18375615460599));
#174515=CARTESIAN_POINT('Ctrl Pts',(16.9204543816215,-17.8596687687294,
7.18197605638755));
#174516=CARTESIAN_POINT('Ctrl Pts',(16.9096454223261,-17.8778186592026,
7.1806881747611));
#174517=CARTESIAN_POINT('Ctrl Pts',(16.8384380928337,-18.0015623051455,
7.17191696790891));
#174518=CARTESIAN_POINT('Ctrl Pts',(16.7870403110365,-18.1119034699418,
7.16412181699196));
#174519=CARTESIAN_POINT('Ctrl Pts',(16.7454193236514,-18.2258898887546,
7.15616137122351));
#174520=CARTESIAN_POINT('',(16.620190946188,-18.9524614545077,7.68893946617128));
#174521=CARTESIAN_POINT('Ctrl Pts',(16.6203930087273,-18.9524685809736,
7.68905589348695));
#174522=CARTESIAN_POINT('Ctrl Pts',(16.6197601590257,-19.2779557757106,
7.66955339595332));
#174523=CARTESIAN_POINT('Ctrl Pts',(16.8436653962077,-20.3101166792811,
7.60765896285921));
#174524=CARTESIAN_POINT('Ctrl Pts',(18.4531255376191,-21.4394563861295,
7.50337259420462));
#174525=CARTESIAN_POINT('Ctrl Pts',(20.673525152946,-20.5345839369853,7.3761967875232));
#174526=CARTESIAN_POINT('Ctrl Pts',(21.1145308209525,-18.1777889518937,
7.24902098084176));
#174527=CARTESIAN_POINT('Ctrl Pts',(19.371547213141,-16.5312845504829,7.12184517416032));
#174528=CARTESIAN_POINT('Ctrl Pts',(17.4471161563804,-17.0060916441732,
7.01671104281645));
#174529=CARTESIAN_POINT('Ctrl Pts',(16.8648290660527,-17.9078853718336,
6.95396884703307));
#174530=CARTESIAN_POINT('Ctrl Pts',(16.7486737197731,-18.2270709325543,
6.93361858681016));
#174531=CARTESIAN_POINT('Ctrl Pts',(16.6170000287534,-18.9523489152706,
7.68710087722452));
#174532=CARTESIAN_POINT('Ctrl Pts',(16.6169985639086,-18.9434611516821,
7.68762144269225));
#174533=CARTESIAN_POINT('Ctrl Pts',(16.6170530690849,-18.9345735467869,
7.68814369652498));
#174534=CARTESIAN_POINT('Ctrl Pts',(16.617270741598,-18.9170624098664,7.6891761672149));
#174535=CARTESIAN_POINT('Ctrl Pts',(16.6174306467703,-18.9084390286407,
7.68968627225728));
#174536=CARTESIAN_POINT('Ctrl Pts',(16.6177963854143,-18.8936059821696,
7.69056666148997));
#174537=CARTESIAN_POINT('Ctrl Pts',(16.6179768690861,-18.8873957595661,
7.69093615093166));
#174538=CARTESIAN_POINT('Ctrl Pts',(16.6183911393856,-18.8750179065797,
7.69167441356522));
#174539=CARTESIAN_POINT('Ctrl Pts',(16.6186245666237,-18.8688503250775,
7.6920431719162));
#174540=CARTESIAN_POINT('Ctrl Pts',(16.6191442764769,-18.8565429565483,
7.69278085784545));
#174541=CARTESIAN_POINT('Ctrl Pts',(16.6194303341952,-18.8504032201223,
7.69314977482355));
#174542=CARTESIAN_POINT('Ctrl Pts',(16.6202771216525,-18.8337853709109,
7.6941507934745));
#174543=CARTESIAN_POINT('Ctrl Pts',(16.620889018733,-18.8233101417259,7.69478449461903));
#174544=CARTESIAN_POINT('Ctrl Pts',(16.6234852736034,-18.7838994956495,
7.69717905954279));
#174545=CARTESIAN_POINT('Ctrl Pts',(16.6259862430238,-18.7550023876169,
7.69895602655921));
#174546=CARTESIAN_POINT('Ctrl Pts',(16.6474328530892,-18.555105247614,7.71140127744809));
#174547=CARTESIAN_POINT('Ctrl Pts',(16.6865510291809,-18.3871110626015,
7.72271575218188));
#174548=CARTESIAN_POINT('Ctrl Pts',(16.7454193803189,-18.2258897335605,
7.7340522080425));
#174549=CARTESIAN_POINT('Origin',(18.734,-18.952,0.));
#174550=CARTESIAN_POINT('',(16.7454192490578,-18.2258900930424,8.75434673926218));
#174551=CARTESIAN_POINT('',(16.74541940036,-18.2258896786745,8.53521106622902));
#174552=CARTESIAN_POINT('',(16.7454193692319,-18.2258897639242,0.));
#174553=CARTESIAN_POINT('Ctrl Pts',(16.7454192490578,-18.2258900930424,
8.75434673926218));
#174554=CARTESIAN_POINT('Ctrl Pts',(16.7157810160982,-18.3070596501447,
8.74958602597419));
#174555=CARTESIAN_POINT('Ctrl Pts',(16.6911130922396,-18.3900421657471,
8.74492440772906));
#174556=CARTESIAN_POINT('Ctrl Pts',(16.6409703506581,-18.6065647959986,
8.73282224506912));
#174557=CARTESIAN_POINT('Ctrl Pts',(16.6231411488845,-18.741366281552,8.72532552821618));
#174558=CARTESIAN_POINT('Ctrl Pts',(16.6177334387486,-18.8937846281362,
8.71640095673513));
#174559=CARTESIAN_POINT('Ctrl Pts',(16.6173369769236,-18.9106380599995,
8.7154084548658));
#174560=CARTESIAN_POINT('Ctrl Pts',(16.6170471059385,-18.935677546351,8.71392476474412));
#174561=CARTESIAN_POINT('Ctrl Pts',(16.6169998255506,-18.9438614082098,
8.71343839415166));
#174562=CARTESIAN_POINT('Ctrl Pts',(16.6170001372493,-18.9584435198302,
8.71256912102238));
#174563=CARTESIAN_POINT('Ctrl Pts',(16.6170292805039,-18.9648416993522,
8.71218680132263));
#174564=CARTESIAN_POINT('Ctrl Pts',(16.6171518843144,-18.9783316689556,
8.71137875762645));
#174565=CARTESIAN_POINT('Ctrl Pts',(16.6172519794822,-18.985423306241,8.71095283028561));
#174566=CARTESIAN_POINT('Ctrl Pts',(16.6176113756808,-19.0041994799665,
8.70982204028203));
#174567=CARTESIAN_POINT('Ctrl Pts',(16.6179318028016,-19.0158824786473,
8.7091152711121));
#174568=CARTESIAN_POINT('Ctrl Pts',(16.619877996158,-19.0703736724706,8.70580362709433));
#174569=CARTESIAN_POINT('Ctrl Pts',(16.6227060712927,-19.1131263516106,
8.7031613837008));
#174570=CARTESIAN_POINT('Ctrl Pts',(16.6340979487179,-19.2309338546192,
8.69575360055693));
#174571=CARTESIAN_POINT('Ctrl Pts',(16.645383694069,-19.3056561876156,8.69090978752918));
#174572=CARTESIAN_POINT('Ctrl Pts',(16.6865619595508,-19.5053184250742,
8.67762193844367));
#174573=CARTESIAN_POINT('Ctrl Pts',(16.7238652491619,-19.6284024291809,
8.66904373553352));
#174574=CARTESIAN_POINT('Ctrl Pts',(16.7783254108682,-19.7627415339463,
8.65959210382905));
#174575=CARTESIAN_POINT('Ctrl Pts',(16.7847472716301,-19.7780621979819,
8.65851318248265));
#174576=CARTESIAN_POINT('Ctrl Pts',(16.8125068973829,-19.8421616690798,
8.65399898355628));
#174577=CARTESIAN_POINT('Ctrl Pts',(16.8355023896456,-19.8902064779321,
8.65061472602623));
#174578=CARTESIAN_POINT('Ctrl Pts',(16.8643428448303,-19.9450493699819,
8.64679237499746));
#174579=CARTESIAN_POINT('Ctrl Pts',(16.8684462246156,-19.9527367517207,
8.64625755796771));
#174580=CARTESIAN_POINT('Ctrl Pts',(16.8747318708117,-19.9643394245033,
8.64545207073187));
#174581=CARTESIAN_POINT('Ctrl Pts',(16.8768792398725,-19.9682733735453,
8.64517926733447));
#174582=CARTESIAN_POINT('Ctrl Pts',(16.8807565447678,-19.9753232121195,
8.64469097276679));
#174583=CARTESIAN_POINT('Ctrl Pts',(16.8824818622009,-19.9784415652183,
8.64447519392715));
#174584=CARTESIAN_POINT('Ctrl Pts',(16.8862483303803,-19.9852087139538,
8.64400738909291));
#174585=CARTESIAN_POINT('Ctrl Pts',(16.888292411181,-19.9888558127542,8.64375555448036));
#174586=CARTESIAN_POINT('Ctrl Pts',(16.8940655242946,-19.9990851713286,
8.64304994399046));
#174587=CARTESIAN_POINT('Ctrl Pts',(16.8978190974434,-20.0056536090705,
8.64259771630789));
#174588=CARTESIAN_POINT('Ctrl Pts',(16.9204917409967,-20.0448397054969,
8.63990408704711));
#174589=CARTESIAN_POINT('Ctrl Pts',(16.9402455788541,-20.0769694662312,
8.63771329709888));
#174590=CARTESIAN_POINT('Ctrl Pts',(17.0081344025204,-20.1810518571699,
8.63061758543766));
#174591=CARTESIAN_POINT('Ctrl Pts',(17.0598256572541,-20.250585063833,8.62587708537816));
#174592=CARTESIAN_POINT('Ctrl Pts',(17.2291736386244,-20.4514018409526,
8.61158243682669));
#174593=CARTESIAN_POINT('Ctrl Pts',(17.3590568528564,-20.5713310132791,
8.60211687602608));
#174594=CARTESIAN_POINT('Ctrl Pts',(17.5209474976524,-20.6871423988481,
8.59054985572336));
#174595=CARTESIAN_POINT('Ctrl Pts',(17.5398251033512,-20.7001881401564,
8.58920551242383));
#174596=CARTESIAN_POINT('Ctrl Pts',(17.5668448400371,-20.7182187916646,
8.58728582490246));
#174597=CARTESIAN_POINT('Ctrl Pts',(17.5748147687717,-20.7234597321511,
8.58672012596513));
#174598=CARTESIAN_POINT('Ctrl Pts',(17.5878261733346,-20.7318904871905,
8.5857973509874));
#174599=CARTESIAN_POINT('Ctrl Pts',(17.5928462491103,-20.7351132053329,
8.58544150799897));
#174600=CARTESIAN_POINT('Ctrl Pts',(17.6033863050286,-20.7418168228078,
8.58469473570081));
#174601=CARTESIAN_POINT('Ctrl Pts',(17.608908885671,-20.7452934978525,8.58430365480356));
#174602=CARTESIAN_POINT('Ctrl Pts',(17.6220914693385,-20.7535075735396,
8.58337055818764));
#174603=CARTESIAN_POINT('Ctrl Pts',(17.629765756773,-20.7582217057285,8.58282769275946));
#174604=CARTESIAN_POINT('Ctrl Pts',(17.6557517539132,-20.7739567769158,
8.58099048444875));
#174605=CARTESIAN_POINT('Ctrl Pts',(17.6741997456372,-20.7847490677745,
8.57968785099279));
#174606=CARTESIAN_POINT('Ctrl Pts',(17.7757283767702,-20.8420990125517,
8.57252537896947));
#174607=CARTESIAN_POINT('Ctrl Pts',(17.8617042598789,-20.883283172637,8.56647650732707));
#174608=CARTESIAN_POINT('Ctrl Pts',(18.1086077821844,-20.981697404587,8.5492049106827));
#174609=CARTESIAN_POINT('Ctrl Pts',(18.2741076234026,-21.0254712030293,
8.53769532032363));
#174610=CARTESIAN_POINT('Ctrl Pts',(18.4795036363772,-21.0539691283966,
8.52446036907041));
#174611=CARTESIAN_POINT('Ctrl Pts',(18.5160742971354,-21.0580748754707,
8.52214606145962));
#174612=CARTESIAN_POINT('Ctrl Pts',(18.5598516626819,-21.061837047248,8.51944030043692));
#174613=CARTESIAN_POINT('Ctrl Pts',(18.5669706811736,-21.0624125708737,
8.51900232918123));
#174614=CARTESIAN_POINT('Ctrl Pts',(18.5785920842403,-21.0632929075178,
8.51829083659204));
#174615=CARTESIAN_POINT('Ctrl Pts',(18.5830927043418,-21.0636193668852,
8.51801614566152));
#174616=CARTESIAN_POINT('Ctrl Pts',(18.5911518109754,-21.0641780490793,
8.51752582701449));
#174617=CARTESIAN_POINT('Ctrl Pts',(18.594709859013,-21.0644156724828,8.51730990110314));
#174618=CARTESIAN_POINT('Ctrl Pts',(18.6024178398849,-21.0649108884691,
8.51684331964734));
#174619=CARTESIAN_POINT('Ctrl Pts',(18.6065679231275,-21.0651652452988,
8.51659284717148));
#174620=CARTESIAN_POINT('Ctrl Pts',(18.6181655874626,-21.0658417709624,
8.51589489080486));
#174621=CARTESIAN_POINT('Ctrl Pts',(18.6256147748996,-21.066236810419,8.51544890158573));
#174622=CARTESIAN_POINT('Ctrl Pts',(18.6689430807067,-21.0683049622748,
8.51286741728908));
#174623=CARTESIAN_POINT('Ctrl Pts',(18.7048603489582,-21.0691042304372,
8.51077775520912));
#174624=CARTESIAN_POINT('Ctrl Pts',(18.8205143230973,-21.0687336723076,
8.50416145657084));
#174625=CARTESIAN_POINT('Ctrl Pts',(18.9001742030535,-21.0639740260526,
8.49977486958345));
#174626=CARTESIAN_POINT('Ctrl Pts',(19.1643321808389,-21.033147756535,8.48527488305165));
#174627=CARTESIAN_POINT('Ctrl Pts',(19.3456060267506,-20.987262607043,8.47531870978353));
#174628=CARTESIAN_POINT('Ctrl Pts',(19.5390171582457,-20.9100915444266,
8.46320679728048));
#174629=CARTESIAN_POINT('Ctrl Pts',(19.5593659222989,-20.9016015392574,
8.46191427218898));
#174630=CARTESIAN_POINT('Ctrl Pts',(19.5873242460484,-20.8894204832188,
8.46011152219675));
#174631=CARTESIAN_POINT('Ctrl Pts',(19.5950503025094,-20.8859991652254,
8.45961047622032));
#174632=CARTESIAN_POINT('Ctrl Pts',(19.6082960307969,-20.880038475588,8.45874643662393));
#174633=CARTESIAN_POINT('Ctrl Pts',(19.6138256722399,-20.8775214094106,
8.45838421117874));
#174634=CARTESIAN_POINT('Ctrl Pts',(19.6252035963097,-20.8722829889565,
8.45763571584839));
#174635=CARTESIAN_POINT('Ctrl Pts',(19.631050423789,-20.8695586414769,8.45724934557353));
#174636=CARTESIAN_POINT('Ctrl Pts',(19.6446285239896,-20.8631561924117,
8.45634798178006));
#174637=CARTESIAN_POINT('Ctrl Pts',(19.6523500760168,-20.8594578461956,
8.45583229000792));
#174638=CARTESIAN_POINT('Ctrl Pts',(19.6769969751317,-20.8474685200703,
8.454176124448));
#174639=CARTESIAN_POINT('Ctrl Pts',(19.6938337578429,-20.8389984968026,
8.45302942603647));
#174640=CARTESIAN_POINT('Ctrl Pts',(19.7773927470935,-20.795555109936,8.44725982575586));
#174641=CARTESIAN_POINT('Ctrl Pts',(19.8423209852681,-20.7572662662378,
8.44252053346244));
#174642=CARTESIAN_POINT('Ctrl Pts',(19.9960070390426,-20.6552158438107,
8.43066518235256));
#174643=CARTESIAN_POINT('Ctrl Pts',(20.0821353815349,-20.5878892072224,
8.42344928725966));
#174644=CARTESIAN_POINT('Ctrl Pts',(20.173122420313,-20.504680215372,8.41530416857833));
#174645=CARTESIAN_POINT('Ctrl Pts',(20.1834675881393,-20.4950271889208,
8.41436997166442));
#174646=CARTESIAN_POINT('Ctrl Pts',(20.269508973462,-20.4131134830144,8.40653561155425));
#174647=CARTESIAN_POINT('Ctrl Pts',(20.3398574719983,-20.3354259662255,
8.39969810472665));
#174648=CARTESIAN_POINT('Ctrl Pts',(20.4101290099512,-20.2452031417365,
8.39263251411188));
#174649=CARTESIAN_POINT('Ctrl Pts',(20.4160285993265,-20.2375203705226,
8.39203736458283));
#174650=CARTESIAN_POINT('Ctrl Pts',(20.4246626345543,-20.2261154501457,
8.39116377634351));
#174651=CARTESIAN_POINT('Ctrl Pts',(20.4274378694937,-20.2224245382058,
8.39088257730593));
#174652=CARTESIAN_POINT('Ctrl Pts',(20.4323404553899,-20.2158597555363,
8.39038515391424));
#174653=CARTESIAN_POINT('Ctrl Pts',(20.4344726226762,-20.2129895496339,
8.39016859523483));
#174654=CARTESIAN_POINT('Ctrl Pts',(20.4390258794515,-20.2068276560915,
8.38970565670783));
#174655=CARTESIAN_POINT('Ctrl Pts',(20.4414447069695,-20.2035343660414,
8.38945943343401));
#174656=CARTESIAN_POINT('Ctrl Pts',(20.448059518757,-20.194473275021,8.38878520297246));
#174657=CARTESIAN_POINT('Ctrl Pts',(20.4522359574534,-20.1886911784249,
8.38835852996528));
#174658=CARTESIAN_POINT('Ctrl Pts',(20.4743977322523,-20.1576801782317,
8.38608852389913));
#174659=CARTESIAN_POINT('Ctrl Pts',(20.4918578235873,-20.1320784122042,
8.38427905887846));
#174660=CARTESIAN_POINT('Ctrl Pts',(20.5979099846711,-19.9689937939593,
8.37309021314127));
#174661=CARTESIAN_POINT('Ctrl Pts',(20.6708907465366,-19.822001949655,8.3644462344041));
#174662=CARTESIAN_POINT('Ctrl Pts',(20.7660349872544,-19.5572910783922,
8.34905144674781));
#174663=CARTESIAN_POINT('Ctrl Pts',(20.7965356025286,-19.4434112557633,
8.34248333727952));
#174664=CARTESIAN_POINT('Ctrl Pts',(20.8199519372763,-19.3135218283323,
8.33475142543334));
#174665=CARTESIAN_POINT('Ctrl Pts',(20.8223464710435,-19.2994226804983,
8.33390927611133));
#174666=CARTESIAN_POINT('Ctrl Pts',(20.8259295438054,-19.2769481804365,
8.33256186165773));
#174667=CARTESIAN_POINT('Ctrl Pts',(20.8272110756077,-19.2685879435499,
8.33205954349965));
#174668=CARTESIAN_POINT('Ctrl Pts',(20.8293826061142,-19.2538317932811,
8.33117091255808));
#174669=CARTESIAN_POINT('Ctrl Pts',(20.8302935087911,-19.2474390309615,
8.33078526685305));
#174670=CARTESIAN_POINT('Ctrl Pts',(20.8321168000064,-19.2342099582484,
8.32998579914036));
#174671=CARTESIAN_POINT('Ctrl Pts',(20.8330250559964,-19.2273731641823,
8.32957185131814));
#174672=CARTESIAN_POINT('Ctrl Pts',(20.8352701963922,-19.2098163441194,
8.32850677519392));
#174673=CARTESIAN_POINT('Ctrl Pts',(20.8365584494455,-19.1990903993113,
8.32785411979507));
#174674=CARTESIAN_POINT('Ctrl Pts',(20.8415891532997,-19.1543128121803,
8.32512097083759));
#174675=CARTESIAN_POINT('Ctrl Pts',(20.8445867308715,-19.1201842714433,
8.32301720800361));
#174676=CARTESIAN_POINT('Ctrl Pts',(20.8502360494753,-19.0311121246598,
8.31746979021053));
#174677=CARTESIAN_POINT('Ctrl Pts',(20.851576785722,-18.9761140106063,8.3139878713536));
#174678=CARTESIAN_POINT('Ctrl Pts',(20.8491809905767,-18.8118350162185,
8.30342826234796));
#174679=CARTESIAN_POINT('Ctrl Pts',(20.8391247986837,-18.7028354774673,
8.2962021486675));
#174680=CARTESIAN_POINT('Ctrl Pts',(20.8141516884167,-18.5568204474596,
8.28641655421683));
#174681=CARTESIAN_POINT('Ctrl Pts',(20.8065503686207,-18.5187183361101,
8.28385447449473));
#174682=CARTESIAN_POINT('Ctrl Pts',(20.7915455180272,-18.4529890664879,
8.27943831844381));
#174683=CARTESIAN_POINT('Ctrl Pts',(20.7846226373766,-18.425262527147,8.27757664320697));
#174684=CARTESIAN_POINT('Ctrl Pts',(20.7634343267692,-18.3471650462427,
8.27235015105871));
#174685=CARTESIAN_POINT('Ctrl Pts',(20.7478579873175,-18.2971671965401,
8.26902454029946));
#174686=CARTESIAN_POINT('Ctrl Pts',(20.7275521347833,-18.2395995564061,
8.26525910813474));
#174687=CARTESIAN_POINT('Ctrl Pts',(20.724611172247,-18.2314226807587,8.26472580091698));
#174688=CARTESIAN_POINT('Ctrl Pts',(20.7200789161847,-18.2190609995525,
8.26392213281046));
#174689=CARTESIAN_POINT('Ctrl Pts',(20.7185245998338,-18.2148628667633,
8.26364965281869));
#174690=CARTESIAN_POINT('Ctrl Pts',(20.7157091024435,-18.2073317975665,
8.26316170322544));
#174691=CARTESIAN_POINT('Ctrl Pts',(20.7144528180605,-18.2039971026539,
8.26294594776046));
#174692=CARTESIAN_POINT('Ctrl Pts',(20.7117028615495,-18.1967530837837,
8.26247792499275));
#174693=CARTESIAN_POINT('Ctrl Pts',(20.7102060208389,-18.1928450244311,
8.26222585052816));
#174694=CARTESIAN_POINT('Ctrl Pts',(20.7059640713711,-18.1818674045298,
8.26151888954884));
#174695=CARTESIAN_POINT('Ctrl Pts',(20.7031925171357,-18.1748080367215,
8.26106556076175));
#174696=CARTESIAN_POINT('Ctrl Pts',(20.6862933924865,-18.1324354155725,
8.25835147320396));
#174697=CARTESIAN_POINT('Ctrl Pts',(20.6712532371401,-18.0974908431281,
8.25614222485884));
#174698=CARTESIAN_POINT('Ctrl Pts',(20.618387017022,-17.9832421357649,8.24895634796574));
#174699=CARTESIAN_POINT('Ctrl Pts',(20.5765656166621,-17.905883073821,8.24414894956654));
#174700=CARTESIAN_POINT('Ctrl Pts',(20.4377981800777,-17.6834835102052,
8.22988831967376));
#174701=CARTESIAN_POINT('Ctrl Pts',(20.3276493221905,-17.5476006951211,
8.22051299753978));
#174702=CARTESIAN_POINT('Ctrl Pts',(20.1854714729081,-17.4107497918513,
8.20904691332124));
#174703=CARTESIAN_POINT('Ctrl Pts',(20.1685835225989,-17.3950184022049,
8.20769489533522));
#174704=CARTESIAN_POINT('Ctrl Pts',(20.1443409473992,-17.3731653609786,
8.20576612629853));
#174705=CARTESIAN_POINT('Ctrl Pts',(20.1371964692755,-17.3668122920801,
8.20519914683374));
#174706=CARTESIAN_POINT('Ctrl Pts',(20.1255216297847,-17.3565714718254,
8.20427485361015));
#174707=CARTESIAN_POINT('Ctrl Pts',(20.1210173752236,-17.3526540604435,
8.20391878111463));
#174708=CARTESIAN_POINT('Ctrl Pts',(20.1115571240338,-17.3444963727913,
8.20317199165996));
#174709=CARTESIAN_POINT('Ctrl Pts',(20.1065979860016,-17.3402598507168,
8.20278112516494));
#174710=CARTESIAN_POINT('Ctrl Pts',(20.0947589921745,-17.3302402331746,
8.2018493971262));
#174711=CARTESIAN_POINT('Ctrl Pts',(20.0878617723182,-17.3244779345155,
8.20130769244963));
#174712=CARTESIAN_POINT('Ctrl Pts',(20.0645262536377,-17.3052332043154,
8.19947848690033));
#174713=CARTESIAN_POINT('Ctrl Pts',(20.0479220171919,-17.2919548584491,
8.19818279334596));
#174714=CARTESIAN_POINT('Ctrl Pts',(19.9114075633507,-17.1861160763221,
8.1875737599483));
#174715=CARTESIAN_POINT('Ctrl Pts',(19.7821003146753,-17.1064365206708,
8.17774705098268));
#174716=CARTESIAN_POINT('Ctrl Pts',(19.5191246388494,-16.9809977040795,
8.15851560158897));
#174717=CARTESIAN_POINT('Ctrl Pts',(19.3871506701713,-16.9334184897505,
8.14919461729016));
#174718=CARTESIAN_POINT('Ctrl Pts',(19.23644457044,-16.8954306371134,8.13950223934659));
#174719=CARTESIAN_POINT('Ctrl Pts',(19.2214095381892,-16.891815526537,8.13854575362525));
#174720=CARTESIAN_POINT('Ctrl Pts',(19.2007251342864,-16.8870811693372,
8.13724545788543));
#174721=CARTESIAN_POINT('Ctrl Pts',(19.1951092245429,-16.8858198498143,
8.13689399154264));
#174722=CARTESIAN_POINT('Ctrl Pts',(19.1861635909178,-16.8838489715824,
8.13633671070011));
#174723=CARTESIAN_POINT('Ctrl Pts',(19.1828372269972,-16.8831245244486,
8.13613005524956));
#174724=CARTESIAN_POINT('Ctrl Pts',(19.1759522425594,-16.8816424335891,
8.13570350426253));
#174725=CARTESIAN_POINT('Ctrl Pts',(19.1723934130695,-16.8808859391544,
8.13548368062842));
#174726=CARTESIAN_POINT('Ctrl Pts',(19.1638900632026,-16.8791012956302,
8.13495998133655));
#174727=CARTESIAN_POINT('Ctrl Pts',(19.1589437408244,-16.8780816497858,
8.13465659087138));
#174728=CARTESIAN_POINT('Ctrl Pts',(19.1421626701402,-16.8746849193374,
8.13363135550849));
#174729=CARTESIAN_POINT('Ctrl Pts',(19.1303110049797,-16.8723913079019,
8.13291411399844));
#174730=CARTESIAN_POINT('Ctrl Pts',(19.1017333270388,-16.86711395191,8.13119965966214));
#174731=CARTESIAN_POINT('Ctrl Pts',(19.0849895158324,-16.8642298904186,
8.13020748512273));
#174732=CARTESIAN_POINT('Ctrl Pts',(19.0217244606241,-16.8541153536498,
8.12649892941144));
#174733=CARTESIAN_POINT('Ctrl Pts',(18.9749985768257,-16.8482353714438,
8.12384163635732));
#174734=CARTESIAN_POINT('Ctrl Pts',(18.7632271502125,-16.8287354086484,
8.11201370457759));
#174735=CARTESIAN_POINT('Ctrl Pts',(18.5971284965,-16.8329489394972,8.10327870512878));
#174736=CARTESIAN_POINT('Ctrl Pts',(18.4027335682835,-16.8608520798403,
8.09232662014656));
#174737=CARTESIAN_POINT('Ctrl Pts',(18.3723551781013,-16.86589118554,8.09059532991768));
#174738=CARTESIAN_POINT('Ctrl Pts',(18.2937323065434,-16.8807019426397,
8.08605037475608));
#174739=CARTESIAN_POINT('Ctrl Pts',(18.2457018107127,-16.8914962726911,
8.08321018944067));
#174740=CARTESIAN_POINT('Ctrl Pts',(18.1858482775165,-16.9071579758446,
8.07957177276679));
#174741=CARTESIAN_POINT('Ctrl Pts',(18.1736321517393,-16.9104718765634,
8.07882394229243));
#174742=CARTESIAN_POINT('Ctrl Pts',(18.1543405001009,-16.915891371491,8.07763438708182));
#174743=CARTESIAN_POINT('Ctrl Pts',(18.1472448854976,-16.9179248007014,
8.07719501152915));
#174744=CARTESIAN_POINT('Ctrl Pts',(18.1340548380325,-16.9217795044507,
8.07637475104678));
#174745=CARTESIAN_POINT('Ctrl Pts',(18.1279576822433,-16.9235912232399,
8.07599418210902));
#174746=CARTESIAN_POINT('Ctrl Pts',(18.1144478245515,-16.9276719144909,
8.07514778032247));
#174747=CARTESIAN_POINT('Ctrl Pts',(18.1070392608751,-16.9299541733713,
8.07468151631386));
#174748=CARTESIAN_POINT('Ctrl Pts',(18.0855918511831,-16.9366903964074,
8.07332548491994));
#174749=CARTESIAN_POINT('Ctrl Pts',(18.0715869542553,-16.9412501733404,
8.07243225241572));
#174750=CARTESIAN_POINT('Ctrl Pts',(17.9873784937238,-16.9696423609099,
8.06701348595055));
#174751=CARTESIAN_POINT('Ctrl Pts',(17.9184263739569,-16.9970005007686,
8.06237164937812));
#174752=CARTESIAN_POINT('Ctrl Pts',(17.7205270314199,-17.0878145250312,
8.04843614210774));
#174753=CARTESIAN_POINT('Ctrl Pts',(17.5964399298002,-17.1608371091457,
8.0388698710998));
#174754=CARTESIAN_POINT('Ctrl Pts',(17.4064916748834,-17.3003667216467,
8.02337001411286));
#174755=CARTESIAN_POINT('Ctrl Pts',(17.3358956587051,-17.3596812259989,
8.01738979410201));
#174756=CARTESIAN_POINT('Ctrl Pts',(17.2623997116989,-17.4301014891053,
8.01110119090848));
#174757=CARTESIAN_POINT('Ctrl Pts',(17.2554640631812,-17.4368386298259,
8.01050712697695));
#174758=CARTESIAN_POINT('Ctrl Pts',(17.2452868616776,-17.4468609749741,
8.00963482222536));
#174759=CARTESIAN_POINT('Ctrl Pts',(17.2420096152402,-17.4501095294314,
8.00935383252509));
#174760=CARTESIAN_POINT('Ctrl Pts',(17.2362121345813,-17.4558939570463,
8.00885664041529));
#174761=CARTESIAN_POINT('Ctrl Pts',(17.2336876790408,-17.4584255218394,
8.00864010483995));
#174762=CARTESIAN_POINT('Ctrl Pts',(17.2282901889713,-17.463865705465,8.00817706177173));
#174763=CARTESIAN_POINT('Ctrl Pts',(17.2254191711242,-17.466776246824,8.00793071165759));
#174764=CARTESIAN_POINT('Ctrl Pts',(17.2195440036225,-17.4727669059542,
8.00742643931674));
#174765=CARTESIAN_POINT('Ctrl Pts',(17.216540774211,-17.4758479040816,8.00716858826537));
#174766=CARTESIAN_POINT('Ctrl Pts',(17.20275671955,-17.49007541738,8.00598462437137));
#174767=CARTESIAN_POINT('Ctrl Pts',(17.1920888537718,-17.5013313549203,
8.00506692452257));
#174768=CARTESIAN_POINT('Ctrl Pts',(17.1269831423748,-17.5715557275963,
7.99944984538999));
#174769=CARTESIAN_POINT('Ctrl Pts',(17.0758055800885,-17.6334691607406,
7.99496142150964));
#174770=CARTESIAN_POINT('Ctrl Pts',(16.9870647272263,-17.7541917324801,
7.98672447870772));
#174771=CARTESIAN_POINT('Ctrl Pts',(16.9486527687872,-17.8122354844151,
7.98296209881663));
#174772=CARTESIAN_POINT('Ctrl Pts',(16.8464128603342,-17.9846179973398,
7.97206948302796));
#174773=CARTESIAN_POINT('Ctrl Pts',(16.7902668398971,-18.1030670588315,
7.96490115903004));
#174774=CARTESIAN_POINT('Ctrl Pts',(16.7454193380512,-18.2258898493182,
7.95734463868439));
#174775=CARTESIAN_POINT('Ctrl Pts',(16.7454193803189,-18.2258897335605,
7.7340522080425));
#174776=CARTESIAN_POINT('Ctrl Pts',(16.7619322267477,-18.1806664005465,
7.73723213666382));
#174777=CARTESIAN_POINT('Ctrl Pts',(16.779998976002,-18.1359755434987,7.74040817555081));
#174778=CARTESIAN_POINT('Ctrl Pts',(16.8255358480881,-18.0335613432304,
7.74771677785878));
#174779=CARTESIAN_POINT('Ctrl Pts',(16.8541026592798,-17.9764219531316,
7.75181782248633));
#174780=CARTESIAN_POINT('Ctrl Pts',(16.8915487563,-17.9092959968522,7.75659240664854));
#174781=CARTESIAN_POINT('Ctrl Pts',(16.8979909436681,-17.8979938387207,
7.75739475456953));
#174782=CARTESIAN_POINT('Ctrl Pts',(16.9071560003972,-17.8822537265884,
7.7585091882223));
#174783=CARTESIAN_POINT('Ctrl Pts',(16.9097915255555,-17.8777656068379,
7.75882661551778));
#174784=CARTESIAN_POINT('Ctrl Pts',(16.9143119584172,-17.8701322280941,
7.75936585096772));
#174785=CARTESIAN_POINT('Ctrl Pts',(16.9161885259259,-17.8669820784768,
7.75958819498853));
#174786=CARTESIAN_POINT('Ctrl Pts',(16.9198038258629,-17.8609488662358,
7.76001364754557));
#174787=CARTESIAN_POINT('Ctrl Pts',(16.9215412559203,-17.8580650676948,
7.76021684147643));
#174788=CARTESIAN_POINT('Ctrl Pts',(16.9261670066246,-17.85042848667,7.76075450913471));
#174789=CARTESIAN_POINT('Ctrl Pts',(16.929067212396,-17.8456828823784,7.76108820995248));
#174790=CARTESIAN_POINT('Ctrl Pts',(16.9394508641136,-17.8288416397558,
7.76227114815962));
#174791=CARTESIAN_POINT('Ctrl Pts',(16.9470376561362,-17.8168097474834,
7.7631138752276));
#174792=CARTESIAN_POINT('Ctrl Pts',(17.0551881142097,-17.649065318899,7.77484241498185));
#174793=CARTESIAN_POINT('Ctrl Pts',(17.1756723125731,-17.5071175146947,
7.78457133713022));
#174794=CARTESIAN_POINT('Ctrl Pts',(17.3915911146781,-17.3116247103171,
7.80052204703916));
#174795=CARTESIAN_POINT('Ctrl Pts',(17.475264179863,-17.2465754267534,7.80642246470033));
#174796=CARTESIAN_POINT('Ctrl Pts',(17.5762508346356,-17.1795604063647,
7.81347122822371));
#174797=CARTESIAN_POINT('Ctrl Pts',(17.5891496151711,-17.1712016337461,
7.81437005807411));
#174798=CARTESIAN_POINT('Ctrl Pts',(17.6099153271888,-17.1580637285884,
7.81581532395711));
#174799=CARTESIAN_POINT('Ctrl Pts',(17.6177245335891,-17.1531940692189,
7.81635844164296));
#174800=CARTESIAN_POINT('Ctrl Pts',(17.6326611028114,-17.1440146562094,
7.81739664682125));
#174801=CARTESIAN_POINT('Ctrl Pts',(17.6397826475457,-17.1396957340488,
7.8178913874317));
#174802=CARTESIAN_POINT('Ctrl Pts',(17.6523561103436,-17.1321715765748,
7.81876450383632));
#174803=CARTESIAN_POINT('Ctrl Pts',(17.6577972825859,-17.1289485184373,
7.8191422230715));
#174804=CARTESIAN_POINT('Ctrl Pts',(17.6684890635192,-17.1226798288853,
7.81988423028138));
#174805=CARTESIAN_POINT('Ctrl Pts',(17.6737384940372,-17.1196323016415,
7.82024844459872));
#174806=CARTESIAN_POINT('Ctrl Pts',(17.6863080467173,-17.1124072171097,
7.82112035062422));
#174807=CARTESIAN_POINT('Ctrl Pts',(17.6936401107291,-17.1082507400902,
7.8216287970201));
#174808=CARTESIAN_POINT('Ctrl Pts',(17.7201258929756,-17.093444492107,7.82346504575633));
#174809=CARTESIAN_POINT('Ctrl Pts',(17.7394193751252,-17.0830487955071,
7.82480188044333));
#174810=CARTESIAN_POINT('Ctrl Pts',(17.9252216831591,-16.9866267596963,
7.83767285470048));
#174811=CARTESIAN_POINT('Ctrl Pts',(18.1022711915946,-16.9227871890543,
7.85002447788917));
#174812=CARTESIAN_POINT('Ctrl Pts',(18.362532564999,-16.8663497467016,7.86760356587159));
#174813=CARTESIAN_POINT('Ctrl Pts',(18.4405888349051,-16.8539445666954,
7.87278915021938));
#174814=CARTESIAN_POINT('Ctrl Pts',(18.5546862687292,-16.8423055161878,
7.88009811166932));
#174815=CARTESIAN_POINT('Ctrl Pts',(18.5903007764088,-16.8395807443077,
7.88234120915035));
#174816=CARTESIAN_POINT('Ctrl Pts',(18.6334065997711,-16.8373781844339,
7.88499652782441));
#174817=CARTESIAN_POINT('Ctrl Pts',(18.6408457924727,-16.8370374111,7.88545263849376));
#174818=CARTESIAN_POINT('Ctrl Pts',(18.6524384052315,-16.8365676633924,
7.88615990157103));
#174819=CARTESIAN_POINT('Ctrl Pts',(18.6565905836826,-16.8364116545375,
7.88641252567698));
#174820=CARTESIAN_POINT('Ctrl Pts',(18.6643073826521,-16.8361444620529,
7.88688069236927));
#174821=CARTESIAN_POINT('Ctrl Pts',(18.6678717904873,-16.8360300619921,
7.88709640717752));
#174822=CARTESIAN_POINT('Ctrl Pts',(18.6759507355909,-16.8357912015704,
7.88758414484032));
#174823=CARTESIAN_POINT('Ctrl Pts',(18.6804653808177,-16.8356721801511,
7.88785586045923));
#174824=CARTESIAN_POINT('Ctrl Pts',(18.6938518795006,-16.8353621298321,
7.88865913214287));
#174825=CARTESIAN_POINT('Ctrl Pts',(18.7027247184456,-16.8352124320093,
7.88918843209379));
#174826=CARTESIAN_POINT('Ctrl Pts',(18.7689738607688,-16.8345113601344,
7.89311886455338));
#174827=CARTESIAN_POINT('Ctrl Pts',(18.8263558471927,-16.8362370289468,
7.89640252499328));
#174828=CARTESIAN_POINT('Ctrl Pts',(18.9373969122156,-16.8441036246973,
7.90264250938221));
#174829=CARTESIAN_POINT('Ctrl Pts',(18.9910290967687,-16.8499690835869,
7.90560438632877));
#174830=CARTESIAN_POINT('Ctrl Pts',(19.1590174935583,-16.874867505714,7.91486773977388));
#174831=CARTESIAN_POINT('Ctrl Pts',(19.272061961036,-16.9012421038396,7.92109154937541));
#174832=CARTESIAN_POINT('Ctrl Pts',(19.4555541449726,-16.9602777650855,
7.93180169213588));
#174833=CARTESIAN_POINT('Ctrl Pts',(19.5273857443055,-16.9877863932878,
7.9361563097903));
#174834=CARTESIAN_POINT('Ctrl Pts',(19.6149542720312,-17.0269099726207,
7.94175497383186));
#174835=CARTESIAN_POINT('Ctrl Pts',(19.6322444966816,-17.0349165818859,
7.94287486320842));
#174836=CARTESIAN_POINT('Ctrl Pts',(19.6571777634614,-17.0468738185945,
7.94451186082426));
#174837=CARTESIAN_POINT('Ctrl Pts',(19.6649088220748,-17.0506395103291,
7.94502256021687));
#174838=CARTESIAN_POINT('Ctrl Pts',(19.6784036865335,-17.0573147066109,
7.94591956771264));
#174839=CARTESIAN_POINT('Ctrl Pts',(19.6841775606311,-17.0602036880333,
7.94630515477249));
#174840=CARTESIAN_POINT('Ctrl Pts',(19.6953492316343,-17.0658575253039,
7.94705474327523));
#174841=CARTESIAN_POINT('Ctrl Pts',(19.7007485461323,-17.0686192558652,
7.94741863198299));
#174842=CARTESIAN_POINT('Ctrl Pts',(19.7136050897967,-17.0752651852286,
7.9482889880279));
#174843=CARTESIAN_POINT('Ctrl Pts',(19.7210511489608,-17.0791706636548,
7.94879620397142));
#174844=CARTESIAN_POINT('Ctrl Pts',(19.7477072312569,-17.0933549755273,
7.95062340435189));
#174845=CARTESIAN_POINT('Ctrl Pts',(19.7667810685412,-17.1038855862021,
7.9519523052246));
#174846=CARTESIAN_POINT('Ctrl Pts',(19.9494190141715,-17.2084298056783,
7.96488992636055));
#174847=CARTESIAN_POINT('Ctrl Pts',(20.0998578013824,-17.3236008205379,
7.97732859494697));
#174848=CARTESIAN_POINT('Ctrl Pts',(20.2882103200328,-17.5124763347102,
7.99493368496722));
#174849=CARTESIAN_POINT('Ctrl Pts',(20.340298153315,-17.5708388955554,8.00006424234782));
#174850=CARTESIAN_POINT('Ctrl Pts',(20.4111709102989,-17.6596973118171,
8.00730621820389));
#174851=CARTESIAN_POINT('Ctrl Pts',(20.4326005973129,-17.6879964974435,
8.00953510571154));
#174852=CARTESIAN_POINT('Ctrl Pts',(20.4576469260583,-17.7228598422889,
8.01217592008974));
#174853=CARTESIAN_POINT('Ctrl Pts',(20.4619521441968,-17.7289196084709,
8.01263118941461));
#174854=CARTESIAN_POINT('Ctrl Pts',(20.4686123393807,-17.7383994594772,
8.01333743474378));
#174855=CARTESIAN_POINT('Ctrl Pts',(20.4709892738495,-17.7418039402209,
8.01358987573566));
#174856=CARTESIAN_POINT('Ctrl Pts',(20.4753893193302,-17.7481457899185,
8.01405787710751));
#174857=CARTESIAN_POINT('Ctrl Pts',(20.4774150039841,-17.7510812497255,
8.01427360862288));
#174858=CARTESIAN_POINT('Ctrl Pts',(20.4819912336812,-17.7577487369091,
8.01476160568835));
#174859=CARTESIAN_POINT('Ctrl Pts',(20.4845372437389,-17.7614838129727,
8.01503356263084));
#174860=CARTESIAN_POINT('Ctrl Pts',(20.4920565838355,-17.7725911940076,
8.01583820945556));
#174861=CARTESIAN_POINT('Ctrl Pts',(20.4969955169397,-17.7799868187015,
8.01636863173673));
#174862=CARTESIAN_POINT('Ctrl Pts',(20.5337421013779,-17.8357695688771,
8.02033127904505));
#174863=CARTESIAN_POINT('Ctrl Pts',(20.5636021136094,-17.8854169582913,
8.02364384496398));
#174864=CARTESIAN_POINT('Ctrl Pts',(20.6709720017695,-18.081748845276,8.03618223822287));
#174865=CARTESIAN_POINT('Ctrl Pts',(20.7331795830118,-18.236119283212,8.04492057814872));
#174866=CARTESIAN_POINT('Ctrl Pts',(20.7976855332202,-18.4731881153562,
8.0585476936874));
#174867=CARTESIAN_POINT('Ctrl Pts',(20.8142664358205,-18.5513151337539,
8.06306155630676));
#174868=CARTESIAN_POINT('Ctrl Pts',(20.8293525981671,-18.6494036783684,
8.06885223255477));
#174869=CARTESIAN_POINT('Ctrl Pts',(20.8320432964963,-18.6686603923205,
8.06999469803572));
#174870=CARTESIAN_POINT('Ctrl Pts',(20.8355497042471,-18.6965533123941,
8.07165871287179));
#174871=CARTESIAN_POINT('Ctrl Pts',(20.8365782324318,-18.7051621124621,
8.07217354827358));
#174872=CARTESIAN_POINT('Ctrl Pts',(20.8382816334519,-18.7202034565729,
8.0730753600271));
#174873=CARTESIAN_POINT('Ctrl Pts',(20.8389799678123,-18.7266332675303,
8.07346159151261));
#174874=CARTESIAN_POINT('Ctrl Pts',(20.8402739886179,-18.7390788215124,
8.07421062968914));
#174875=CARTESIAN_POINT('Ctrl Pts',(20.8408733942546,-18.7450941209619,
8.0745733151487));
#174876=CARTESIAN_POINT('Ctrl Pts',(20.8422377982908,-18.7594076049884,
8.07543791860648));
#174877=CARTESIAN_POINT('Ctrl Pts',(20.8429795748212,-18.767707855188,8.07594056272967));
#174878=CARTESIAN_POINT('Ctrl Pts',(20.845445486719,-18.7972682303203,8.07773530678394));
#174879=CARTESIAN_POINT('Ctrl Pts',(20.8468972533344,-18.8185492280345,
8.07903591663865));
#174880=CARTESIAN_POINT('Ctrl Pts',(20.8582309521455,-19.0321854861355,
8.09218220035401));
#174881=CARTESIAN_POINT('Ctrl Pts',(20.8421358513437,-19.2249821324295,
8.1048984775538));
#174882=CARTESIAN_POINT('Ctrl Pts',(20.7837496616184,-19.4867327030221,
8.12259031213804));
#174883=CARTESIAN_POINT('Ctrl Pts',(20.763331094302,-19.5596426708577,8.12755035236347));
#174884=CARTESIAN_POINT('Ctrl Pts',(20.727886639083,-19.6642609590438,8.13458397055187));
#174885=CARTESIAN_POINT('Ctrl Pts',(20.7159104693788,-19.6969367889989,
8.13676813031065));
#174886=CARTESIAN_POINT('Ctrl Pts',(20.7004201116911,-19.7361782665043,
8.13936322713852));
#174887=CARTESIAN_POINT('Ctrl Pts',(20.6976707559909,-19.7430377836054,
8.13981580567058));
#174888=CARTESIAN_POINT('Ctrl Pts',(20.6933241716792,-19.7537199956716,
8.14051879525213));
#174889=CARTESIAN_POINT('Ctrl Pts',(20.6917515766215,-19.7575525594904,
8.14077064991461));
#174890=CARTESIAN_POINT('Ctrl Pts',(20.6888037283009,-19.7646771264926,
8.14123812476935));
#174891=CARTESIAN_POINT('Ctrl Pts',(20.6874314171975,-19.767970236387,8.14145391261085));
#174892=CARTESIAN_POINT('Ctrl Pts',(20.6842963624851,-19.7754401316373,
8.14194275317121));
#174893=CARTESIAN_POINT('Ctrl Pts',(20.6825285274285,-19.779614723521,8.14221549283492));
#174894=CARTESIAN_POINT('Ctrl Pts',(20.6772288581636,-19.792018329585,8.14302460758111));
#174895=CARTESIAN_POINT('Ctrl Pts',(20.673658155661,-19.8002307674279,8.14355867753926));
#174896=CARTESIAN_POINT('Ctrl Pts',(20.6458890944605,-19.8630058728969,
8.14763024012297));
#174897=CARTESIAN_POINT('Ctrl Pts',(20.6194426832431,-19.9165511277936,
8.15104051929581));
#174898=CARTESIAN_POINT('Ctrl Pts',(20.5139728921885,-20.109127048501,8.16332629922221));
#174899=CARTESIAN_POINT('Ctrl Pts',(20.42154249325,-20.2401974200527,8.17176668649212));
#174900=CARTESIAN_POINT('Ctrl Pts',(20.2747034011892,-20.4051474471537,
8.18399127114817));
#174901=CARTESIAN_POINT('Ctrl Pts',(20.2322291312334,-20.4489011702537,
8.18741377976112));
#174902=CARTESIAN_POINT('Ctrl Pts',(20.1611141954442,-20.516095588868,8.1930302633218));
#174903=CARTESIAN_POINT('Ctrl Pts',(20.1336433628314,-20.5407253230825,
8.19517466091691));
#174904=CARTESIAN_POINT('Ctrl Pts',(20.0970921595499,-20.5718122969972,
8.19800331523234));
#174905=CARTESIAN_POINT('Ctrl Pts',(20.0885838117698,-20.5789341728332,
8.1986600818738));
#174906=CARTESIAN_POINT('Ctrl Pts',(20.0746469565321,-20.5904148430398,
8.19973335037634));
#174907=CARTESIAN_POINT('Ctrl Pts',(20.0692521725673,-20.5948143820369,
8.20014819115289));
#174908=CARTESIAN_POINT('Ctrl Pts',(20.0588299209313,-20.6032286556426,
8.20094851183168));
#174909=CARTESIAN_POINT('Ctrl Pts',(20.0538056516013,-20.6072472423159,
8.20133383029686));
#174910=CARTESIAN_POINT('Ctrl Pts',(20.0422514520509,-20.6164026449629,
8.20221885494527));
#174911=CARTESIAN_POINT('Ctrl Pts',(20.035709475102,-20.6215240236994,8.20271916946415));
#174912=CARTESIAN_POINT('Ctrl Pts',(20.0182311539396,-20.6350417235495,
8.2040538829054));
#174913=CARTESIAN_POINT('Ctrl Pts',(20.007242780248,-20.6433698319372,8.20489095314936));
#174914=CARTESIAN_POINT('Ctrl Pts',(19.9216924994318,-20.7069024207235,
8.21139328751848));
#174915=CARTESIAN_POINT('Ctrl Pts',(19.8436657339346,-20.7572517580322,
8.21724511602407));
#174916=CARTESIAN_POINT('Ctrl Pts',(19.6063279225209,-20.8891886399429,
8.23479889722253));
#174917=CARTESIAN_POINT('Ctrl Pts',(19.4396987615087,-20.9559057976099,
8.24688040733223));
#174918=CARTESIAN_POINT('Ctrl Pts',(19.2273849944582,-21.0111037886464,
8.26091880600298));
#174919=CARTESIAN_POINT('Ctrl Pts',(19.1878047697689,-21.0201873452203,
8.2634771630064));
#174920=CARTESIAN_POINT('Ctrl Pts',(19.1404107505338,-21.0296378297155,
8.26645193086106));
#174921=CARTESIAN_POINT('Ctrl Pts',(19.1328282038753,-21.0311067114566,
8.26692517995119));
#174922=CARTESIAN_POINT('Ctrl Pts',(19.1210952105125,-21.033313062624,8.26765314845265));
#174923=CARTESIAN_POINT('Ctrl Pts',(19.1169504064292,-21.0340796703251,
8.26790947909269));
#174924=CARTESIAN_POINT('Ctrl Pts',(19.1092994189575,-21.0354711491618,
8.26838107640478));
#174925=CARTESIAN_POINT('Ctrl Pts',(19.105793974438,-21.0360995475655,8.2685965370917));
#174926=CARTESIAN_POINT('Ctrl Pts',(19.0979157755039,-21.0374913116965,
8.26907940641547));
#174927=CARTESIAN_POINT('Ctrl Pts',(19.0935422101888,-21.0382497699798,
8.26934653398458));
#174928=CARTESIAN_POINT('Ctrl Pts',(19.0823622400183,-21.0401523854795,
8.27002706491561));
#174929=CARTESIAN_POINT('Ctrl Pts',(19.0755525064793,-21.0412770336968,
8.27043938622134));
#174930=CARTESIAN_POINT('Ctrl Pts',(19.0360540379946,-21.0476020481865,
8.27281891744481));
#174931=CARTESIAN_POINT('Ctrl Pts',(19.0032504759751,-21.0520688180703,
8.27474734115056));
#174932=CARTESIAN_POINT('Ctrl Pts',(18.9517122908287,-21.0578590279552,
8.27772129711128));
#174933=CARTESIAN_POINT('Ctrl Pts',(18.9330433891822,-21.0597055426208,
8.27878715527497));
#174934=CARTESIAN_POINT('Ctrl Pts',(18.8831924885211,-21.0639679471237,
8.28160859935259));
#174935=CARTESIAN_POINT('Ctrl Pts',(18.8519767947686,-21.0659414875312,
8.28334967659106));
#174936=CARTESIAN_POINT('Ctrl Pts',(18.7822691807166,-21.0687996229342,
8.28720198555414));
#174937=CARTESIAN_POINT('Ctrl Pts',(18.7437737750249,-21.069327362334,8.28930524138088));
#174938=CARTESIAN_POINT('Ctrl Pts',(18.5960095125387,-21.067322877649,8.29735057932324));
#174939=CARTESIAN_POINT('Ctrl Pts',(18.4870143111089,-21.0573810651917,
8.30323550843215));
#174940=CARTESIAN_POINT('Ctrl Pts',(18.3250240604673,-21.0298489412745,
8.31237249618763));
#174941=CARTESIAN_POINT('Ctrl Pts',(18.2711534090569,-21.0185163759503,
8.31547580097375));
#174942=CARTESIAN_POINT('Ctrl Pts',(18.1845501275153,-20.9967416549042,
8.32061346158843));
#174943=CARTESIAN_POINT('Ctrl Pts',(18.1515215739635,-20.9875791030728,
8.32260855716529));
#174944=CARTESIAN_POINT('Ctrl Pts',(18.1083928115484,-20.9744790211142,
8.32526689862377));
#174945=CARTESIAN_POINT('Ctrl Pts',(18.0980786827963,-20.9712597200122,
8.32590666819378));
#174946=CARTESIAN_POINT('Ctrl Pts',(18.0812216952832,-20.9658562653355,
8.32695908473673));
#174947=CARTESIAN_POINT('Ctrl Pts',(18.0746639870634,-20.963718815554,8.32737019209324));
#174948=CARTESIAN_POINT('Ctrl Pts',(18.0619874506889,-20.9595183259161,
8.32816823083397));
#174949=CARTESIAN_POINT('Ctrl Pts',(18.055867379102,-20.9574592597113,8.3285550272166));
#174950=CARTESIAN_POINT('Ctrl Pts',(18.0417538772452,-20.9526388541996,
8.32945056231596));
#174951=CARTESIAN_POINT('Ctrl Pts',(18.0337674219762,-20.9498575657025,
8.32995995788408));
#174952=CARTESIAN_POINT('Ctrl Pts',(18.0123241681034,-20.9422455659553,
8.33133486694411));
#174953=CARTESIAN_POINT('Ctrl Pts',(17.9988994683721,-20.937326323758,8.33220331248653));
#174954=CARTESIAN_POINT('Ctrl Pts',(17.875670993979,-20.8907502251318,8.34024723497498));
#174955=CARTESIAN_POINT('Ctrl Pts',(17.7694797713999,-20.8401668164009,
8.34772770467395));
#174956=CARTESIAN_POINT('Ctrl Pts',(17.5265483616413,-20.6985881747918,
8.36609795142342));
#174957=CARTESIAN_POINT('Ctrl Pts',(17.3951035307402,-20.5999885505734,
8.37712897988476));
#174958=CARTESIAN_POINT('Ctrl Pts',(17.2538230692569,-20.4658458363614,
8.38949101534657));
#174959=CARTESIAN_POINT('Ctrl Pts',(17.2317792058561,-20.4439738215517,
8.39143495164522));
#174960=CARTESIAN_POINT('Ctrl Pts',(17.2052685503269,-20.4164862902024,
8.39378276540116));
#174961=CARTESIAN_POINT('Ctrl Pts',(17.2003398384282,-20.4113239707356,
8.39421969402791));
#174962=CARTESIAN_POINT('Ctrl Pts',(17.1926298699967,-20.403166367725,8.39490372547208));
#174963=CARTESIAN_POINT('Ctrl Pts',(17.1898310722684,-20.4001878427069,
8.39515215021537));
#174964=CARTESIAN_POINT('Ctrl Pts',(17.1846001212378,-20.3945885757427,
8.39561663827477));
#174965=CARTESIAN_POINT('Ctrl Pts',(17.1821660092802,-20.3919698082353,
8.39583284861467));
#174966=CARTESIAN_POINT('Ctrl Pts',(17.1766043151379,-20.3859557140663,
8.3963270476929));
#174967=CARTESIAN_POINT('Ctrl Pts',(17.1734812015023,-20.3825563217124,
8.39660469554475));
#174968=CARTESIAN_POINT('Ctrl Pts',(17.1638449846068,-20.3719985524893,
8.3974618864648));
#174969=CARTESIAN_POINT('Ctrl Pts',(17.1573697245677,-20.3648055931578,
8.39803863741119));
#174970=CARTESIAN_POINT('Ctrl Pts',(17.0888253090605,-20.2876057486507,
8.4041550904539));
#174971=CARTESIAN_POINT('Ctrl Pts',(17.0314046716022,-20.2135926837676,
8.40937985811453));
#174972=CARTESIAN_POINT('Ctrl Pts',(16.9052198204781,-20.0265625621903,
8.42175707351962));
#174973=CARTESIAN_POINT('Ctrl Pts',(16.8417777048939,-19.9104449575379,
8.42880642808041));
#174974=CARTESIAN_POINT('Ctrl Pts',(16.7672717970289,-19.7373961120652,
8.43927195262707));
#174975=CARTESIAN_POINT('Ctrl Pts',(16.7470574651501,-19.6847520432532,
8.4424477018452));
#174976=CARTESIAN_POINT('Ctrl Pts',(16.7177768297081,-19.5983354043262,
8.44769447256432));
#174977=CARTESIAN_POINT('Ctrl Pts',(16.7074032721517,-19.5650341130707,
8.4497240100253));
#174978=CARTESIAN_POINT('Ctrl Pts',(16.6948809048811,-19.5210347555933,
8.45242171395637));
#174979=CARTESIAN_POINT('Ctrl Pts',(16.6919850793017,-19.510553752222,8.45306550738155));
#174980=CARTESIAN_POINT('Ctrl Pts',(16.6873806765225,-19.4933742939246,
8.45412285755148));
#174981=CARTESIAN_POINT('Ctrl Pts',(16.6856239146994,-19.4866888747486,
8.45453484623635));
#174982=CARTESIAN_POINT('Ctrl Pts',(16.6822909630589,-19.4737476841383,
8.45533339730518));
#174983=CARTESIAN_POINT('Ctrl Pts',(16.680710562815,-19.4674930687072,8.45571981833572));
#174984=CARTESIAN_POINT('Ctrl Pts',(16.6771333681844,-19.4530584379528,
8.45661274639762));
#174985=CARTESIAN_POINT('Ctrl Pts',(16.6751567490611,-19.4448735782977,
8.45711989825493));
#174986=CARTESIAN_POINT('Ctrl Pts',(16.6699846634008,-19.4228826879038,
8.45848483774115));
#174987=CARTESIAN_POINT('Ctrl Pts',(16.6668789476151,-19.4090561835746,
8.45934549164943));
#174988=CARTESIAN_POINT('Ctrl Pts',(16.6325818105127,-19.2488618864125,
8.46934706920211));
#174989=CARTESIAN_POINT('Ctrl Pts',(16.6168624934317,-19.0996426934776,
8.47899859255897));
#174990=CARTESIAN_POINT('Ctrl Pts',(16.6171394762141,-18.8002697688707,
8.49872815360886));
#174991=CARTESIAN_POINT('Ctrl Pts',(16.6331712122105,-18.6509266940689,
8.50874331107301));
#174992=CARTESIAN_POINT('Ctrl Pts',(16.6681544975829,-18.4891628821534,
8.51906805533745));
#174993=CARTESIAN_POINT('Ctrl Pts',(16.6716463807226,-18.4738437285133,
8.52004014730388));
#174994=CARTESIAN_POINT('Ctrl Pts',(16.6766589553073,-18.4529304758363,
8.52135811576691));
#174995=CARTESIAN_POINT('Ctrl Pts',(16.6780324478155,-18.4473020801462,
8.52171191459495));
#174996=CARTESIAN_POINT('Ctrl Pts',(16.6802514660228,-18.4383682263632,
8.52227197272355));
#174997=CARTESIAN_POINT('Ctrl Pts',(16.6810818949191,-18.435059100171,8.52247908773211));
#174998=CARTESIAN_POINT('Ctrl Pts',(16.682813267587,-18.4282298294263,8.52290581785142));
#174999=CARTESIAN_POINT('Ctrl Pts',(16.6837152749943,-18.4247099950044,
8.52312536430036));
#175000=CARTESIAN_POINT('Ctrl Pts',(16.6858857791515,-18.416329981778,8.5236471584064));
#175001=CARTESIAN_POINT('Ctrl Pts',(16.6871625295355,-18.4114719241799,
8.52394893028115));
#175002=CARTESIAN_POINT('Ctrl Pts',(16.6915249191276,-18.3951100642402,
8.52496299762822));
#175003=CARTESIAN_POINT('Ctrl Pts',(16.6946904095671,-18.3836275291725,
8.52567082472598));
#175004=CARTESIAN_POINT('Ctrl Pts',(16.7120038283707,-18.3228320159641,
8.52940108849747));
#175005=CARTESIAN_POINT('Ctrl Pts',(16.727837983075,-18.2740394767152,8.53233405453527));
#175006=CARTESIAN_POINT('Ctrl Pts',(16.74541940036,-18.2258896786745,8.53521106622902));
#175007=CARTESIAN_POINT('Origin',(18.734,-18.952,0.));
#175008=CARTESIAN_POINT('',(16.7437494325541,-18.2252642451362,9.55561791118868));
#175009=CARTESIAN_POINT('',(16.7454193880554,-18.2258897123729,9.33206801777758));
#175010=CARTESIAN_POINT('',(16.7454193692319,-18.2258897639242,0.));
#175011=CARTESIAN_POINT('',(16.6163525130807,-18.950106484017,9.51094372097752));
#175012=CARTESIAN_POINT('Ctrl Pts',(16.6163525130807,-18.950106484017,9.51094372097752));
#175013=CARTESIAN_POINT('Ctrl Pts',(16.6150298054201,-18.8071177642836,
9.51955279572483));
#175014=CARTESIAN_POINT('Ctrl Pts',(16.6379357302198,-18.5602068930662,
9.53444419246188));
#175015=CARTESIAN_POINT('Ctrl Pts',(16.7071052757493,-18.3228113044306,
9.54933558919893));
#175016=CARTESIAN_POINT('Ctrl Pts',(16.7437494325541,-18.2252642451362,
9.55561791118868));
#175017=CARTESIAN_POINT('Ctrl Pts',(16.6170008641637,-18.9500871830904,
9.51057060101912));
#175018=CARTESIAN_POINT('Ctrl Pts',(16.6168630285762,-19.1026359284247,
9.50227624137429));
#175019=CARTESIAN_POINT('Ctrl Pts',(16.6332131376109,-19.2547442788604,
9.49405436693276));
#175020=CARTESIAN_POINT('Ctrl Pts',(16.6711097710214,-19.4282348466107,
9.4838681377401));
#175021=CARTESIAN_POINT('Ctrl Pts',(16.6768854893957,-19.4525951877099,
9.48241989998714));
#175022=CARTESIAN_POINT('Ctrl Pts',(16.6863088548723,-19.4894182436269,
9.48020049124768));
#175023=CARTESIAN_POINT('Ctrl Pts',(16.6896415039904,-19.5019597468797,
9.47943921501431));
#175024=CARTESIAN_POINT('Ctrl Pts',(16.6960379446959,-19.5251691160293,
9.47801999813407));
#175025=CARTESIAN_POINT('Ctrl Pts',(16.6990707475128,-19.5358451033516,
9.4773630695322));
#175026=CARTESIAN_POINT('Ctrl Pts',(16.7041423648668,-19.5531783841545,
9.4762896021547));
#175027=CARTESIAN_POINT('Ctrl Pts',(16.7061303467709,-19.5598504225682,
9.47587472563739));
#175028=CARTESIAN_POINT('Ctrl Pts',(16.7100186725365,-19.5726689746564,
9.47507438167625));
#175029=CARTESIAN_POINT('Ctrl Pts',(16.7119141981425,-19.5788168779883,
9.47468907591658));
#175030=CARTESIAN_POINT('Ctrl Pts',(16.7163213512743,-19.5928828868289,
9.47380414513183));
#175031=CARTESIAN_POINT('Ctrl Pts',(16.7188516072731,-19.6007950033501,
9.47330391220546));
#175032=CARTESIAN_POINT('Ctrl Pts',(16.7257038508009,-19.621795156383,9.47196955823238));
#175033=CARTESIAN_POINT('Ctrl Pts',(16.7301071476363,-19.6348560584379,
9.47113276814319));
#175034=CARTESIAN_POINT('Ctrl Pts',(16.7650760746778,-19.7353278097386,
9.46464131649608));
#175035=CARTESIAN_POINT('Ctrl Pts',(16.801215612779,-19.8206796802427,9.45880081225721));
#175036=CARTESIAN_POINT('Ctrl Pts',(16.8638223093732,-19.9451305581103,
9.44979592761911));
#175037=CARTESIAN_POINT('Ctrl Pts',(16.8861995929533,-19.986169343978,9.44674237297692));
#175038=CARTESIAN_POINT('Ctrl Pts',(16.9361603738986,-20.0709887023405,
9.44027008730656));
#175039=CARTESIAN_POINT('Ctrl Pts',(16.9640285347178,-20.1145678142593,
9.43684913489017));
#175040=CARTESIAN_POINT('Ctrl Pts',(17.0413692551478,-20.226273322753,9.42787444805212));
#175041=CARTESIAN_POINT('Ctrl Pts',(17.0933610523225,-20.2925510143061,
9.4223349661178));
#175042=CARTESIAN_POINT('Ctrl Pts',(17.1737192473799,-20.3832877870346,
9.41460144864412));
#175043=CARTESIAN_POINT('Ctrl Pts',(17.1989999424321,-20.4103675689605,
9.41227279420793));
#175044=CARTESIAN_POINT('Ctrl Pts',(17.2302741118558,-20.4421524866696,
9.40952892294982));
#175045=CARTESIAN_POINT('Ctrl Pts',(17.2355971505706,-20.4475048929915,
9.40906649769853));
#175046=CARTESIAN_POINT('Ctrl Pts',(17.2439142735717,-20.455778914969,9.40835124419744));
#175047=CARTESIAN_POINT('Ctrl Pts',(17.2468885184086,-20.4587202591152,
9.40809689566886));
#175048=CARTESIAN_POINT('Ctrl Pts',(17.2524127758881,-20.464151115818,9.40762715223498));
#175049=CARTESIAN_POINT('Ctrl Pts',(17.2549603344813,-20.4666429836246,
9.4074115749229));
#175050=CARTESIAN_POINT('Ctrl Pts',(17.2607240770139,-20.4722523199491,
9.40692618985666));
#175051=CARTESIAN_POINT('Ctrl Pts',(17.2639438602511,-20.4753660126167,
9.40665667679774));
#175052=CARTESIAN_POINT('Ctrl Pts',(17.2734472413167,-20.4844980725033,
9.40586590515163));
#175053=CARTESIAN_POINT('Ctrl Pts',(17.2797581754032,-20.4904880320007,
9.4053467995836));
#175054=CARTESIAN_POINT('Ctrl Pts',(17.3247712329339,-20.5326872613134,
9.40168516972385));
#175055=CARTESIAN_POINT('Ctrl Pts',(17.3647876100627,-20.5674740385254,
9.39864270924847));
#175056=CARTESIAN_POINT('Ctrl Pts',(17.4206664686786,-20.6124804292018,
9.39460645865098));
#175057=CARTESIAN_POINT('Ctrl Pts',(17.4354176666934,-20.6240419171314,
9.39355996207498));
#175058=CARTESIAN_POINT('Ctrl Pts',(17.6009950400266,-20.7503027312398,
9.38199931053239));
#175059=CARTESIAN_POINT('Ctrl Pts',(17.7664088634658,-20.8444495644443,
9.3720574552812));
#175060=CARTESIAN_POINT('Ctrl Pts',(17.9920076087095,-20.9354380281162,
9.35827608787552));
#175061=CARTESIAN_POINT('Ctrl Pts',(18.0426094513431,-20.9536387080224,
9.3551786841135));
#175062=CARTESIAN_POINT('Ctrl Pts',(18.1058854203258,-20.9737122951147,
9.35127380574584));
#175063=CARTESIAN_POINT('Ctrl Pts',(18.1179583581891,-20.9774237123538,
9.35052740289039));
#175064=CARTESIAN_POINT('Ctrl Pts',(18.1370610730952,-20.9831096032239,
9.34934396473204));
#175065=CARTESIAN_POINT('Ctrl Pts',(18.1440692141918,-20.9851561594403,
9.34890929003115));
#175066=CARTESIAN_POINT('Ctrl Pts',(18.1572084480777,-20.9889194981888,
9.34809332630986));
#175067=CARTESIAN_POINT('Ctrl Pts',(18.1633369862294,-20.9906449567822,
9.34771232532133));
#175068=CARTESIAN_POINT('Ctrl Pts',(18.1770446299411,-20.9944376199626,
9.34685918695421));
#175069=CARTESIAN_POINT('Ctrl Pts',(18.1846276176632,-20.9964903273447,
9.34638658425659));
#175070=CARTESIAN_POINT('Ctrl Pts',(18.203823792604,-21.0015722065065,9.34518847903388));
#175071=CARTESIAN_POINT('Ctrl Pts',(18.2154515255211,-21.0045448864476,
9.34446116041709));
#175072=CARTESIAN_POINT('Ctrl Pts',(18.2810967571627,-21.0207339612208,
9.34034559922399));
#175073=CARTESIAN_POINT('Ctrl Pts',(18.3355890743815,-21.0319157143376,
9.33689253613938));
#175074=CARTESIAN_POINT('Ctrl Pts',(18.4150613046443,-21.0449856603688,
9.33180051495979));
#175075=CARTESIAN_POINT('Ctrl Pts',(18.4397368265098,-21.0485972379414,
9.33021189789655));
#175076=CARTESIAN_POINT('Ctrl Pts',(18.6245329149065,-21.0723179789876,
9.31826188679705));
#175077=CARTESIAN_POINT('Ctrl Pts',(18.7864149674423,-21.0744926401331,
9.30744168130844));
#175078=CARTESIAN_POINT('Ctrl Pts',(18.995687590613,-21.0533349845132,9.29371561837982));
#175079=CARTESIAN_POINT('Ctrl Pts',(19.0442476776019,-21.0467162397084,
9.29055402263721));
#175080=CARTESIAN_POINT('Ctrl Pts',(19.1184180868714,-21.0339705402854,
9.28580165823864));
#175081=CARTESIAN_POINT('Ctrl Pts',(19.1442153128678,-21.0290416798979,
9.284163221157));
#175082=CARTESIAN_POINT('Ctrl Pts',(19.1765304713502,-21.0222418886843,
9.28213469462177));
#175083=CARTESIAN_POINT('Ctrl Pts',(19.1831388721314,-21.0208182549778,
9.28172112802435));
#175084=CARTESIAN_POINT('Ctrl Pts',(19.1936500341221,-21.018501118757,9.28106545813052));
#175085=CARTESIAN_POINT('Ctrl Pts',(19.1975572104995,-21.0176281710175,
9.28082220625388));
#175086=CARTESIAN_POINT('Ctrl Pts',(19.2049662109763,-21.0159507594879,
9.2803618654251));
#175087=CARTESIAN_POINT('Ctrl Pts',(19.208468419012,-21.0151484747797,9.28014466145809));
#175088=CARTESIAN_POINT('Ctrl Pts',(19.2165293682955,-21.0132802638661,
9.27964562006103));
#175089=CARTESIAN_POINT('Ctrl Pts',(19.2210866263909,-21.0122081294922,
9.2793641423444));
#175090=CARTESIAN_POINT('Ctrl Pts',(19.2332997661203,-21.0092920927271,
9.27861146892223));
#175091=CARTESIAN_POINT('Ctrl Pts',(19.2409490626484,-21.0074205563547,
9.27814181724887));
#175092=CARTESIAN_POINT('Ctrl Pts',(19.2983816324014,-20.9930285366406,
9.2746276045876));
#175093=CARTESIAN_POINT('Ctrl Pts',(19.3477095205682,-20.9787426223841,
9.27167729450712));
#175094=CARTESIAN_POINT('Ctrl Pts',(19.4099602963827,-20.958232370704,9.26798503429809));
#175095=CARTESIAN_POINT('Ctrl Pts',(19.4234025416554,-20.9536530159695,
9.267189625697));
#175096=CARTESIAN_POINT('Ctrl Pts',(19.57171929182,-20.9014547674071,9.25842426669654));
#175097=CARTESIAN_POINT('Ctrl Pts',(19.7014852396573,-20.840418299427,9.25083035381799));
#175098=CARTESIAN_POINT('Ctrl Pts',(19.9038114445807,-20.7188827754983,
9.23783216521445));
#175099=CARTESIAN_POINT('Ctrl Pts',(19.980264472034,-20.6658131544802,9.23261206732595));
#175100=CARTESIAN_POINT('Ctrl Pts',(20.0694824216427,-20.5947479920948,
9.22596826874101));
#175101=CARTESIAN_POINT('Ctrl Pts',(20.0857896716596,-20.5813553633962,
9.22472985428435));
#175102=CARTESIAN_POINT('Ctrl Pts',(20.1087323899523,-20.5619317213766,
9.22295150285492));
#175103=CARTESIAN_POINT('Ctrl Pts',(20.1155342873075,-20.5560985944487,
9.22241965478348));
#175104=CARTESIAN_POINT('Ctrl Pts',(20.1272192451607,-20.5459484348279,
9.22149787738007));
#175105=CARTESIAN_POINT('Ctrl Pts',(20.1321198142782,-20.5416516792789,
9.22110879221236));
#175106=CARTESIAN_POINT('Ctrl Pts',(20.1414750085189,-20.5333724430294,
9.22036117783167));
#175107=CARTESIAN_POINT('Ctrl Pts',(20.1459327734786,-20.5293935923596,
9.22000280286259));
#175108=CARTESIAN_POINT('Ctrl Pts',(20.1575026569676,-20.5189783644121,
9.21906703842031));
#175109=CARTESIAN_POINT('Ctrl Pts',(20.1645879218864,-20.5125124805477,
9.21848840416575));
#175110=CARTESIAN_POINT('Ctrl Pts',(20.1887103820941,-20.4901964097252,
9.21649896808299));
#175111=CARTESIAN_POINT('Ctrl Pts',(20.2055295826899,-20.4741140266492,
9.21507825397089));
#175112=CARTESIAN_POINT('Ctrl Pts',(20.3440141903878,-20.3372553014399,
9.20309082120404));
#175113=CARTESIAN_POINT('Ctrl Pts',(20.4508381515618,-20.2024090510055,
9.19185658233501));
#175114=CARTESIAN_POINT('Ctrl Pts',(20.5871043900858,-19.979507910268,9.17459271599519));
#175115=CARTESIAN_POINT('Ctrl Pts',(20.6290584778028,-19.8999049204125,
9.1686615346981));
#175116=CARTESIAN_POINT('Ctrl Pts',(20.6815904813275,-19.7827019421545,
9.16045637286842));
#175117=CARTESIAN_POINT('Ctrl Pts',(20.6963918647558,-19.7471056538739,
9.15803089502281));
#175118=CARTESIAN_POINT('Ctrl Pts',(20.7129436603057,-19.7040165795312,
9.15519024427024));
#175119=CARTESIAN_POINT('Ctrl Pts',(20.7156349976042,-19.6968957557035,
9.15472387953935));
#175120=CARTESIAN_POINT('Ctrl Pts',(20.7197484629079,-19.6858321380763,
9.15400422203568));
#175121=CARTESIAN_POINT('Ctrl Pts',(20.7211973585329,-19.6818994614036,
9.15374937473223));
#175122=CARTESIAN_POINT('Ctrl Pts',(20.7238564117507,-19.6746154964506,
9.1532791688215));
#175123=CARTESIAN_POINT('Ctrl Pts',(20.7250697775859,-19.671265483801,9.15306362487697));
#175124=CARTESIAN_POINT('Ctrl Pts',(20.727785886357,-19.6637069679382,9.1525788911479));
#175125=CARTESIAN_POINT('Ctrl Pts',(20.7292837607456,-19.6594967729928,
9.15230999255343));
#175126=CARTESIAN_POINT('Ctrl Pts',(20.7336428087024,-19.6471204985923,
9.15152269194647));
#175127=CARTESIAN_POINT('Ctrl Pts',(20.7364673011132,-19.6389414703811,
9.15100641474822));
#175128=CARTESIAN_POINT('Ctrl Pts',(20.7558475575602,-19.5816856739003,
9.14741883653966));
#175129=CARTESIAN_POINT('Ctrl Pts',(20.7706489808566,-19.532028847478,9.14444304396547));
#175130=CARTESIAN_POINT('Ctrl Pts',(20.7889953217657,-19.4610631632442,
9.14031546702329));
#175131=CARTESIAN_POINT('Ctrl Pts',(20.7940584928292,-19.4401701816199,
9.13911537110776));
#175132=CARTESIAN_POINT('Ctrl Pts',(20.8292194241577,-19.2847765979516,
9.13027778356622));
#175133=CARTESIAN_POINT('Ctrl Pts',(20.8464368504934,-19.1476985621164,
9.12294755883473));
#175134=CARTESIAN_POINT('Ctrl Pts',(20.8526907917146,-18.9191824569172,
9.11034420747673));
#175135=CARTESIAN_POINT('Ctrl Pts',(20.8493359723429,-18.8283931623072,
9.10524188335007));
#175136=CARTESIAN_POINT('Ctrl Pts',(20.8380618689454,-18.7173797977746,
9.09874057585315));
#175137=CARTESIAN_POINT('Ctrl Pts',(20.8356512825713,-18.6966868032178,
9.09751771301583));
#175138=CARTESIAN_POINT('Ctrl Pts',(20.8317736991271,-18.6671948462735,
9.09575784127902));
#175139=CARTESIAN_POINT('Ctrl Pts',(20.8305558260603,-18.6583639449104,
9.09522868979839));
#175140=CARTESIAN_POINT('Ctrl Pts',(20.8283522355628,-18.6430985848412,
9.09431009661379));
#175141=CARTESIAN_POINT('Ctrl Pts',(20.8273925425078,-18.6366604490288,
9.093921483184));
#175142=CARTESIAN_POINT('Ctrl Pts',(20.825493449877,-18.6243111649564,9.09317372452792));
#175143=CARTESIAN_POINT('Ctrl Pts',(20.8245586428585,-18.6183993658331,
9.09281472849929));
#175144=CARTESIAN_POINT('Ctrl Pts',(20.8220516560144,-18.6029694160947,
9.09187500465252));
#175145=CARTESIAN_POINT('Ctrl Pts',(20.8204394760468,-18.5934579875939,
9.09129301129374));
#175146=CARTESIAN_POINT('Ctrl Pts',(20.8146594297214,-18.5607170936752,
9.08928005889486));
#175147=CARTESIAN_POINT('Ctrl Pts',(20.8101682864919,-18.537547167095,9.08783887014091));
#175148=CARTESIAN_POINT('Ctrl Pts',(20.7711450461931,-18.3528141391553,
9.0762103655146));
#175149=CARTESIAN_POINT('Ctrl Pts',(20.718200834135,-18.1957520440936,9.06540857010438));
#175150=CARTESIAN_POINT('Ctrl Pts',(20.5930548615233,-17.9312940756027,
9.04607406590476));
#175151=CARTESIAN_POINT('Ctrl Pts',(20.5282575334772,-17.8212603286336,
9.03764638292147));
#175152=CARTESIAN_POINT('Ctrl Pts',(20.4469596082138,-17.7079734169417,
9.02899834211065));
#175153=CARTESIAN_POINT('Ctrl Pts',(20.4398862330722,-17.6982915275852,
9.02825963610064));
#175154=CARTESIAN_POINT('Ctrl Pts',(20.429725237027,-17.6846285915678,9.02721834955958));
#175155=CARTESIAN_POINT('Ctrl Pts',(20.4267052287265,-17.6805978699693,
9.02691130383708));
#175156=CARTESIAN_POINT('Ctrl Pts',(20.4214803304768,-17.6736759589614,
9.02638432512594));
#175157=CARTESIAN_POINT('Ctrl Pts',(20.4192823334509,-17.6707796142039,
9.02616391457937));
#175158=CARTESIAN_POINT('Ctrl Pts',(20.4150096533626,-17.6651794376228,
9.02573794579844));
#175159=CARTESIAN_POINT('Ctrl Pts',(20.4129359031929,-17.6624749526261,
9.02553232236138));
#175160=CARTESIAN_POINT('Ctrl Pts',(20.4073307929739,-17.6552014794134,
9.0249795211916));
#175161=CARTESIAN_POINT('Ctrl Pts',(20.4037872245758,-17.65064187399,9.02463319910274));
#175162=CARTESIAN_POINT('Ctrl Pts',(20.3906101320906,-17.6338289890199,
9.02335676117982));
#175163=CARTESIAN_POINT('Ctrl Pts',(20.3808597597506,-17.6216673695781,
9.02243458343505));
#175164=CARTESIAN_POINT('Ctrl Pts',(20.2843001082529,-17.5039174710135,
9.01350486822727));
#175165=CARTESIAN_POINT('Ctrl Pts',(20.1875786924896,-17.4068486173566,
9.00612142620185));
#175166=CARTESIAN_POINT('Ctrl Pts',(19.9630196291148,-17.2213707213965,
8.99030483061929));
#175167=CARTESIAN_POINT('Ctrl Pts',(19.8334806452871,-17.1363178140282,
8.98188544487261));
#175168=CARTESIAN_POINT('Ctrl Pts',(19.6768994420232,-17.0564573188982,
8.97164904727588));
#175169=CARTESIAN_POINT('Ctrl Pts',(19.6578075229907,-17.0470797849851,
8.97040087663036));
#175170=CARTESIAN_POINT('Ctrl Pts',(19.6304507516507,-17.0341507211708,
8.96861094213637));
#175171=CARTESIAN_POINT('Ctrl Pts',(19.6222991734192,-17.030361537347,8.96807741411682));
#175172=CARTESIAN_POINT('Ctrl Pts',(19.6081915301588,-17.0239126798679,
8.96715364965005));
#175173=CARTESIAN_POINT('Ctrl Pts',(19.6022468072357,-17.0212283859265,
8.96676426729695));
#175174=CARTESIAN_POINT('Ctrl Pts',(19.590838302584,-17.0161403063087,8.96601672877439));
#175175=CARTESIAN_POINT('Ctrl Pts',(19.5853765656866,-17.0137320689082,
8.96565872996057));
#175176=CARTESIAN_POINT('Ctrl Pts',(19.5711423429917,-17.007527561138,8.96472537405398));
#175177=CARTESIAN_POINT('Ctrl Pts',(19.562354273364,-17.0037675803344,8.96414878476424));
#175178=CARTESIAN_POINT('Ctrl Pts',(19.5322725828297,-16.9911374403592,
8.96217376390338));
#175179=CARTESIAN_POINT('Ctrl Pts',(19.5108601772163,-16.9825560954173,
8.96076561271371));
#175180=CARTESIAN_POINT('Ctrl Pts',(19.3263064449611,-16.9120713856958,
8.94860481902744));
#175181=CARTESIAN_POINT('Ctrl Pts',(19.1562579689345,-16.8702193128321,
8.93715752021208));
#175182=CARTESIAN_POINT('Ctrl Pts',(18.8959421133494,-16.839381431829,8.91983712807145));
#175183=CARTESIAN_POINT('Ctrl Pts',(18.8082760399015,-16.8344855449401,
8.9140546311083));
#175184=CARTESIAN_POINT('Ctrl Pts',(18.6825554808543,-16.835284044295,8.90602655449178));
#175185=CARTESIAN_POINT('Ctrl Pts',(18.6445671301375,-16.8365484754125,
8.90363599244644));
#175186=CARTESIAN_POINT('Ctrl Pts',(18.5990627640118,-16.8392912112434,
8.90083070727008));
#175187=CARTESIAN_POINT('Ctrl Pts',(18.5914970681917,-16.8397880309577,
8.90036623056498));
#175188=CARTESIAN_POINT('Ctrl Pts',(18.5797601669503,-16.8406221126032,
8.89964885381658));
#175189=CARTESIAN_POINT('Ctrl Pts',(18.5755871061486,-16.8409311083605,
8.89939441463954));
#175190=CARTESIAN_POINT('Ctrl Pts',(18.5678619268868,-16.841526157585,8.8989245873623));
#175191=CARTESIAN_POINT('Ctrl Pts',(18.5643096450214,-16.8418088042587,
8.89870901632222));
#175192=CARTESIAN_POINT('Ctrl Pts',(18.5562959080279,-16.8424668051246,
8.89822375057582));
#175193=CARTESIAN_POINT('Ctrl Pts',(18.5518349327411,-16.842847342248,8.89795434992376));
#175194=CARTESIAN_POINT('Ctrl Pts',(18.5387170287545,-16.8440082753117,
8.89716421376405));
#175195=CARTESIAN_POINT('Ctrl Pts',(18.5300635393934,-16.8448278484872,
8.89664562609733));
#175196=CARTESIAN_POINT('Ctrl Pts',(18.4689435004876,-16.8509965790054,
8.89299995147784));
#175197=CARTESIAN_POINT('Ctrl Pts',(18.4166832583751,-16.8582518305724,
8.8899719299562));
#175198=CARTESIAN_POINT('Ctrl Pts',(18.3492009418416,-16.8702056154985,
8.8861158071719));
#175199=CARTESIAN_POINT('Ctrl Pts',(18.3336886604828,-16.8731327547037,
8.88523314299887));
#175200=CARTESIAN_POINT('Ctrl Pts',(18.2683583034559,-16.8862188532635,
8.88152637930244));
#175201=CARTESIAN_POINT('Ctrl Pts',(18.218880467618,-16.8979975289314,8.87874487286666));
#175202=CARTESIAN_POINT('Ctrl Pts',(18.0644204496828,-16.9407012860923,
8.87001964490624));
#175203=CARTESIAN_POINT('Ctrl Pts',(17.9613874506527,-16.9779867623235,
8.86412866468287));
#175204=CARTESIAN_POINT('Ctrl Pts',(17.8114225671373,-17.0458035634928,
8.8549776090888));
#175205=CARTESIAN_POINT('Ctrl Pts',(17.7620546639081,-17.0704964548709,
8.85186624081543));
#175206=CARTESIAN_POINT('Ctrl Pts',(17.6836215447672,-17.1136384126272,
8.84671642245495));
#175207=CARTESIAN_POINT('Ctrl Pts',(17.6539415351062,-17.1309174262474,
8.8447174767515));
#175208=CARTESIAN_POINT('Ctrl Pts',(17.615486751019,-17.1545757249732,8.84205473274584));
#175209=CARTESIAN_POINT('Ctrl Pts',(17.6063211130725,-17.160311903814,8.84141451012977));
#175210=CARTESIAN_POINT('Ctrl Pts',(17.5913800238297,-17.1698226277735,
8.84036153816167));
#175211=CARTESIAN_POINT('Ctrl Pts',(17.5855782989727,-17.1735556823739,
8.83995033161849));
#175212=CARTESIAN_POINT('Ctrl Pts',(17.5743824824523,-17.1808371335567,
8.83915223598762));
#175213=CARTESIAN_POINT('Ctrl Pts',(17.5689861668501,-17.1843819831173,
8.83876548261964));
#175214=CARTESIAN_POINT('Ctrl Pts',(17.5565627275212,-17.1926245659259,
8.83787024469848));
#175215=CARTESIAN_POINT('Ctrl Pts',(17.5495473900773,-17.1973397878062,
8.83736110466524));
#175216=CARTESIAN_POINT('Ctrl Pts',(17.5307542226738,-17.210135307839,8.83598733247383));
#175217=CARTESIAN_POINT('Ctrl Pts',(17.5190297758388,-17.2182928894541,
8.83511977580285));
#175218=CARTESIAN_POINT('Ctrl Pts',(17.3924219239212,-17.3082985312384,
8.82563479820473));
#175219=CARTESIAN_POINT('Ctrl Pts',(17.2859326239898,-17.4012989398142,
8.8165676813664));
#175220=CARTESIAN_POINT('Ctrl Pts',(17.1234054325967,-17.5746791701776,
8.80093330374722));
#175221=CARTESIAN_POINT('Ctrl Pts',(17.0622207663085,-17.649624508218,8.79450513321501));
#175222=CARTESIAN_POINT('Ctrl Pts',(16.9686660987399,-17.7817260525203,
8.78394199412348));
#175223=CARTESIAN_POINT('Ctrl Pts',(16.9334397144459,-17.836684264969,8.77974786839756));
#175224=CARTESIAN_POINT('Ctrl Pts',(16.8942250415197,-17.9045792667621,
8.77487642530745));
#175225=CARTESIAN_POINT('Ctrl Pts',(16.8877510578125,-17.9160333240194,
8.77406483650845));
#175226=CARTESIAN_POINT('Ctrl Pts',(16.8788540525536,-17.9321226307659,
8.77293983791907));
#175227=CARTESIAN_POINT('Ctrl Pts',(16.8763409389655,-17.936707357999,8.77262095320507));
#175228=CARTESIAN_POINT('Ctrl Pts',(16.8720920953019,-17.9445272052275,
8.7720799852235));
#175229=CARTESIAN_POINT('Ctrl Pts',(16.8703477576582,-17.947757599918,8.77185735784182));
#175230=CARTESIAN_POINT('Ctrl Pts',(16.8670223269083,-17.9539545761097,
8.77143192836215));
#175231=CARTESIAN_POINT('Ctrl Pts',(16.8654398911356,-17.9569203951959,
8.77122903816278));
#175232=CARTESIAN_POINT('Ctrl Pts',(16.8612708339721,-17.9647791020992,
8.77069328874368));
#175233=CARTESIAN_POINT('Ctrl Pts',(16.858696303531,-17.9696784242801,8.77036119213161));
#175234=CARTESIAN_POINT('Ctrl Pts',(16.8496512053957,-17.9870563738762,
8.76918976646572));
#175235=CARTESIAN_POINT('Ctrl Pts',(16.8432855757738,-17.999589599478,8.76835678229432));
#175236=CARTESIAN_POINT('Ctrl Pts',(16.8025847915486,-18.0817415215493,
8.76296777001828));
#175237=CARTESIAN_POINT('Ctrl Pts',(16.7720027305155,-18.1530865146677,
8.75861677565704));
#175238=CARTESIAN_POINT('Ctrl Pts',(16.7454192490578,-18.2258900930424,
8.75434673926218));
#175239=CARTESIAN_POINT('',(16.6170000979997,-18.9526441512856,9.29097292592683));
#175240=CARTESIAN_POINT('Ctrl Pts',(16.74541940036,-18.2258896786745,8.53521106622902));
#175241=CARTESIAN_POINT('Ctrl Pts',(16.7707333810102,-18.1565628982361,
8.53935342956444));
#175242=CARTESIAN_POINT('Ctrl Pts',(16.7996695249671,-18.0885686098479,
8.54338075134243));
#175243=CARTESIAN_POINT('Ctrl Pts',(16.9057914982917,-17.8715014022299,
8.55651366874445));
#175244=CARTESIAN_POINT('Ctrl Pts',(16.9970988704475,-17.7301198635963,
8.56556714094202));
#175245=CARTESIAN_POINT('Ctrl Pts',(17.1191104689661,-17.5829229396598,
8.57667155906595));
#175246=CARTESIAN_POINT('Ctrl Pts',(17.1343922610984,-17.5650987016149,
8.578046558463));
#175247=CARTESIAN_POINT('Ctrl Pts',(17.1563534137942,-17.5403297407529,
8.58000255525429));
#175248=CARTESIAN_POINT('Ctrl Pts',(17.1627889134241,-17.5331704159487,
8.58057339835522));
#175249=CARTESIAN_POINT('Ctrl Pts',(17.173301900474,-17.5216342353551,8.58150227676022));
#175250=CARTESIAN_POINT('Ctrl Pts',(17.1773495487018,-17.5172302798447,
8.58185904591863));
#175251=CARTESIAN_POINT('Ctrl Pts',(17.1858429074168,-17.5080675130306,
8.58260591182747));
#175252=CARTESIAN_POINT('Ctrl Pts',(17.190292015493,-17.5033119496111,8.58299615200241));
#175253=CARTESIAN_POINT('Ctrl Pts',(17.2008948677985,-17.4920830758555,
8.58392385028291));
#175254=CARTESIAN_POINT('Ctrl Pts',(17.2070677385546,-17.4856280700579,
8.58446213218822));
#175255=CARTESIAN_POINT('Ctrl Pts',(17.2278430921896,-17.4641765920693,
8.58626788552569));
#175256=CARTESIAN_POINT('Ctrl Pts',(17.2426267496613,-17.4493580257008,
8.58754326629444));
#175257=CARTESIAN_POINT('Ctrl Pts',(17.3232616703567,-17.3708949518692,
8.5944509953967));
#175258=CARTESIAN_POINT('Ctrl Pts',(17.3929624790881,-17.3113628103603,
8.6002576527638));
#175259=CARTESIAN_POINT('Ctrl Pts',(17.5419206457441,-17.199985842425,8.61232139718495));
#175260=CARTESIAN_POINT('Ctrl Pts',(17.6212468292611,-17.1485628769628,
8.61857368246792));
#175261=CARTESIAN_POINT('Ctrl Pts',(17.768585038123,-17.0664832176997,8.62971089495122));
#175262=CARTESIAN_POINT('Ctrl Pts',(17.8352936647747,-17.0337904807951,
8.63459302445037));
#175263=CARTESIAN_POINT('Ctrl Pts',(17.9424467806769,-16.9880963998862,
8.64206172811646));
#175264=CARTESIAN_POINT('Ctrl Pts',(17.9817987943188,-16.9726900828249,
8.64472884211933));
#175265=CARTESIAN_POINT('Ctrl Pts',(18.0286043463917,-16.9559635570945,
8.64779172826197));
#175266=CARTESIAN_POINT('Ctrl Pts',(18.0356335873788,-16.9534933407631,
8.64824884770175));
#175267=CARTESIAN_POINT('Ctrl Pts',(18.0470291418705,-16.9495561796841,
8.64898511912869));
#175268=CARTESIAN_POINT('Ctrl Pts',(18.0513873874885,-16.9480663095785,
8.6492655770485));
#175269=CARTESIAN_POINT('Ctrl Pts',(18.0591363508056,-16.9454455327002,
8.64976218236681));
#175270=CARTESIAN_POINT('Ctrl Pts',(18.0625251001908,-16.9443089792394,
8.64997865998579));
#175271=CARTESIAN_POINT('Ctrl Pts',(18.0698013086391,-16.9418890933881,
8.65044197204889));
#175272=CARTESIAN_POINT('Ctrl Pts',(18.0736896053204,-16.9406084563625,
8.65068864705649));
#175273=CARTESIAN_POINT('Ctrl Pts',(18.0843955128988,-16.9371167830364,
8.65136539024046));
#175274=CARTESIAN_POINT('Ctrl Pts',(18.0912207481571,-16.9349290532042,
8.65179410762295));
#175275=CARTESIAN_POINT('Ctrl Pts',(18.1280704624381,-16.9233234487379,
8.65409478999922));
#175276=CARTESIAN_POINT('Ctrl Pts',(18.158292699233,-16.9145406761252,8.65593179343324));
#175277=CARTESIAN_POINT('Ctrl Pts',(18.3467774069107,-16.8642951730654,
8.66714516335542));
#175278=CARTESIAN_POINT('Ctrl Pts',(18.5092219737297,-16.8406165988855,
8.67579049982962));
#175279=CARTESIAN_POINT('Ctrl Pts',(18.7898605169018,-16.8324985983528,
8.69115899577846));
#175280=CARTESIAN_POINT('Ctrl Pts',(18.9069971206828,-16.8388333486223,
8.69769646010416));
#175281=CARTESIAN_POINT('Ctrl Pts',(19.037160292252,-16.8567703830268,8.70539387941988));
#175282=CARTESIAN_POINT('Ctrl Pts',(19.0512998106917,-16.8588650005664,
8.70623560963288));
#175283=CARTESIAN_POINT('Ctrl Pts',(19.0737683371549,-16.8624263645663,
8.70758247870083));
#175284=CARTESIAN_POINT('Ctrl Pts',(19.08211179315,-16.863800134772,8.70808467435583));
#175285=CARTESIAN_POINT('Ctrl Pts',(19.0968115300974,-16.8663110283114,
8.70897316252749));
#175286=CARTESIAN_POINT('Ctrl Pts',(19.1031712938407,-16.8674273225974,
8.70935878865232));
#175287=CARTESIAN_POINT('Ctrl Pts',(19.1163141391513,-16.8697962449153,
8.71015828837228));
#175288=CARTESIAN_POINT('Ctrl Pts',(19.1230963970159,-16.8710529630091,
8.71057228813985));
#175289=CARTESIAN_POINT('Ctrl Pts',(19.1404885970841,-16.8743636484169,
8.71163765078004));
#175290=CARTESIAN_POINT('Ctrl Pts',(19.1510890762332,-16.8764657351217,
8.71229054233705));
#175291=CARTESIAN_POINT('Ctrl Pts',(19.1952560089527,-16.8855761059651,
8.71502597897021));
#175292=CARTESIAN_POINT('Ctrl Pts',(19.2286642496198,-16.8933179264966,
8.71713184207863));
#175293=CARTESIAN_POINT('Ctrl Pts',(19.3152006939139,-16.9155993350422,
8.7226861181525));
#175294=CARTESIAN_POINT('Ctrl Pts',(19.3679729758349,-16.9314061859861,
8.72617291309199));
#175295=CARTESIAN_POINT('Ctrl Pts',(19.5235311801617,-16.9846945198407,
8.73674189068159));
#175296=CARTESIAN_POINT('Ctrl Pts',(19.6240874574687,-17.0281000056727,
8.74397246603521));
#175297=CARTESIAN_POINT('Ctrl Pts',(19.7612298217737,-17.1003593926661,
8.75421234953124));
#175298=CARTESIAN_POINT('Ctrl Pts',(19.8009293096326,-17.1229466699482,
8.75722311688506));
#175299=CARTESIAN_POINT('Ctrl Pts',(19.859354122805,-17.1587378044619,8.76169856617015));
#175300=CARTESIAN_POINT('Ctrl Pts',(19.8786461373539,-17.1709900403236,
8.76318389400198));
#175301=CARTESIAN_POINT('Ctrl Pts',(19.8983381788674,-17.1839484950669,
8.76470522952686));
#175302=CARTESIAN_POINT('Ctrl Pts',(19.8989397027039,-17.1843447711925,
8.76475170612455));
#175303=CARTESIAN_POINT('Ctrl Pts',(19.9093196853547,-17.1911905691447,
8.76555379886705));
#175304=CARTESIAN_POINT('Ctrl Pts',(19.9190448152208,-17.1977209430552,
8.7663066054662));
#175305=CARTESIAN_POINT('Ctrl Pts',(19.9615332160783,-17.2267662429557,
8.76959978061649));
#175306=CARTESIAN_POINT('Ctrl Pts',(19.993715118187,-17.2501223306543,8.77210533928319));
#175307=CARTESIAN_POINT('Ctrl Pts',(20.0310198149775,-17.2788347001436,
8.77500533300245));
#175308=CARTESIAN_POINT('Ctrl Pts',(20.036794194504,-17.2833269309374,8.77545408978137));
#175309=CARTESIAN_POINT('Ctrl Pts',(20.0461338900775,-17.2906708648774,
8.77617954991592));
#175310=CARTESIAN_POINT('Ctrl Pts',(20.0497134163073,-17.2935042816611,
8.77645749887072));
#175311=CARTESIAN_POINT('Ctrl Pts',(20.056076061162,-17.2985742726507,8.77695135128344));
#175312=CARTESIAN_POINT('Ctrl Pts',(20.0588627078105,-17.3008063246679,
8.7771675710494));
#175313=CARTESIAN_POINT('Ctrl Pts',(20.0648532866858,-17.3056295957145,
8.77763222374122));
#175314=CARTESIAN_POINT('Ctrl Pts',(20.0680552947937,-17.3082231143224,
8.77788048725601));
#175315=CARTESIAN_POINT('Ctrl Pts',(20.0769004824201,-17.3154302872363,
8.77856608325657));
#175316=CARTESIAN_POINT('Ctrl Pts',(20.0825274994277,-17.320063813374,8.7790020056961));
#175317=CARTESIAN_POINT('Ctrl Pts',(20.1136815796057,-17.3459885821679,
8.78141492372732));
#175318=CARTESIAN_POINT('Ctrl Pts',(20.1387298970722,-17.367850976131,8.78335279928629));
#175319=CARTESIAN_POINT('Ctrl Pts',(20.2828303393658,-17.4997300914263,
8.79455974396646));
#175320=CARTESIAN_POINT('Ctrl Pts',(20.3894542881583,-17.6225467322782,
8.80312847868512));
#175321=CARTESIAN_POINT('Ctrl Pts',(20.5468989136072,-17.8525951960539,
8.81839057546747));
#175322=CARTESIAN_POINT('Ctrl Pts',(20.6046989046002,-17.9541153572129,
8.82490257014341));
#175323=CARTESIAN_POINT('Ctrl Pts',(20.6598629322717,-18.0728270393192,
8.83257131875202));
#175324=CARTESIAN_POINT('Ctrl Pts',(20.6657523681689,-18.0858441815338,
8.83341267923289));
#175325=CARTESIAN_POINT('Ctrl Pts',(20.6749161555204,-18.106656905823,8.8347590671924));
#175326=CARTESIAN_POINT('Ctrl Pts',(20.678276408377,-18.1144143540516,8.83526115479853));
#175327=CARTESIAN_POINT('Ctrl Pts',(20.6841209298184,-18.1281316560446,
8.83614951711061));
#175328=CARTESIAN_POINT('Ctrl Pts',(20.6866245797609,-18.1340831716026,
8.83653512603061));
#175329=CARTESIAN_POINT('Ctrl Pts',(20.6917467853633,-18.1464169109117,
8.8373346542141));
#175330=CARTESIAN_POINT('Ctrl Pts',(20.6943614467336,-18.152800659764,8.83774869996632));
#175331=CARTESIAN_POINT('Ctrl Pts',(20.7009932277821,-18.1692206539178,
8.83881431603844));
#175332=CARTESIAN_POINT('Ctrl Pts',(20.7049647226067,-18.1792750047753,
8.83946741644684));
#175333=CARTESIAN_POINT('Ctrl Pts',(20.7212225845643,-18.2213747510842,
8.84220487724658));
#175334=CARTESIAN_POINT('Ctrl Pts',(20.7328052184087,-18.2536846434152,
8.84431259885345));
#175335=CARTESIAN_POINT('Ctrl Pts',(20.7609362091929,-18.3386006516564,
8.84987294595921));
#175336=CARTESIAN_POINT('Ctrl Pts',(20.7762227953239,-18.3915944426824,
8.85336405812305));
#175337=CARTESIAN_POINT('Ctrl Pts',(20.815622075701,-18.5513607421501,8.86394132841973));
#175338=CARTESIAN_POINT('Ctrl Pts',(20.8335432536107,-18.6594646310493,
8.8711758515804));
#175339=CARTESIAN_POINT('Ctrl Pts',(20.8474060880404,-18.8187596475218,
8.8817381523845));
#175340=CARTESIAN_POINT('Ctrl Pts',(20.8499827578842,-18.8692018768008,
8.88506646946332));
#175341=CARTESIAN_POINT('Ctrl Pts',(20.8509990984719,-18.9357845838867,
8.88940640514325));
#175342=CARTESIAN_POINT('Ctrl Pts',(20.8510612007608,-18.9518825741748,
8.89045153783671));
#175343=CARTESIAN_POINT('Ctrl Pts',(20.8505408594561,-19.0208144810576,
8.89490519603126));
#175344=CARTESIAN_POINT('Ctrl Pts',(20.8481641613965,-19.0736205240313,
8.89826291639159));
#175345=CARTESIAN_POINT('Ctrl Pts',(20.8430977553295,-19.1349514952874,
8.90205897609979));
#175346=CARTESIAN_POINT('Ctrl Pts',(20.8423285908031,-19.1436119785177,
8.90259258713674));
#175347=CARTESIAN_POINT('Ctrl Pts',(20.8410824960576,-19.156725191264,8.90339662131618));
#175348=CARTESIAN_POINT('Ctrl Pts',(20.8406447683038,-19.161181428815,8.90366916639451));
#175349=CARTESIAN_POINT('Ctrl Pts',(20.8398332862593,-19.1691816506499,
8.90415718533631));
#175350=CARTESIAN_POINT('Ctrl Pts',(20.8394647209433,-19.1727260934717,
8.9043729454267));
#175351=CARTESIAN_POINT('Ctrl Pts',(20.8386439520309,-19.1804301673681,
8.90484092401625));
#175352=CARTESIAN_POINT('Ctrl Pts',(20.8381883677766,-19.1845893802244,
8.90509294997138));
#175353=CARTESIAN_POINT('Ctrl Pts',(20.8368727698817,-19.1962796960497,
8.90579963787527));
#175354=CARTESIAN_POINT('Ctrl Pts',(20.8359846249692,-19.2038076578319,
8.90625274402571));
#175355=CARTESIAN_POINT('Ctrl Pts',(20.8304050277208,-19.2490126464546,
8.90896267933825));
#175356=CARTESIAN_POINT('Ctrl Pts',(20.8247407956105,-19.2865652127778,
8.91116818116476));
#175357=CARTESIAN_POINT('Ctrl Pts',(20.8026809969307,-19.4101690270752,
8.91833568787673));
#175358=CARTESIAN_POINT('Ctrl Pts',(20.7819557481995,-19.49535955668,8.92312944802086));
#175359=CARTESIAN_POINT('Ctrl Pts',(20.7042810264226,-19.7458418592295,
8.9373967861409));
#175360=CARTESIAN_POINT('Ctrl Pts',(20.6321156280594,-19.9055945393919,
8.94679033544867));
#175361=CARTESIAN_POINT('Ctrl Pts',(20.5291478701635,-20.0743478175533,
8.9582769002772));
#175362=CARTESIAN_POINT('Ctrl Pts',(20.5168194381478,-20.0938297985582,
8.95962749100166));
#175363=CARTESIAN_POINT('Ctrl Pts',(20.4989341961079,-20.1210969210556,
8.96155457079823));
#175364=CARTESIAN_POINT('Ctrl Pts',(20.493638762524,-20.1290521434007,8.96212131182955));
#175365=CARTESIAN_POINT('Ctrl Pts',(20.484948766516,-20.1419172420257,8.96304532225663));
#175366=CARTESIAN_POINT('Ctrl Pts',(20.4815869445198,-20.1468491520082,
8.96340135191915));
#175367=CARTESIAN_POINT('Ctrl Pts',(20.4745075487481,-20.1571410799231,
8.96414813773317));
#175368=CARTESIAN_POINT('Ctrl Pts',(20.4707859734524,-20.1624982572097,
8.96453904380131));
#175369=CARTESIAN_POINT('Ctrl Pts',(20.4618759675462,-20.1751984630982,
8.96547102512627));
#175370=CARTESIAN_POINT('Ctrl Pts',(20.4566654305012,-20.1825257616187,
8.96601294473323));
#175371=CARTESIAN_POINT('Ctrl Pts',(20.4389654320089,-20.2070835629081,
8.96784363054389));
#175372=CARTESIAN_POINT('Ctrl Pts',(20.4262631924642,-20.2241584452287,
8.96914060749162));
#175373=CARTESIAN_POINT('Ctrl Pts',(20.316513208859,-20.3671361899699,8.98021090387019));
#175374=CARTESIAN_POINT('Ctrl Pts',(20.2058436204575,-20.4819074450298,
8.99055444421387));
#175375=CARTESIAN_POINT('Ctrl Pts',(19.9816860549938,-20.667341056288,9.00977090472789));
#175376=CARTESIAN_POINT('Ctrl Pts',(19.8723136670722,-20.7417942748256,
9.01853740067588));
#175377=CARTESIAN_POINT('Ctrl Pts',(19.7428964467634,-20.8132001163442,
9.02775916370466));
#175378=CARTESIAN_POINT('Ctrl Pts',(19.7289973681852,-20.8206674890089,
9.02873539691066));
#175379=CARTESIAN_POINT('Ctrl Pts',(19.7098729082994,-20.8306683440707,
9.03005805370258));
#175380=CARTESIAN_POINT('Ctrl Pts',(19.7047190655604,-20.8333365402677,
9.03041247088327));
#175381=CARTESIAN_POINT('Ctrl Pts',(19.6965163204595,-20.8375405023389,
9.03097326549515));
#175382=CARTESIAN_POINT('Ctrl Pts',(19.6934746079729,-20.8390901224238,
9.03118050256191));
#175383=CARTESIAN_POINT('Ctrl Pts',(19.6871886278916,-20.842273428251,9.03160728263267));
#175384=CARTESIAN_POINT('Ctrl Pts',(19.6839439025983,-20.8439061223958,
9.03182675782657));
#175385=CARTESIAN_POINT('Ctrl Pts',(19.6762085905846,-20.8477734913775,
9.03234805716762));
#175386=CARTESIAN_POINT('Ctrl Pts',(19.6717141986754,-20.8500005905063,
9.03264940797466));
#175387=CARTESIAN_POINT('Ctrl Pts',(19.6565584903362,-20.8574437016793,
9.03366058426841));
#175388=CARTESIAN_POINT('Ctrl Pts',(19.6458610133971,-20.8625861339258,
9.03436597598689));
#175389=CARTESIAN_POINT('Ctrl Pts',(19.5216139043341,-20.9210322495935,
9.04246922492686));
#175390=CARTESIAN_POINT('Ctrl Pts',(19.403569002682,-20.9642400456941,9.04931465220911));
#175391=CARTESIAN_POINT('Ctrl Pts',(19.1205901345057,-21.0401319521696,
9.06523873236093));
#175392=CARTESIAN_POINT('Ctrl Pts',(18.954245119642,-21.064162901218,9.07428093662903));
#175393=CARTESIAN_POINT('Ctrl Pts',(18.763330926184,-21.0689271218655,9.08537263647293));
#175394=CARTESIAN_POINT('Ctrl Pts',(18.7398416394232,-21.0691222338113,
9.08674830842891));
#175395=CARTESIAN_POINT('Ctrl Pts',(18.7067264063761,-21.0688462061143,
9.08870510288752));
#175396=CARTESIAN_POINT('Ctrl Pts',(18.6970989597298,-21.0687002664106,
9.08927605979562));
#175397=CARTESIAN_POINT('Ctrl Pts',(18.6814925356846,-21.0683571884216,
9.09020507335883));
#175398=CARTESIAN_POINT('Ctrl Pts',(18.6755127405624,-21.0682003738174,
9.09056186313289));
#175399=CARTESIAN_POINT('Ctrl Pts',(18.6630247316007,-21.0678199161917,
9.09130873184955));
#175400=CARTESIAN_POINT('Ctrl Pts',(18.6565167329074,-21.0675915835359,
9.09169895403839));
#175401=CARTESIAN_POINT('Ctrl Pts',(18.6410870944815,-21.0669789442939,
9.09262653584781));
#175402=CARTESIAN_POINT('Ctrl Pts',(18.63216668178,-21.0665682098953,9.09316471870992));
#175403=CARTESIAN_POINT('Ctrl Pts',(18.6023559332431,-21.0650065234067,
9.09496979662281));
#175404=CARTESIAN_POINT('Ctrl Pts',(18.5814806166089,-21.0636023576063,
9.09624459292769));
#175405=CARTESIAN_POINT('Ctrl Pts',(18.4694354938249,-21.0543955936917,
9.10314691339842));
#175406=CARTESIAN_POINT('Ctrl Pts',(18.3788344572455,-21.0409986283336,
9.10894844110241));
#175407=CARTESIAN_POINT('Ctrl Pts',(18.1531878048994,-20.9925279187472,
9.12391743573088));
#175408=CARTESIAN_POINT('Ctrl Pts',(18.0202131521194,-20.9498993305473,
9.13323938819729));
#175409=CARTESIAN_POINT('Ctrl Pts',(17.8281654951898,-20.8666938525714,
9.14689238567651));
#175410=CARTESIAN_POINT('Ctrl Pts',(17.7653491741727,-20.8356948704209,
9.15138499664787));
#175411=CARTESIAN_POINT('Ctrl Pts',(17.6959956719678,-20.7970809552874,
9.15628648949651));
#175412=CARTESIAN_POINT('Ctrl Pts',(17.6878429362671,-20.7924706251381,
9.15686170508571));
#175413=CARTESIAN_POINT('Ctrl Pts',(17.6757709390881,-20.7855378377513,
9.15771168739144));
#175414=CARTESIAN_POINT('Ctrl Pts',(17.671828271653,-20.7832566636659,9.15798900771693));
#175415=CARTESIAN_POINT('Ctrl Pts',(17.6649129401629,-20.7792256993459,
9.15847488380465));
#175416=CARTESIAN_POINT('Ctrl Pts',(17.6619371654353,-20.7774813549325,
9.15868378663543));
#175417=CARTESIAN_POINT('Ctrl Pts',(17.6555274277038,-20.7737030052578,
9.1591333667015));
#175418=CARTESIAN_POINT('Ctrl Pts',(17.652094958916,-20.7716665659519,9.15937388243075));
#175419=CARTESIAN_POINT('Ctrl Pts',(17.6450113625614,-20.7674368312581,
9.15986978594795));
#175420=CARTESIAN_POINT('Ctrl Pts',(17.6413610502791,-20.7652421975629,
9.16012508641768));
#175421=CARTESIAN_POINT('Ctrl Pts',(17.6321699391551,-20.759678502172,9.1607673446987));
#175422=CARTESIAN_POINT('Ctrl Pts',(17.6266379070732,-20.7562949447757,
9.16115339571808));
#175423=CARTESIAN_POINT('Ctrl Pts',(17.6108813636068,-20.7465580042894,
9.16225173783336));
#175424=CARTESIAN_POINT('Ctrl Pts',(17.6006952046886,-20.740142655728,9.16296030543165));
#175425=CARTESIAN_POINT('Ctrl Pts',(17.5664517758317,-20.7181656271403,
9.16533926958006));
#175426=CARTESIAN_POINT('Ctrl Pts',(17.542654945412,-20.702201987201,9.1669873235692));
#175427=CARTESIAN_POINT('Ctrl Pts',(17.4296327733063,-20.6230095455563,
9.17482668618842));
#175428=CARTESIAN_POINT('Ctrl Pts',(17.3450663812284,-20.5534099958714,
9.18073558902244));
#175429=CARTESIAN_POINT('Ctrl Pts',(17.1610092087018,-20.3763303474538,
9.19460722556702));
#175430=CARTESIAN_POINT('Ctrl Pts',(17.0665396363283,-20.2644733542615,
9.20257816518851));
#175431=CARTESIAN_POINT('Ctrl Pts',(16.9708097368195,-20.1239327853639,
9.21244913664345));
#175432=CARTESIAN_POINT('Ctrl Pts',(16.9576222347561,-20.1038456161284,
9.21385587400786));
#175433=CARTESIAN_POINT('Ctrl Pts',(16.9395851049211,-20.0753248156304,
9.2158495496874));
#175434=CARTESIAN_POINT('Ctrl Pts',(16.9344470335754,-20.0670751424633,
9.21642579402243));
#175435=CARTESIAN_POINT('Ctrl Pts',(16.9262299301674,-20.0536770655229,
9.21736109271528));
#175436=CARTESIAN_POINT('Ctrl Pts',(16.9231156186708,-20.0485503811497,
9.21771884587233));
#175437=CARTESIAN_POINT('Ctrl Pts',(16.9166725990919,-20.03784177286,9.21846587846381));
#175438=CARTESIAN_POINT('Ctrl Pts',(16.9133477267191,-20.0322576248815,
9.21885529296861));
#175439=CARTESIAN_POINT('Ctrl Pts',(16.9055529058073,-20.019027955422,9.21977759822382));
#175440=CARTESIAN_POINT('Ctrl Pts',(16.9011051428366,-20.0113695638317,
9.22031128696624));
#175441=CARTESIAN_POINT('Ctrl Pts',(16.8865236913145,-19.9858957240665,
9.22208590464507));
#175442=CARTESIAN_POINT('Ctrl Pts',(16.8766009171385,-19.9679614559711,
9.22333437484109));
#175443=CARTESIAN_POINT('Ctrl Pts',(16.8254384926348,-19.8722358350156,
9.22999540829818));
#175444=CARTESIAN_POINT('Ctrl Pts',(16.7888263458494,-19.7920815953588,
9.2355686450241));
#175445=CARTESIAN_POINT('Ctrl Pts',(16.6888399781642,-19.5313024798964,
9.25364997506636));
#175446=CARTESIAN_POINT('Ctrl Pts',(16.6448890658211,-19.3442761693131,
9.2666242487563));
#175447=CARTESIAN_POINT('Ctrl Pts',(16.6241532271979,-19.1278429736965,
9.28035986942869));
#175448=CARTESIAN_POINT('Ctrl Pts',(16.6221401954527,-19.1017413330554,
9.2819938706623));
#175449=CARTESIAN_POINT('Ctrl Pts',(16.6202046990401,-19.0686491058861,
9.28403145854135));
#175450=CARTESIAN_POINT('Ctrl Pts',(16.6198320670926,-19.0616883897599,
9.28445814625456));
#175451=CARTESIAN_POINT('Ctrl Pts',(16.6192953239925,-19.0506400838953,
9.28513224348439));
#175452=CARTESIAN_POINT('Ctrl Pts',(16.6191086720229,-19.0465537116183,
9.28538088288105));
#175453=CARTESIAN_POINT('Ctrl Pts',(16.6187836663981,-19.0389552499614,
9.28584191301783));
#175454=CARTESIAN_POINT('Ctrl Pts',(16.6186422162471,-19.0354433961295,
9.28605446952001));
#175455=CARTESIAN_POINT('Ctrl Pts',(16.6183781735518,-19.0284551322572,
9.28647641291076));
#175456=CARTESIAN_POINT('Ctrl Pts',(16.6182554037863,-19.0249787899557,
9.28668580824344));
#175457=CARTESIAN_POINT('Ctrl Pts',(16.6179937476281,-19.017013171257,9.28716449377872));
#175458=CARTESIAN_POINT('Ctrl Pts',(16.6178605777674,-19.0125237062291,
9.28743346964533));
#175459=CARTESIAN_POINT('Ctrl Pts',(16.6175253051032,-18.9998612865493,
9.28818989902979));
#175460=CARTESIAN_POINT('Ctrl Pts',(16.6173562536645,-18.991687437871,9.28867559344325));
#175461=CARTESIAN_POINT('Ctrl Pts',(16.617081385903,-18.9732240527242,9.28976724482838));
#175462=CARTESIAN_POINT('Ctrl Pts',(16.6170032290319,-18.9629342723496,
9.29037180646726));
#175463=CARTESIAN_POINT('Ctrl Pts',(16.6170000979997,-18.9526441512856,
9.29097292592683));
#175464=CARTESIAN_POINT('Ctrl Pts',(16.6170000985829,-18.9526460648981,
9.29097281413902));
#175465=CARTESIAN_POINT('Ctrl Pts',(16.6169387608845,-18.7516571212849,
9.30271402210781));
#175466=CARTESIAN_POINT('Ctrl Pts',(16.6454993572956,-18.5516397308117,
9.31315827170977));
#175467=CARTESIAN_POINT('Ctrl Pts',(16.7149206738938,-18.3138947250748,
9.32683236820389));
#175468=CARTESIAN_POINT('Ctrl Pts',(16.7294486235981,-18.2696284571598,
9.32943042288601));
#175469=CARTESIAN_POINT('Ctrl Pts',(16.7454193880554,-18.2258897123729,
9.33206801777758));
#175470=CARTESIAN_POINT('Origin',(18.734,-18.952,0.));
#175471=CARTESIAN_POINT('',(16.7454193692319,-18.2258897639242,10.3555828645479));
#175472=CARTESIAN_POINT('',(16.7454193829761,-18.2258897262833,10.1325348909312));
#175473=CARTESIAN_POINT('',(16.7454193692319,-18.2258897639242,0.));
#175474=CARTESIAN_POINT('',(16.6146463628246,-18.9530771010625,10.3109437268626));
#175475=CARTESIAN_POINT('Ctrl Pts',(16.6170002731508,-18.9530754163976,
10.3109437563772));
#175476=CARTESIAN_POINT('Ctrl Pts',(16.6169638477093,-18.8813704936142,
10.3152783077143));
#175477=CARTESIAN_POINT('Ctrl Pts',(16.6205747319161,-18.8095176190282,
10.3196128590514));
#175478=CARTESIAN_POINT('Ctrl Pts',(16.6278517403648,-18.7379240591854,
10.3239474103886));
#175479=CARTESIAN_POINT('Ctrl Pts',(16.6351199717668,-18.6664168507633,
10.3282767336763));
#175480=CARTESIAN_POINT('Ctrl Pts',(16.6460455147318,-18.5951688250439,
10.3326060569641));
#175481=CARTESIAN_POINT('Ctrl Pts',(16.6605951836021,-18.5245874740512,
10.3369353802518));
#175482=CARTESIAN_POINT('Ctrl Pts',(16.675130891217,-18.454073849979,10.3412605493015));
#175483=CARTESIAN_POINT('Ctrl Pts',(16.6932837245189,-18.384226113485,10.3455857183512));
#175484=CARTESIAN_POINT('Ctrl Pts',(16.7149688972722,-18.3154448914527,
10.3499108874009));
#175485=CARTESIAN_POINT('Ctrl Pts',(16.7244481263206,-18.2853785892241,
10.3518015464499));
#175486=CARTESIAN_POINT('Ctrl Pts',(16.7346016608924,-18.2555159614414,
10.3536922054989));
#175487=CARTESIAN_POINT('Ctrl Pts',(16.7454193692319,-18.2258897639242,
10.3555828645479));
#175488=CARTESIAN_POINT('Ctrl Pts',(16.7437494325541,-18.2252642451362,
9.55561791118868));
#175489=CARTESIAN_POINT('Ctrl Pts',(16.9543732025563,-17.6645819652671,
9.5917275247594));
#175490=CARTESIAN_POINT('Ctrl Pts',(17.9482900541193,-16.6327269270279,
9.67022907389064));
#175491=CARTESIAN_POINT('Ctrl Pts',(20.2082247500812,-16.9288855714836,
9.79112255858232));
#175492=CARTESIAN_POINT('Ctrl Pts',(21.2330889659179,-19.0965162449377,
9.91829836526374));
#175493=CARTESIAN_POINT('Ctrl Pts',(19.9651941664792,-21.1315622333512,
10.0454741719452));
#175494=CARTESIAN_POINT('Ctrl Pts',(17.5677551358241,-21.1669951515536,
10.1726499786266));
#175495=CARTESIAN_POINT('Ctrl Pts',(16.6440836935421,-19.7776853836357,
10.2611398283041));
#175496=CARTESIAN_POINT('Ctrl Pts',(16.6137958948767,-19.014466075178,10.307237742421));
#175497=CARTESIAN_POINT('Ctrl Pts',(16.614176999282,-18.9530774369802,10.3109437209775));
#175498=CARTESIAN_POINT('Ctrl Pts',(16.7454193880554,-18.2258897123729,
9.33206801777758));
#175499=CARTESIAN_POINT('Ctrl Pts',(16.7596276849878,-18.1869777945967,
9.33441453860362));
#175500=CARTESIAN_POINT('Ctrl Pts',(16.7749779213659,-18.1484833900871,
9.33679229479106));
#175501=CARTESIAN_POINT('Ctrl Pts',(16.799599094585,-18.0916499580595,9.34040226076874));
#175502=CARTESIAN_POINT('Ctrl Pts',(16.8080187823558,-18.0729633890997,
9.34160562443898));
#175503=CARTESIAN_POINT('Ctrl Pts',(16.8204632264257,-18.0463817313513,
9.34334229753595));
#175504=CARTESIAN_POINT('Ctrl Pts',(16.8242684619941,-18.0383847191264,
9.34386803505926));
#175505=CARTESIAN_POINT('Ctrl Pts',(16.8309529325593,-18.0245610010983,
9.34478260677337));
#175506=CARTESIAN_POINT('Ctrl Pts',(16.8338090477498,-18.0187232023072,
9.34517063272239));
#175507=CARTESIAN_POINT('Ctrl Pts',(16.8393529215622,-18.0075226680877,
9.34591861534346));
#175508=CARTESIAN_POINT('Ctrl Pts',(16.842036684437,-18.0021580164354,9.3462784293009));
#175509=CARTESIAN_POINT('Ctrl Pts',(16.8491284318565,-17.9881314244748,
9.34722333745082));
#175510=CARTESIAN_POINT('Ctrl Pts',(16.8535732922065,-17.9794883800337,
9.34780972450416));
#175511=CARTESIAN_POINT('Ctrl Pts',(16.8692136776856,-17.9495837374694,
9.34985322993656));
#175512=CARTESIAN_POINT('Ctrl Pts',(16.8807112371142,-17.9284829859791,
9.35132099652751));
#175513=CARTESIAN_POINT('Ctrl Pts',(16.9645626868343,-17.7806426021488,
9.36179322854543));
#175514=CARTESIAN_POINT('Ctrl Pts',(17.0494805740375,-17.6615090250345,
9.37126514852381));
#175515=CARTESIAN_POINT('Ctrl Pts',(17.2364663648891,-17.4493967086943,
9.38992675272336));
#175516=CARTESIAN_POINT('Ctrl Pts',(17.3367292888721,-17.3557344181346,
9.39904432072308));
#175517=CARTESIAN_POINT('Ctrl Pts',(17.4554185362512,-17.2646708028595,
9.40841263101319));
#175518=CARTESIAN_POINT('Ctrl Pts',(17.465566973191,-17.2570285983539,9.40920310389339));
#175519=CARTESIAN_POINT('Ctrl Pts',(17.4812017559145,-17.2454740126953,
9.4104040915905));
#175520=CARTESIAN_POINT('Ctrl Pts',(17.4866388264741,-17.2414958371181,
9.41081866996757));
#175521=CARTESIAN_POINT('Ctrl Pts',(17.495628865917,-17.2349836993859,9.41149899437401));
#175522=CARTESIAN_POINT('Ctrl Pts',(17.4991707986244,-17.2324346809424,
9.4117657198194));
#175523=CARTESIAN_POINT('Ctrl Pts',(17.5060325439406,-17.2275286308589,
9.41227987360158));
#175524=CARTESIAN_POINT('Ctrl Pts',(17.5093513209997,-17.2251701908422,
9.41252739622004));
#175525=CARTESIAN_POINT('Ctrl Pts',(17.5126866069157,-17.2228144703318,
9.41277497694871));
#175526=CARTESIAN_POINT('Ctrl Pts',(17.5126963004708,-17.2228076238726,
9.41277569649852));
#175527=CARTESIAN_POINT('Ctrl Pts',(17.5127157223261,-17.2227939066588,
9.41277713815739));
#175528=CARTESIAN_POINT('Ctrl Pts',(17.5127254500437,-17.2227870363166,
9.41277786022313));
#175529=CARTESIAN_POINT('Ctrl Pts',(17.512744940083,-17.2227732714389,9.41277930690319));
#175530=CARTESIAN_POINT('Ctrl Pts',(17.5127547027751,-17.2227663766429,
9.41278003154492));
#175531=CARTESIAN_POINT('Ctrl Pts',(17.5127748948248,-17.2227521164816,
9.41278153029124));
#175532=CARTESIAN_POINT('Ctrl Pts',(17.5127853244933,-17.2227447509144,
9.41278230441747));
#175533=CARTESIAN_POINT('Ctrl Pts',(17.512806352193,-17.2227299011652,9.41278386514324));
#175534=CARTESIAN_POINT('Ctrl Pts',(17.5128169496939,-17.2227224173622,
9.41278465170306));
#175535=CARTESIAN_POINT('Ctrl Pts',(17.5128383163199,-17.2227073288522,
9.41278623753695));
#175536=CARTESIAN_POINT('Ctrl Pts',(17.5128490858015,-17.2226997238982,
9.41278703683709));
#175537=CARTESIAN_POINT('Ctrl Pts',(17.512870800011,-17.2226843905424,9.4127886484193));
#175538=CARTESIAN_POINT('Ctrl Pts',(17.5128817447291,-17.2226766621526,
9.41278946070024));
#175539=CARTESIAN_POINT('Ctrl Pts',(17.5129038132836,-17.2226610792063,
9.4127910985302));
#175540=CARTESIAN_POINT('Ctrl Pts',(17.5129149371519,-17.2226532246323,
9.41279192408116));
#175541=CARTESIAN_POINT('Ctrl Pts',(17.5129373680329,-17.2226373864903,
9.4127935887487));
#175542=CARTESIAN_POINT('Ctrl Pts',(17.5129486748447,-17.2226294030694,
9.41279442784993));
#175543=CARTESIAN_POINT('Ctrl Pts',(17.5129714756278,-17.2226133044147,
9.41279611991465));
#175544=CARTESIAN_POINT('Ctrl Pts',(17.5129829694858,-17.2226051892664,
9.4127969728693));
#175545=CARTESIAN_POINT('Ctrl Pts',(17.5130061483692,-17.2225888243439,
9.41279869293691));
#175546=CARTESIAN_POINT('Ctrl Pts',(17.5130178333919,-17.2225805745772,
9.41279956004922));
#175547=CARTESIAN_POINT('Ctrl Pts',(17.5130413986242,-17.2225639375976,
9.41280130872903));
#175548=CARTESIAN_POINT('Ctrl Pts',(17.5130532790921,-17.2225555502082,
9.41280219031522));
#175549=CARTESIAN_POINT('Ctrl Pts',(17.5130772396492,-17.2225386348704,
9.41280396827037));
#175550=CARTESIAN_POINT('Ctrl Pts',(17.5130893197452,-17.2225301069234,
9.41280486463933));
#175551=CARTESIAN_POINT('Ctrl Pts',(17.5131136840949,-17.2225129072868,
9.41280667249513));
#175552=CARTESIAN_POINT('Ctrl Pts',(17.5131259683995,-17.2225042355676,
9.41280758398522));
#175553=CARTESIAN_POINT('Ctrl Pts',(17.5131507459074,-17.2224867450594,
9.41280942243346));
#175554=CARTESIAN_POINT('Ctrl Pts',(17.5131632389502,-17.2224779263902,
9.41281034937916));
#175555=CARTESIAN_POINT('Ctrl Pts',(17.5131884386196,-17.2224601386953,
9.41281221908457));
#175556=CARTESIAN_POINT('Ctrl Pts',(17.513201145293,-17.2224511696434,9.41281316184721));
#175557=CARTESIAN_POINT('Ctrl Pts',(17.5132267769499,-17.2224330778677,
9.41281506353545));
#175558=CARTESIAN_POINT('Ctrl Pts',(17.5132397021304,-17.2224239550122,
9.41281602247508));
#175559=CARTESIAN_POINT('Ctrl Pts',(17.5132657758111,-17.2224055521155,
9.41281795688722));
#175560=CARTESIAN_POINT('Ctrl Pts',(17.5132789244848,-17.2223962719594,
9.41281893237198));
#175561=CARTESIAN_POINT('Ctrl Pts',(17.5161294850279,-17.2203844335687,
9.41303040817569));
#175562=CARTESIAN_POINT('Ctrl Pts',(17.5189717797181,-17.2183888886933,
9.41324041720716));
#175563=CARTESIAN_POINT('Ctrl Pts',(17.525590943879,-17.2137659189939,9.41372752539437));
#175564=CARTESIAN_POINT('Ctrl Pts',(17.5293714723193,-17.2111438087823,
9.41400426053556));
#175565=CARTESIAN_POINT('Ctrl Pts',(17.5410657491037,-17.2030891929109,
9.41485583718684));
#175566=CARTESIAN_POINT('Ctrl Pts',(17.5490080471362,-17.1976980825398,
9.41542793908332));
#175567=CARTESIAN_POINT('Ctrl Pts',(17.6515166969557,-17.1291305937148,
9.42273564472652));
#175568=CARTESIAN_POINT('Ctrl Pts',(17.7510022998792,-17.0736108423631,
9.4290038457494));
#175569=CARTESIAN_POINT('Ctrl Pts',(17.9581854581276,-16.9789821990892,
9.44141734454648));
#175570=CARTESIAN_POINT('Ctrl Pts',(18.0655443869056,-16.9400721317457,
9.4475464669605));
#175571=CARTESIAN_POINT('Ctrl Pts',(18.2286276583947,-16.8954689386177,
9.45694786152188));
#175572=CARTESIAN_POINT('Ctrl Pts',(18.2822857600101,-16.8830208286609,
9.4600529683545));
#175573=CARTESIAN_POINT('Ctrl Pts',(18.3700426733623,-16.8662388210013,
9.46519334628232));
#175574=CARTESIAN_POINT('Ctrl Pts',(18.4038698619593,-16.860618034139,9.46718930263892));
#175575=CARTESIAN_POINT('Ctrl Pts',(18.4485175927613,-16.8543094656963,
9.46984862841864));
#175576=CARTESIAN_POINT('Ctrl Pts',(18.4592291698385,-16.8528795253993,
9.4704884993312));
#175577=CARTESIAN_POINT('Ctrl Pts',(18.4767948791167,-16.8506713480323,
9.47154104010516));
#175578=CARTESIAN_POINT('Ctrl Pts',(18.4836427812187,-16.8498444779081,
9.47195216963619));
#175579=CARTESIAN_POINT('Ctrl Pts',(18.4969087207802,-16.8483083831865,
9.47275022105392));
#175580=CARTESIAN_POINT('Ctrl Pts',(18.5033262097073,-16.8475950260531,
9.47313700777826));
#175581=CARTESIAN_POINT('Ctrl Pts',(18.5181552073712,-16.8460153065518,
9.4740324762627));
#175582=CARTESIAN_POINT('Ctrl Pts',(18.5265688017917,-16.845169964541,9.47454181456681));
#175583=CARTESIAN_POINT('Ctrl Pts',(18.5492181256979,-16.8430312981077,
9.47591646886654));
#175584=CARTESIAN_POINT('Ctrl Pts',(18.5634620726007,-16.8418317303546,
9.47678471522296));
#175585=CARTESIAN_POINT('Ctrl Pts',(18.6945796772711,-16.8321257573915,
9.4848126999604));
#175586=CARTESIAN_POINT('Ctrl Pts',(18.8119397005935,-16.8331941337924,
9.49227603027375));
#175587=CARTESIAN_POINT('Ctrl Pts',(19.0917049283942,-16.8590192387907,
9.51063007243621));
#175588=CARTESIAN_POINT('Ctrl Pts',(19.2525142793748,-16.8929554484554,
9.52166370538066));
#175589=CARTESIAN_POINT('Ctrl Pts',(19.437425977985,-16.955037959666,9.53404313472439));
#175590=CARTESIAN_POINT('Ctrl Pts',(19.4668278890122,-16.965639251686,9.53599994777887));
#175591=CARTESIAN_POINT('Ctrl Pts',(19.5026583171494,-16.979462411726,9.53836109540091));
#175592=CARTESIAN_POINT('Ctrl Pts',(19.509317636307,-16.9820703789543,9.5387989181054));
#175593=CARTESIAN_POINT('Ctrl Pts',(19.5197647541113,-16.9862229318375,
9.53948403360274));
#175594=CARTESIAN_POINT('Ctrl Pts',(19.5235614386363,-16.9877448063477,
9.53973265515284));
#175595=CARTESIAN_POINT('Ctrl Pts',(19.5306680435971,-16.990617373441,9.54019730998764));
#175596=CARTESIAN_POINT('Ctrl Pts',(19.5339789155852,-16.9919654303331,
9.54041349149122));
#175597=CARTESIAN_POINT('Ctrl Pts',(19.5415527401777,-16.9950715816339,
9.54090736211619));
#175598=CARTESIAN_POINT('Ctrl Pts',(19.5458133664464,-16.9968352187708,
9.54118471203861));
#175599=CARTESIAN_POINT('Ctrl Pts',(19.5589743308678,-17.0023334860903,
9.54204006799652));
#175600=CARTESIAN_POINT('Ctrl Pts',(19.5678550600484,-17.0061151347389,
9.54261529912772));
#175601=CARTESIAN_POINT('Ctrl Pts',(19.6762368192341,-17.0531451917887,
9.54961529955773));
#175602=CARTESIAN_POINT('Ctrl Pts',(19.772311207705,-17.1039263668871,9.55561523347598));
#175603=CARTESIAN_POINT('Ctrl Pts',(19.9635525619985,-17.2246529631629,
9.5679577273629));
#175604=CARTESIAN_POINT('Ctrl Pts',(20.0576162106425,-17.2956284133548,
9.57427145519332));
#175605=CARTESIAN_POINT('Ctrl Pts',(20.2026253366148,-17.4253225178517,
9.58508081897925));
#175606=CARTESIAN_POINT('Ctrl Pts',(20.2571115128213,-17.4796773391617,
9.5894377876174));
#175607=CARTESIAN_POINT('Ctrl Pts',(20.3212568871287,-17.5510475246551,
9.59503928573504));
#175608=CARTESIAN_POINT('Ctrl Pts',(20.3338050359408,-17.5653940445243,
9.59615951109523));
#175609=CARTESIAN_POINT('Ctrl Pts',(20.3517317035072,-17.5864572127967,
9.59779691111755));
#175610=CARTESIAN_POINT('Ctrl Pts',(20.3572659078999,-17.5930405608937,
9.59830767244357));
#175611=CARTESIAN_POINT('Ctrl Pts',(20.3668841974132,-17.6046248168695,
9.59920475171686));
#175612=CARTESIAN_POINT('Ctrl Pts',(20.3709858310344,-17.6096110571651,
9.59959034826484));
#175613=CARTESIAN_POINT('Ctrl Pts',(20.3788956225875,-17.6193169292136,
9.60033992786648));
#175614=CARTESIAN_POINT('Ctrl Pts',(20.3827064404254,-17.6240343195407,
9.60070379805627));
#175615=CARTESIAN_POINT('Ctrl Pts',(20.3917517061395,-17.6353303533347,
9.60157406586847));
#175616=CARTESIAN_POINT('Ctrl Pts',(20.3969673088234,-17.6419238937171,
9.60208121175134));
#175617=CARTESIAN_POINT('Ctrl Pts',(20.4155535289775,-17.6657103371306,
9.60390790801144));
#175618=CARTESIAN_POINT('Ctrl Pts',(20.4286975572695,-17.683077819019,9.60523636842149));
#175619=CARTESIAN_POINT('Ctrl Pts',(20.5531443718273,-17.8528950794568,
9.61817956209638));
#175620=CARTESIAN_POINT('Ctrl Pts',(20.6438341549979,-18.0193573318385,
9.63062523874681));
#175621=CARTESIAN_POINT('Ctrl Pts',(20.7391536177478,-18.2685188771991,
9.64823217801498));
#175622=CARTESIAN_POINT('Ctrl Pts',(20.7630014530789,-18.3429497318971,
9.65335810412934));
#175623=CARTESIAN_POINT('Ctrl Pts',(20.7916212284576,-18.4528586818725,
9.66059443667281));
#175624=CARTESIAN_POINT('Ctrl Pts',(20.7996960862217,-18.4874064167957,
9.6628221232846));
#175625=CARTESIAN_POINT('Ctrl Pts',(20.8084084945525,-18.5294202636081,
9.66546171145211));
#175626=CARTESIAN_POINT('Ctrl Pts',(20.8098792731637,-18.536705546754,9.66591690937895));
#175627=CARTESIAN_POINT('Ctrl Pts',(20.8121118488182,-18.5480725540374,
9.6666230683348));
#175628=CARTESIAN_POINT('Ctrl Pts',(20.812900039275,-18.5521489462482,9.66687549378249));
#175629=CARTESIAN_POINT('Ctrl Pts',(20.8143430189101,-18.5597314128401,
9.66734348113989));
#175630=CARTESIAN_POINT('Ctrl Pts',(20.815000933894,-18.5632367890323,9.66755921409265));
#175631=CARTESIAN_POINT('Ctrl Pts',(20.8164726651625,-18.5711889780945,
9.66804723326561));
#175632=CARTESIAN_POINT('Ctrl Pts',(20.8172810968247,-18.5756367339425,
9.66831921076136));
#175633=CARTESIAN_POINT('Ctrl Pts',(20.8196378665154,-18.5888432813987,
9.66912397475711));
#175634=CARTESIAN_POINT('Ctrl Pts',(20.8211452811711,-18.5976094046622,
9.66965449267586));
#175635=CARTESIAN_POINT('Ctrl Pts',(20.8320582462934,-18.6635578936841,
9.67361991007654));
#175636=CARTESIAN_POINT('Ctrl Pts',(20.8391684225418,-18.7211007988519,
9.67693496138901));
#175637=CARTESIAN_POINT('Ctrl Pts',(20.857158271779,-18.9403378880945,9.68926003309523));
#175638=CARTESIAN_POINT('Ctrl Pts',(20.8518296659783,-19.1028006017573,
9.69780683165734));
#175639=CARTESIAN_POINT('Ctrl Pts',(20.8190932103625,-19.3231690468967,
9.71014097930096));
#175640=CARTESIAN_POINT('Ctrl Pts',(20.8075836130097,-19.3828483879239,
9.71355275612229));
#175641=CARTESIAN_POINT('Ctrl Pts',(20.7850065449133,-19.4777525340239,
9.71915322129601));
#175642=CARTESIAN_POINT('Ctrl Pts',(20.7755568386602,-19.5133278968979,
9.72129270112995));
#175643=CARTESIAN_POINT('Ctrl Pts',(20.7620605955166,-19.5592743434434,
9.72411575837883));
#175644=CARTESIAN_POINT('Ctrl Pts',(20.75885264916,-19.5698864373096,9.72477198317596));
#175645=CARTESIAN_POINT('Ctrl Pts',(20.7534955477933,-19.5871182282838,
9.72584458650863));
#175646=CARTESIAN_POINT('Ctrl Pts',(20.7513968153266,-19.5937534722835,
9.72625930788545));
#175647=CARTESIAN_POINT('Ctrl Pts',(20.747294749064,-19.6065033649665,9.72705955127081));
#175648=CARTESIAN_POINT('Ctrl Pts',(20.745296176942,-19.6126194733447,9.7274449126698));
#175649=CARTESIAN_POINT('Ctrl Pts',(20.7406517755257,-19.62661600391,9.72833025288092));
#175650=CARTESIAN_POINT('Ctrl Pts',(20.7379873633738,-19.6344901063839,
9.72883084148726));
#175651=CARTESIAN_POINT('Ctrl Pts',(20.7307755624286,-19.6553966698757,
9.73016676218824));
#175652=CARTESIAN_POINT('Ctrl Pts',(20.7261470296075,-19.6684005305464,
9.73100477326359));
#175653=CARTESIAN_POINT('Ctrl Pts',(20.6892292403148,-19.7689960043559,
9.73754353809784));
#175654=CARTESIAN_POINT('Ctrl Pts',(20.6513096232959,-19.8543987811313,
9.7434332824999));
#175655=CARTESIAN_POINT('Ctrl Pts',(20.5249511349982,-20.0947827722979,
9.76099378517052));
#175656=CARTESIAN_POINT('Ctrl Pts',(20.4224349717483,-20.241433728627,9.77303670911449));
#175657=CARTESIAN_POINT('Ctrl Pts',(20.2755389873639,-20.4035476333015,
9.78703587150884));
#175658=CARTESIAN_POINT('Ctrl Pts',(20.2474538429422,-20.4328075309318,
9.78959089361936));
#175659=CARTESIAN_POINT('Ctrl Pts',(20.213039365163,-20.4666587616583,9.79256230445));
#175660=CARTESIAN_POINT('Ctrl Pts',(20.2075055322638,-20.4720427818222,
9.79303538636506));
#175661=CARTESIAN_POINT('Ctrl Pts',(20.1989055518307,-20.480318843031,9.79376315314813));
#175662=CARTESIAN_POINT('Ctrl Pts',(20.1958600814827,-20.4832321393666,
9.79401944785775));
#175663=CARTESIAN_POINT('Ctrl Pts',(20.1902250503846,-20.4885904744419,
9.79449101119004));
#175664=CARTESIAN_POINT('Ctrl Pts',(20.187638039065,-20.4910380551589,9.79470647361805));
#175665=CARTESIAN_POINT('Ctrl Pts',(20.1818122150451,-20.4965220940686,
9.79518938685155));
#175666=CARTESIAN_POINT('Ctrl Pts',(20.1785700305081,-20.4995548897806,
9.7954565563493));
#175667=CARTESIAN_POINT('Ctrl Pts',(20.1702614301382,-20.5072780366454,
9.79613726570796));
#175668=CARTESIAN_POINT('Ctrl Pts',(20.1651815215219,-20.5119538847005,
9.79654972254341));
#175669=CARTESIAN_POINT('Ctrl Pts',(20.1355914857509,-20.5389240942688,
9.79893134219442));
#175670=CARTESIAN_POINT('Ctrl Pts',(20.1105820799534,-20.560666784958,9.80086164003915));
#175671=CARTESIAN_POINT('Ctrl Pts',(20.0710469395953,-20.5934403161374,
9.80380627737103));
#175672=CARTESIAN_POINT('Ctrl Pts',(20.0568729890853,-20.604884726693,9.80484155601451));
#175673=CARTESIAN_POINT('Ctrl Pts',(20.0413800411324,-20.6170671618631,
9.80595343800128));
#175674=CARTESIAN_POINT('Ctrl Pts',(20.040206381039,-20.6179880298538,9.80603754692448));
#175675=CARTESIAN_POINT('Ctrl Pts',(20.0209856109252,-20.6330360830935,
9.80741301737463));
#175676=CARTESIAN_POINT('Ctrl Pts',(20.0027107691817,-20.6468708836604,
9.8086925189548));
#175677=CARTESIAN_POINT('Ctrl Pts',(19.9473564856489,-20.6873792305149,
9.81249592546884));
#175678=CARTESIAN_POINT('Ctrl Pts',(19.9096342252567,-20.7131528723076,
9.8149933681089));
#175679=CARTESIAN_POINT('Ctrl Pts',(19.7788703607878,-20.7964219471259,
9.82343360672363));
#175680=CARTESIAN_POINT('Ctrl Pts',(19.6822226017222,-20.8479217820874,
9.82932170052626));
#175681=CARTESIAN_POINT('Ctrl Pts',(19.5315380753926,-20.913799976287,9.83846604524153));
#175682=CARTESIAN_POINT('Ctrl Pts',(19.4802031270367,-20.9338946431348,
9.84157356654434));
#175683=CARTESIAN_POINT('Ctrl Pts',(19.3957342438674,-20.9632120244641,
9.84671758500308));
#175684=CARTESIAN_POINT('Ctrl Pts',(19.363056050306,-20.973671166593,9.84871469434997));
#175685=CARTESIAN_POINT('Ctrl Pts',(19.319767937305,-20.9863750284397,9.85137533855444));
#175686=CARTESIAN_POINT('Ctrl Pts',(19.3093734142952,-20.9893392599853,
9.85201534514958));
#175687=CARTESIAN_POINT('Ctrl Pts',(19.2923087886658,-20.9940646124243,
9.85306805225241));
#175688=CARTESIAN_POINT('Ctrl Pts',(19.2856518901842,-20.9958729841019,
9.85347921147363));
#175689=CARTESIAN_POINT('Ctrl Pts',(19.2727471210776,-20.9993109754522,
9.85427727988268));
#175690=CARTESIAN_POINT('Ctrl Pts',(19.2665003924563,-21.0009446115689,
9.85466405369288));
#175691=CARTESIAN_POINT('Ctrl Pts',(19.2520570035944,-21.004651315581,9.85555943306801));
#175692=CARTESIAN_POINT('Ctrl Pts',(19.2438552437113,-21.0067038982662,
9.85606869476603));
#175693=CARTESIAN_POINT('Ctrl Pts',(19.2217585237242,-21.0120934021167,
9.85744300828095));
#175694=CARTESIAN_POINT('Ctrl Pts',(19.2078418939486,-21.0153388104556,
9.85831098819905));
#175695=CARTESIAN_POINT('Ctrl Pts',(19.0798345003788,-21.0438272797968,
9.86631834025349));
#175696=CARTESIAN_POINT('Ctrl Pts',(18.9638883005151,-21.0597206722713,
9.87375949716051));
#175697=CARTESIAN_POINT('Ctrl Pts',(18.6847491590449,-21.0746733430815,
9.89201886092508));
#175698=CARTESIAN_POINT('Ctrl Pts',(18.5218018231455,-21.0646144403409,
9.90297712326021));
#175699=CARTESIAN_POINT('Ctrl Pts',(18.3296136859093,-21.0302727317604,
9.91538262508376));
#175700=CARTESIAN_POINT('Ctrl Pts',(18.2977453968435,-21.0238175663966,
9.91742015007815));
#175701=CARTESIAN_POINT('Ctrl Pts',(18.2589759004651,-21.0150301786804,
9.91986466572181));
#175702=CARTESIAN_POINT('Ctrl Pts',(18.2519234288635,-21.013393605388,9.92030794431918));
#175703=CARTESIAN_POINT('Ctrl Pts',(18.2408808805105,-21.0107713383333,
9.92099967250386));
#175704=CARTESIAN_POINT('Ctrl Pts',(18.236885119741,-21.0098101676388,9.92124949285123));
#175705=CARTESIAN_POINT('Ctrl Pts',(18.2294217708606,-21.0079918698817,
9.92171517610271));
#175706=CARTESIAN_POINT('Ctrl Pts',(18.2259535912148,-21.0071376122031,
9.92193119447293));
#175707=CARTESIAN_POINT('Ctrl Pts',(18.2180419437898,-21.0051676192209,
9.92242312163059));
#175708=CARTESIAN_POINT('Ctrl Pts',(18.2135999339337,-21.0040462374247,
9.9226987012499));
#175709=CARTESIAN_POINT('Ctrl Pts',(18.1999587797943,-21.00055539645,9.92354320032073));
#175710=CARTESIAN_POINT('Ctrl Pts',(18.1907717693831,-20.9981383956788,
9.92410944563108));
#175711=CARTESIAN_POINT('Ctrl Pts',(18.108445438004,-20.9758856822973,9.92916368761632));
#175712=CARTESIAN_POINT('Ctrl Pts',(18.0363956240174,-20.9521956140284,
9.93344589650438));
#175713=CARTESIAN_POINT('Ctrl Pts',(17.9259442317426,-20.9091819038263,
9.94000667512318));
#175714=CARTESIAN_POINT('Ctrl Pts',(17.8866016392593,-20.8924719358181,
9.94234269522203));
#175715=CARTESIAN_POINT('Ctrl Pts',(17.748509231106,-20.828818611868,9.95062116095358));
#175716=CARTESIAN_POINT('Ctrl Pts',(17.6529225571144,-20.7754338027292,
9.95650785989923));
#175717=CARTESIAN_POINT('Ctrl Pts',(17.5160260225288,-20.6844149999887,
9.96564896184914));
#175718=CARTESIAN_POINT('Ctrl Pts',(17.4713725018903,-20.6521451404657,
9.96875462450005));
#175719=CARTESIAN_POINT('Ctrl Pts',(17.4010406010917,-20.5970179911439,
9.97389584051523));
#175720=CARTESIAN_POINT('Ctrl Pts',(17.37457038908,-20.5752115964785,9.97589206232658));
#175721=CARTESIAN_POINT('Ctrl Pts',(17.3404706757043,-20.5457006671356,
9.97855169165393));
#175722=CARTESIAN_POINT('Ctrl Pts',(17.3323532377909,-20.5385661478596,
9.97919159381127));
#175723=CARTESIAN_POINT('Ctrl Pts',(17.3191448626728,-20.5267766571123,
9.98024417288709));
#175724=CARTESIAN_POINT('Ctrl Pts',(17.314021357719,-20.5221583465184,9.98065530925501));
#175725=CARTESIAN_POINT('Ctrl Pts',(17.3041456362353,-20.5131685338695,
9.98145336458347));
#175726=CARTESIAN_POINT('Ctrl Pts',(17.2993906642057,-20.5088001621725,
9.98184014833224));
#175727=CARTESIAN_POINT('Ctrl Pts',(17.2884551799496,-20.4986611367334,
9.98273559628881));
#175728=CARTESIAN_POINT('Ctrl Pts',(17.2822891391559,-20.4928750993909,
9.98324491694591));
#175729=CARTESIAN_POINT('Ctrl Pts',(17.2657938265297,-20.4772094709614,
9.98461949273961));
#175730=CARTESIAN_POINT('Ctrl Pts',(17.2555298121516,-20.4672620849351,
9.98548767771643));
#175731=CARTESIAN_POINT('Ctrl Pts',(17.1621045911684,-20.3748659001916,
9.99351084267146));
#175732=CARTESIAN_POINT('Ctrl Pts',(17.0858313941751,-20.2857671975202,
10.0009689917939));
#175733=CARTESIAN_POINT('Ctrl Pts',(16.9216222301059,-20.0582193023279,
10.0193000830356));
#175734=CARTESIAN_POINT('Ctrl Pts',(16.8416122337423,-19.9149657665934,
10.0303152198449));
#175735=CARTESIAN_POINT('Ctrl Pts',(16.7667878036911,-19.7347904076777,
10.0427007538937));
#175736=CARTESIAN_POINT('Ctrl Pts',(16.7553382284179,-19.7053807060988,
10.0446770876979));
#175737=CARTESIAN_POINT('Ctrl Pts',(16.742097493446,-19.6689831662001,10.047058431303));
#175738=CARTESIAN_POINT('Ctrl Pts',(16.7396794444265,-19.6622295271547,
10.0474975967757));
#175739=CARTESIAN_POINT('Ctrl Pts',(16.7359349675651,-19.6516012405593,
10.0481843401434));
#175740=CARTESIAN_POINT('Ctrl Pts',(16.7345854008489,-19.6477348855633,
10.0484332570824));
#175741=CARTESIAN_POINT('Ctrl Pts',(16.7320789915784,-19.6404867827741,
10.0488981633403));
#175742=CARTESIAN_POINT('Ctrl Pts',(16.7309195071483,-19.6371060599562,
10.0491143026685));
#175743=CARTESIAN_POINT('Ctrl Pts',(16.7282860719902,-19.6293638851444,
10.0496076853711));
#175744=CARTESIAN_POINT('Ctrl Pts',(16.7268177853927,-19.6250005588354,
10.0498845920573));
#175745=CARTESIAN_POINT('Ctrl Pts',(16.7223273455718,-19.6115108447702,
10.050737222297));
#175746=CARTESIAN_POINT('Ctrl Pts',(16.7193530677632,-19.6023684872821,
10.0513101964217));
#175747=CARTESIAN_POINT('Ctrl Pts',(16.6905474223959,-19.5117313338043,
10.0569454309902));
#175748=CARTESIAN_POINT('Ctrl Pts',(16.6696095020876,-19.4287525817019,
10.0617451503291));
#175749=CARTESIAN_POINT('Ctrl Pts',(16.6294008321654,-19.2157687439358,
10.0736795303986));
#175750=CARTESIAN_POINT('Ctrl Pts',(16.6170990832059,-19.0848277878281,
10.0806785850671));
#175751=CARTESIAN_POINT('Ctrl Pts',(16.6169313786705,-18.8613529308207,
10.0930378829247));
#175752=CARTESIAN_POINT('Ctrl Pts',(16.6228899854673,-18.7692216646518,
10.0982490862488));
#175753=CARTESIAN_POINT('Ctrl Pts',(16.6366195100423,-18.6641219266842,
10.104462743823));
#175754=CARTESIAN_POINT('Ctrl Pts',(16.6385368154061,-18.6504826151109,
10.1052742404711));
#175755=CARTESIAN_POINT('Ctrl Pts',(16.641823177128,-18.6286517383975,10.106581719328));
#175756=CARTESIAN_POINT('Ctrl Pts',(16.6431076017403,-18.6204476928975,
10.1070750246083));
#175757=CARTESIAN_POINT('Ctrl Pts',(16.6454726643887,-18.6059018161945,
10.107953215884));
#175758=CARTESIAN_POINT('Ctrl Pts',(16.6465340099925,-18.5995569215029,
10.1083374851181));
#175759=CARTESIAN_POINT('Ctrl Pts',(16.6488043601941,-18.5863545015927,
10.1091396183901));
#175760=CARTESIAN_POINT('Ctrl Pts',(16.6500183104995,-18.5794979157171,
10.1095576355982));
#175761=CARTESIAN_POINT('Ctrl Pts',(16.6532558814742,-18.5617228935686,
10.110645087726));
#175762=CARTESIAN_POINT('Ctrl Pts',(16.6553316014101,-18.5508142725261,
10.1113161754137));
#175763=CARTESIAN_POINT('Ctrl Pts',(16.6646897604107,-18.5036573919809,
10.1142336488192));
#175764=CARTESIAN_POINT('Ctrl Pts',(16.6728349138898,-18.467588832413,10.116507408672));
#175765=CARTESIAN_POINT('Ctrl Pts',(16.6969459033728,-18.3724844854234,
10.1226194523867));
#175766=CARTESIAN_POINT('Ctrl Pts',(16.7145313844524,-18.3138988809202,
10.1265064270926));
#175767=CARTESIAN_POINT('Ctrl Pts',(16.7381478933373,-18.2460409537553,
10.1311462799043));
#175768=CARTESIAN_POINT('Ctrl Pts',(16.7417458099075,-18.2359504518563,
10.1318398405155));
#175769=CARTESIAN_POINT('Ctrl Pts',(16.7454193829761,-18.2258897262833,
10.1325348909312));
#175770=CARTESIAN_POINT('Origin',(18.734,-18.952,0.));
#175771=CARTESIAN_POINT('',(16.7454193125898,-18.2258899190485,11.1558808694255));
#175772=CARTESIAN_POINT('',(16.7454193692319,-18.2258897639242,10.9336112441224));
#175773=CARTESIAN_POINT('',(16.7454193692319,-18.2258897639242,0.));
#175774=CARTESIAN_POINT('',(16.6170004031077,-18.9533064294667,11.1109437209282));
#175775=CARTESIAN_POINT('Ctrl Pts',(16.7454193125899,-18.2258899190484,
11.1558808694255));
#175776=CARTESIAN_POINT('Ctrl Pts',(16.7234360607655,-18.2860949364022,
11.1523878540446));
#175777=CARTESIAN_POINT('Ctrl Pts',(16.7041774484112,-18.3473239923796,
11.1488669690875));
#175778=CARTESIAN_POINT('Ctrl Pts',(16.6773854477283,-18.4483623928592,
11.1430184399809));
#175779=CARTESIAN_POINT('Ctrl Pts',(16.6681681730665,-18.4876156162813,
11.1407373991175));
#175780=CARTESIAN_POINT('Ctrl Pts',(16.6588573176701,-18.5330622867407,
11.1380746208254));
#175781=CARTESIAN_POINT('Ctrl Pts',(16.6576628095842,-18.5390232085414,
11.1377249391111));
#175782=CARTESIAN_POINT('Ctrl Pts',(16.6558534146321,-18.5482589055261,
11.1371824507173));
#175783=CARTESIAN_POINT('Ctrl Pts',(16.6552205494197,-18.5515301542999,
11.1369901675784));
#175784=CARTESIAN_POINT('Ctrl Pts',(16.6491723940305,-18.5831934296378,
11.1351276504799));
#175785=CARTESIAN_POINT('Ctrl Pts',(16.6443315832669,-18.611690990428,11.1334407270184));
#175786=CARTESIAN_POINT('Ctrl Pts',(16.638532301595,-18.6506463611421,11.1311167916703));
#175787=CARTESIAN_POINT('Ctrl Pts',(16.6370657847835,-18.6610261493246,
11.1304958503707));
#175788=CARTESIAN_POINT('Ctrl Pts',(16.634862067329,-18.6775064781172,11.1295070779318));
#175789=CARTESIAN_POINT('Ctrl Pts',(16.6340742205913,-18.6836001607958,
11.1291408506994));
#175790=CARTESIAN_POINT('Ctrl Pts',(16.6325483605536,-18.6958202122398,
11.1284051467365));
#175791=CARTESIAN_POINT('Ctrl Pts',(16.6318105825134,-18.7019465490214,
11.1280356664325));
#175792=CARTESIAN_POINT('Ctrl Pts',(16.6303836083735,-18.7142486765774,
11.1272923938588));
#175793=CARTESIAN_POINT('Ctrl Pts',(16.6296947991971,-18.7204244496969,
11.126918593272));
#175794=CARTESIAN_POINT('Ctrl Pts',(16.6281826815492,-18.7345460177625,
11.1260622899236));
#175795=CARTESIAN_POINT('Ctrl Pts',(16.6273771405484,-18.7424935839338,
11.1255792320414));
#175796=CARTESIAN_POINT('Ctrl Pts',(16.6254321889814,-18.7628293109863,
11.1243402456562));
#175797=CARTESIAN_POINT('Ctrl Pts',(16.6243569717784,-18.7752231736112,
11.1235823147682));
#175798=CARTESIAN_POINT('Ctrl Pts',(16.6190952486443,-18.8427850268363,
11.1194348782796));
#175799=CARTESIAN_POINT('Ctrl Pts',(16.6169637969027,-18.8980864419166,
11.1159819897524));
#175800=CARTESIAN_POINT('Ctrl Pts',(16.6170004651092,-18.9534033075656,
11.1124693548963));
#175801=CARTESIAN_POINT('Ctrl Pts',(16.7454193692319,-18.2258897639242,
10.3555828645479));
#175802=CARTESIAN_POINT('Ctrl Pts',(16.7701522594713,-18.1581543925862,
10.3599055418906));
#175803=CARTESIAN_POINT('Ctrl Pts',(16.7983602529091,-18.091656257472,10.3642282192334));
#175804=CARTESIAN_POINT('Ctrl Pts',(16.8298869258318,-18.0267744054655,
10.3685508965761));
#175805=CARTESIAN_POINT('Ctrl Pts',(16.8614136604731,-17.9618924264424,
10.3728735823811));
#175806=CARTESIAN_POINT('Ctrl Pts',(16.896258868959,-17.8986271805337,10.3771962681862));
#175807=CARTESIAN_POINT('Ctrl Pts',(16.9342193564648,-17.8373347430031,
10.3815189539912));
#175808=CARTESIAN_POINT('Ctrl Pts',(16.972217854968,-17.7759809314797,10.3858459682338));
#175809=CARTESIAN_POINT('Ctrl Pts',(17.0133375966607,-17.7166042917782,
10.3901729824764));
#175810=CARTESIAN_POINT('Ctrl Pts',(17.0573316320686,-17.6595325211139,
10.394499996719));
#175811=CARTESIAN_POINT('Ctrl Pts',(17.1013502294102,-17.6024288871973,
10.3988294267399));
#175812=CARTESIAN_POINT('Ctrl Pts',(17.1482459902095,-17.5476330570704,
10.4031588567608));
#175813=CARTESIAN_POINT('Ctrl Pts',(17.1977330353864,-17.4954380159303,
10.4074882867817));
#175814=CARTESIAN_POINT('Ctrl Pts',(17.2473041777985,-17.4431542756441,
10.4118250741442));
#175815=CARTESIAN_POINT('Ctrl Pts',(17.2994750328197,-17.3934804831633,
10.4161618615067));
#175816=CARTESIAN_POINT('Ctrl Pts',(17.3539250843281,-17.3466706795386,
10.4204986488692));
#175817=CARTESIAN_POINT('Ctrl Pts',(17.3811407440825,-17.3232738295205,
10.422666296576));
#175818=CARTESIAN_POINT('Ctrl Pts',(17.4089253292483,-17.3005918231404,
10.4248339442827));
#175819=CARTESIAN_POINT('Ctrl Pts',(17.4372361998844,-17.2786522636614,
10.4270015919895));
#175820=CARTESIAN_POINT('Ctrl Pts',(17.494549025663,-17.2342375875375,10.4313898009204));
#175821=CARTESIAN_POINT('Ctrl Pts',(17.5542581954978,-17.1926841015565,
10.4357780098513));
#175822=CARTESIAN_POINT('Ctrl Pts',(17.6160462231313,-17.1542602099344,
10.4401662187822));
#175823=CARTESIAN_POINT('Ctrl Pts',(17.6777425470872,-17.1158933457383,
10.4445479148834));
#175824=CARTESIAN_POINT('Ctrl Pts',(17.7415111977167,-17.0806471078961,
10.4489296109847));
#175825=CARTESIAN_POINT('Ctrl Pts',(17.8070029012401,-17.0487487346935,
10.453311307086));
#175826=CARTESIAN_POINT('Ctrl Pts',(17.8724176467997,-17.0168878446181,
10.4576878543456));
#175827=CARTESIAN_POINT('Ctrl Pts',(17.9395509916045,-16.9883672144276,
10.4620644016053));
#175828=CARTESIAN_POINT('Ctrl Pts',(18.0080275301105,-16.9633690707015,
10.4664409488649));
#175829=CARTESIAN_POINT('Ctrl Pts',(18.0764606417909,-16.9383867804349,
10.4708147205819));
#175830=CARTESIAN_POINT('Ctrl Pts',(18.1462348050105,-16.9169227092787,
10.4751884922988));
#175831=CARTESIAN_POINT('Ctrl Pts',(18.2169543269192,-16.8991111155378,
10.4795622640158));
#175832=CARTESIAN_POINT('Ctrl Pts',(18.2876523286398,-16.8813049419247,
10.4839347047794));
#175833=CARTESIAN_POINT('Ctrl Pts',(18.359294650436,-16.8671491568768,10.4883071455429));
#175834=CARTESIAN_POINT('Ctrl Pts',(18.4314717388387,-16.8567277858954,
10.4926795863064));
#175835=CARTESIAN_POINT('Ctrl Pts',(18.5036506728176,-16.8463061484384,
10.4970521388738));
#175836=CARTESIAN_POINT('Ctrl Pts',(18.5763639228391,-16.8396191815878,
10.5014246914411));
#175837=CARTESIAN_POINT('Ctrl Pts',(18.6491947479436,-16.8366992957918,
10.5057972440085));
#175838=CARTESIAN_POINT('Ctrl Pts',(18.7221011596255,-16.8337763796282,
10.5101743345758));
#175839=CARTESIAN_POINT('Ctrl Pts',(18.7951249069977,-16.8346283697016,
10.5145514251431));
#175840=CARTESIAN_POINT('Ctrl Pts',(18.8678480060379,-16.8392355286782,
10.5189285157104));
#175841=CARTESIAN_POINT('Ctrl Pts',(18.9406108218616,-16.8438452037953,
10.5233079967694));
#175842=CARTESIAN_POINT('Ctrl Pts',(19.0130721829178,-16.8522140756297,
10.5276874778283));
#175843=CARTESIAN_POINT('Ctrl Pts',(19.0848207051463,-16.8642706514396,
10.5320669588873));
#175844=CARTESIAN_POINT('Ctrl Pts',(19.156696401149,-16.8763485974491,10.536454202547));
#175845=CARTESIAN_POINT('Ctrl Pts',(19.2278562638074,-16.8921271959049,
10.5408414462067));
#175846=CARTESIAN_POINT('Ctrl Pts',(19.2979011262236,-16.911484251508,10.5452286898664));
#175847=CARTESIAN_POINT('Ctrl Pts',(19.3455248831598,-16.9246451840768,
10.5482115928012));
#175848=CARTESIAN_POINT('Ctrl Pts',(19.3926335158209,-16.9394592758343,
10.5511944957361));
#175849=CARTESIAN_POINT('Ctrl Pts',(19.4391069833084,-16.9558754692931,
10.5541773986709));
#175850=CARTESIAN_POINT('Ctrl Pts',(19.507475042724,-16.9800256640268,10.5585656076018));
#175851=CARTESIAN_POINT('Ctrl Pts',(19.5747343896099,-17.0077395128395,
10.5629538165327));
#175852=CARTESIAN_POINT('Ctrl Pts',(19.6404874892068,-17.0388953421437,
10.5673420254636));
#175853=CARTESIAN_POINT('Ctrl Pts',(19.7061430003017,-17.0700049310314,
10.5717237215648));
#175854=CARTESIAN_POINT('Ctrl Pts',(19.7702962696065,-17.1045461545567,
10.5761054176661));
#175855=CARTESIAN_POINT('Ctrl Pts',(19.8325671704115,-17.1423483285189,
10.5804871137674));
#175856=CARTESIAN_POINT('Ctrl Pts',(19.8947648979524,-17.1801060819184,
10.584863661027));
#175857=CARTESIAN_POINT('Ctrl Pts',(19.9550842407134,-17.2211169246315,
10.5892402082867));
#175858=CARTESIAN_POINT('Ctrl Pts',(20.013168775078,-17.2651638357963,10.5936167555463));
#175859=CARTESIAN_POINT('Ctrl Pts',(20.071216473075,-17.3091828130501,10.5979905272633));
#175860=CARTESIAN_POINT('Ctrl Pts',(20.1270317913336,-17.3562337476985,
10.6023642989803));
#175861=CARTESIAN_POINT('Ctrl Pts',(20.1802876588313,-17.4060565961484,
10.6067380706972));
#175862=CARTESIAN_POINT('Ctrl Pts',(20.2335273203896,-17.4558642833382,
10.6111105114608));
#175863=CARTESIAN_POINT('Ctrl Pts',(20.2842087253976,-17.5084418803649,
10.6154829522244));
#175864=CARTESIAN_POINT('Ctrl Pts',(20.332039538181,-17.5634904989845,10.6198553929879));
#175865=CARTESIAN_POINT('Ctrl Pts',(20.3798715740035,-17.6185405252034,
10.6242279455553));
#175866=CARTESIAN_POINT('Ctrl Pts',(20.4248525580102,-17.6760613330223,
10.6286004981226));
#175867=CARTESIAN_POINT('Ctrl Pts',(20.4667296641659,-17.735720052406,10.63297305069));
#175868=CARTESIAN_POINT('Ctrl Pts',(20.508650231962,-17.7954406878589,10.6373501412573));
#175869=CARTESIAN_POINT('Ctrl Pts',(20.5474602125883,-17.8573032692078,
10.6417272318246));
#175870=CARTESIAN_POINT('Ctrl Pts',(20.5829499551955,-17.920945654593,10.646104322392));
#175871=CARTESIAN_POINT('Ctrl Pts',(20.6184590800684,-17.984622797447,10.6504838034509));
#175872=CARTESIAN_POINT('Ctrl Pts',(20.6506441436597,-18.0500812464321,
10.6548632845098));
#175873=CARTESIAN_POINT('Ctrl Pts',(20.679342585662,-18.1169363949915,10.6592427655688));
#175874=CARTESIAN_POINT('Ctrl Pts',(20.7080918954602,-18.1839100438528,
10.6636300092285));
#175875=CARTESIAN_POINT('Ctrl Pts',(20.7333420751797,-18.2522848831355,
10.6680172528882));
#175876=CARTESIAN_POINT('Ctrl Pts',(20.7549798102579,-18.3216591346502,
10.672404496548));
#175877=CARTESIAN_POINT('Ctrl Pts',(20.7696913851038,-18.368826940793,10.6753873994828));
#175878=CARTESIAN_POINT('Ctrl Pts',(20.7827340876901,-18.4164564326549,
10.6783703024176));
#175879=CARTESIAN_POINT('Ctrl Pts',(20.794085873422,-18.4644190383875,10.6813532053524));
#175880=CARTESIAN_POINT('Ctrl Pts',(20.8107857153611,-18.5349777992406,
10.6857414142833));
#175881=CARTESIAN_POINT('Ctrl Pts',(20.8238889631161,-18.6065332466769,
10.6901296232142));
#175882=CARTESIAN_POINT('Ctrl Pts',(20.8332827468939,-18.6786852572696,
10.6945178321451));
#175883=CARTESIAN_POINT('Ctrl Pts',(20.8426625887389,-18.7507301823154,
10.6988995282463));
#175884=CARTESIAN_POINT('Ctrl Pts',(20.8483438339329,-18.8233694384939,
10.7032812243476));
#175885=CARTESIAN_POINT('Ctrl Pts',(20.8502642454991,-18.896191011278,10.7076629204489));
#175886=CARTESIAN_POINT('Ctrl Pts',(20.8521824004289,-18.9689270129188,
10.7120394677085));
#175887=CARTESIAN_POINT('Ctrl Pts',(20.8503484880034,-19.0418444257663,
10.7164160149681));
#175888=CARTESIAN_POINT('Ctrl Pts',(20.8447520630799,-19.1145260846878,
10.7207925622278));
#175889=CARTESIAN_POINT('Ctrl Pts',(20.8391591873278,-19.1871616499575,
10.7251663339448));
#175890=CARTESIAN_POINT('Ctrl Pts',(20.8298085704124,-19.2595612781811,
10.7295401056617));
#175891=CARTESIAN_POINT('Ctrl Pts',(20.8167418305018,-19.3313091977237,
10.7339138773787));
#175892=CARTESIAN_POINT('Ctrl Pts',(20.8036790668441,-19.4030352841335,
10.7382863181423));
#175893=CARTESIAN_POINT('Ctrl Pts',(20.7869025116117,-19.4741095812966,
10.7426587589058));
#175894=CARTESIAN_POINT('Ctrl Pts',(20.7665052467619,-19.5441244986363,
10.7470311996694));
#175895=CARTESIAN_POINT('Ctrl Pts',(20.7461074603518,-19.6141412062652,
10.7514037522367));
#175896=CARTESIAN_POINT('Ctrl Pts',(20.7220889173522,-19.6830980177239,
10.755776304804));
#175897=CARTESIAN_POINT('Ctrl Pts',(20.6945926588476,-19.7506021700904,
10.7601488573714));
#175898=CARTESIAN_POINT('Ctrl Pts',(20.6670678636887,-19.8181763808124,
10.7645259479387));
#175899=CARTESIAN_POINT('Ctrl Pts',(20.6360583291635,-19.884294474674,10.768903038506));
#175900=CARTESIAN_POINT('Ctrl Pts',(20.6017550792374,-19.9485841479688,
10.7732801290734));
#175901=CARTESIAN_POINT('Ctrl Pts',(20.5674330950334,-20.0129089322404,
10.7776596101323));
#175902=CARTESIAN_POINT('Ctrl Pts',(20.5298140629451,-20.0754028942418,
10.7820390911912));
#175903=CARTESIAN_POINT('Ctrl Pts',(20.4891333854102,-20.1357211662458,
10.7864185722502));
#175904=CARTESIAN_POINT('Ctrl Pts',(20.4483806016475,-20.1961463519821,
10.7908058159099));
#175905=CARTESIAN_POINT('Ctrl Pts',(20.4045556257384,-20.2543877608709,
10.7951930595696));
#175906=CARTESIAN_POINT('Ctrl Pts',(20.3579349545336,-20.310132638384,10.7995803032293));
#175907=CARTESIAN_POINT('Ctrl Pts',(20.3262373904716,-20.3480337835292,
10.8025632061641));
#175908=CARTESIAN_POINT('Ctrl Pts',(20.2932482928817,-20.384781572932,10.8055461090989));
#175909=CARTESIAN_POINT('Ctrl Pts',(20.2590638380205,-20.4202878770739,
10.8085290120338));
#175910=CARTESIAN_POINT('Ctrl Pts',(20.208774394013,-20.4725219203344,10.8129172209647));
#175911=CARTESIAN_POINT('Ctrl Pts',(20.1557001261013,-20.5222712846033,
10.8173054298956));
#175912=CARTESIAN_POINT('Ctrl Pts',(20.1001163804877,-20.5692244850246,
10.8216936388265));
#175913=CARTESIAN_POINT('Ctrl Pts',(20.0446151303687,-20.6161079991114,
10.8260753349277));
#175914=CARTESIAN_POINT('Ctrl Pts',(19.9866121616043,-20.6602032788999,
10.830457031029));
#175915=CARTESIAN_POINT('Ctrl Pts',(19.9264202255139,-20.7012349772931,
10.8348387271302));
#175916=CARTESIAN_POINT('Ctrl Pts',(19.8662990197386,-20.7422184601752,
10.8392152743899));
#175917=CARTESIAN_POINT('Ctrl Pts',(19.8039943529516,-20.7801452426345,
10.8435918216495));
#175918=CARTESIAN_POINT('Ctrl Pts',(19.739851341254,-20.8147807383848,10.8479683689092));
#175919=CARTESIAN_POINT('Ctrl Pts',(19.6757490081222,-20.8493942688071,
10.8523421406261));
#175920=CARTESIAN_POINT('Ctrl Pts',(19.6098110666879,-20.8807204253384,
10.8567159123431));
#175921=CARTESIAN_POINT('Ctrl Pts',(19.5424096422237,-20.9085691529715,
10.8610896840601));
#175922=CARTESIAN_POINT('Ctrl Pts',(19.4750287282393,-20.9364094061433,
10.8654621248236));
#175923=CARTESIAN_POINT('Ctrl Pts',(19.4061856609217,-20.9607741471641,
10.8698345655872));
#175924=CARTESIAN_POINT('Ctrl Pts',(19.3362735429414,-20.9815210221806,
10.8742070063508));
#175925=CARTESIAN_POINT('Ctrl Pts',(19.2663596373003,-21.002268427697,10.8785795589181));
#175926=CARTESIAN_POINT('Ctrl Pts',(19.1953770897375,-21.0193976482244,
10.8829521114855));
#175927=CARTESIAN_POINT('Ctrl Pts',(19.1237335771401,-21.0328163635577,
10.8873246640528));
#175928=CARTESIAN_POINT('Ctrl Pts',(19.0520157102031,-21.0462490053399,
10.8917017546201));
#175929=CARTESIAN_POINT('Ctrl Pts',(18.9796359837846,-21.0559633643479,
10.8960788451875));
#175930=CARTESIAN_POINT('Ctrl Pts',(18.9070108440327,-21.0619185405714,
10.9004559357548));
#175931=CARTESIAN_POINT('Ctrl Pts',(18.8343460409964,-21.0678769691378,
10.9048354168137));
#175932=CARTESIAN_POINT('Ctrl Pts',(18.7614360402691,-21.070072112832,10.9092148978727));
#175933=CARTESIAN_POINT('Ctrl Pts',(18.6886982399077,-21.0685152374912,
10.9135943789316));
#175934=CARTESIAN_POINT('Ctrl Pts',(18.6158315122834,-21.0669556025994,
10.9179816225913));
#175935=CARTESIAN_POINT('Ctrl Pts',(18.5431380760574,-21.0616307033084,
10.9223688662511));
#175936=CARTESIAN_POINT('Ctrl Pts',(18.4710305707949,-21.0526037416189,
10.9267561099108));
#175937=CARTESIAN_POINT('Ctrl Pts',(18.4220044154792,-21.0464662775061,
10.9297390128456));
#175938=CARTESIAN_POINT('Ctrl Pts',(18.3732489672178,-21.0386185484977,
10.9327219157804));
#175939=CARTESIAN_POINT('Ctrl Pts',(18.3248903873721,-21.0290937207684,
10.9357048187152));
#175940=CARTESIAN_POINT('Ctrl Pts',(18.2537491009802,-21.0150815537551,
10.9400930276461));
#175941=CARTESIAN_POINT('Ctrl Pts',(18.1831896640503,-20.9973828809338,
10.944481236577));
#175942=CARTESIAN_POINT('Ctrl Pts',(18.1136230257297,-20.9760606240415,
10.9488694455079));
#175943=CARTESIAN_POINT('Ctrl Pts',(18.0441596358346,-20.9547700129136,
10.9532511416091));
#175944=CARTESIAN_POINT('Ctrl Pts',(17.9756865768829,-20.929866633968,10.9576328377104));
#175945=CARTESIAN_POINT('Ctrl Pts',(17.9086046585659,-20.9014644214088,
10.9620145338117));
#175946=CARTESIAN_POINT('Ctrl Pts',(17.8416015668415,-20.8730955837098,
10.9663910810713));
#175947=CARTESIAN_POINT('Ctrl Pts',(17.7759868104063,-20.8412362668761,
10.970767628331));
#175948=CARTESIAN_POINT('Ctrl Pts',(17.7121444440029,-20.8060496818256,
10.9751441755906));
#175949=CARTESIAN_POINT('Ctrl Pts',(17.6483425655005,-20.7708854115961,
10.9795179473076));
#175950=CARTESIAN_POINT('Ctrl Pts',(17.5863112682431,-20.7323982921383,
10.9838917190245));
#175951=CARTESIAN_POINT('Ctrl Pts',(17.5264117827671,-20.6907983487456,
10.9882654907415));
#175952=CARTESIAN_POINT('Ctrl Pts',(17.4665305249056,-20.6492110643553,
10.9926379315051));
#175953=CARTESIAN_POINT('Ctrl Pts',(17.4087801868841,-20.6045131115935,
10.9970103722686));
#175954=CARTESIAN_POINT('Ctrl Pts',(17.3534932447848,-20.5569579741555,
11.0013828130322));
#175955=CARTESIAN_POINT('Ctrl Pts',(17.2982048889925,-20.5094016207274,
11.0057553655995));
#175956=CARTESIAN_POINT('Ctrl Pts',(17.2453804185818,-20.4589882536492,
11.0101279181668));
#175957=CARTESIAN_POINT('Ctrl Pts',(17.1953181280021,-20.4060106934906,
11.0145004707342));
#175958=CARTESIAN_POINT('Ctrl Pts',(17.1452038808888,-20.3529781512217,
11.0188775613015));
#175959=CARTESIAN_POINT('Ctrl Pts',(17.0978578691735,-20.2973764539274,
11.0232546518688));
#175960=CARTESIAN_POINT('Ctrl Pts',(17.0535398976935,-20.2395336285146,
11.0276317424362));
#175961=CARTESIAN_POINT('Ctrl Pts',(17.0091977225243,-20.1816592129879,
11.0320112234951));
#175962=CARTESIAN_POINT('Ctrl Pts',(16.9678871535202,-20.1215416302814,
11.036390704554));
#175963=CARTESIAN_POINT('Ctrl Pts',(16.9298246475467,-20.0595379440905,
11.040770185613));
#175964=CARTESIAN_POINT('Ctrl Pts',(16.8916946760369,-19.997424356782,11.0451574292727));
#175965=CARTESIAN_POINT('Ctrl Pts',(16.856824495368,-19.9334184139102,11.0495446729324));
#175966=CARTESIAN_POINT('Ctrl Pts',(16.8253843166295,-19.8679012900919,
11.0539319165921));
#175967=CARTESIAN_POINT('Ctrl Pts',(16.8040080246555,-19.8233559591102,
11.056914819527));
#175968=CARTESIAN_POINT('Ctrl Pts',(16.7842163233976,-19.7781125159704,
11.0598977224618));
#175969=CARTESIAN_POINT('Ctrl Pts',(16.7660496141036,-19.7322949946336,
11.0628806253966));
#175970=CARTESIAN_POINT('Ctrl Pts',(16.7358636223541,-19.6561641280759,
11.0678370477142));
#175971=CARTESIAN_POINT('Ctrl Pts',(16.7100671742202,-19.578198920716,11.0727934700317));
#175972=CARTESIAN_POINT('Ctrl Pts',(16.6888585600969,-19.4988870914467,
11.0777498923492));
#175973=CARTESIAN_POINT('Ctrl Pts',(16.6677318984788,-19.4198817321365,
11.0826871624852));
#175974=CARTESIAN_POINT('Ctrl Pts',(16.6511578246449,-19.3395403557194,
11.0876244326213));
#175975=CARTESIAN_POINT('Ctrl Pts',(16.6392856441441,-19.2583670468102,
11.0925617027573));
#175976=CARTESIAN_POINT('Ctrl Pts',(16.6274900435723,-19.1777173355868,
11.0974671256858));
#175977=CARTESIAN_POINT('Ctrl Pts',(16.6203359927508,-19.0962466252342,
11.1023725486143));
#175978=CARTESIAN_POINT('Ctrl Pts',(16.6179218376289,-19.0144676775316,
11.1072779715428));
#175979=CARTESIAN_POINT('Ctrl Pts',(16.6173204835912,-18.9940969482629,
11.1084998880046));
#175980=CARTESIAN_POINT('Ctrl Pts',(16.6170129926863,-18.9737071731887,
11.1097218044664));
#175981=CARTESIAN_POINT('Ctrl Pts',(16.6170004031077,-18.9533064294667,
11.1109437209282));
#175982=CARTESIAN_POINT('',(16.6170004031077,-18.9506935705328,10.8890562790718));
#175983=CARTESIAN_POINT('Ctrl Pts',(16.7454193829761,-18.2258897262833,
10.1325348909312));
#175984=CARTESIAN_POINT('Ctrl Pts',(16.7957300955987,-18.0881049963718,
10.1420538200687));
#175985=CARTESIAN_POINT('Ctrl Pts',(16.8602294232363,-17.9559072036814,
10.1518904229148));
#175986=CARTESIAN_POINT('Ctrl Pts',(16.9705620789177,-17.7790615297577,
10.1654299256796));
#175987=CARTESIAN_POINT('Ctrl Pts',(17.0055077313234,-17.7281479046147,
10.1693725844016));
#175988=CARTESIAN_POINT('Ctrl Pts',(17.0481243243609,-17.6715330475318,
10.1737463481034));
#175989=CARTESIAN_POINT('Ctrl Pts',(17.0536641597985,-17.6642718139689,
10.1743070933956));
#175990=CARTESIAN_POINT('Ctrl Pts',(17.0620088150317,-17.6534797633357,
10.175139888946));
#175991=CARTESIAN_POINT('Ctrl Pts',(17.064778120803,-17.6499217970805,10.1754143473587));
#175992=CARTESIAN_POINT('Ctrl Pts',(17.0697578837249,-17.6435658623637,
10.1759044156734));
#175993=CARTESIAN_POINT('Ctrl Pts',(17.0719640541656,-17.6407646170597,
10.1761203224753));
#175994=CARTESIAN_POINT('Ctrl Pts',(17.0767598422769,-17.6347068017437,
10.1765870501452));
#175995=CARTESIAN_POINT('Ctrl Pts',(17.0793519775629,-17.6314522980704,
10.1768376869375));
#175996=CARTESIAN_POINT('Ctrl Pts',(17.0866262035549,-17.6223743351843,
10.177536565398));
#175997=CARTESIAN_POINT('Ctrl Pts',(17.0913296095108,-17.61656792545,10.1779833059919));
#175998=CARTESIAN_POINT('Ctrl Pts',(17.1189523502469,-17.5828340816282,
10.1805779702704));
#175999=CARTESIAN_POINT('Ctrl Pts',(17.1425543086516,-17.555470306126,10.182679512319));
#176000=CARTESIAN_POINT('Ctrl Pts',(17.2209746894621,-17.469122602259,10.1893509058033));
#176001=CARTESIAN_POINT('Ctrl Pts',(17.2784630223073,-17.41265432694,10.1937780093484));
#176002=CARTESIAN_POINT('Ctrl Pts',(17.4407098117256,-17.2705240626054,
10.205535089745));
#176003=CARTESIAN_POINT('Ctrl Pts',(17.550678297492,-17.1914009901979,10.2127865843535));
#176004=CARTESIAN_POINT('Ctrl Pts',(17.7219085497416,-17.0915333198103,
10.223936955663));
#176005=CARTESIAN_POINT('Ctrl Pts',(17.7777672580292,-17.0622160944038,
10.2275505927027));
#176006=CARTESIAN_POINT('Ctrl Pts',(17.8461537358047,-17.0301326842564,
10.2319867407696));
#176007=CARTESIAN_POINT('Ctrl Pts',(17.8575065578041,-17.0249285939676,
10.2327235176444));
#176008=CARTESIAN_POINT('Ctrl Pts',(17.8762116742383,-17.0165537245252,
10.2339382828108));
#176009=CARTESIAN_POINT('Ctrl Pts',(17.8835371883593,-17.0133236215431,
10.2344142317329));
#176010=CARTESIAN_POINT('Ctrl Pts',(17.8967322480422,-17.0075945880762,
10.23527198129));
#176011=CARTESIAN_POINT('Ctrl Pts',(17.9025951268876,-17.0050804767594,
10.2356532576554));
#176012=CARTESIAN_POINT('Ctrl Pts',(17.915097202723,-16.9997861242286,10.2364666714788));
#176013=CARTESIAN_POINT('Ctrl Pts',(17.9217393818782,-16.9970131728325,
10.2368990510978));
#176014=CARTESIAN_POINT('Ctrl Pts',(17.9396436277685,-16.9896455727855,
10.2380652135793));
#176015=CARTESIAN_POINT('Ctrl Pts',(17.9509312379949,-16.985114073362,10.2388011205731));
#176016=CARTESIAN_POINT('Ctrl Pts',(18.0072714631114,-16.9630576984454,
10.2424782702486));
#176017=CARTESIAN_POINT('Ctrl Pts',(18.0528730393969,-16.9469834640486,
10.2454676595449));
#176018=CARTESIAN_POINT('Ctrl Pts',(18.1854403760795,-16.9052988818691,
10.2542017471225));
#176019=CARTESIAN_POINT('Ctrl Pts',(18.2735461488255,-16.883695804691,10.2600638157415));
#176020=CARTESIAN_POINT('Ctrl Pts',(18.5213291246805,-16.8395598987305,
10.2765863302488));
#176021=CARTESIAN_POINT('Ctrl Pts',(18.6826103942637,-16.8295026002585,
10.2874126707951));
#176022=CARTESIAN_POINT('Ctrl Pts',(18.8634558574733,-16.8388671481655,
10.2987727144306));
#176023=CARTESIAN_POINT('Ctrl Pts',(18.883420982029,-16.8401849735893,10.3000154305921));
#176024=CARTESIAN_POINT('Ctrl Pts',(18.9097266868776,-16.8422962624498,
10.3016351183705));
#176025=CARTESIAN_POINT('Ctrl Pts',(18.9160858892075,-16.8428356014584,
10.3020252987239));
#176026=CARTESIAN_POINT('Ctrl Pts',(18.9263462769461,-16.8437525596449,
10.3026525301919));
#176027=CARTESIAN_POINT('Ctrl Pts',(18.9302489657443,-16.8441122648393,
10.3028905662142));
#176028=CARTESIAN_POINT('Ctrl Pts',(18.9377548121748,-16.8448250942274,
10.3033472991222));
#176029=CARTESIAN_POINT('Ctrl Pts',(18.9413580661832,-16.8451766235564,
10.3035660799459));
#176030=CARTESIAN_POINT('Ctrl Pts',(18.9498804195589,-16.8460301299421,
10.3040824355745));
#176031=CARTESIAN_POINT('Ctrl Pts',(18.9547987304329,-16.8465401046539,
10.3043795614182));
#176032=CARTESIAN_POINT('Ctrl Pts',(18.9711072085082,-16.8482888885894,
10.3053620494374));
#176033=CARTESIAN_POINT('Ctrl Pts',(18.9824893314753,-16.8496029552277,
10.306043313592));
#176034=CARTESIAN_POINT('Ctrl Pts',(19.0908934098305,-16.8630108870786,
10.3124941111033));
#176035=CARTESIAN_POINT('Ctrl Pts',(19.1869913741393,-16.8817217354081,
10.3179276581124));
#176036=CARTESIAN_POINT('Ctrl Pts',(19.3427049008834,-16.9234076637989,
10.3267475068387));
#176037=CARTESIAN_POINT('Ctrl Pts',(19.4031811908957,-16.9425460341899,
10.3301766235674));
#176038=CARTESIAN_POINT('Ctrl Pts',(19.598052165044,-17.0139899175417,10.3414650180681));
#176039=CARTESIAN_POINT('Ctrl Pts',(19.7279547876522,-17.0772959386383,
10.3494033927115));
#176040=CARTESIAN_POINT('Ctrl Pts',(19.8625423237699,-17.1608313634513,
10.3586834022296));
#176041=CARTESIAN_POINT('Ctrl Pts',(19.8745968344252,-17.1684833313024,
10.3595242186359));
#176042=CARTESIAN_POINT('Ctrl Pts',(19.8936617334745,-17.1808576884849,
10.3608698985987));
#176043=CARTESIAN_POINT('Ctrl Pts',(19.9007229663745,-17.1855012198422,
10.3613718271763));
#176044=CARTESIAN_POINT('Ctrl Pts',(19.9131291707898,-17.1937664882229,
10.362260004276));
#176045=CARTESIAN_POINT('Ctrl Pts',(19.9184857630501,-17.1973706490971,
10.3626455879037));
#176046=CARTESIAN_POINT('Ctrl Pts',(19.9295324842425,-17.2048770268249,
10.363445158131));
#176047=CARTESIAN_POINT('Ctrl Pts',(19.9352201842589,-17.2087826666043,
10.3638592716852));
#176048=CARTESIAN_POINT('Ctrl Pts',(19.9497743039565,-17.2188817658624,
10.3649252613995));
#176049=CARTESIAN_POINT('Ctrl Pts',(19.9586124573843,-17.2251154369552,
10.3655786697191));
#176050=CARTESIAN_POINT('Ctrl Pts',(19.9953313402991,-17.2514374114025,
10.3683191174326));
#176051=CARTESIAN_POINT('Ctrl Pts',(20.0227673488513,-17.2721344188028,
10.3704295818428));
#176052=CARTESIAN_POINT('Ctrl Pts',(20.0929585128365,-17.3278166276143,
10.3759988928031));
#176053=CARTESIAN_POINT('Ctrl Pts',(20.1348674597177,-17.363821987084,10.3794963808924));
#176054=CARTESIAN_POINT('Ctrl Pts',(20.2555226388132,-17.4759753460129,
10.3900858946476));
#176055=CARTESIAN_POINT('Ctrl Pts',(20.3298163930958,-17.5566339203428,
10.3973262438312));
#176056=CARTESIAN_POINT('Ctrl Pts',(20.4322357464445,-17.6867598286241,
10.4082648890072));
#176057=CARTESIAN_POINT('Ctrl Pts',(20.4651734761693,-17.7322147127585,
10.4119625540102));
#176058=CARTESIAN_POINT('Ctrl Pts',(20.5072149341785,-17.7953720873743,
10.4168929756721));
#176059=CARTESIAN_POINT('Ctrl Pts',(20.5179321087802,-17.8119712278225,
10.4181702261452));
#176060=CARTESIAN_POINT('Ctrl Pts',(20.5517785990921,-17.8660401880973,
10.4222657511306));
#176061=CARTESIAN_POINT('Ctrl Pts',(20.5739734608864,-17.9040849126947,
10.4250486655385));
#176062=CARTESIAN_POINT('Ctrl Pts',(20.5985622110295,-17.9494264940757,
10.4282277276706));
#176063=CARTESIAN_POINT('Ctrl Pts',(20.6021219391083,-17.9560751543949,
10.4286904986772));
#176064=CARTESIAN_POINT('Ctrl Pts',(20.6077880740002,-17.9667953184576,
10.4294310513469));
#176065=CARTESIAN_POINT('Ctrl Pts',(20.6099168813717,-17.9708548191551,
10.4297101978003));
#176066=CARTESIAN_POINT('Ctrl Pts',(20.613684915443,-17.9780973167066,10.4302058901149));
#176067=CARTESIAN_POINT('Ctrl Pts',(20.6153292700714,-17.9812775905825,
10.4304227568122));
#176068=CARTESIAN_POINT('Ctrl Pts',(20.6188210100783,-17.9880730103868,
10.4308844322552));
#176069=CARTESIAN_POINT('Ctrl Pts',(20.6206660621078,-17.9916892939962,
10.4311290944162));
#176070=CARTESIAN_POINT('Ctrl Pts',(20.6256700598912,-18.0015671669466,
10.4317946569639));
#176071=CARTESIAN_POINT('Ctrl Pts',(20.6288083440272,-18.0078392466441,
10.4322142797877));
#176072=CARTESIAN_POINT('Ctrl Pts',(20.6449306666892,-18.0404649883131,
10.4343821965714));
#176073=CARTESIAN_POINT('Ctrl Pts',(20.6573969642439,-18.0670726556243,
10.4361001290225));
#176074=CARTESIAN_POINT('Ctrl Pts',(20.6927930372405,-18.1469058250094,
10.4411321133958));
#176075=CARTESIAN_POINT('Ctrl Pts',(20.7140968879184,-18.2008248804714,
10.4443722525155));
#176076=CARTESIAN_POINT('Ctrl Pts',(20.7880001367405,-18.4129655902131,
10.4567569627002));
#176077=CARTESIAN_POINT('Ctrl Pts',(20.8240537212191,-18.5762984991833,
10.4655773723993));
#176078=CARTESIAN_POINT('Ctrl Pts',(20.8467111687562,-18.8037693452038,
10.4784462498715));
#176079=CARTESIAN_POINT('Ctrl Pts',(20.8501415170503,-18.8656006986345,
10.481995657321));
#176080=CARTESIAN_POINT('Ctrl Pts',(20.851001813363,-18.9399010419642,10.4863598615508));
#176081=CARTESIAN_POINT('Ctrl Pts',(20.8510363611967,-18.9523132244191,
10.4870921832702));
#176082=CARTESIAN_POINT('Ctrl Pts',(20.8509137753343,-18.9727072276153,
10.4883010838398));
#176083=CARTESIAN_POINT('Ctrl Pts',(20.8508206458101,-18.9806892362942,
10.4887756571352));
#176084=CARTESIAN_POINT('Ctrl Pts',(20.8505719131426,-18.9950465220383,
10.4896319060536));
#176085=CARTESIAN_POINT('Ctrl Pts',(20.8504326424018,-19.0014220129529,
10.4900130651295));
#176086=CARTESIAN_POINT('Ctrl Pts',(20.8500744597129,-19.0150072072234,
10.4908272862738));
#176087=CARTESIAN_POINT('Ctrl Pts',(20.8498475025669,-19.0222166012236,
10.4912605959793));
#176088=CARTESIAN_POINT('Ctrl Pts',(20.8491363508173,-19.0416484168717,
10.4924318670969));
#176089=CARTESIAN_POINT('Ctrl Pts',(20.8485830661029,-19.0538678943721,
10.4931719848728));
#176090=CARTESIAN_POINT('Ctrl Pts',(20.84527274177,-19.1152079183555,10.4969057361948));
#176091=CARTESIAN_POINT('Ctrl Pts',(20.8409100773936,-19.1642232531996,
10.4999493174715));
#176092=CARTESIAN_POINT('Ctrl Pts',(20.8233582365969,-19.3054805611817,
10.5089013130598));
#176093=CARTESIAN_POINT('Ctrl Pts',(20.8057844131461,-19.3970531799347,
10.5149344377632));
#176094=CARTESIAN_POINT('Ctrl Pts',(20.7404394493395,-19.6471496014099,
10.5319198922653));
#176095=CARTESIAN_POINT('Ctrl Pts',(20.68003645299,-19.8016941123581,10.5430358164807));
#176096=CARTESIAN_POINT('Ctrl Pts',(20.5956714639142,-19.9600002883786,
10.5541994886098));
#176097=CARTESIAN_POINT('Ctrl Pts',(20.5889607295882,-19.9722969844839,
10.5550647355217));
#176098=CARTESIAN_POINT('Ctrl Pts',(20.5794327277478,-19.9893512379545,
10.5562611083863));
#176099=CARTESIAN_POINT('Ctrl Pts',(20.5767183061933,-19.9941654327063,
10.5565984207689));
#176100=CARTESIAN_POINT('Ctrl Pts',(20.5723233068981,-20.0018893795181,
10.5571388818417));
#176101=CARTESIAN_POINT('Ctrl Pts',(20.5706546217147,-20.0048058181875,
10.5573427838927));
#176102=CARTESIAN_POINT('Ctrl Pts',(20.5671475192382,-20.0109016293311,
10.5577685998503));
#176103=CARTESIAN_POINT('Ctrl Pts',(20.5653077651162,-20.0140802029747,
10.557990421151));
#176104=CARTESIAN_POINT('Ctrl Pts',(20.56082543039,-20.021778133228,10.558527149732));
#176105=CARTESIAN_POINT('Ctrl Pts',(20.5581743168869,-20.0262925441416,
10.5588415070615));
#176106=CARTESIAN_POINT('Ctrl Pts',(20.548779785926,-20.0421548395615,10.5599448062051));
#176107=CARTESIAN_POINT('Ctrl Pts',(20.5419468468524,-20.0534497103275,
10.5607281413541));
#176108=CARTESIAN_POINT('Ctrl Pts',(20.500501331558,-20.1205343252392,10.5653715579759));
#176109=CARTESIAN_POINT('Ctrl Pts',(20.4634110576857,-20.1747585579245,
10.5690872775558));
#176110=CARTESIAN_POINT('Ctrl Pts',(20.3658366028335,-20.3040637622089,
10.5780787822703));
#176111=CARTESIAN_POINT('Ctrl Pts',(20.3026344321485,-20.3769051043167,
10.58326573562));
#176112=CARTESIAN_POINT('Ctrl Pts',(20.1353215694684,-20.5450581279599,
10.596173804659));
#176113=CARTESIAN_POINT('Ctrl Pts',(20.0262483793294,-20.6347426860893,
10.6039450996367));
#176114=CARTESIAN_POINT('Ctrl Pts',(19.8972047642764,-20.7208549094597,
10.6130336388409));
#176115=CARTESIAN_POINT('Ctrl Pts',(19.8852441157579,-20.7286625975121,
10.6138747668989));
#176116=CARTESIAN_POINT('Ctrl Pts',(19.8660809969454,-20.7408971648408,
10.6152208524136));
#176117=CARTESIAN_POINT('Ctrl Pts',(19.8589293061762,-20.7454030508966,
10.6157228720888));
#176118=CARTESIAN_POINT('Ctrl Pts',(19.8462676904791,-20.7532749016597,
10.6166111552809));
#176119=CARTESIAN_POINT('Ctrl Pts',(19.8407689618323,-20.7566587351442,
10.6169967533925));
#176120=CARTESIAN_POINT('Ctrl Pts',(19.8293628577293,-20.763606139712,10.6177962995137));
#176121=CARTESIAN_POINT('Ctrl Pts',(19.8234533765537,-20.7671660899483,
10.6182103742107));
#176122=CARTESIAN_POINT('Ctrl Pts',(19.8082377604992,-20.7762311101344,
10.6192761497955));
#176123=CARTESIAN_POINT('Ctrl Pts',(19.7989067446197,-20.7816938344257,
10.619929381656));
#176124=CARTESIAN_POINT('Ctrl Pts',(19.7597685938769,-20.8042059637299,
10.6226681172258));
#176125=CARTESIAN_POINT('Ctrl Pts',(19.7295920764681,-20.8205995666826,
10.6247770093685));
#176126=CARTESIAN_POINT('Ctrl Pts',(19.6499190661354,-20.8614046162073,
10.6303411813431));
#176127=CARTESIAN_POINT('Ctrl Pts',(19.599845617929,-20.8846262613374,10.6338350138812));
#176128=CARTESIAN_POINT('Ctrl Pts',(19.4479034434923,-20.9479989179057,
10.6444175085463));
#176129=CARTESIAN_POINT('Ctrl Pts',(19.343772485754,-20.9822324641211,10.6516545180829));
#176130=CARTESIAN_POINT('Ctrl Pts',(19.1859148345377,-21.0208836174798,
10.6623900390253));
#176131=CARTESIAN_POINT('Ctrl Pts',(19.1339001047365,-21.0315640599736,
10.665888562512));
#176132=CARTESIAN_POINT('Ctrl Pts',(19.0703147680502,-21.0421461233079,
10.6700841988521));
#176133=CARTESIAN_POINT('Ctrl Pts',(19.0590769322727,-21.0439233816769,
10.6708226466741));
#176134=CARTESIAN_POINT('Ctrl Pts',(18.9936910705494,-21.0537245048849,
10.6750995285825));
#176135=CARTESIAN_POINT('Ctrl Pts',(18.9392573580883,-21.0597371452283,
10.6785821640569));
#176136=CARTESIAN_POINT('Ctrl Pts',(18.8758953721517,-21.0642574858035,
10.6825011444287));
#176137=CARTESIAN_POINT('Ctrl Pts',(18.8671396493571,-21.064827447488,10.6830397054138));
#176138=CARTESIAN_POINT('Ctrl Pts',(18.8538934582752,-21.0656070499557,
10.683849701606));
#176139=CARTESIAN_POINT('Ctrl Pts',(18.8494055749012,-21.065856844042,10.6841233051208));
#176140=CARTESIAN_POINT('Ctrl Pts',(18.8413570849555,-21.0662791119787,
10.6846124554604));
#176141=CARTESIAN_POINT('Ctrl Pts',(18.8377968223099,-21.0664568870779,
10.6848282944198));
#176142=CARTESIAN_POINT('Ctrl Pts',(18.8300697887916,-21.06682315865,10.6852955705623));
#176143=CARTESIAN_POINT('Ctrl Pts',(18.8259029180993,-21.0670083335568,
10.6855468199258));
#176144=CARTESIAN_POINT('Ctrl Pts',(18.8142222737853,-21.0674928343694,
10.686249138739));
#176145=CARTESIAN_POINT('Ctrl Pts',(18.8067073264849,-21.0677644467195,
10.6866986831168));
#176146=CARTESIAN_POINT('Ctrl Pts',(18.7622839394637,-21.0691330709559,
10.6893433078396));
#176147=CARTESIAN_POINT('Ctrl Pts',(18.7253509201075,-21.0693044155801,
10.6914898955078));
#176148=CARTESIAN_POINT('Ctrl Pts',(18.6049318609852,-21.0667116984082,
10.6983731024294));
#176149=CARTESIAN_POINT('Ctrl Pts',(18.5216064838216,-21.0599742269612,
10.7029563517985));
#176150=CARTESIAN_POINT('Ctrl Pts',(18.2601185176632,-21.0231635594019,
10.7173370130993));
#176151=CARTESIAN_POINT('Ctrl Pts',(18.0853202367127,-20.9752375786342,
10.727017925168));
#176152=CARTESIAN_POINT('Ctrl Pts',(17.8978823138714,-20.8970208991988,
10.7388247297871));
#176153=CARTESIAN_POINT('Ctrl Pts',(17.8771803841266,-20.8879904884649,
10.7401482447523));
#176154=CARTESIAN_POINT('Ctrl Pts',(17.8480006649476,-20.8747022737725,
10.7420432804298));
#176155=CARTESIAN_POINT('Ctrl Pts',(17.8394004628251,-20.8707158515336,
10.7426054945982));
#176156=CARTESIAN_POINT('Ctrl Pts',(17.8254417699695,-20.8641313767579,
10.7435241416538));
#176157=CARTESIAN_POINT('Ctrl Pts',(17.8200668973459,-20.8615682082857,
10.7438793637465));
#176158=CARTESIAN_POINT('Ctrl Pts',(17.8089337632939,-20.8562012698316,
10.7446182815487));
#176159=CARTESIAN_POINT('Ctrl Pts',(17.8031772745161,-20.8533939809112,
10.7450020970094));
#176160=CARTESIAN_POINT('Ctrl Pts',(17.7895799502217,-20.846686375174,10.7459128997777));
#176161=CARTESIAN_POINT('Ctrl Pts',(17.7817504481549,-20.8427634643451,
10.7464406737091));
#176162=CARTESIAN_POINT('Ctrl Pts',(17.7651878395372,-20.834335930139,10.7475642902708));
#176163=CARTESIAN_POINT('Ctrl Pts',(17.7564613274093,-20.8298188662999,
10.7481605624398));
#176164=CARTESIAN_POINT('Ctrl Pts',(17.7328116850041,-20.8173676858811,
10.7497882722988));
#176165=CARTESIAN_POINT('Ctrl Pts',(17.7179518542265,-20.8093154780856,
10.750823855531));
#176166=CARTESIAN_POINT('Ctrl Pts',(17.6715974713707,-20.7834743140046,
10.7540953971307));
#176167=CARTESIAN_POINT('Ctrl Pts',(17.640462742649,-20.7650563467883,10.7563532611225));
#176168=CARTESIAN_POINT('Ctrl Pts',(17.5223271831559,-20.6910222879548,
10.7651576708815));
#176169=CARTESIAN_POINT('Ctrl Pts',(17.4389755575171,-20.6298727551388,
10.7718885583543));
#176170=CARTESIAN_POINT('Ctrl Pts',(17.2487296242411,-20.4676541413711,
10.7883751432879));
#176171=CARTESIAN_POINT('Ctrl Pts',(17.1472350425231,-20.3610489322348,
10.7981784475442));
#176172=CARTESIAN_POINT('Ctrl Pts',(17.0481865570513,-20.232608755723,10.8082923099319));
#176173=CARTESIAN_POINT('Ctrl Pts',(17.0389231444625,-20.2203218183561,
10.8092440311345));
#176174=CARTESIAN_POINT('Ctrl Pts',(17.0263864314903,-20.2033104714594,
10.8105389288538));
#176175=CARTESIAN_POINT('Ctrl Pts',(17.0229974326688,-20.1986724556584,
10.8108896812994));
#176176=CARTESIAN_POINT('Ctrl Pts',(17.0176313651076,-20.1912656224869,
10.8114461123316));
#176177=CARTESIAN_POINT('Ctrl Pts',(17.0156420493707,-20.1885057734634,
10.8116526273709));
#176178=CARTESIAN_POINT('Ctrl Pts',(17.0115381591573,-20.1827832690152,
10.8120791264237));
#176179=CARTESIAN_POINT('Ctrl Pts',(17.0094245702003,-20.1798199524105,
10.8122990375342));
#176180=CARTESIAN_POINT('Ctrl Pts',(17.0043917280901,-20.1727251192859,
10.8128233322706));
#176181=CARTESIAN_POINT('Ctrl Pts',(17.0014795978504,-20.1685885288209,
10.8131272277598));
#176182=CARTESIAN_POINT('Ctrl Pts',(16.9916401219008,-20.1545048794572,
10.8141559659486));
#176183=CARTESIAN_POINT('Ctrl Pts',(16.98478324214,-20.1445085657595,10.8148761624763));
#176184=CARTESIAN_POINT('Ctrl Pts',(16.9468326402009,-20.0881505125467,
10.8188842381444));
#176185=CARTESIAN_POINT('Ctrl Pts',(16.9174936642302,-20.0406280304542,
10.8220673839729));
#176186=CARTESIAN_POINT('Ctrl Pts',(16.8017811735682,-19.8354676295683,
10.8352404974851));
#176187=CARTESIAN_POINT('Ctrl Pts',(16.7337847484734,-19.6683315026262,
10.8446698548588));
#176188=CARTESIAN_POINT('Ctrl Pts',(16.6773854537441,-19.4556376310195,
10.8569814738632));
#176189=CARTESIAN_POINT('Ctrl Pts',(16.6681681805087,-19.416384416081,10.8592625142186));
#176190=CARTESIAN_POINT('Ctrl Pts',(16.6588573271048,-19.3709377599084,
10.8619252916509));
#176191=CARTESIAN_POINT('Ctrl Pts',(16.6576628200196,-19.3649768438394,
10.8622749730256));
#176192=CARTESIAN_POINT('Ctrl Pts',(16.6558534175158,-19.3557411096778,
10.8628174635971));
#176193=CARTESIAN_POINT('Ctrl Pts',(16.6552205440034,-19.3524698179488,
10.8630097492605));
#176194=CARTESIAN_POINT('Ctrl Pts',(16.6491723847003,-19.3208065162759,
10.8648722679232));
#176195=CARTESIAN_POINT('Ctrl Pts',(16.6443315774318,-19.2923089722863,
10.8665591904008));
#176196=CARTESIAN_POINT('Ctrl Pts',(16.6385322991908,-19.2533536220153,
10.8688831245356));
#176197=CARTESIAN_POINT('Ctrl Pts',(16.6370657829552,-19.2429738373706,
10.8695040656248));
#176198=CARTESIAN_POINT('Ctrl Pts',(16.6348620662406,-19.2264935135277,
10.8704928377682));
#176199=CARTESIAN_POINT('Ctrl Pts',(16.6340742197072,-19.2203998322545,
10.8708590649165));
#176200=CARTESIAN_POINT('Ctrl Pts',(16.6325483600413,-19.2081797835257,
10.8715947687167));
#176201=CARTESIAN_POINT('Ctrl Pts',(16.6318105821695,-19.2020534480552,
10.871964248942));
#176202=CARTESIAN_POINT('Ctrl Pts',(16.6303836082939,-19.1897513226952,
10.8727075213834));
#176203=CARTESIAN_POINT('Ctrl Pts',(16.6296947992169,-19.1835755504594,
10.8730813219168));
#176204=CARTESIAN_POINT('Ctrl Pts',(16.6281826817397,-19.1694539840531,
10.873937625165));
#176205=CARTESIAN_POINT('Ctrl Pts',(16.627377140809,-19.1615064186572,10.8744206830002));
#176206=CARTESIAN_POINT('Ctrl Pts',(16.6254321893507,-19.1411706930838,
10.8756596692955));
#176207=CARTESIAN_POINT('Ctrl Pts',(16.6243569721826,-19.1287768311628,
10.8764176001408));
#176208=CARTESIAN_POINT('Ctrl Pts',(16.6190952486464,-19.0612149750404,
10.880565036809));
#176209=CARTESIAN_POINT('Ctrl Pts',(16.6169637967638,-19.0059135563383,
10.8840179255723));
#176210=CARTESIAN_POINT('Ctrl Pts',(16.6170004651128,-18.9505966870723,
10.8875305606756));
#176211=CARTESIAN_POINT('Ctrl Pts',(16.7454193692319,-18.2258897639242,
10.9336112441224));
#176212=CARTESIAN_POINT('Ctrl Pts',(16.7173390189837,-18.3027927434369,
10.9286590665973));
#176213=CARTESIAN_POINT('Ctrl Pts',(16.6936915557445,-18.3814141688881,
10.9237068890722));
#176214=CARTESIAN_POINT('Ctrl Pts',(16.6746638753179,-18.4612620601793,
10.9187547115471));
#176215=CARTESIAN_POINT('Ctrl Pts',(16.6556455653778,-18.5410706290957,
10.9138049728012));
#176216=CARTESIAN_POINT('Ctrl Pts',(16.6412426589815,-18.6221042452712,
10.9088552340553));
#176217=CARTESIAN_POINT('Ctrl Pts',(16.631594073455,-18.7038502064707,10.9039054953094));
#176218=CARTESIAN_POINT('Ctrl Pts',(16.6219454879286,-18.7855961676703,
10.8989557565636));
#176219=CARTESIAN_POINT('Ctrl Pts',(16.6170514009679,-18.8680542455025,
10.8940060178177));
#176220=CARTESIAN_POINT('Ctrl Pts',(16.6170004031077,-18.9506935705328,
10.8890562790718));
#176221=CARTESIAN_POINT('Origin',(18.734,-18.952,0.));
#176222=CARTESIAN_POINT('',(16.7454193692303,-18.2258897639288,11.9535387439396));
#176223=CARTESIAN_POINT('',(16.7460270540484,-18.2261211809512,11.7337477306398));
#176224=CARTESIAN_POINT('',(16.7454193692319,-18.2258897639242,0.));
#176225=CARTESIAN_POINT('Ctrl Pts',(16.7454193692303,-18.2258897639288,
11.9535387439396));
#176226=CARTESIAN_POINT('Ctrl Pts',(16.7451290313697,-18.2266849052409,
11.9534866460791));
#176227=CARTESIAN_POINT('Ctrl Pts',(16.7448391690267,-18.2274802245064,
11.9534345739916));
#176228=CARTESIAN_POINT('Ctrl Pts',(16.7420974951151,-18.2350168291508,
11.952941484476));
#176229=CARTESIAN_POINT('Ctrl Pts',(16.7396794456739,-18.2417704693304,
11.9525023189287));
#176230=CARTESIAN_POINT('Ctrl Pts',(16.7359349681624,-18.2523987577304,
11.9518155754438));
#176231=CARTESIAN_POINT('Ctrl Pts',(16.7345854012106,-18.2562651133931,
11.9515666584617));
#176232=CARTESIAN_POINT('Ctrl Pts',(16.7320789914993,-18.2635132174528,
11.9511017521223));
#176233=CARTESIAN_POINT('Ctrl Pts',(16.7309195068626,-18.2668939408757,
11.9508856127554));
#176234=CARTESIAN_POINT('Ctrl Pts',(16.728286071218,-18.2746361171363,11.9503922299608));
#176235=CARTESIAN_POINT('Ctrl Pts',(16.7268177843428,-18.2789994442898,
11.9501153232214));
#176236=CARTESIAN_POINT('Ctrl Pts',(16.7223273436014,-18.2924891612093,
11.9492626928028));
#176237=CARTESIAN_POINT('Ctrl Pts',(16.7193530651715,-18.3016315207151,
11.9486897185535));
#176238=CARTESIAN_POINT('Ctrl Pts',(16.69054739244,-18.3922687618546,11.9430544785594));
#176239=CARTESIAN_POINT('Ctrl Pts',(16.6696094557974,-18.4752476026412,
11.9382547544529));
#176240=CARTESIAN_POINT('Ctrl Pts',(16.6294008149711,-18.6882314405354,
11.9263203751348));
#176241=CARTESIAN_POINT('Ctrl Pts',(16.6170990834496,-18.8191723022085,
11.9193213252498));
#176242=CARTESIAN_POINT('Ctrl Pts',(16.6169313784565,-19.0426470627529,
11.9069620326645));
#176243=CARTESIAN_POINT('Ctrl Pts',(16.6228899848523,-19.1347783275372,
11.9017508294066));
#176244=CARTESIAN_POINT('Ctrl Pts',(16.6366195089841,-19.2398780656785,
11.8955371718309));
#176245=CARTESIAN_POINT('Ctrl Pts',(16.6385368145142,-19.2535173787598,
11.894725675094));
#176246=CARTESIAN_POINT('Ctrl Pts',(16.6418231765904,-19.2753482581545,
11.8934181960775));
#176247=CARTESIAN_POINT('Ctrl Pts',(16.6431076013751,-19.2835523048294,
11.8929248907268));
#176248=CARTESIAN_POINT('Ctrl Pts',(16.6454726643814,-19.2980981837816,
11.8920466993155));
#176249=CARTESIAN_POINT('Ctrl Pts',(16.6465340101666,-19.3044430795483,
11.8916624300161));
#176250=CARTESIAN_POINT('Ctrl Pts',(16.6488043607967,-19.3176455018698,
11.8908602965971));
#176251=CARTESIAN_POINT('Ctrl Pts',(16.6500183113524,-19.3245020890798,
11.8904422793072));
#176252=CARTESIAN_POINT('Ctrl Pts',(16.6532558830817,-19.3422771150747,
11.8893548269423));
#176253=CARTESIAN_POINT('Ctrl Pts',(16.6553316035485,-19.3531857386245,
11.8886837390985));
#176254=CARTESIAN_POINT('Ctrl Pts',(16.6646897658045,-19.4003426339501,
11.8857662647677));
#176255=CARTESIAN_POINT('Ctrl Pts',(16.6728349226117,-19.4364112056578,
11.8834925041284));
#176256=CARTESIAN_POINT('Ctrl Pts',(16.6969459239199,-19.5315155895575,
11.8773804579494));
#176257=CARTESIAN_POINT('Ctrl Pts',(16.7145314150298,-19.590101218353,11.8734934815245));
#176258=CARTESIAN_POINT('Ctrl Pts',(16.786380727417,-19.7965476692969,11.859377500952));
#176259=CARTESIAN_POINT('Ctrl Pts',(16.8545582245221,-19.9390026063447,
11.8488054461995));
#176260=CARTESIAN_POINT('Ctrl Pts',(16.9705616337224,-20.1249378200564,
11.8345700401006));
#176261=CARTESIAN_POINT('Ctrl Pts',(17.0055074777054,-20.1758517555411,
11.8306273573295));
#176262=CARTESIAN_POINT('Ctrl Pts',(17.0481242954733,-20.232466914524,11.8262535703029));
#176263=CARTESIAN_POINT('Ctrl Pts',(17.0536641383772,-20.2397281581677,
11.8256928242317));
#176264=CARTESIAN_POINT('Ctrl Pts',(17.0620088029932,-20.2505202211737,
11.824860027726));
#176265=CARTESIAN_POINT('Ctrl Pts',(17.0647781105656,-20.2540781898058,
11.8245855691298));
#176266=CARTESIAN_POINT('Ctrl Pts',(17.0697578757739,-20.2604341275253,
11.8240955005831));
#176267=CARTESIAN_POINT('Ctrl Pts',(17.0719640466883,-20.2632353734647,
11.8238795937321));
#176268=CARTESIAN_POINT('Ctrl Pts',(17.0767598347342,-20.2692931887643,
11.823412866063));
#176269=CARTESIAN_POINT('Ctrl Pts',(17.079351969474,-20.2725476917915,11.8231622293202));
#176270=CARTESIAN_POINT('Ctrl Pts',(17.0866261911816,-20.2816256494522,
11.8224633512611));
#176271=CARTESIAN_POINT('Ctrl Pts',(17.0913295933534,-20.2874320546423,
11.822016611016));
#176272=CARTESIAN_POINT('Ctrl Pts',(17.1189522583881,-20.3211658070405,
11.8194219537641));
#176273=CARTESIAN_POINT('Ctrl Pts',(17.1425541404909,-20.3485294993241,
11.8173204180937));
#176274=CARTESIAN_POINT('Ctrl Pts',(17.2209741446432,-20.4348768187709,
11.8106490545618));
#176275=CARTESIAN_POINT('Ctrl Pts',(17.2784621466692,-20.4913448228593,
11.8062219730963));
#176276=CARTESIAN_POINT('Ctrl Pts',(17.4407087500992,-20.6334751469453,
11.794464896498));
#176277=CARTESIAN_POINT('Ctrl Pts',(17.5506774578682,-20.7125984704076,
11.7872133859732));
#176278=CARTESIAN_POINT('Ctrl Pts',(17.7219081254075,-20.8124664558866,
11.7760629870063));
#176279=CARTESIAN_POINT('Ctrl Pts',(17.777766999318,-20.8417837811185,11.7724493392766));
#176280=CARTESIAN_POINT('Ctrl Pts',(17.8461536649455,-20.8738672831149,
11.7680131790284));
#176281=CARTESIAN_POINT('Ctrl Pts',(17.8575065016266,-20.879071380587,11.7672764012017));
#176282=CARTESIAN_POINT('Ctrl Pts',(17.8762116380342,-20.8874462594529,
11.7660616347395));
#176283=CARTESIAN_POINT('Ctrl Pts',(17.8835371573524,-20.8906763648784,
11.7655856854802));
#176284=CARTESIAN_POINT('Ctrl Pts',(17.8967322236305,-20.896405401417,11.7647279354952));
#176285=CARTESIAN_POINT('Ctrl Pts',(17.9025951038541,-20.8989195134094,
11.7643466590406));
#176286=CARTESIAN_POINT('Ctrl Pts',(17.9150971796616,-20.9042138660923,
11.7635332452201));
#176287=CARTESIAN_POINT('Ctrl Pts',(17.9217393573994,-20.9069868169915,
11.7631008656941));
#176288=CARTESIAN_POINT('Ctrl Pts',(17.9396435922347,-20.9143544127663,
11.7619347039349));
#176289=CARTESIAN_POINT('Ctrl Pts',(17.9509311927632,-20.9188859085661,
11.7611987975757));
#176290=CARTESIAN_POINT('Ctrl Pts',(18.007271272777,-20.9409422284897,11.7575216573875));
#176291=CARTESIAN_POINT('Ctrl Pts',(18.0528727102851,-20.9570164206582,
11.7545322772497));
#176292=CARTESIAN_POINT('Ctrl Pts',(18.185439492042,-20.9987008622925,11.7457982265456));
#176293=CARTESIAN_POINT('Ctrl Pts',(18.2735448375389,-21.0203038846941,
11.7399361868778));
#176294=CARTESIAN_POINT('Ctrl Pts',(18.5213236825052,-21.0644392688341,
11.7234139481658));
#176295=CARTESIAN_POINT('Ctrl Pts',(18.6826011555627,-21.0744968926795,
11.7125878646361));
#176296=CARTESIAN_POINT('Ctrl Pts',(18.8634464080747,-21.0651334635202,
11.7012277896952));
#176297=CARTESIAN_POINT('Ctrl Pts',(18.8834149961614,-21.0638154827722,
11.6999848545792));
#176298=CARTESIAN_POINT('Ctrl Pts',(18.9097245880237,-21.0617039136759,
11.698364925974));
#176299=CARTESIAN_POINT('Ctrl Pts',(18.9160842203008,-21.0611645439232,
11.6979747189619));
#176300=CARTESIAN_POINT('Ctrl Pts',(18.9263451340498,-21.0602475448066,
11.6973474550377));
#176301=CARTESIAN_POINT('Ctrl Pts',(18.9302479191835,-21.0598878327771,
11.6971094130369));
#176302=CARTESIAN_POINT('Ctrl Pts',(18.9377538248305,-21.0591750011801,
11.6966526763518));
#176303=CARTESIAN_POINT('Ctrl Pts',(18.9413570417738,-21.0588234772036,
11.6964338976899));
#176304=CARTESIAN_POINT('Ctrl Pts',(18.9498791280524,-21.0579700019049,
11.6959175580283));
#176305=CARTESIAN_POINT('Ctrl Pts',(18.9547972090244,-21.0574600543514,
11.6956204459109));
#176306=CARTESIAN_POINT('Ctrl Pts',(18.971104141749,-21.0557114498484,11.6946380503377));
#176307=CARTESIAN_POINT('Ctrl Pts',(18.9824849514607,-21.0543975552393,
11.6939568638423));
#176308=CARTESIAN_POINT('Ctrl Pts',(19.1213023619589,-21.0372283395965,
11.6856962451954));
#176309=CARTESIAN_POINT('Ctrl Pts',(19.2470709261268,-21.0098989680273,
11.6786989162827));
#176310=CARTESIAN_POINT('Ctrl Pts',(19.5269345964225,-20.9218096773956,
11.6627560944265));
#176311=CARTESIAN_POINT('Ctrl Pts',(19.67792252022,-20.8540774792264,11.6538404551469));
#176312=CARTESIAN_POINT('Ctrl Pts',(19.8397851365438,-20.7574045920512,
11.6428917697373));
#176313=CARTESIAN_POINT('Ctrl Pts',(19.8598518696124,-20.7449595675927,
11.6415090402226));
#176314=CARTESIAN_POINT('Ctrl Pts',(19.8878195113245,-20.7269598977285,
11.639543872987));
#176315=CARTESIAN_POINT('Ctrl Pts',(19.8958974415166,-20.7216825800045,
11.6389717198014));
#176316=CARTESIAN_POINT('Ctrl Pts',(19.9089274486118,-20.7130423953321,
11.6380412851637));
#176317=CARTESIAN_POINT('Ctrl Pts',(19.913901893711,-20.7097133861192,11.6376842783305));
#176318=CARTESIAN_POINT('Ctrl Pts',(19.9242561526218,-20.7027203255881,
11.6369373781025));
#176319=CARTESIAN_POINT('Ctrl Pts',(19.9296333128062,-20.6990524740605,
11.6365473433291));
#176320=CARTESIAN_POINT('Ctrl Pts',(19.9423332736559,-20.6903035236184,
11.635620978014));
#176321=CARTESIAN_POINT('Ctrl Pts',(19.9496410260951,-20.6852008920854,
11.6350838300585));
#176322=CARTESIAN_POINT('Ctrl Pts',(19.9739137702612,-20.6680234415619,
11.633285799285));
#176323=CARTESIAN_POINT('Ctrl Pts',(19.9907323859878,-20.6557447787339,
11.6320170992865));
#176324=CARTESIAN_POINT('Ctrl Pts',(20.0798208976864,-20.5886675688534,
11.6251710596367));
#176325=CARTESIAN_POINT('Ctrl Pts',(20.1486853110398,-20.5295222361244,
11.6194228779019));
#176326=CARTESIAN_POINT('Ctrl Pts',(20.311924953861,-20.3700140739128,11.6046262247822));
#176327=CARTESIAN_POINT('Ctrl Pts',(20.4007047734906,-20.2645176635251,
11.595426390967));
#176328=CARTESIAN_POINT('Ctrl Pts',(20.4911335336766,-20.1329568415172,
11.5850001177481));
#176329=CARTESIAN_POINT('Ctrl Pts',(20.5033652197423,-20.1145506799144,
11.5835638053869));
#176330=CARTESIAN_POINT('Ctrl Pts',(20.5431736663893,-20.0525631052629,
11.5788081830348));
#176331=CARTESIAN_POINT('Ctrl Pts',(20.5694482699565,-20.0081624399646,
11.5755333908071));
#176332=CARTESIAN_POINT('Ctrl Pts',(20.5982039387647,-19.9552484138165,
11.5718189370328));
#176333=CARTESIAN_POINT('Ctrl Pts',(20.6022845056128,-19.9476288048573,
11.5712885005483));
#176334=CARTESIAN_POINT('Ctrl Pts',(20.6084028878481,-19.9360339244516,
11.5704882925831));
#176335=CARTESIAN_POINT('Ctrl Pts',(20.6104749198411,-19.9320769492741,
11.5702164286705));
#176336=CARTESIAN_POINT('Ctrl Pts',(20.6141772140292,-19.9249518682232,
11.5697291347125));
#176337=CARTESIAN_POINT('Ctrl Pts',(20.6158120076387,-19.9217861942259,
11.5695134222468));
#176338=CARTESIAN_POINT('Ctrl Pts',(20.6193531971344,-19.9148862344291,
11.569044977352));
#176339=CARTESIAN_POINT('Ctrl Pts',(20.6212564878531,-19.9111504199832,
11.5687924405615));
#176340=CARTESIAN_POINT('Ctrl Pts',(20.6265875001978,-19.9006093055345,
11.5680828740836));
#176341=CARTESIAN_POINT('Ctrl Pts',(20.6299896370554,-19.8937910387281,
11.5676274205919));
#176342=CARTESIAN_POINT('Ctrl Pts',(20.6504355311775,-19.8522553139292,
11.5648732652217));
#176343=CARTESIAN_POINT('Ctrl Pts',(20.6665632688079,-19.8170921409814,
11.5626278582963));
#176344=CARTESIAN_POINT('Ctrl Pts',(20.7171525708346,-19.6983058236882,
11.5552628194603));
#176345=CARTESIAN_POINT('Ctrl Pts',(20.7472212624142,-19.6129154630708,
11.5503221825712));
#176346=CARTESIAN_POINT('Ctrl Pts',(20.8179978025325,-19.3615918143733,
11.5361254691591));
#176347=CARTESIAN_POINT('Ctrl Pts',(20.8442214334236,-19.1923558174504,
11.5269280730812));
#176348=CARTESIAN_POINT('Ctrl Pts',(20.8506174542962,-18.9985100483466,
11.5156614898658));
#176349=CARTESIAN_POINT('Ctrl Pts',(20.8510012979536,-18.9751964095409,
11.5142958082286));
#176350=CARTESIAN_POINT('Ctrl Pts',(20.8509994609138,-18.9422820921322,
11.5123508577701));
#176351=CARTESIAN_POINT('Ctrl Pts',(20.8509336285808,-18.9326825774612,
11.5117815872653));
#176352=CARTESIAN_POINT('Ctrl Pts',(20.8507208748756,-18.9171079139512,
11.5108545758878));
#176353=CARTESIAN_POINT('Ctrl Pts',(20.8506139347375,-18.9111322871954,
11.5104980910136));
#176354=CARTESIAN_POINT('Ctrl Pts',(20.8503375057484,-18.8986424830744,
11.5097512605741));
#176355=CARTESIAN_POINT('Ctrl Pts',(20.8501632410867,-18.8921284838209,
11.5093607691106));
#176356=CARTESIAN_POINT('Ctrl Pts',(20.84967812505,-18.876665765734,11.5084314482702));
#176357=CARTESIAN_POINT('Ctrl Pts',(20.8493405699849,-18.8677180636594,
11.507891787315));
#176358=CARTESIAN_POINT('Ctrl Pts',(20.8480186877883,-18.8377299039485,
11.5060766111868));
#176359=CARTESIAN_POINT('Ctrl Pts',(20.8467771350606,-18.8167025705487,
11.5047930734651));
#176360=CARTESIAN_POINT('Ctrl Pts',(20.8383803990078,-18.703285233948,11.4978096228056));
#176361=CARTESIAN_POINT('Ctrl Pts',(20.8254795101571,-18.6114336461119,
11.4919310928861));
#176362=CARTESIAN_POINT('Ctrl Pts',(20.775836577602,-18.3728574942928,11.4761164732412));
#176363=CARTESIAN_POINT('Ctrl Pts',(20.7293326848203,-18.2287114025861,
11.4659781783952));
#176364=CARTESIAN_POINT('Ctrl Pts',(20.6444862812803,-18.0381945165704,
11.4524640226368));
#176365=CARTESIAN_POINT('Ctrl Pts',(20.618948293174,-17.9866143313949,11.4487979893458));
#176366=CARTESIAN_POINT('Ctrl Pts',(20.587077525497,-17.9283440397123,11.4446996785264));
#176367=CARTESIAN_POINT('Ctrl Pts',(20.5827676794663,-17.9205806312505,
11.4441545793538));
#176368=CARTESIAN_POINT('Ctrl Pts',(20.5761916553775,-17.9089087715374,
11.4433367157967));
#176369=CARTESIAN_POINT('Ctrl Pts',(20.5739616657005,-17.9049801932793,
11.4430617211631));
#176370=CARTESIAN_POINT('Ctrl Pts',(20.569948658204,-17.8979628833771,11.4425710751942));
#176371=CARTESIAN_POINT('Ctrl Pts',(20.5681704008008,-17.8948715025046,
11.442355123973));
#176372=CARTESIAN_POINT('Ctrl Pts',(20.5643038219199,-17.8881888433521,
11.4418887318417));
#176373=CARTESIAN_POINT('Ctrl Pts',(20.5622127458144,-17.8845992250958,
11.4416384726911));
#176374=CARTESIAN_POINT('Ctrl Pts',(20.5563457178263,-17.874595487962,11.4409417127407));
#176375=CARTESIAN_POINT('Ctrl Pts',(20.5525464433895,-17.8681950199373,
11.4404966983238));
#176376=CARTESIAN_POINT('Ctrl Pts',(20.5303560265555,-17.8312570386012,
11.4379321829172));
#176377=CARTESIAN_POINT('Ctrl Pts',(20.5112284850662,-17.8011659502717,
11.4358578136591));
#176378=CARTESIAN_POINT('Ctrl Pts',(20.4474450096976,-17.7062091528249,
11.429311978285));
#176379=CARTESIAN_POINT('Ctrl Pts',(20.3999252865499,-17.6433428612584,
11.4249771496786));
#176380=CARTESIAN_POINT('Ctrl Pts',(20.2276281177025,-17.4400442664173,
11.4104428664405));
#176381=CARTESIAN_POINT('Ctrl Pts',(20.0877502995649,-17.3136198827431,
11.4004124995281));
#176382=CARTESIAN_POINT('Ctrl Pts',(19.9150047501476,-17.1949013545242,
11.388218921189));
#176383=CARTESIAN_POINT('Ctrl Pts',(19.8967794471314,-17.1827878096589,
11.3869359264506));
#176384=CARTESIAN_POINT('Ctrl Pts',(19.8712833607534,-17.1664058374112,
11.3851443884386));
#176385=CARTESIAN_POINT('Ctrl Pts',(19.8641695629118,-17.1618947762579,
11.3846448734637));
#176386=CARTESIAN_POINT('Ctrl Pts',(19.8518846932427,-17.1542070080992,
11.3837827731188));
#176387=CARTESIAN_POINT('Ctrl Pts',(19.8467264999286,-17.151009837814,11.3834209479963));
#176388=CARTESIAN_POINT('Ctrl Pts',(19.8360543094168,-17.1444583118117,
11.382672623711));
#176389=CARTESIAN_POINT('Ctrl Pts',(19.8305385824702,-17.1411069078584,
11.3822860212385));
#176390=CARTESIAN_POINT('Ctrl Pts',(19.8176502736626,-17.1333563318903,
11.3813829850102));
#176391=CARTESIAN_POINT('Ctrl Pts',(19.8102661239642,-17.1289767049816,
11.3808658450498));
#176392=CARTESIAN_POINT('Ctrl Pts',(19.7864755946789,-17.1150611814342,
11.3792003487391));
#176393=CARTESIAN_POINT('Ctrl Pts',(19.7699679215923,-17.1057011268004,
11.378045668821));
#176394=CARTESIAN_POINT('Ctrl Pts',(19.6864705672357,-17.0598294448661,
11.3722084542298));
#176395=CARTESIAN_POINT('Ctrl Pts',(19.6176745788376,-17.0267398669967,
11.3674064393238));
#176396=CARTESIAN_POINT('Ctrl Pts',(19.4458934726787,-16.9552656247558,
11.3554427339591));
#176397=CARTESIAN_POINT('Ctrl Pts',(19.3414175873303,-16.9210443378806,
11.3481824164327));
#176398=CARTESIAN_POINT('Ctrl Pts',(19.1693169898725,-16.8791454418259,
11.3364828919027));
#176399=CARTESIAN_POINT('Ctrl Pts',(19.1031384871142,-16.866343149384,11.3320467893725));
#176400=CARTESIAN_POINT('Ctrl Pts',(19.035577865389,-16.8565905925698,11.3276415407469));
#176401=CARTESIAN_POINT('Ctrl Pts',(19.0346960587832,-16.8564638695848,
11.3275840644883));
#176402=CARTESIAN_POINT('Ctrl Pts',(19.0183690273553,-16.8541280565072,
11.3265202656629));
#176403=CARTESIAN_POINT('Ctrl Pts',(19.002899569418,-16.8520891736199,11.3255189494647));
#176404=CARTESIAN_POINT('Ctrl Pts',(18.9515895239313,-16.8459027897029,
11.3222224409731));
#176405=CARTESIAN_POINT('Ctrl Pts',(18.9156633223501,-16.8425001885016,
11.3199540831028));
#176406=CARTESIAN_POINT('Ctrl Pts',(18.8725846449321,-16.839529012918,11.3172952456587));
#176407=CARTESIAN_POINT('Ctrl Pts',(18.8655014001075,-16.8390762531264,
11.3168600390575));
#176408=CARTESIAN_POINT('Ctrl Pts',(18.8539248818732,-16.8383947242109,
11.3161521310599));
#176409=CARTESIAN_POINT('Ctrl Pts',(18.8494329856097,-16.8381446440607,
11.3158782792194));
#176410=CARTESIAN_POINT('Ctrl Pts',(18.8413802010849,-16.837722061443,11.315388862573));
#176411=CARTESIAN_POINT('Ctrl Pts',(18.8378196576743,-16.8375442335365,
11.3151730042479));
#176412=CARTESIAN_POINT('Ctrl Pts',(18.8300953662342,-16.8371780093704,
11.3147058890192));
#176413=CARTESIAN_POINT('Ctrl Pts',(18.8259315192207,-16.8369929153963,
11.3144548188415));
#176414=CARTESIAN_POINT('Ctrl Pts',(18.8142677900671,-16.8365089415146,
11.3137535070402));
#176415=CARTESIAN_POINT('Ctrl Pts',(18.8067667393094,-16.8362376451665,
11.3133047834457));
#176416=CARTESIAN_POINT('Ctrl Pts',(18.7625926037332,-16.8348751680644,
11.3106749145689));
#176417=CARTESIAN_POINT('Ctrl Pts',(18.7258951899899,-16.8346975251789,
11.308541633289));
#176418=CARTESIAN_POINT('Ctrl Pts',(18.6066075792878,-16.837221933677,11.3017214832842));
#176419=CARTESIAN_POINT('Ctrl Pts',(18.5241722098006,-16.8438041974536,
11.2971847810895));
#176420=CARTESIAN_POINT('Ctrl Pts',(18.262198199831,-16.8802455989509,11.2827770310715));
#176421=CARTESIAN_POINT('Ctrl Pts',(18.0860701303168,-16.9284032516508,
11.2730315254473));
#176422=CARTESIAN_POINT('Ctrl Pts',(17.8975352559485,-17.007129710186,11.2611530364774));
#176423=CARTESIAN_POINT('Ctrl Pts',(17.8769439725337,-17.0161155455159,
11.259836402694));
#176424=CARTESIAN_POINT('Ctrl Pts',(17.8478917470067,-17.0293480184882,
11.2579495247959));
#176425=CARTESIAN_POINT('Ctrl Pts',(17.8393098243508,-17.0333265094823,
11.2573884766855));
#176426=CARTESIAN_POINT('Ctrl Pts',(17.8253726254387,-17.0399014902429,
11.2564712095513));
#176427=CARTESIAN_POINT('Ctrl Pts',(17.8200010668774,-17.0424633111787,
11.2561161939027));
#176428=CARTESIAN_POINT('Ctrl Pts',(17.8088683755985,-17.0478304860607,
11.2553772810711));
#176429=CARTESIAN_POINT('Ctrl Pts',(17.8031090417456,-17.0506394127566,
11.2549932622602));
#176430=CARTESIAN_POINT('Ctrl Pts',(17.7894934637189,-17.057356656793,11.2540812020395));
#176431=CARTESIAN_POINT('Ctrl Pts',(17.781648636919,-17.0612877340402,11.2535523681956));
#176432=CARTESIAN_POINT('Ctrl Pts',(17.7650495022696,-17.069735150008,11.2524262017514));
#176433=CARTESIAN_POINT('Ctrl Pts',(17.7563018463904,-17.074264036706,11.2518284358722));
#176434=CARTESIAN_POINT('Ctrl Pts',(17.7325789402395,-17.08675670847,11.2501955197829));
#176435=CARTESIAN_POINT('Ctrl Pts',(17.7176675222309,-17.0948395481439,
11.2491561902378));
#176436=CARTESIAN_POINT('Ctrl Pts',(17.6711091087536,-17.1208055174505,
11.2458696200076));
#176437=CARTESIAN_POINT('Ctrl Pts',(17.6398259276486,-17.1393243175908,
11.2436002440543));
#176438=CARTESIAN_POINT('Ctrl Pts',(17.5216997100359,-17.2134240963125,
11.234792448448));
#176439=CARTESIAN_POINT('Ctrl Pts',(17.4384910833157,-17.2745106271483,
11.2280708160822));
#176440=CARTESIAN_POINT('Ctrl Pts',(17.2484788401491,-17.4366021491222,
11.2116009775031));
#176441=CARTESIAN_POINT('Ctrl Pts',(17.1470748224785,-17.5431427985949,
11.2018054480092));
#176442=CARTESIAN_POINT('Ctrl Pts',(17.0481227365419,-17.6714756891822,
11.1917010530353));
#176443=CARTESIAN_POINT('Ctrl Pts',(17.0388812168322,-17.6837346491298,
11.1907515613367));
#176444=CARTESIAN_POINT('Ctrl Pts',(17.0263690634383,-17.7007132551913,
11.1894591898376));
#176445=CARTESIAN_POINT('Ctrl Pts',(17.0229833141161,-17.7053469465696,
11.1891087715995));
#176446=CARTESIAN_POINT('Ctrl Pts',(17.0176211044971,-17.7127485913637,
11.188552738323));
#176447=CARTESIAN_POINT('Ctrl Pts',(17.0156324285234,-17.7155075995335,
11.1883462889346));
#176448=CARTESIAN_POINT('Ctrl Pts',(17.0115287800884,-17.7212298548417,
11.1879198135975));
#176449=CARTESIAN_POINT('Ctrl Pts',(17.0094148001329,-17.7241937684648,
11.1876998610218));
#176450=CARTESIAN_POINT('Ctrl Pts',(17.0043792803727,-17.7312925010446,
11.1871752852511));
#176451=CARTESIAN_POINT('Ctrl Pts',(17.001464883944,-17.7354324085303,11.1868711515815));
#176452=CARTESIAN_POINT('Ctrl Pts',(16.9916096540791,-17.7495390273418,
11.1858407586687));
#176453=CARTESIAN_POINT('Ctrl Pts',(16.9847395997665,-17.7595552104824,
11.1851191658798));
#176454=CARTESIAN_POINT('Ctrl Pts',(16.9466622529028,-17.8161073145345,
11.1810975798336));
#176455=CARTESIAN_POINT('Ctrl Pts',(16.9172232111286,-17.8638126894764,
11.1779030951105));
#176456=CARTESIAN_POINT('Ctrl Pts',(16.8331218727429,-18.013045296126,11.1683245428783));
#176457=CARTESIAN_POINT('Ctrl Pts',(16.7848807143242,-18.1178179015326,
11.1621510647684));
#176458=CARTESIAN_POINT('Ctrl Pts',(16.7454193125899,-18.2258899190484,
11.1558808694255));
#176459=CARTESIAN_POINT('',(16.6169841393337,-18.9509245720249,11.6890562438269));
#176460=CARTESIAN_POINT('Ctrl Pts',(16.6170002731508,-18.9509245835716,
11.6890562436247));
#176461=CARTESIAN_POINT('Ctrl Pts',(16.6169638390757,-19.0226464998436,
11.6847206650338));
#176462=CARTESIAN_POINT('Ctrl Pts',(16.6205764456708,-19.0945164382378,
11.680385086443));
#176463=CARTESIAN_POINT('Ctrl Pts',(16.6278569147557,-19.1661268420297,
11.6760495078521));
#176464=CARTESIAN_POINT('Ctrl Pts',(16.6351262827891,-19.2376280563218,
11.6717205400277));
#176465=CARTESIAN_POINT('Ctrl Pts',(16.6460523594263,-19.3088700336267,
11.6673915722034));
#176466=CARTESIAN_POINT('Ctrl Pts',(16.6606019569669,-19.3794453826474,
11.663062604379));
#176467=CARTESIAN_POINT('Ctrl Pts',(16.6751392352657,-19.4499609750466,
11.6587373019208));
#176468=CARTESIAN_POINT('Ctrl Pts',(16.6932938534711,-19.5198105757981,
11.6544119994625));
#176469=CARTESIAN_POINT('Ctrl Pts',(16.7149810087477,-19.588593522558,11.6500866970042));
#176470=CARTESIAN_POINT('Ctrl Pts',(16.7366573538933,-19.6573421839236,
11.6457635505266));
#176471=CARTESIAN_POINT('Ctrl Pts',(16.7618625956117,-19.725024774734,11.6414404040489));
#176472=CARTESIAN_POINT('Ctrl Pts',(16.7904616388555,-19.7912542158128,
11.6371172575713));
#176473=CARTESIAN_POINT('Ctrl Pts',(16.8190563851712,-19.8574737060992,
11.6327947606345));
#176474=CARTESIAN_POINT('Ctrl Pts',(16.8510437238668,-19.9222400264108,
11.6284722636978));
#176475=CARTESIAN_POINT('Ctrl Pts',(16.8862405216003,-19.9851862900678,
11.6241497667611));
#176476=CARTESIAN_POINT('Ctrl Pts',(16.9214689659601,-20.0481891508306,
11.6198233833218));
#176477=CARTESIAN_POINT('Ctrl Pts',(16.9599123931247,-20.1093682524578,
11.6154969998825));
#176478=CARTESIAN_POINT('Ctrl Pts',(17.0013422781536,-20.1683824311975,
11.6111706164432));
#176479=CARTESIAN_POINT('Ctrl Pts',(17.0427896393186,-20.2274215035574,
11.6068424080298));
#176480=CARTESIAN_POINT('Ctrl Pts',(17.0872256618383,-20.2842934442302,
11.6025141996165));
#176481=CARTESIAN_POINT('Ctrl Pts',(17.1343808833966,-20.3386894684092,
11.5981859912031));
#176482=CARTESIAN_POINT('Ctrl Pts',(17.1816225942444,-20.3931852625252,
11.5938498442485));
#176483=CARTESIAN_POINT('Ctrl Pts',(17.2315931237805,-20.4451957108515,
11.5895136972939));
#176484=CARTESIAN_POINT('Ctrl Pts',(17.2839858438636,-20.4944486853714,
11.5851775503393));
#176485=CARTESIAN_POINT('Ctrl Pts',(17.3330384860336,-20.5405617432754,
11.5811178362297));
#176486=CARTESIAN_POINT('Ctrl Pts',(17.3842137273589,-20.584257877088,11.5770581221201));
#176487=CARTESIAN_POINT('Ctrl Pts',(17.4372361998843,-20.6253477363386,
11.5729984080105));
#176488=CARTESIAN_POINT('Ctrl Pts',(17.494549025663,-20.6697624124625,11.5686101990796));
#176489=CARTESIAN_POINT('Ctrl Pts',(17.5542581954977,-20.7113158984435,
11.5642219901487));
#176490=CARTESIAN_POINT('Ctrl Pts',(17.6160462231313,-20.7497397900656,
11.5598337812178));
#176491=CARTESIAN_POINT('Ctrl Pts',(17.6777425470871,-20.7881066542617,
11.5554520851166));
#176492=CARTESIAN_POINT('Ctrl Pts',(17.7415111977165,-20.8233528921038,
11.5510703890153));
#176493=CARTESIAN_POINT('Ctrl Pts',(17.8070029012398,-20.8552512653063,
11.546688692914));
#176494=CARTESIAN_POINT('Ctrl Pts',(17.8724176467993,-20.8871121553817,
11.5423121456544));
#176495=CARTESIAN_POINT('Ctrl Pts',(17.9395509916041,-20.9156327855723,
11.5379355983948));
#176496=CARTESIAN_POINT('Ctrl Pts',(18.00802753011,-20.9406309292983,11.5335590511351));
#176497=CARTESIAN_POINT('Ctrl Pts',(18.0764606417904,-20.9656132195649,
11.5291852794182));
#176498=CARTESIAN_POINT('Ctrl Pts',(18.14623480501,-20.9870772907212,11.5248115077012));
#176499=CARTESIAN_POINT('Ctrl Pts',(18.2169543269187,-21.0048888844621,
11.5204377359842));
#176500=CARTESIAN_POINT('Ctrl Pts',(18.2876523286393,-21.0226950580752,
11.5160652952207));
#176501=CARTESIAN_POINT('Ctrl Pts',(18.3592946504355,-21.0368508431231,
11.5116928544571));
#176502=CARTESIAN_POINT('Ctrl Pts',(18.4314717388382,-21.0472722141045,
11.5073204136936));
#176503=CARTESIAN_POINT('Ctrl Pts',(18.5036506728172,-21.0576938515615,
11.5029478611262));
#176504=CARTESIAN_POINT('Ctrl Pts',(18.5763639228387,-21.0643808184122,
11.4985753085589));
#176505=CARTESIAN_POINT('Ctrl Pts',(18.6491947479433,-21.0673007042082,
11.4942027559915));
#176506=CARTESIAN_POINT('Ctrl Pts',(18.7221011596252,-21.0702236203718,
11.4898256654242));
#176507=CARTESIAN_POINT('Ctrl Pts',(18.7951249069974,-21.0693716302984,
11.4854485748569));
#176508=CARTESIAN_POINT('Ctrl Pts',(18.8678480060375,-21.0647644713218,
11.4810714842896));
#176509=CARTESIAN_POINT('Ctrl Pts',(18.9406108218612,-21.0601547962048,
11.4766920032306));
#176510=CARTESIAN_POINT('Ctrl Pts',(19.0130721829174,-21.0517859243704,
11.4723125221717));
#176511=CARTESIAN_POINT('Ctrl Pts',(19.084820705146,-21.0397293485605,11.4679330411128));
#176512=CARTESIAN_POINT('Ctrl Pts',(19.1566964011486,-21.0276514025509,
11.463545797453));
#176513=CARTESIAN_POINT('Ctrl Pts',(19.227856263807,-21.0118728040952,11.4591585537933));
#176514=CARTESIAN_POINT('Ctrl Pts',(19.2979011262233,-20.9925157484921,
11.4547713101336));
#176515=CARTESIAN_POINT('Ctrl Pts',(19.3455248831596,-20.9793548159233,
11.4517884071988));
#176516=CARTESIAN_POINT('Ctrl Pts',(19.3926335158208,-20.9645407241657,
11.4488055042639));
#176517=CARTESIAN_POINT('Ctrl Pts',(19.4391069833085,-20.9481245307068,
11.4458226013291));
#176518=CARTESIAN_POINT('Ctrl Pts',(19.507475042724,-20.9239743359732,11.4414343923982));
#176519=CARTESIAN_POINT('Ctrl Pts',(19.5747343896099,-20.8962604871605,
11.4370461834673));
#176520=CARTESIAN_POINT('Ctrl Pts',(19.6404874892068,-20.8651046578563,
11.4326579745364));
#176521=CARTESIAN_POINT('Ctrl Pts',(19.7061430003018,-20.8339950689686,
11.4282762784352));
#176522=CARTESIAN_POINT('Ctrl Pts',(19.7702962696065,-20.7994538454432,
11.4238945823339));
#176523=CARTESIAN_POINT('Ctrl Pts',(19.8325671704115,-20.761651671481,11.4195128862326));
#176524=CARTESIAN_POINT('Ctrl Pts',(19.8947648979524,-20.7238939180816,
11.415136338973));
#176525=CARTESIAN_POINT('Ctrl Pts',(19.9550842407134,-20.6828830753685,
11.4107597917133));
#176526=CARTESIAN_POINT('Ctrl Pts',(20.013168775078,-20.6388361642037,11.4063832444537));
#176527=CARTESIAN_POINT('Ctrl Pts',(20.071216473075,-20.5948171869499,11.4020094727367));
#176528=CARTESIAN_POINT('Ctrl Pts',(20.1270317913337,-20.5477662523015,
11.3976357010197));
#176529=CARTESIAN_POINT('Ctrl Pts',(20.1802876588313,-20.4979434038516,
11.3932619293028));
#176530=CARTESIAN_POINT('Ctrl Pts',(20.2335273203897,-20.4481357166618,
11.3888894885392));
#176531=CARTESIAN_POINT('Ctrl Pts',(20.2842087253977,-20.395558119635,11.3845170477756));
#176532=CARTESIAN_POINT('Ctrl Pts',(20.3320395381811,-20.3405095010154,
11.3801446070121));
#176533=CARTESIAN_POINT('Ctrl Pts',(20.3798715740035,-20.2854594747966,
11.3757720544447));
#176534=CARTESIAN_POINT('Ctrl Pts',(20.4248525580102,-20.2279386669777,
11.3713995018774));
#176535=CARTESIAN_POINT('Ctrl Pts',(20.4667296641659,-20.1682799475942,
11.3670269493101));
#176536=CARTESIAN_POINT('Ctrl Pts',(20.5086502319619,-20.1085593121413,
11.3626498587427));
#176537=CARTESIAN_POINT('Ctrl Pts',(20.5474602125882,-20.0466967307923,
11.3582727681754));
#176538=CARTESIAN_POINT('Ctrl Pts',(20.5829499551954,-19.9830543454071,
11.3538956776081));
#176539=CARTESIAN_POINT('Ctrl Pts',(20.6184590800683,-19.9193772025531,
11.3495161965491));
#176540=CARTESIAN_POINT('Ctrl Pts',(20.6506441436595,-19.8539187535681,
11.3451367154902));
#176541=CARTESIAN_POINT('Ctrl Pts',(20.6793425856619,-19.7870636050088,
11.3407572344312));
#176542=CARTESIAN_POINT('Ctrl Pts',(20.7080918954601,-19.7200899561474,
11.3363699907715));
#176543=CARTESIAN_POINT('Ctrl Pts',(20.7333420751796,-19.6517151168647,
11.3319827471118));
#176544=CARTESIAN_POINT('Ctrl Pts',(20.7549798102578,-19.58234086535,11.327595503452));
#176545=CARTESIAN_POINT('Ctrl Pts',(20.7696913851038,-19.5351730592071,
11.3246126005172));
#176546=CARTESIAN_POINT('Ctrl Pts',(20.7827340876901,-19.4875435673451,
11.3216296975824));
#176547=CARTESIAN_POINT('Ctrl Pts',(20.7940858734221,-19.4395809616124,
11.3186467946476));
#176548=CARTESIAN_POINT('Ctrl Pts',(20.8107857153611,-19.3690222007593,
11.3142585857167));
#176549=CARTESIAN_POINT('Ctrl Pts',(20.8238889631161,-19.2974667533231,
11.3098703767858));
#176550=CARTESIAN_POINT('Ctrl Pts',(20.8332827468938,-19.2253147427305,
11.3054821678549));
#176551=CARTESIAN_POINT('Ctrl Pts',(20.8426625887389,-19.1532698176848,
11.3011004717537));
#176552=CARTESIAN_POINT('Ctrl Pts',(20.8483438339328,-19.0806305615065,
11.2967187756524));
#176553=CARTESIAN_POINT('Ctrl Pts',(20.8502642454991,-19.0078089887226,
11.2923370795512));
#176554=CARTESIAN_POINT('Ctrl Pts',(20.8521824004289,-18.9350729870818,
11.2879605322915));
#176555=CARTESIAN_POINT('Ctrl Pts',(20.8503484880034,-18.8621555742344,
11.2835839850319));
#176556=CARTESIAN_POINT('Ctrl Pts',(20.84475206308,-18.789473915313,11.2792074377723));
#176557=CARTESIAN_POINT('Ctrl Pts',(20.8391591873278,-18.7168383500433,
11.2748336660553));
#176558=CARTESIAN_POINT('Ctrl Pts',(20.8298085704126,-18.6444387218197,
11.2704598943383));
#176559=CARTESIAN_POINT('Ctrl Pts',(20.816741830502,-18.5726908022771,11.2660861226214));
#176560=CARTESIAN_POINT('Ctrl Pts',(20.8036790668443,-18.5009647158674,
11.2617136818578));
#176561=CARTESIAN_POINT('Ctrl Pts',(20.786902511612,-18.4298904187043,11.2573412410943));
#176562=CARTESIAN_POINT('Ctrl Pts',(20.7665052467622,-18.3598755013645,
11.2529688003307));
#176563=CARTESIAN_POINT('Ctrl Pts',(20.7461074603521,-18.2898587937358,
11.2485962477634));
#176564=CARTESIAN_POINT('Ctrl Pts',(20.7220889173527,-18.2209019822774,
11.244223695196));
#176565=CARTESIAN_POINT('Ctrl Pts',(20.6945926588482,-18.1533978299111,
11.2398511426287));
#176566=CARTESIAN_POINT('Ctrl Pts',(20.6670678636894,-18.0858236191891,
11.2354740520614));
#176567=CARTESIAN_POINT('Ctrl Pts',(20.6360583291642,-18.0197055253275,
11.2310969614941));
#176568=CARTESIAN_POINT('Ctrl Pts',(20.6017550792382,-17.9554158520327,
11.2267198709267));
#176569=CARTESIAN_POINT('Ctrl Pts',(20.5674330950343,-17.8910910677612,
11.2223403898678));
#176570=CARTESIAN_POINT('Ctrl Pts',(20.5298140629461,-17.8285971057597,
11.2179609088089));
#176571=CARTESIAN_POINT('Ctrl Pts',(20.4891333854113,-17.7682788337557,
11.2135814277499));
#176572=CARTESIAN_POINT('Ctrl Pts',(20.4483806016486,-17.7078536480194,
11.2091941840902));
#176573=CARTESIAN_POINT('Ctrl Pts',(20.4045556257396,-17.6496122391306,
11.2048069404305));
#176574=CARTESIAN_POINT('Ctrl Pts',(20.3579349545348,-17.5938673616175,
11.2004196967708));
#176575=CARTESIAN_POINT('Ctrl Pts',(20.3262373904725,-17.5559662164717,
11.1974367938359));
#176576=CARTESIAN_POINT('Ctrl Pts',(20.2932482928822,-17.5192184270685,
11.1944538909011));
#176577=CARTESIAN_POINT('Ctrl Pts',(20.2590638380205,-17.4837121229261,
11.1914709879662));
#176578=CARTESIAN_POINT('Ctrl Pts',(20.2087743940131,-17.4314780796656,
11.1870827790353));
#176579=CARTESIAN_POINT('Ctrl Pts',(20.1557001261014,-17.3817287153967,
11.1826945701045));
#176580=CARTESIAN_POINT('Ctrl Pts',(20.1001163804879,-17.3347755149755,
11.1783063611736));
#176581=CARTESIAN_POINT('Ctrl Pts',(20.0446151303687,-17.2878920008886,
11.1739246650723));
#176582=CARTESIAN_POINT('Ctrl Pts',(19.9866121616042,-17.2437967211,11.169542968971));
#176583=CARTESIAN_POINT('Ctrl Pts',(19.9264202255137,-17.2027650227068,
11.1651612728698));
#176584=CARTESIAN_POINT('Ctrl Pts',(19.8662990197384,-17.1617815398247,
11.1607847256101));
#176585=CARTESIAN_POINT('Ctrl Pts',(19.8039943529514,-17.1238547573654,
11.1564081783505));
#176586=CARTESIAN_POINT('Ctrl Pts',(19.7398513412539,-17.0892192616151,
11.1520316310908));
#176587=CARTESIAN_POINT('Ctrl Pts',(19.675749008122,-17.0546057311928,11.1476578593739));
#176588=CARTESIAN_POINT('Ctrl Pts',(19.6098110666878,-17.0232795746615,
11.1432840876569));
#176589=CARTESIAN_POINT('Ctrl Pts',(19.5424096422235,-16.9954308470284,
11.1389103159399));
#176590=CARTESIAN_POINT('Ctrl Pts',(19.4750287282391,-16.9675905938566,
11.1345378751763));
#176591=CARTESIAN_POINT('Ctrl Pts',(19.4061856609216,-16.9432258528359,
11.1301654344128));
#176592=CARTESIAN_POINT('Ctrl Pts',(19.3362735429412,-16.9224789778194,
11.1257929936492));
#176593=CARTESIAN_POINT('Ctrl Pts',(19.2663596373004,-16.901731572303,11.1214204410819));
#176594=CARTESIAN_POINT('Ctrl Pts',(19.1953770897379,-16.8846023517757,
11.1170478885146));
#176595=CARTESIAN_POINT('Ctrl Pts',(19.1237335771408,-16.8711836364424,
11.1126753359472));
#176596=CARTESIAN_POINT('Ctrl Pts',(19.0520157102038,-16.8577509946602,
11.1082982453799));
#176597=CARTESIAN_POINT('Ctrl Pts',(18.9796359837852,-16.8480366356522,
11.1039211548126));
#176598=CARTESIAN_POINT('Ctrl Pts',(18.9070108440333,-16.8420814594286,
11.0995440642452));
#176599=CARTESIAN_POINT('Ctrl Pts',(18.834346040997,-16.8361230308623,11.0951645831863));
#176600=CARTESIAN_POINT('Ctrl Pts',(18.7614360402697,-16.833927887168,11.0907851021274));
#176601=CARTESIAN_POINT('Ctrl Pts',(18.6886982399084,-16.8354847625088,
11.0864056210684));
#176602=CARTESIAN_POINT('Ctrl Pts',(18.6158315122841,-16.8370443974006,
11.0820183774087));
#176603=CARTESIAN_POINT('Ctrl Pts',(18.5431380760581,-16.8423692966915,
11.077631133749));
#176604=CARTESIAN_POINT('Ctrl Pts',(18.4710305707955,-16.851396258381,11.0732438900893));
#176605=CARTESIAN_POINT('Ctrl Pts',(18.4220044154797,-16.8575337224938,
11.0702609871544));
#176606=CARTESIAN_POINT('Ctrl Pts',(18.373248967218,-16.8653814515023,11.0672780842196));
#176607=CARTESIAN_POINT('Ctrl Pts',(18.3248903873721,-16.8749062792316,
11.0642951812848));
#176608=CARTESIAN_POINT('Ctrl Pts',(18.2537491009801,-16.8889184462449,
11.0599069723539));
#176609=CARTESIAN_POINT('Ctrl Pts',(18.1831896640499,-16.9066171190663,
11.055518763423));
#176610=CARTESIAN_POINT('Ctrl Pts',(18.1136230257292,-16.9279393759587,
11.0511305544921));
#176611=CARTESIAN_POINT('Ctrl Pts',(18.0441596358342,-16.9492299870865,
11.0467488583908));
#176612=CARTESIAN_POINT('Ctrl Pts',(17.9756865768825,-16.9741333660322,
11.0423671622896));
#176613=CARTESIAN_POINT('Ctrl Pts',(17.9086046585656,-17.0025355785913,
11.0379854661883));
#176614=CARTESIAN_POINT('Ctrl Pts',(17.8416015668411,-17.0309044162904,
11.0336089189287));
#176615=CARTESIAN_POINT('Ctrl Pts',(17.775986810406,-17.062763733124,11.029232371669));
#176616=CARTESIAN_POINT('Ctrl Pts',(17.7121444440025,-17.0979503181745,
11.0248558244094));
#176617=CARTESIAN_POINT('Ctrl Pts',(17.6483425655001,-17.1331145884041,
11.0204820526924));
#176618=CARTESIAN_POINT('Ctrl Pts',(17.5863112682427,-17.171601707862,11.0161082809754));
#176619=CARTESIAN_POINT('Ctrl Pts',(17.5264117827666,-17.2132016512548,
11.0117345092585));
#176620=CARTESIAN_POINT('Ctrl Pts',(17.466530524905,-17.2547889356452,11.0073620684949));
#176621=CARTESIAN_POINT('Ctrl Pts',(17.4087801868835,-17.299486888407,11.0029896277313));
#176622=CARTESIAN_POINT('Ctrl Pts',(17.3534932447841,-17.3470420258451,
10.9986171869678));
#176623=CARTESIAN_POINT('Ctrl Pts',(17.2982048889918,-17.3945983792732,
10.9942446344004));
#176624=CARTESIAN_POINT('Ctrl Pts',(17.2453804185812,-17.4450117463514,
10.9898720818331));
#176625=CARTESIAN_POINT('Ctrl Pts',(17.1953181280015,-17.49798930651,10.9854995292658));
#176626=CARTESIAN_POINT('Ctrl Pts',(17.1452038808882,-17.551021848779,10.9811224386984));
#176627=CARTESIAN_POINT('Ctrl Pts',(17.0978578691728,-17.6066235460734,
10.9767453481311));
#176628=CARTESIAN_POINT('Ctrl Pts',(17.0535398976928,-17.6644663714863,
10.9723682575638));
#176629=CARTESIAN_POINT('Ctrl Pts',(17.0091977225237,-17.722340787013,10.9679887765048));
#176630=CARTESIAN_POINT('Ctrl Pts',(16.9678871535196,-17.7824583697196,
10.9636092954459));
#176631=CARTESIAN_POINT('Ctrl Pts',(16.9298246475461,-17.8444620559106,
10.9592298143869));
#176632=CARTESIAN_POINT('Ctrl Pts',(16.8916946760363,-17.9065756432192,
10.9548425707272));
#176633=CARTESIAN_POINT('Ctrl Pts',(16.8568244953673,-17.970581586091,10.9504553270675));
#176634=CARTESIAN_POINT('Ctrl Pts',(16.8253843166288,-18.0360987099094,
10.9460680834078));
#176635=CARTESIAN_POINT('Ctrl Pts',(16.8040080246551,-18.0806440408907,
10.943085180473));
#176636=CARTESIAN_POINT('Ctrl Pts',(16.7842163233974,-18.1258874840301,
10.9401022775381));
#176637=CARTESIAN_POINT('Ctrl Pts',(16.7660496141036,-18.1717050053665,
10.9371193746033));
#176638=CARTESIAN_POINT('Ctrl Pts',(16.7589277836804,-18.1896666852772,
10.9359499977764));
#176639=CARTESIAN_POINT('Ctrl Pts',(16.7520500909108,-18.2077303660208,
10.9347806209494));
#176640=CARTESIAN_POINT('Ctrl Pts',(16.7454193692319,-18.2258897639242,
10.9336112441224));
#176641=CARTESIAN_POINT('Ctrl Pts',(16.7460270540486,-18.2261211809509,
11.7337477306398));
#176642=CARTESIAN_POINT('Ctrl Pts',(16.6804602716594,-18.4003673855785,
11.7225565586572));
#176643=CARTESIAN_POINT('Ctrl Pts',(16.6235839437207,-18.6428895340021,
11.7076594081181));
#176644=CARTESIAN_POINT('Ctrl Pts',(16.6137960417384,-18.8895339291486,
11.692762257579));
#176645=CARTESIAN_POINT('Ctrl Pts',(16.6141771461173,-18.9509225630941,
11.6890562790225));
#176646=CARTESIAN_POINT('Origin',(18.734,-18.952,0.));
#176647=CARTESIAN_POINT('',(16.745419233475,-18.2258901357187,12.7565301047573));
#176648=CARTESIAN_POINT('',(16.7454193796745,-18.2258897353253,12.5316746168857));
#176649=CARTESIAN_POINT('',(16.7454193692319,-18.2258897639242,0.));
#176650=CARTESIAN_POINT('',(16.6170000980012,-18.9513558437923,12.7090269898315));
#176651=CARTESIAN_POINT('Ctrl Pts',(16.745419233475,-18.2258901357186,12.7565301047573));
#176652=CARTESIAN_POINT('Ctrl Pts',(16.7109376370553,-18.3203241088848,
12.749989613753));
#176653=CARTESIAN_POINT('Ctrl Pts',(16.6831993464591,-18.4171689088752,
12.7433091961978));
#176654=CARTESIAN_POINT('Ctrl Pts',(16.6461463540984,-18.5930957097835,
12.7314611488217));
#176655=CARTESIAN_POINT('Ctrl Pts',(16.6341942133272,-18.6713528334904,
12.726291292972));
#176656=CARTESIAN_POINT('Ctrl Pts',(16.6241532254521,-18.7761570463455,
12.7196400447783));
#176657=CARTESIAN_POINT('Ctrl Pts',(16.6221401935253,-18.802258693066,12.7180060431816));
#176658=CARTESIAN_POINT('Ctrl Pts',(16.6202046975953,-18.8353509206357,
12.715968455308));
#176659=CARTESIAN_POINT('Ctrl Pts',(16.6198320660307,-18.8423116310697,
12.7155417679485));
#176660=CARTESIAN_POINT('Ctrl Pts',(16.6192953233298,-18.8533599303491,
12.7148676711254));
#176661=CARTESIAN_POINT('Ctrl Pts',(16.6191086714274,-18.8574463017393,
12.7146190317843));
#176662=CARTESIAN_POINT('Ctrl Pts',(16.6187836658968,-18.8650447622431,
12.7141580017202));
#176663=CARTESIAN_POINT('Ctrl Pts',(16.6186422157767,-18.8685566158062,
12.7139454452355));
#176664=CARTESIAN_POINT('Ctrl Pts',(16.6183781730859,-18.8755448805823,
12.7135235017923));
#176665=CARTESIAN_POINT('Ctrl Pts',(16.618255403301,-18.8790212240566,12.7133141063902));
#176666=CARTESIAN_POINT('Ctrl Pts',(16.617993747079,-18.8869868464393,12.7128354206365));
#176667=CARTESIAN_POINT('Ctrl Pts',(16.6178605771841,-18.8914763139796,
12.7125664446215));
#176668=CARTESIAN_POINT('Ctrl Pts',(16.6175253047138,-18.9041387314715,
12.7118100153744));
#176669=CARTESIAN_POINT('Ctrl Pts',(16.617356253433,-18.9123125754478,12.7113243212429));
#176670=CARTESIAN_POINT('Ctrl Pts',(16.6170813858838,-18.9307759513804,
12.7102326704046));
#176671=CARTESIAN_POINT('Ctrl Pts',(16.6170032290559,-18.9410657272419,
12.70962810903));
#176672=CARTESIAN_POINT('Ctrl Pts',(16.6170000980012,-18.9513558437923,
12.7090269898315));
#176673=CARTESIAN_POINT('Ctrl Pts',(16.6170000985844,-18.951353930096,12.7090271016242));
#176674=CARTESIAN_POINT('Ctrl Pts',(16.6169387584984,-19.1523491399336,
12.6972855275493));
#176675=CARTESIAN_POINT('Ctrl Pts',(16.6455011370249,-19.3523727029926,
12.6868409881406));
#176676=CARTESIAN_POINT('Ctrl Pts',(16.7265430572823,-19.6299053113378,
12.6708783895896));
#176677=CARTESIAN_POINT('Ctrl Pts',(16.7564635988091,-19.7127800125277,
12.6659221852056));
#176678=CARTESIAN_POINT('Ctrl Pts',(16.7995999890664,-19.8123520374021,
12.659597526166));
#176679=CARTESIAN_POINT('Ctrl Pts',(16.8080194228569,-19.8310379989043,
12.6583942005727));
#176680=CARTESIAN_POINT('Ctrl Pts',(16.8204635507149,-19.8576189527489,
12.656657572754));
#176681=CARTESIAN_POINT('Ctrl Pts',(16.8242687401447,-19.8656158611914,
12.6561318418787));
#176682=CARTESIAN_POINT('Ctrl Pts',(16.8309531565167,-19.8794394583158,
12.6552172779321));
#176683=CARTESIAN_POINT('Ctrl Pts',(16.8338092647821,-19.8852772394481,
12.6548292530634));
#176684=CARTESIAN_POINT('Ctrl Pts',(16.839353145055,-19.8964777804216,12.6540812698207));
#176685=CARTESIAN_POINT('Ctrl Pts',(16.8420369216835,-19.9018424563047,
12.6537214541484));
#176686=CARTESIAN_POINT('Ctrl Pts',(16.8491287513787,-19.915869201835,12.6527765353977));
#176687=CARTESIAN_POINT('Ctrl Pts',(16.8535736818294,-19.9245123747944,
12.6521901394028));
#176688=CARTESIAN_POINT('Ctrl Pts',(16.8692145486086,-19.9544179033586,
12.6501465724257));
#176689=CARTESIAN_POINT('Ctrl Pts',(16.8807125432645,-19.9755193993012,
12.6486787523838));
#176690=CARTESIAN_POINT('Ctrl Pts',(16.9644713381321,-20.1231958391753,
12.6382181144485));
#176691=CARTESIAN_POINT('Ctrl Pts',(17.0492628607079,-20.2421853723023,
12.628759163819));
#176692=CARTESIAN_POINT('Ctrl Pts',(17.2361826289279,-20.454336360999,12.6100989798091));
#176693=CARTESIAN_POINT('Ctrl Pts',(17.3365605456481,-20.5481328257092,
12.6009691548132));
#176694=CARTESIAN_POINT('Ctrl Pts',(17.4553919521303,-20.6393091050874,
12.5915893604774));
#176695=CARTESIAN_POINT('Ctrl Pts',(17.4655458525329,-20.646955648069,12.5907984450836));
#176696=CARTESIAN_POINT('Ctrl Pts',(17.4811882495519,-20.6585160822712,
12.5895968554965));
#176697=CARTESIAN_POINT('Ctrl Pts',(17.4866274100139,-20.6624958478733,
12.5891821130145));
#176698=CARTESIAN_POINT('Ctrl Pts',(17.4956204221168,-20.6690102133911,
12.5885015577888));
#176699=CARTESIAN_POINT('Ctrl Pts',(17.4991632266578,-20.6715598843255,
12.5882347646989));
#176700=CARTESIAN_POINT('Ctrl Pts',(17.5060264636832,-20.6764670412889,
12.5877204959167));
#176701=CARTESIAN_POINT('Ctrl Pts',(17.5093458592576,-20.6788259375495,
12.5874729258201));
#176702=CARTESIAN_POINT('Ctrl Pts',(17.5126817605774,-20.6811821067182,
12.5872252982733));
#176703=CARTESIAN_POINT('Ctrl Pts',(17.512691448454,-20.6811889492075,12.5872245791417));
#176704=CARTESIAN_POINT('Ctrl Pts',(17.512710858349,-20.6812026580558,12.587223138364));
#176705=CARTESIAN_POINT('Ctrl Pts',(17.5127205805917,-20.6812095245722,
12.5872224167013));
#176706=CARTESIAN_POINT('Ctrl Pts',(17.5127400599372,-20.6812232819797,
12.5872209708083));
#176707=CARTESIAN_POINT('Ctrl Pts',(17.5127498165402,-20.6812301725167,
12.5872202466152));
#176708=CARTESIAN_POINT('Ctrl Pts',(17.5127699763166,-20.6812444099712,
12.5872187502574));
#176709=CARTESIAN_POINT('Ctrl Pts',(17.5127803797835,-20.6812517570789,
12.5872179780724));
#176710=CARTESIAN_POINT('Ctrl Pts',(17.51280135382,-20.6812665690216,12.5872164213223));
#176711=CARTESIAN_POINT('Ctrl Pts',(17.5128119249259,-20.6812740342306,
12.5872156367178));
#176712=CARTESIAN_POINT('Ctrl Pts',(17.5128332384424,-20.6812890853295,
12.5872140548181));
#176713=CARTESIAN_POINT('Ctrl Pts',(17.5128439802992,-20.6812966708236,
12.5872132575644));
#176714=CARTESIAN_POINT('Ctrl Pts',(17.5128656391579,-20.68131196519,12.5872116500824));
#176715=CARTESIAN_POINT('Ctrl Pts',(17.5128765558774,-20.6813196738581,
12.5872108398754));
#176716=CARTESIAN_POINT('Ctrl Pts',(17.5128985675731,-20.6813352167551,
12.5872092062572));
#176717=CARTESIAN_POINT('Ctrl Pts',(17.5129096631058,-20.6813430513719,
12.587208382805));
#176718=CARTESIAN_POINT('Ctrl Pts',(17.5129320361737,-20.6813588487956,
12.5872067224197));
#176719=CARTESIAN_POINT('Ctrl Pts',(17.5129433140281,-20.6813668118228,
12.5872058854632));
#176720=CARTESIAN_POINT('Ctrl Pts',(17.5129660562625,-20.6813828692449,
12.5872041977348));
#176721=CARTESIAN_POINT('Ctrl Pts',(17.5129775202629,-20.6813909633665,
12.5872033469915));
#176722=CARTESIAN_POINT('Ctrl Pts',(17.5158229631571,-20.6833999370059,
12.5869921901589));
#176723=CARTESIAN_POINT('Ctrl Pts',(17.5186618181092,-20.6853938210381,
12.5867823736062));
#176724=CARTESIAN_POINT('Ctrl Pts',(17.525220924777,-20.6899766077734,12.5862995428218));
#176725=CARTESIAN_POINT('Ctrl Pts',(17.5289445907593,-20.6925605428716,
12.5860268688936));
#176726=CARTESIAN_POINT('Ctrl Pts',(17.5402942394825,-20.7003824375166,
12.5852000211581));
#176727=CARTESIAN_POINT('Ctrl Pts',(17.5479464019355,-20.7055824645766,
12.5846483616946));
#176728=CARTESIAN_POINT('Ctrl Pts',(17.6100857169512,-20.7472163998169,
12.5802133160385));
#176729=CARTESIAN_POINT('Ctrl Pts',(17.6662097271447,-20.781155800408,12.5764835169958));
#176730=CARTESIAN_POINT('Ctrl Pts',(17.8585115394434,-20.8855713347812,
12.5642916148332));
#176731=CARTESIAN_POINT('Ctrl Pts',(18.0007454983207,-20.9438635182883,
12.5561801606446));
#176732=CARTESIAN_POINT('Ctrl Pts',(18.2068817673174,-21.0032400936249,
12.5443080186182));
#176733=CARTESIAN_POINT('Ctrl Pts',(18.2664347852464,-21.0176285926644,
12.540870094101));
#176734=CARTESIAN_POINT('Ctrl Pts',(18.362847280636,-21.0365394573643,12.5352306100049));
#176735=CARTESIAN_POINT('Ctrl Pts',(18.3993487191498,-21.0427097755614,
12.533079160296));
#176736=CARTESIAN_POINT('Ctrl Pts',(18.4469898674044,-21.0494836331061,
12.5302424811072));
#176737=CARTESIAN_POINT('Ctrl Pts',(18.4580001124448,-21.0509608053313,
12.5295849394513));
#176738=CARTESIAN_POINT('Ctrl Pts',(18.4759307960182,-21.0532229264647,
12.5285107194485));
#176739=CARTESIAN_POINT('Ctrl Pts',(18.4828444693868,-21.0540605125461,
12.5280957078072));
#176740=CARTESIAN_POINT('Ctrl Pts',(18.4961518778526,-21.0556061064271,
12.5272952759627));
#176741=CARTESIAN_POINT('Ctrl Pts',(18.5025449627141,-21.056319116604,12.5269100183782));
#176742=CARTESIAN_POINT('Ctrl Pts',(18.5171959173523,-21.0578855405652,
12.5260254427567));
#176743=CARTESIAN_POINT('Ctrl Pts',(18.5254557174255,-21.0587195350482,
12.5255255184606));
#176744=CARTESIAN_POINT('Ctrl Pts',(18.5474242848536,-21.0608072464684,
12.5241925233397));
#176745=CARTESIAN_POINT('Ctrl Pts',(18.5611405658324,-21.0619758534661,
12.5233567920771));
#176746=CARTESIAN_POINT('Ctrl Pts',(18.666550141721,-21.069921877109,12.5169066518896));
#176747=CARTESIAN_POINT('Ctrl Pts',(18.7585737897712,-21.0708522280832,
12.5111091269597));
#176748=CARTESIAN_POINT('Ctrl Pts',(18.9909055698545,-21.0580632370058,
12.4960736927044));
#176749=CARTESIAN_POINT('Ctrl Pts',(19.1303286609935,-21.0363276217036,
12.4866630167631));
#176750=CARTESIAN_POINT('Ctrl Pts',(19.3179759046464,-20.9875551404384,
12.4739796095789));
#176751=CARTESIAN_POINT('Ctrl Pts',(19.3688867110647,-20.9722554831229,
12.4705406573022));
#176752=CARTESIAN_POINT('Ctrl Pts',(19.4454171487295,-20.9460772571932,
12.4654251230767));
#176753=CARTESIAN_POINT('Ctrl Pts',(19.471485893641,-20.9365838846983,12.4636924881725));
#176754=CARTESIAN_POINT('Ctrl Pts',(19.50378263953,-20.9240981403221,12.4615648784054));
#176755=CARTESIAN_POINT('Ctrl Pts',(19.5101913265726,-20.9215845792313,
12.4611436376714));
#176756=CARTESIAN_POINT('Ctrl Pts',(19.5203332228452,-20.9175496207974,
12.4604786444813));
#176757=CARTESIAN_POINT('Ctrl Pts',(19.5240744783274,-20.9160487693766,
12.4602336875952));
#176758=CARTESIAN_POINT('Ctrl Pts',(19.531136059079,-20.9131924853526,12.4597720337456));
#176759=CARTESIAN_POINT('Ctrl Pts',(19.5344571854397,-20.9118393188562,
12.4595552110787));
#176760=CARTESIAN_POINT('Ctrl Pts',(19.5420600916517,-20.908719025256,12.4590595086698));
#176761=CARTESIAN_POINT('Ctrl Pts',(19.5463395171316,-20.9069462819625,
12.4587809723338));
#176762=CARTESIAN_POINT('Ctrl Pts',(19.5577219916981,-20.9021872859304,
12.458041305005));
#176763=CARTESIAN_POINT('Ctrl Pts',(19.5648146896711,-20.8991762440327,
12.4575816355015));
#176764=CARTESIAN_POINT('Ctrl Pts',(19.6153759309035,-20.8773850670431,
12.454312580212));
#176765=CARTESIAN_POINT('Ctrl Pts',(19.6582235658535,-20.8571883700647,
12.4515832835482));
#176766=CARTESIAN_POINT('Ctrl Pts',(19.8433928338141,-20.7621877190933,
12.4398180639204));
#176767=CARTESIAN_POINT('Ctrl Pts',(19.9776098584288,-20.6727483314295,
12.4313328864275));
#176768=CARTESIAN_POINT('Ctrl Pts',(20.1719595324536,-20.5085136753798,
12.4173245874353));
#176769=CARTESIAN_POINT('Ctrl Pts',(20.2394035446849,-20.4433817956119,
12.4120677355598));
#176770=CARTESIAN_POINT('Ctrl Pts',(20.3165393595728,-20.3583096967044,
12.4053794477549));
#176771=CARTESIAN_POINT('Ctrl Pts',(20.330532436469,-20.3424035094087,12.4041362151558));
#176772=CARTESIAN_POINT('Ctrl Pts',(20.3501102097249,-20.3194638335095,
12.4023521424112));
#176773=CARTESIAN_POINT('Ctrl Pts',(20.355892791097,-20.3126003514418,12.4018194635633));
#176774=CARTESIAN_POINT('Ctrl Pts',(20.3658006983028,-20.3006875072799,
12.4008967038198));
#176775=CARTESIAN_POINT('Ctrl Pts',(20.3699466909577,-20.2956554372874,
12.4005074719962));
#176776=CARTESIAN_POINT('Ctrl Pts',(20.3778456198546,-20.2859776029158,
12.3997598964505));
#176777=CARTESIAN_POINT('Ctrl Pts',(20.3816022779119,-20.2813349463847,
12.3994017085141));
#176778=CARTESIAN_POINT('Ctrl Pts',(20.3913309177388,-20.2692072423718,
12.3984671406283));
#176779=CARTESIAN_POINT('Ctrl Pts',(20.3972718000627,-20.2616975241075,
12.3978895221537));
#176780=CARTESIAN_POINT('Ctrl Pts',(20.4174127358698,-20.235879815631,12.3959072370737));
#176781=CARTESIAN_POINT('Ctrl Pts',(20.4313626889712,-20.217379648732,12.3944927539433));
#176782=CARTESIAN_POINT('Ctrl Pts',(20.5468826537919,-20.0588310872862,
12.3824160627589));
#176783=CARTESIAN_POINT('Ctrl Pts',(20.6312175552133,-19.9070715305983,
12.371072494265));
#176784=CARTESIAN_POINT('Ctrl Pts',(20.7294681025797,-19.6645133292593,
12.3537798377189));
#176785=CARTESIAN_POINT('Ctrl Pts',(20.7575877815373,-19.5802218108695,
12.3479253459652));
#176786=CARTESIAN_POINT('Ctrl Pts',(20.7901372059195,-19.4574234435621,
12.339811425075));
#176787=CARTESIAN_POINT('Ctrl Pts',(20.798937023073,-19.4201758014434,12.3374038693267));
#176788=CARTESIAN_POINT('Ctrl Pts',(20.8082684141023,-19.3752697202377,
12.334581364908));
#176789=CARTESIAN_POINT('Ctrl Pts',(20.8097739569206,-19.3678235125622,
12.3341159650303));
#176790=CARTESIAN_POINT('Ctrl Pts',(20.8120472110773,-19.3562602195026,
12.3333974730016));
#176791=CARTESIAN_POINT('Ctrl Pts',(20.8128428257087,-19.3521487763807,
12.3331428341966));
#176792=CARTESIAN_POINT('Ctrl Pts',(20.8142928397379,-19.344534581819,12.3326728219506));
#176793=CARTESIAN_POINT('Ctrl Pts',(20.8149505899459,-19.3410325686837,
12.3324572643964));
#176794=CARTESIAN_POINT('Ctrl Pts',(20.8164140859918,-19.3331306624519,
12.3319722599344));
#176795=CARTESIAN_POINT('Ctrl Pts',(20.8172147287858,-19.3287298793731,
12.3317031056756));
#176796=CARTESIAN_POINT('Ctrl Pts',(20.8195267345964,-19.3157890255295,
12.3309143616869));
#176797=CARTESIAN_POINT('Ctrl Pts',(20.820999594904,-19.3072420477756,12.3303969084771));
#176798=CARTESIAN_POINT('Ctrl Pts',(20.8309784506855,-19.247129913356,12.3267805164844));
#176799=CARTESIAN_POINT('Ctrl Pts',(20.8376256911425,-19.1952698181811,
12.3237788397212));
#176800=CARTESIAN_POINT('Ctrl Pts',(20.8557089524903,-18.99588020985,12.3125092756898));
#176801=CARTESIAN_POINT('Ctrl Pts',(20.8535918344382,-18.8475449365391,
12.3046645302514));
#176802=CARTESIAN_POINT('Ctrl Pts',(20.8272110131162,-18.6269377144654,
12.2924688625413));
#176803=CARTESIAN_POINT('Ctrl Pts',(20.8145292331848,-18.5537605871344,
12.288339082253));
#176804=CARTESIAN_POINT('Ctrl Pts',(20.7886214857222,-18.4401291292198,
12.2816783201896));
#176805=CARTESIAN_POINT('Ctrl Pts',(20.7779752625796,-18.3991473947878,
12.2792246775098));
#176806=CARTESIAN_POINT('Ctrl Pts',(20.762844837689,-18.3473404860542,12.2760455634214));
#176807=CARTESIAN_POINT('Ctrl Pts',(20.7594894287573,-18.3361939680028,
12.2753569542095));
#176808=CARTESIAN_POINT('Ctrl Pts',(20.7539450662766,-18.3183115246201,
12.2742445632182));
#176809=CARTESIAN_POINT('Ctrl Pts',(20.7518139095322,-18.3115578252244,
12.2738226795348));
#176810=CARTESIAN_POINT('Ctrl Pts',(20.7476922206989,-18.2987208809542,
12.2730173763892));
#176811=CARTESIAN_POINT('Ctrl Pts',(20.7457079062284,-18.2926357109243,
12.2726341654605));
#176812=CARTESIAN_POINT('Ctrl Pts',(20.7411175449446,-18.2787723625611,
12.2717577299614));
#176813=CARTESIAN_POINT('Ctrl Pts',(20.7384938348935,-18.2710001806513,
12.2712639260701));
#176814=CARTESIAN_POINT('Ctrl Pts',(20.7315513730298,-18.2508223752519,
12.2699754606284));
#176815=CARTESIAN_POINT('Ctrl Pts',(20.7271622603064,-18.2384414941896,
12.2691784769792));
#176816=CARTESIAN_POINT('Ctrl Pts',(20.6968874511393,-18.1555010677523,
12.2637955428458));
#176817=CARTESIAN_POINT('Ctrl Pts',(20.6673780879971,-18.0863299267917,
12.2590888855984));
#176818=CARTESIAN_POINT('Ctrl Pts',(20.5478302745639,-17.8428761851375,
12.241723105962));
#176819=CARTESIAN_POINT('Ctrl Pts',(20.4373868060522,-17.6797599433705,
12.2284365607606));
#176820=CARTESIAN_POINT('Ctrl Pts',(20.2779186885959,-17.5029404374827,
12.2131811693824));
#176821=CARTESIAN_POINT('Ctrl Pts',(20.2488188000974,-17.47254635569,12.2105277724223));
#176822=CARTESIAN_POINT('Ctrl Pts',(20.2132718230554,-17.4375678664744,
12.2074575205682));
#176823=CARTESIAN_POINT('Ctrl Pts',(20.2076830418903,-17.4321289166766,
12.2069796221389));
#176824=CARTESIAN_POINT('Ctrl Pts',(20.1990156959125,-17.4237866923221,
12.206246045626));
#176825=CARTESIAN_POINT('Ctrl Pts',(20.195958336003,-17.4208616236448,12.2059887175285));
#176826=CARTESIAN_POINT('Ctrl Pts',(20.190312161353,-17.415492087379,12.2055161716218));
#176827=CARTESIAN_POINT('Ctrl Pts',(20.1877259672089,-17.4130450008326,
12.2053007539933));
#176828=CARTESIAN_POINT('Ctrl Pts',(20.1819157175426,-17.4075749915894,
12.2048190797231));
#176829=CARTESIAN_POINT('Ctrl Pts',(20.1786883732793,-17.4045556434437,
12.2045530975841));
#176830=CARTESIAN_POINT('Ctrl Pts',(20.170442699461,-17.3968896679103,12.203877436766));
#176831=CARTESIAN_POINT('Ctrl Pts',(20.1654112213633,-17.3922571711833,
12.2034688138349));
#176832=CARTESIAN_POINT('Ctrl Pts',(20.1365546941091,-17.365946119365,12.201145493204));
#176833=CARTESIAN_POINT('Ctrl Pts',(20.1122583785761,-17.3447879177703,
12.1992674936093));
#176834=CARTESIAN_POINT('Ctrl Pts',(20.0726371808267,-17.3118437632991,
12.1963097891391));
#176835=CARTESIAN_POINT('Ctrl Pts',(20.0576184774976,-17.2996997396068,
12.1952117566252));
#176836=CARTESIAN_POINT('Ctrl Pts',(20.0412973964723,-17.2868679895253,
12.1940405545374));
#176837=CARTESIAN_POINT('Ctrl Pts',(20.0401585879162,-17.2859745385022,
12.1939589475208));
#176838=CARTESIAN_POINT('Ctrl Pts',(20.0209801434389,-17.2709598613527,
12.1925865202655));
#176839=CARTESIAN_POINT('Ctrl Pts',(20.0027129111959,-17.257130849011,12.1913075521928));
#176840=CARTESIAN_POINT('Ctrl Pts',(19.9473633596232,-17.2166254707547,
12.1875044452394));
#176841=CARTESIAN_POINT('Ctrl Pts',(19.9096378810851,-17.190849464661,12.185006783572));
#176842=CARTESIAN_POINT('Ctrl Pts',(19.7788706322771,-17.1075782042713,
12.176566325358));
#176843=CARTESIAN_POINT('Ctrl Pts',(19.6822228443343,-17.0560783369137,
12.1706782295262));
#176844=CARTESIAN_POINT('Ctrl Pts',(19.5315382449814,-16.9902000913379,
12.1615338802592));
#176845=CARTESIAN_POINT('Ctrl Pts',(19.480203254375,-16.9701054035043,12.1584263564109));
#176846=CARTESIAN_POINT('Ctrl Pts',(19.3957343068887,-16.9407879958885,
12.1532823340521));
#176847=CARTESIAN_POINT('Ctrl Pts',(19.3630560922159,-16.9303288460667,
12.1512852234229));
#176848=CARTESIAN_POINT('Ctrl Pts',(19.3197679542108,-16.9176249764081,
12.1486245776851));
#176849=CARTESIAN_POINT('Ctrl Pts',(19.3093734276155,-16.9146607437567,
12.1479845708699));
#176850=CARTESIAN_POINT('Ctrl Pts',(19.2923087968333,-16.9099353898033,
12.14693186345));
#176851=CARTESIAN_POINT('Ctrl Pts',(19.2856518967962,-16.9081270176773,
12.146520704133));
#176852=CARTESIAN_POINT('Ctrl Pts',(19.2727471251941,-16.904689025628,12.14572263557));
#176853=CARTESIAN_POINT('Ctrl Pts',(19.2665003956321,-16.9030553892533,
12.1453358617018));
#176854=CARTESIAN_POINT('Ctrl Pts',(19.2520570053359,-16.8993486848564,
12.1444404822383));
#176855=CARTESIAN_POINT('Ctrl Pts',(19.2438552449605,-16.8972961020417,
12.1439312205101));
#176856=CARTESIAN_POINT('Ctrl Pts',(19.2217585252902,-16.8919065982599,
12.1425569070159));
#176857=CARTESIAN_POINT('Ctrl Pts',(19.2078418963296,-16.888661190097,12.1416889271498));
#176858=CARTESIAN_POINT('Ctrl Pts',(19.0798346869732,-16.8601727615451,
12.1336815866335));
#176859=CARTESIAN_POINT('Ctrl Pts',(18.9638886762455,-16.8442793791146,
12.1262404422541));
#176860=CARTESIAN_POINT('Ctrl Pts',(18.6847501670076,-16.8293266673691,
12.1079811209209));
#176861=CARTESIAN_POINT('Ctrl Pts',(18.5218032703257,-16.8393854483171,
12.0970228893712));
#176862=CARTESIAN_POINT('Ctrl Pts',(18.3296149874438,-16.8737270062533,
12.0846173736403));
#176863=CARTESIAN_POINT('Ctrl Pts',(18.2977461474967,-16.8801822667745,
12.0825798128478));
#176864=CARTESIAN_POINT('Ctrl Pts',(18.2589760673537,-16.8889697827556,
12.0801352602503));
#176865=CARTESIAN_POINT('Ctrl Pts',(18.2519235576139,-16.8906063643655,
12.0796919792357));
#176866=CARTESIAN_POINT('Ctrl Pts',(18.2408809623921,-16.8932286420363,
12.0790002480952));
#176867=CARTESIAN_POINT('Ctrl Pts',(18.2368851928136,-16.8941898146907,
12.0787504271908));
#176868=CARTESIAN_POINT('Ctrl Pts',(18.2294218356467,-16.8960081142196,
12.0782847434123));
#176869=CARTESIAN_POINT('Ctrl Pts',(18.2259536565098,-16.8968623716565,
12.0780687250689));
#176870=CARTESIAN_POINT('Ctrl Pts',(18.2180420208525,-16.8988323614393,
12.0775767986321));
#176871=CARTESIAN_POINT('Ctrl Pts',(18.2136000222378,-16.8999537402073,
12.0773012197026));
#176872=CARTESIAN_POINT('Ctrl Pts',(18.1999589389986,-16.903444562333,12.0764567249938));
#176873=CARTESIAN_POINT('Ctrl Pts',(18.1907719880553,-16.9058615465525,
12.0758904833148));
#176874=CARTESIAN_POINT('Ctrl Pts',(18.1084481485608,-16.9281135743674,
12.0708363939015));
#176875=CARTESIAN_POINT('Ctrl Pts',(18.0364006911938,-16.9518027143419,
12.0665543201682));
#176876=CARTESIAN_POINT('Ctrl Pts',(17.9259491138241,-16.9948160248289,
12.0599935301445));
#176877=CARTESIAN_POINT('Ctrl Pts',(17.8866041397313,-17.0115269160435,
12.0576573699983));
#176878=CARTESIAN_POINT('Ctrl Pts',(17.748509387532,-17.0751813046516,12.0493787639311));
#176879=CARTESIAN_POINT('Ctrl Pts',(17.652922689133,-17.1285661176162,12.0434920638108));
#176880=CARTESIAN_POINT('Ctrl Pts',(17.5160261081469,-17.2195849389946,
12.0343509592961));
#176881=CARTESIAN_POINT('Ctrl Pts',(17.4713725651031,-17.2518548117505,
12.0312452952386));
#176882=CARTESIAN_POINT('Ctrl Pts',(17.4010406323783,-17.3069819832352,
12.0261040770406));
#176883=CARTESIAN_POINT('Ctrl Pts',(17.3745704100411,-17.3287883856939,
12.0241078544905));
#176884=CARTESIAN_POINT('Ctrl Pts',(17.3404706846839,-17.3582993249946,
12.0214482242515));
#176885=CARTESIAN_POINT('Ctrl Pts',(17.3323532447383,-17.3654338459847,
12.020808321938));
#176886=CARTESIAN_POINT('Ctrl Pts',(17.3191448665736,-17.3772233393769,
12.0197557426236));
#176887=CARTESIAN_POINT('Ctrl Pts',(17.3140213605869,-17.3818416508819,
12.019344606174));
#176888=CARTESIAN_POINT('Ctrl Pts',(17.30414563728,-17.3908314651692,12.0185465506995));
#176889=CARTESIAN_POINT('Ctrl Pts',(17.2993906644587,-17.3951998375899,
12.0181597668866));
#176890=CARTESIAN_POINT('Ctrl Pts',(17.2884551786142,-17.4053388645086,
12.0172643187998));
#176891=CARTESIAN_POINT('Ctrl Pts',(17.2822891370255,-17.4111249026102,
12.0167549980764));
#176892=CARTESIAN_POINT('Ctrl Pts',(17.2657938227598,-17.4267905326563,
12.0153804221432));
#176893=CARTESIAN_POINT('Ctrl Pts',(17.2555298075458,-17.4367379195475,
12.0145122370931));
#176894=CARTESIAN_POINT('Ctrl Pts',(17.1621046109403,-17.5291340808477,
12.0064890741994));
#176895=CARTESIAN_POINT('Ctrl Pts',(17.0858314349433,-17.6182327551735,
11.9990309274255));
#176896=CARTESIAN_POINT('Ctrl Pts',(16.9216222661207,-17.8457806349321,
11.9806998371347));
#176897=CARTESIAN_POINT('Ctrl Pts',(16.8416122532993,-17.9890341906866,
11.9696846986281));
#176898=CARTESIAN_POINT('Ctrl Pts',(16.7671124263905,-18.1684279081479,
11.9573528957394));
#176899=CARTESIAN_POINT('Ctrl Pts',(16.7559529427131,-18.1970417197062,
11.9554288751158));
#176900=CARTESIAN_POINT('Ctrl Pts',(16.7454193692303,-18.2258897639288,
11.9535387439396));
#176901=CARTESIAN_POINT('',(16.6163526597653,-18.9538935158516,12.4890562790225));
#176902=CARTESIAN_POINT('Ctrl Pts',(16.6163526597653,-18.9538935158516,
12.4890562790225));
#176903=CARTESIAN_POINT('Ctrl Pts',(16.6150299521963,-19.0968822256806,
12.4804472042752));
#176904=CARTESIAN_POINT('Ctrl Pts',(16.6934796266312,-19.9425183495545,
12.4294461939675));
#176905=CARTESIAN_POINT('Ctrl Pts',(17.8308508893114,-21.2866630207328,
12.336053248099));
#176906=CARTESIAN_POINT('Ctrl Pts',(20.2082246479652,-20.9751142883798,
12.2088774414178));
#176907=CARTESIAN_POINT('Ctrl Pts',(21.2330887928116,-18.8074837650725,
12.0817016347363));
#176908=CARTESIAN_POINT('Ctrl Pts',(19.9651940811972,-16.7724379176221,
11.9545258280548));
#176909=CARTESIAN_POINT('Ctrl Pts',(17.7787242000293,-16.7401230151528,
11.8385411933561));
#176910=CARTESIAN_POINT('Ctrl Pts',(16.9288259315082,-17.7403262487167,
11.7649484942177));
#176911=CARTESIAN_POINT('Ctrl Pts',(16.7460270540486,-18.2261211809509,
11.7337477306398));
#176912=CARTESIAN_POINT('Ctrl Pts',(16.6170008641597,-18.9539128124127,
12.4894293145889));
#176913=CARTESIAN_POINT('Ctrl Pts',(16.61686182884,-18.8000359085997,12.4977958886218));
#176914=CARTESIAN_POINT('Ctrl Pts',(16.6334990646906,-18.6466112287001,
12.5060892767326));
#176915=CARTESIAN_POINT('Ctrl Pts',(16.6718564308235,-18.4725783837167,
12.5163208831024));
#176916=CARTESIAN_POINT('Ctrl Pts',(16.6775034084717,-18.4489066819874,
12.5177296503482));
#176917=CARTESIAN_POINT('Ctrl Pts',(16.686720476686,-18.4130220320893,12.5198939763803));
#176918=CARTESIAN_POINT('Ctrl Pts',(16.6899947797334,-18.4007347774334,
12.5206402325011));
#176919=CARTESIAN_POINT('Ctrl Pts',(16.6962859720509,-18.3779531736438,
12.5220338660587));
#176920=CARTESIAN_POINT('Ctrl Pts',(16.699273754911,-18.3674511831009,12.5226802921767));
#176921=CARTESIAN_POINT('Ctrl Pts',(16.7042882643285,-18.3503296679285,
12.5237408713038));
#176922=CARTESIAN_POINT('Ctrl Pts',(16.706266479128,-18.3436960587008,12.5241534375387));
#176923=CARTESIAN_POINT('Ctrl Pts',(16.7101499741267,-18.3309028720308,
12.5249523335374));
#176924=CARTESIAN_POINT('Ctrl Pts',(16.7120509309033,-18.324742054533,12.5253385178245));
#176925=CARTESIAN_POINT('Ctrl Pts',(16.7164922824257,-18.3105780534125,
12.5262297814064));
#176926=CARTESIAN_POINT('Ctrl Pts',(16.7190521956296,-18.3025811470815,
12.5267354978479));
#176927=CARTESIAN_POINT('Ctrl Pts',(16.7260350616877,-18.2812061871486,
12.528094072565));
#176928=CARTESIAN_POINT('Ctrl Pts',(16.7305440575928,-18.2678568829419,
12.5289497555122));
#176929=CARTESIAN_POINT('Ctrl Pts',(16.7385289853529,-18.2449728425729,
12.5304292889232));
#176930=CARTESIAN_POINT('Ctrl Pts',(16.7419402632179,-18.2354179074198,
12.5310508845614));
#176931=CARTESIAN_POINT('Ctrl Pts',(16.7454193796745,-18.2258897353253,
12.5316746168857));
#176932=CARTESIAN_POINT('Origin',(18.734,-18.952,0.));
#176933=CARTESIAN_POINT('',(16.7454193670368,-18.225889769936,13.5571445045843));
#176934=CARTESIAN_POINT('',(16.7454194046024,-18.225889667056,13.3344632333882));
#176935=CARTESIAN_POINT('',(16.7454193692319,-18.2258897639242,0.));
#176936=CARTESIAN_POINT('Ctrl Pts',(16.7454193670368,-18.225889769936,13.5571445045843));
#176937=CARTESIAN_POINT('Ctrl Pts',(16.7397540777375,-18.2414051615587,
13.5562052486256));
#176938=CARTESIAN_POINT('Ctrl Pts',(16.7342701807751,-18.2569873757464,
13.5552608713158));
#176939=CARTESIAN_POINT('Ctrl Pts',(16.7177768402589,-18.3056645621676,
13.5523054446821));
#176940=CARTESIAN_POINT('Ctrl Pts',(16.7074032789666,-18.338965863775,13.5502759065929));
#176941=CARTESIAN_POINT('Ctrl Pts',(16.6948809077505,-18.3829652340778,
13.5475782018768));
#176942=CARTESIAN_POINT('Ctrl Pts',(16.6919850814778,-18.393446239775,13.546934408309));
#176943=CARTESIAN_POINT('Ctrl Pts',(16.6873806776799,-18.4106257016832,
13.5458770579171));
#176944=CARTESIAN_POINT('Ctrl Pts',(16.6856239155074,-18.4173111221388,
13.5454650691535));
#176945=CARTESIAN_POINT('Ctrl Pts',(16.6822909632511,-18.4302523150924,
13.5446665179402));
#176946=CARTESIAN_POINT('Ctrl Pts',(16.6807105627383,-18.4365069315847,
13.5442800968442));
#176947=CARTESIAN_POINT('Ctrl Pts',(16.6771333675575,-18.4509415646002,
13.5433871686425));
#176948=CARTESIAN_POINT('Ctrl Pts',(16.6751567481575,-18.4591264254561,
13.5428800167108));
#176949=CARTESIAN_POINT('Ctrl Pts',(16.669984661888,-18.4811173186774,13.5415150770491));
#176950=CARTESIAN_POINT('Ctrl Pts',(16.6668789457878,-18.4949438246381,
13.5406544230393));
#176951=CARTESIAN_POINT('Ctrl Pts',(16.6325818101608,-18.6551381186332,
13.5306528456841));
#176952=CARTESIAN_POINT('Ctrl Pts',(16.61686249379,-18.80435730651,13.5210013227026));
#176953=CARTESIAN_POINT('Ctrl Pts',(16.617139475852,-19.1037302275103,13.5012717620163));
#176954=CARTESIAN_POINT('Ctrl Pts',(16.6331712118,-19.2530733037885,13.491256604518));
#176955=CARTESIAN_POINT('Ctrl Pts',(16.6681544973406,-19.414837116752,13.4809318602064));
#176956=CARTESIAN_POINT('Ctrl Pts',(16.671646380384,-19.4301562700134,13.4799597682651));
#176957=CARTESIAN_POINT('Ctrl Pts',(16.6766589549823,-19.45106952283,13.4786417997937));
#176958=CARTESIAN_POINT('Ctrl Pts',(16.6780324476134,-19.4566979190367,
13.4782880009333));
#176959=CARTESIAN_POINT('Ctrl Pts',(16.6802514660687,-19.4656317738238,
13.4777279427419));
#176960=CARTESIAN_POINT('Ctrl Pts',(16.6810818950885,-19.4689409005052,
13.4775208277027));
#176961=CARTESIAN_POINT('Ctrl Pts',(16.6828132680598,-19.4757701724302,
13.4770940975099));
#176962=CARTESIAN_POINT('Ctrl Pts',(16.683715275648,-19.4792900075426,13.476874551018));
#176963=CARTESIAN_POINT('Ctrl Pts',(16.6858857803258,-19.4876700227241,
13.4763527567906));
#176964=CARTESIAN_POINT('Ctrl Pts',(16.6871625310551,-19.4925280815868,
13.4760509848377));
#176965=CARTESIAN_POINT('Ctrl Pts',(16.6915249222324,-19.5088899472461,
13.4750369171376));
#176966=CARTESIAN_POINT('Ctrl Pts',(16.6946904139781,-19.5203724867509,
13.4743290897684));
#176967=CARTESIAN_POINT('Ctrl Pts',(16.7322349568108,-19.6522089362141,
13.466239928194));
#176968=CARTESIAN_POINT('Ctrl Pts',(16.7771311668151,-19.7693305003975,
13.4594083444331));
#176969=CARTESIAN_POINT('Ctrl Pts',(16.9057920165547,-20.0324993917894,
13.4434861959413));
#176970=CARTESIAN_POINT('Ctrl Pts',(16.9970991412317,-20.1738804480263,
13.4344327500289));
#176971=CARTESIAN_POINT('Ctrl Pts',(17.1191104086189,-20.321076989644,13.4233283615741));
#176972=CARTESIAN_POINT('Ctrl Pts',(17.1343922185398,-20.3389012497791,
13.4219533605422));
#176973=CARTESIAN_POINT('Ctrl Pts',(17.1563533934006,-20.3636702364947,
13.4199973617549));
#176974=CARTESIAN_POINT('Ctrl Pts',(17.1627888967527,-20.3708295656282,
13.4194265183191));
#176975=CARTESIAN_POINT('Ctrl Pts',(17.1733018887458,-20.3823657518555,
13.4184976394722));
#176976=CARTESIAN_POINT('Ctrl Pts',(17.1773495381483,-20.3867697087128,
13.4181408702086));
#176977=CARTESIAN_POINT('Ctrl Pts',(17.1858428983935,-20.3959324772972,
13.4173940041625));
#176978=CARTESIAN_POINT('Ctrl Pts',(17.1902920068177,-20.4006880411471,
13.4170037639558));
#176979=CARTESIAN_POINT('Ctrl Pts',(17.2008948582338,-20.4119169140896,
13.4160760657506));
#176980=CARTESIAN_POINT('Ctrl Pts',(17.2070677277317,-20.4183719186616,
13.4155377839533));
#176981=CARTESIAN_POINT('Ctrl Pts',(17.2278430690836,-20.4398233843199,
13.4137320316772));
#176982=CARTESIAN_POINT('Ctrl Pts',(17.2426267152174,-20.4546419398957,
13.4124566518761));
#176983=CARTESIAN_POINT('Ctrl Pts',(17.3232615220208,-20.5331049076727,
13.4055489324444));
#176984=CARTESIAN_POINT('Ctrl Pts',(17.3929622163251,-20.5926369670539,
13.3997422843461));
#176985=CARTESIAN_POINT('Ctrl Pts',(17.5419203156103,-20.7040139376681,
13.3876785442398));
#176986=CARTESIAN_POINT('Ctrl Pts',(17.621246564242,-20.7554369640963,13.3814262533153));
#176987=CARTESIAN_POINT('Ctrl Pts',(17.7685849134921,-20.8375167217566,
13.3702890295538));
#176988=CARTESIAN_POINT('Ctrl Pts',(17.8352936133738,-20.8702094983373,
13.3654068945094));
#176989=CARTESIAN_POINT('Ctrl Pts',(17.942446797182,-20.9159036065538,13.3579381862308));
#176990=CARTESIAN_POINT('Ctrl Pts',(17.9817988017128,-20.9313099197741,
13.3552710728721));
#176991=CARTESIAN_POINT('Ctrl Pts',(18.0286043447873,-20.9480364423398,
13.3522081873186));
#176992=CARTESIAN_POINT('Ctrl Pts',(18.0356335860942,-20.9505066587893,
13.3517510678581));
#176993=CARTESIAN_POINT('Ctrl Pts',(18.0470291413919,-20.9544438201529,
13.3510147963791));
#176994=CARTESIAN_POINT('Ctrl Pts',(18.0513873874972,-20.9559336904257,
13.350734338428));
#176995=CARTESIAN_POINT('Ctrl Pts',(18.0591363518727,-20.9585544676598,
13.3502377330421));
#176996=CARTESIAN_POINT('Ctrl Pts',(18.0625251018282,-20.9596910213093,
13.3500212553869));
#176997=CARTESIAN_POINT('Ctrl Pts',(18.0698013117486,-20.9621109076413,
13.3495579432307));
#176998=CARTESIAN_POINT('Ctrl Pts',(18.0736896093324,-20.9633915449565,
13.3493112681663));
#176999=CARTESIAN_POINT('Ctrl Pts',(18.0843955200033,-20.9668832192623,
13.3486345247886));
#177000=CARTESIAN_POINT('Ctrl Pts',(18.091220757459,-20.9690709497682,13.3482058072698));
#177001=CARTESIAN_POINT('Ctrl Pts',(18.128070493577,-20.9806765608811,13.3459051235433));
#177002=CARTESIAN_POINT('Ctrl Pts',(18.1582927502702,-20.989459338613,13.3440681189388));
#177003=CARTESIAN_POINT('Ctrl Pts',(18.3467774910431,-21.0397048434727,
13.3328547473846));
#177004=CARTESIAN_POINT('Ctrl Pts',(18.50922207078,-21.0633834123684,13.3242094102949));
#177005=CARTESIAN_POINT('Ctrl Pts',(18.789860587336,-21.0715013976389,13.3088409155415));
#177006=CARTESIAN_POINT('Ctrl Pts',(18.9069971518886,-21.0651666466656,
13.3023034532464));
#177007=CARTESIAN_POINT('Ctrl Pts',(19.0371602860946,-21.047229617872,13.2946060361465));
#177008=CARTESIAN_POINT('Ctrl Pts',(19.0512998056803,-21.0451350002011,
13.2937643058659));
#177009=CARTESIAN_POINT('Ctrl Pts',(19.0737683343618,-21.0415736358923,
13.2924174366657));
#177010=CARTESIAN_POINT('Ctrl Pts',(19.08211179143,-21.0401998655191,13.2919152409463));
#177011=CARTESIAN_POINT('Ctrl Pts',(19.0968115305041,-21.0376889716212,
13.291026752646));
#177012=CARTESIAN_POINT('Ctrl Pts',(19.1031712953016,-21.0365726771472,
13.2906411264571));
#177013=CARTESIAN_POINT('Ctrl Pts',(19.1163141430224,-21.0342037543785,
13.2898416265899));
#177014=CARTESIAN_POINT('Ctrl Pts',(19.1230964022442,-21.0329470360179,
13.2894276267389));
#177015=CARTESIAN_POINT('Ctrl Pts',(19.1404886062956,-21.0296363497948,
13.2883622638528));
#177016=CARTESIAN_POINT('Ctrl Pts',(19.151089088065,-21.0275342625146,13.2877093721325));
#177017=CARTESIAN_POINT('Ctrl Pts',(19.1952560362126,-21.0184238881681,
13.2849739345326));
#177018=CARTESIAN_POINT('Ctrl Pts',(19.228664289554,-21.0106820641266,13.282868070604));
#177019=CARTESIAN_POINT('Ctrl Pts',(19.3152007715219,-20.9884006435209,
13.2773137920213));
#177020=CARTESIAN_POINT('Ctrl Pts',(19.367973078019,-20.9725937826712,13.2738269953561));
#177021=CARTESIAN_POINT('Ctrl Pts',(19.5235313261517,-20.9193054228759,
13.2632580143686));
#177022=CARTESIAN_POINT('Ctrl Pts',(19.624087621682,-20.8758999196903,13.2560274373616));
#177023=CARTESIAN_POINT('Ctrl Pts',(19.7612320605562,-20.803639422771,13.2457873985614));
#177024=CARTESIAN_POINT('Ctrl Pts',(19.8009335352184,-20.7810509233245,
13.2427764779824));
#177025=CARTESIAN_POINT('Ctrl Pts',(19.8593554864681,-20.7452612691464,
13.2383012432287));
#177026=CARTESIAN_POINT('Ctrl Pts',(19.878642827034,-20.7330120160716,13.2368162757804));
#177027=CARTESIAN_POINT('Ctrl Pts',(19.8983116101496,-20.7200689923224,
13.2352967385645));
#177028=CARTESIAN_POINT('Ctrl Pts',(19.8988944629857,-20.7196850333835,
13.235251704772));
#177029=CARTESIAN_POINT('Ctrl Pts',(19.9087866268641,-20.7131614745064,
13.2344873130667));
#177030=CARTESIAN_POINT('Ctrl Pts',(19.9180476216383,-20.7069486019535,
13.2337704997697));
#177031=CARTESIAN_POINT('Ctrl Pts',(19.9605358812947,-20.6779552993115,
13.2304777645199));
#177032=CARTESIAN_POINT('Ctrl Pts',(19.9931601425782,-20.6543008498862,
13.2279377298348));
#177033=CARTESIAN_POINT('Ctrl Pts',(20.0309128500806,-20.6252483415888,
13.2250028957476));
#177034=CARTESIAN_POINT('Ctrl Pts',(20.0367107579682,-20.6207383371908,
13.2245523082544));
#177035=CARTESIAN_POINT('Ctrl Pts',(20.0460809079982,-20.6133710040433,
13.2238244799372));
#177036=CARTESIAN_POINT('Ctrl Pts',(20.0496675121696,-20.6105321584274,
13.2235459804113));
#177037=CARTESIAN_POINT('Ctrl Pts',(20.0560378923598,-20.6054562480978,
13.2230515261108));
#177038=CARTESIAN_POINT('Ctrl Pts',(20.0588252303296,-20.6032237470864,
13.2228352519729));
#177039=CARTESIAN_POINT('Ctrl Pts',(20.064811867015,-20.5984038702072,13.2223709036732));
#177040=CARTESIAN_POINT('Ctrl Pts',(20.0680092664162,-20.5958142252089,
13.2221229966954));
#177041=CARTESIAN_POINT('Ctrl Pts',(20.0768287578111,-20.5886284424818,
13.2214393902693));
#177042=CARTESIAN_POINT('Ctrl Pts',(20.0824348441028,-20.5840126244084,
13.2210050874525));
#177043=CARTESIAN_POINT('Ctrl Pts',(20.1132555913394,-20.558368872483,13.218617978693));
#177044=CARTESIAN_POINT('Ctrl Pts',(20.138003692881,-20.5367841619103,13.2167033145511));
#177045=CARTESIAN_POINT('Ctrl Pts',(20.2821385480707,-20.4050452490167,
13.2054953232617));
#177046=CARTESIAN_POINT('Ctrl Pts',(20.3890376791219,-20.282013335719,13.1969092747812));
#177047=CARTESIAN_POINT('Ctrl Pts',(20.5467790335773,-20.0516148386093,
13.1816227856056));
#177048=CARTESIAN_POINT('Ctrl Pts',(20.6046458040868,-19.9499978158022,
13.1751046545738));
#177049=CARTESIAN_POINT('Ctrl Pts',(20.659860107084,-19.8311791747816,13.1674289980549));
#177050=CARTESIAN_POINT('Ctrl Pts',(20.6657502254931,-19.8181606229958,
13.1665875466499));
#177051=CARTESIAN_POINT('Ctrl Pts',(20.6749148631388,-19.7973460660373,
13.1652410403313));
#177052=CARTESIAN_POINT('Ctrl Pts',(20.6782753076995,-19.7895882055193,
13.1647389261077));
#177053=CARTESIAN_POINT('Ctrl Pts',(20.6841200519565,-19.7758704224686,
13.1638505327387));
#177054=CARTESIAN_POINT('Ctrl Pts',(20.6866237373739,-19.7699188400323,
13.1634649195282));
#177055=CARTESIAN_POINT('Ctrl Pts',(20.6917459140025,-19.7575852051199,
13.1626653981998));
#177056=CARTESIAN_POINT('Ctrl Pts',(20.6943605132158,-19.7512016284852,
13.162251363671));
#177057=CARTESIAN_POINT('Ctrl Pts',(20.7009919329376,-19.7347825882444,
13.161185809666));
#177058=CARTESIAN_POINT('Ctrl Pts',(20.7049631388679,-19.7247290230976,
13.1605327604457));
#177059=CARTESIAN_POINT('Ctrl Pts',(20.7212181732176,-19.6826369044582,
13.1577957965077));
#177060=CARTESIAN_POINT('Ctrl Pts',(20.7327985895077,-19.6503339718685,
13.1556885311821));
#177061=CARTESIAN_POINT('Ctrl Pts',(20.7609232956757,-19.5654405682352,
13.150129674959));
#177062=CARTESIAN_POINT('Ctrl Pts',(20.7762066870715,-19.5124626686873,
13.146639623127));
#177063=CARTESIAN_POINT('Ctrl Pts',(20.8156045875079,-19.3527264517247,
13.1360643892891));
#177064=CARTESIAN_POINT('Ctrl Pts',(20.8335284396875,-19.244636657503,13.1288308354333));
#177065=CARTESIAN_POINT('Ctrl Pts',(20.8473035808731,-19.0864493140128,
13.1183419000024));
#177066=CARTESIAN_POINT('Ctrl Pts',(20.8498652528019,-19.0371065782503,
13.1150857622981));
#177067=CARTESIAN_POINT('Ctrl Pts',(20.8509809436253,-18.9709897139606,
13.1107737986976));
#177068=CARTESIAN_POINT('Ctrl Pts',(20.8510649132769,-18.9542580605904,
13.1096870245731));
#177069=CARTESIAN_POINT('Ctrl Pts',(20.8505861283816,-18.884227330431,13.1051610039506));
#177070=CARTESIAN_POINT('Ctrl Pts',(20.848208890954,-18.8309554902276,13.1017727801264));
#177071=CARTESIAN_POINT('Ctrl Pts',(20.8431056135174,-18.7691380252512,
13.0979464593096));
#177072=CARTESIAN_POINT('Ctrl Pts',(20.8423347399558,-18.7604546500727,
13.0974114224516));
#177073=CARTESIAN_POINT('Ctrl Pts',(20.841086278737,-18.7473136364838,13.0966056703895));
#177074=CARTESIAN_POINT('Ctrl Pts',(20.8406481444158,-18.7428524684915,
13.0963328199396));
#177075=CARTESIAN_POINT('Ctrl Pts',(20.8398362409872,-18.7348469955922,
13.0958444751359));
#177076=CARTESIAN_POINT('Ctrl Pts',(20.8394676904449,-18.731302228704,13.0956286928499));
#177077=CARTESIAN_POINT('Ctrl Pts',(20.8386473941704,-18.7236016189139,
13.0951609195154));
#177078=CARTESIAN_POINT('Ctrl Pts',(20.8381922918668,-18.7194461915745,
13.0949091196381));
#177079=CARTESIAN_POINT('Ctrl Pts',(20.8368793044891,-18.7077771083128,
13.0942037046564));
#177080=CARTESIAN_POINT('Ctrl Pts',(20.8359934530151,-18.7002665745964,
13.0937516363689));
#177081=CARTESIAN_POINT('Ctrl Pts',(20.830455660632,-18.6553841811548,13.0910609516067));
#177082=CARTESIAN_POINT('Ctrl Pts',(20.824847096688,-18.6181346172033,13.0888728180889));
#177083=CARTESIAN_POINT('Ctrl Pts',(20.8031134411284,-18.496019612851,13.0817900122105));
#177084=CARTESIAN_POINT('Ctrl Pts',(20.7827888462894,-18.4119859557136,
13.0770590790458));
#177085=CARTESIAN_POINT('Ctrl Pts',(20.7055121139417,-18.1608351397468,
13.062759428103));
#177086=CARTESIAN_POINT('Ctrl Pts',(20.6327808707394,-17.9994106869022,
13.0532808826202));
#177087=CARTESIAN_POINT('Ctrl Pts',(20.5289324871061,-17.8293103912452,
13.0416993708831));
#177088=CARTESIAN_POINT('Ctrl Pts',(20.5166696699022,-17.8099389777776,
13.0403561933104));
#177089=CARTESIAN_POINT('Ctrl Pts',(20.4988645988361,-17.7827981902561,
13.0384378849605));
#177090=CARTESIAN_POINT('Ctrl Pts',(20.4935804376063,-17.7748608394905,
13.0378723803512));
#177091=CARTESIAN_POINT('Ctrl Pts',(20.4849038996384,-17.76201675878,13.0369498357122));
#177092=CARTESIAN_POINT('Ctrl Pts',(20.4815440523285,-17.7570881353827,
13.03659402749));
#177093=CARTESIAN_POINT('Ctrl Pts',(20.4744645819832,-17.7467968502279,
13.0358472574289));
#177094=CARTESIAN_POINT('Ctrl Pts',(20.4707409054794,-17.7414370651996,
13.03545614369));
#177095=CARTESIAN_POINT('Ctrl Pts',(20.4618179253979,-17.7287194160525,
13.0345228379104));
#177096=CARTESIAN_POINT('Ctrl Pts',(20.4565963498529,-17.7213774006869,
13.0339797951546));
#177097=CARTESIAN_POINT('Ctrl Pts',(20.4388204472616,-17.6967176593755,
13.0321413620442));
#177098=CARTESIAN_POINT('Ctrl Pts',(20.4260508916097,-17.6795573727676,
13.0308376660798));
#177099=CARTESIAN_POINT('Ctrl Pts',(20.3549308423918,-17.5869470855236,
13.0236651602311));
#177100=CARTESIAN_POINT('Ctrl Pts',(20.2917998392333,-17.5153226987362,
13.0176067238052));
#177101=CARTESIAN_POINT('Ctrl Pts',(20.1028893331245,-17.3281371873796,
13.000324262642));
#177102=CARTESIAN_POINT('Ctrl Pts',(19.9676555988288,-17.2231624718423,
12.9888143036815));
#177103=CARTESIAN_POINT('Ctrl Pts',(19.7898606076211,-17.1167371733214,
12.9755907225459));
#177104=CARTESIAN_POINT('Ctrl Pts',(19.7579396454261,-17.0987382157179,
12.9732863797859));
#177105=CARTESIAN_POINT('Ctrl Pts',(19.7192637075255,-17.0782349935799,
12.9705907868171));
#177106=CARTESIAN_POINT('Ctrl Pts',(19.7129450074818,-17.0749260674434,
12.9701534098925));
#177107=CARTESIAN_POINT('Ctrl Pts',(19.7026042291792,-17.069577310355,12.9694426877544));
#177108=CARTESIAN_POINT('Ctrl Pts',(19.6985922028414,-17.0675183157266,
12.9691681770724));
#177109=CARTESIAN_POINT('Ctrl Pts',(19.6913960297823,-17.0638542014124,
12.96867805248));
#177110=CARTESIAN_POINT('Ctrl Pts',(19.6882143907067,-17.0622442983973,
12.9684621413788));
#177111=CARTESIAN_POINT('Ctrl Pts',(19.681312048549,-17.0587736035999,12.9679954465931));
#177112=CARTESIAN_POINT('Ctrl Pts',(19.6775899356073,-17.0569157434413,
12.9677448467576));
#177113=CARTESIAN_POINT('Ctrl Pts',(19.6671694597689,-17.051752766001,12.9670461758156));
#177114=CARTESIAN_POINT('Ctrl Pts',(19.660458969413,-17.0484720719851,12.9665996043409));
#177115=CARTESIAN_POINT('Ctrl Pts',(19.6212336124819,-17.0295517387198,
12.9640079149118));
#177116=CARTESIAN_POINT('Ctrl Pts',(19.5883384451109,-17.0147088572662,
12.9619090544536));
#177117=CARTESIAN_POINT('Ctrl Pts',(19.4810317920743,-16.9695555214973,
12.955250124887));
#177118=CARTESIAN_POINT('Ctrl Pts',(19.4052662102834,-16.9426353487972,
12.9508321908856));
#177119=CARTESIAN_POINT('Ctrl Pts',(19.1503059658817,-16.8680828694102,
12.9363521853746));
#177120=CARTESIAN_POINT('Ctrl Pts',(18.9664274996373,-16.8396570639553,
12.9264403975662));
#177121=CARTESIAN_POINT('Ctrl Pts',(18.7590649119399,-16.8350326020103,
12.9143775668019));
#177122=CARTESIAN_POINT('Ctrl Pts',(18.7369239058494,-16.8348862547774,
12.9130796949431));
#177123=CARTESIAN_POINT('Ctrl Pts',(18.706321392983,-16.8351640266937,12.9112706640304));
#177124=CARTESIAN_POINT('Ctrl Pts',(18.6978581448685,-16.8352916104678,
12.9107687689959));
#177125=CARTESIAN_POINT('Ctrl Pts',(18.6833179082467,-16.8355980332273,
12.9099036533708));
#177126=CARTESIAN_POINT('Ctrl Pts',(18.6772404642275,-16.8357523034161,
12.9095412053612));
#177127=CARTESIAN_POINT('Ctrl Pts',(18.6647182574314,-16.8361241477764,
12.9087926119722));
#177128=CARTESIAN_POINT('Ctrl Pts',(18.658273661797,-16.8363449945344,12.9084063678128));
#177129=CARTESIAN_POINT('Ctrl Pts',(18.6432880912628,-16.8369270868709,
12.9075059189655));
#177130=CARTESIAN_POINT('Ctrl Pts',(18.6347481399251,-16.8373106272641,
12.9069910203738));
#177131=CARTESIAN_POINT('Ctrl Pts',(18.6074589418945,-16.8387018884347,
12.905339950942));
#177132=CARTESIAN_POINT('Ctrl Pts',(18.5887210843969,-16.8399073058309,
12.9041976091759));
#177133=CARTESIAN_POINT('Ctrl Pts',(18.4954173678868,-16.8471570580516,
12.8984647549626));
#177134=CARTESIAN_POINT('Ctrl Pts',(18.4212002243108,-16.8569010390327,
12.8937595130517));
#177135=CARTESIAN_POINT('Ctrl Pts',(18.2406583913333,-16.8904115271796,
12.8819630746622));
#177136=CARTESIAN_POINT('Ctrl Pts',(18.1353541948544,-16.9184925143993,
12.8747714025496));
#177137=CARTESIAN_POINT('Ctrl Pts',(17.9193969649913,-16.994315889852,12.8596504024579));
#177138=CARTESIAN_POINT('Ctrl Pts',(17.8096848777122,-17.0436621333496,
12.8517488716262));
#177139=CARTESIAN_POINT('Ctrl Pts',(17.6964353806998,-17.1066710432259,
12.8437444585833));
#177140=CARTESIAN_POINT('Ctrl Pts',(17.688162584794,-17.1113470162397,12.843160736693));
#177141=CARTESIAN_POINT('Ctrl Pts',(17.6759477966824,-17.1183600328319,
12.8423006712227));
#177142=CARTESIAN_POINT('Ctrl Pts',(17.6719815876047,-17.1206543508156,
12.842021686721));
#177143=CARTESIAN_POINT('Ctrl Pts',(17.6650364034486,-17.1247020556958,
12.8415337012998));
#177144=CARTESIAN_POINT('Ctrl Pts',(17.6620542463398,-17.1264498774787,
12.8413243454292));
#177145=CARTESIAN_POINT('Ctrl Pts',(17.6556512776278,-17.1302237132594,
12.8408752306159));
#177146=CARTESIAN_POINT('Ctrl Pts',(17.652231897653,-17.1322520561036,12.8406356262337));
#177147=CARTESIAN_POINT('Ctrl Pts',(17.6451799244936,-17.136462118738,12.8401419234826));
#177148=CARTESIAN_POINT('Ctrl Pts',(17.6415481234872,-17.1386451386098,
12.8398879099939));
#177149=CARTESIAN_POINT('Ctrl Pts',(17.6324202174276,-17.1441691585595,
12.8392500473204));
#177150=CARTESIAN_POINT('Ctrl Pts',(17.6269326955955,-17.1475243546957,
12.838867086624));
#177151=CARTESIAN_POINT('Ctrl Pts',(17.6113368329068,-17.1571579439384,
12.8377798952498));
#177152=CARTESIAN_POINT('Ctrl Pts',(17.6012658514682,-17.1634967276001,
12.8370792964518));
#177153=CARTESIAN_POINT('Ctrl Pts',(17.5675209042162,-17.1851355376233,
12.8347348248868));
#177154=CARTESIAN_POINT('Ctrl Pts',(17.544098305885,-17.2008239329634,12.8331125786159));
#177155=CARTESIAN_POINT('Ctrl Pts',(17.3581666306147,-17.3308141126764,
12.8202170994803));
#177156=CARTESIAN_POINT('Ctrl Pts',(17.2121628972259,-17.4670122003588,
12.8098882853186));
#177157=CARTESIAN_POINT('Ctrl Pts',(17.0417071984194,-17.6779933069495,
12.7947236966457));
#177158=CARTESIAN_POINT('Ctrl Pts',(16.9990658991834,-17.7367016704979,
12.7905873052676));
#177159=CARTESIAN_POINT('Ctrl Pts',(16.9524196872294,-17.8083959362725,
12.7855679569305));
#177160=CARTESIAN_POINT('Ctrl Pts',(16.9454171332413,-17.8193791530976,
12.784799939161));
#177161=CARTESIAN_POINT('Ctrl Pts',(16.9341882116226,-17.8373550918691,
12.7835441029886));
#177162=CARTESIAN_POINT('Ctrl Pts',(16.9299001205676,-17.8443089930049,
12.7830585681133));
#177163=CARTESIAN_POINT('Ctrl Pts',(16.922326592965,-17.8567514516854,12.7821902283659));
#177164=CARTESIAN_POINT('Ctrl Pts',(16.9190255622627,-17.8622304347635,
12.7818080016268));
#177165=CARTESIAN_POINT('Ctrl Pts',(16.9121128752751,-17.8738225015948,
12.7809995722677));
#177166=CARTESIAN_POINT('Ctrl Pts',(16.90850704683,-17.879938952615,12.7805731633502));
#177167=CARTESIAN_POINT('Ctrl Pts',(16.8990295382294,-17.8962018044484,
12.7794397359913));
#177168=CARTESIAN_POINT('Ctrl Pts',(16.8932113128699,-17.9063789281139,
12.7787307951482));
#177169=CARTESIAN_POINT('Ctrl Pts',(16.8663371941056,-17.9543061334403,
12.7753933757275));
#177170=CARTESIAN_POINT('Ctrl Pts',(16.8463573856811,-17.9926448320317,
12.7727268165693));
#177171=CARTESIAN_POINT('Ctrl Pts',(16.7969423861428,-18.0949948546981,
12.7656112185025));
#177172=CARTESIAN_POINT('Ctrl Pts',(16.769532030164,-18.1598529613437,12.7611038352746));
#177173=CARTESIAN_POINT('Ctrl Pts',(16.745419233475,-18.2258901357186,12.7565301047573));
#177174=CARTESIAN_POINT('Ctrl Pts',(16.7454193796745,-18.2258897353253,
12.5316746168857));
#177175=CARTESIAN_POINT('Ctrl Pts',(16.7953825891274,-18.0890567019958,
12.5406319683147));
#177176=CARTESIAN_POINT('Ctrl Pts',(16.8593353085734,-17.9577454254152,
12.550071381493));
#177177=CARTESIAN_POINT('Ctrl Pts',(16.9723432228534,-17.7760228803993,
12.5641884471658));
#177178=CARTESIAN_POINT('Ctrl Pts',(17.0112103367997,-17.719785447589,12.5687174101842));
#177179=CARTESIAN_POINT('Ctrl Pts',(17.0993279127861,-17.6046261183628,
12.5782308960913));
#177180=CARTESIAN_POINT('Ctrl Pts',(17.1492063641352,-17.5462970787643,
12.5831967070055));
#177181=CARTESIAN_POINT('Ctrl Pts',(17.2123286753608,-17.4801226050842,
12.5888934963698));
#177182=CARTESIAN_POINT('Ctrl Pts',(17.2226240058597,-17.4695529290772,
12.5898054030657));
#177183=CARTESIAN_POINT('Ctrl Pts',(17.2360186887604,-17.4560859113639,
12.5909688368337));
#177184=CARTESIAN_POINT('Ctrl Pts',(17.2390171054497,-17.4530893571951,
12.5912278139004));
#177185=CARTESIAN_POINT('Ctrl Pts',(17.2448933532595,-17.4472519325436,
12.5917324727961));
#177186=CARTESIAN_POINT('Ctrl Pts',(17.2477703619008,-17.4444102629199,
12.5919782163282));
#177187=CARTESIAN_POINT('Ctrl Pts',(17.2532122418611,-17.4390659443687,
12.5924404947478));
#177188=CARTESIAN_POINT('Ctrl Pts',(17.2557752935004,-17.4365615952422,
12.5926571602218));
#177189=CARTESIAN_POINT('Ctrl Pts',(17.2616503745035,-17.4308501604457,
12.593151405721));
#177190=CARTESIAN_POINT('Ctrl Pts',(17.2649665253785,-17.4276473815295,
12.593428649504));
#177191=CARTESIAN_POINT('Ctrl Pts',(17.2737994418166,-17.419172037262,12.5941626251894));
#177192=CARTESIAN_POINT('Ctrl Pts',(17.2793343563971,-17.4139183692787,
12.5946179310359));
#177193=CARTESIAN_POINT('Ctrl Pts',(17.3183293418311,-17.3773036286071,
12.5977944975953));
#177194=CARTESIAN_POINT('Ctrl Pts',(17.3527749539149,-17.3470046349497,
12.6004406740512));
#177195=CARTESIAN_POINT('Ctrl Pts',(17.3951824644032,-17.3120796083725,
12.603550664452));
#177196=CARTESIAN_POINT('Ctrl Pts',(17.4022216829578,-17.306357936064,12.6040621917369));
#177197=CARTESIAN_POINT('Ctrl Pts',(17.4099491733159,-17.3001588737882,
12.6046188905966));
#177198=CARTESIAN_POINT('Ctrl Pts',(17.4106011157436,-17.299636513645,12.6046658199872));
#177199=CARTESIAN_POINT('Ctrl Pts',(17.4342094165713,-17.2807436132308,
12.6063638915347));
#177200=CARTESIAN_POINT('Ctrl Pts',(17.4575463733341,-17.2628523717006,
12.6079963931372));
#177201=CARTESIAN_POINT('Ctrl Pts',(17.5992509773371,-17.1588291430084,
12.6176857349932));
#177202=CARTESIAN_POINT('Ctrl Pts',(17.7259175469084,-17.084678858069,12.6254645859661));
#177203=CARTESIAN_POINT('Ctrl Pts',(17.9082090157549,-17.0019610463819,
12.63660735487));
#177204=CARTESIAN_POINT('Ctrl Pts',(17.9580210497439,-16.9816094974997,
12.6396435760365));
#177205=CARTESIAN_POINT('Ctrl Pts',(18.0400903766667,-16.9516736579726,
12.6446720630314));
#177206=CARTESIAN_POINT('Ctrl Pts',(18.0718969361652,-16.9409218343537,
12.6466268836571));
#177207=CARTESIAN_POINT('Ctrl Pts',(18.1142608484227,-16.9277151496887,
12.6492439561571));
#177208=CARTESIAN_POINT('Ctrl Pts',(18.1246015714009,-16.9245781593697,
12.6498837963592));
#177209=CARTESIAN_POINT('Ctrl Pts',(18.1415813665529,-16.9195687615708,
12.6509362994865));
#177210=CARTESIAN_POINT('Ctrl Pts',(18.1482064560571,-16.9176493669129,
12.6513474222978));
#177211=CARTESIAN_POINT('Ctrl Pts',(18.1610514975836,-16.9139959010065,
12.6521454698726));
#177212=CARTESIAN_POINT('Ctrl Pts',(18.167270242815,-16.9122578410928,12.6525322595226));
#177213=CARTESIAN_POINT('Ctrl Pts',(18.1816512760415,-16.9083093689384,
12.6534277481885));
#177214=CARTESIAN_POINT('Ctrl Pts',(18.1898190101251,-16.9061193692287,
12.6539371038416));
#177215=CARTESIAN_POINT('Ctrl Pts',(18.2118290376171,-16.9003589883457,
12.6553118353226));
#177216=CARTESIAN_POINT('Ctrl Pts',(18.2256945515284,-16.8968798307697,
12.6561801420232));
#177217=CARTESIAN_POINT('Ctrl Pts',(18.3536111382608,-16.8661564866326,
12.6642129062706));
#177218=CARTESIAN_POINT('Ctrl Pts',(18.4696875071382,-16.8482961546333,
12.6716813753892));
#177219=CARTESIAN_POINT('Ctrl Pts',(18.7501379817577,-16.828725674465,12.6900475499762));
#177220=CARTESIAN_POINT('Ctrl Pts',(18.9144144661925,-16.8363428478961,
12.7010881716108));
#177221=CARTESIAN_POINT('Ctrl Pts',(19.1068481775076,-16.8678599255837,
12.7134620491664));
#177222=CARTESIAN_POINT('Ctrl Pts',(19.1374173068122,-16.8735606030679,
12.7154087152327));
#177223=CARTESIAN_POINT('Ctrl Pts',(19.1748402553571,-16.8813962589408,
12.7177593564414));
#177224=CARTESIAN_POINT('Ctrl Pts',(19.1818216264899,-16.8828949332069,
12.718196475163));
#177225=CARTESIAN_POINT('Ctrl Pts',(19.192787739894,-16.8853071056056,12.7188807371032));
#177226=CARTESIAN_POINT('Ctrl Pts',(19.1967775718533,-16.8861968560242,
12.7191292036989));
#177227=CARTESIAN_POINT('Ctrl Pts',(19.2042521005376,-16.8878864507214,
12.7195937271743));
#177228=CARTESIAN_POINT('Ctrl Pts',(19.207737307959,-16.8886835565927,12.7198099313323));
#177229=CARTESIAN_POINT('Ctrl Pts',(19.2157168800142,-16.8905298579046,
12.7203040603352));
#177230=CARTESIAN_POINT('Ctrl Pts',(19.220209836522,-16.8915849216637,12.7205816446536));
#177231=CARTESIAN_POINT('Ctrl Pts',(19.2319770181782,-16.8943887974403,
12.7213070563906));
#177232=CARTESIAN_POINT('Ctrl Pts',(19.2392455589961,-16.8961615091662,
12.721753545481));
#177233=CARTESIAN_POINT('Ctrl Pts',(19.2880753492403,-16.908345133074,12.724743237497));
#177234=CARTESIAN_POINT('Ctrl Pts',(19.3293247931082,-16.919977938457,12.727220989108));
#177235=CARTESIAN_POINT('Ctrl Pts',(19.378859274571,-16.9355853540229,12.7301693795168));
#177236=CARTESIAN_POINT('Ctrl Pts',(19.3875052723908,-16.9383708455907,
12.730682992802));
#177237=CARTESIAN_POINT('Ctrl Pts',(19.4096844266208,-16.9456742278369,
12.731998550123));
#177238=CARTESIAN_POINT('Ctrl Pts',(19.4231904463482,-16.9502734725934,
12.7327977477369));
#177239=CARTESIAN_POINT('Ctrl Pts',(19.5716091996105,-17.0024951953984,
12.7415692161289));
#177240=CARTESIAN_POINT('Ctrl Pts',(19.7014120515451,-17.0635413834698,
12.749165013767));
#177241=CARTESIAN_POINT('Ctrl Pts',(19.90378413461,-17.1850984508933,12.762165895393));
#177242=CARTESIAN_POINT('Ctrl Pts',(19.9802486721115,-17.2381746423221,
12.7673866940842));
#177243=CARTESIAN_POINT('Ctrl Pts',(20.0694783863763,-17.3092487069926,
12.7740313407989));
#177244=CARTESIAN_POINT('Ctrl Pts',(20.085786893264,-17.3226423109305,12.7752698471986));
#177245=CARTESIAN_POINT('Ctrl Pts',(20.1087310498337,-17.3420671327836,
12.7770483077694));
#177246=CARTESIAN_POINT('Ctrl Pts',(20.1155331567506,-17.3479004303477,
12.7775801716598));
#177247=CARTESIAN_POINT('Ctrl Pts',(20.1272183604053,-17.3580507916412,
12.7785019677106));
#177248=CARTESIAN_POINT('Ctrl Pts',(20.1321189677088,-17.362347575957,12.7788910556131));
#177249=CARTESIAN_POINT('Ctrl Pts',(20.1414741574155,-17.3706267996846,
12.7796386690936));
#177250=CARTESIAN_POINT('Ctrl Pts',(20.1459318802807,-17.3746056083598,
12.7799970403982));
#177251=CARTESIAN_POINT('Ctrl Pts',(20.1575014868815,-17.3850205746061,
12.7809327816542));
#177252=CARTESIAN_POINT('Ctrl Pts',(20.1645865196243,-17.3914862359164,
12.7815113962661));
#177253=CARTESIAN_POINT('Ctrl Pts',(20.1887073463387,-17.4138007485738,
12.7835006946144));
#177254=CARTESIAN_POINT('Ctrl Pts',(20.2055251866275,-17.4298817529812,
12.7849212887889));
#177255=CARTESIAN_POINT('Ctrl Pts',(20.3440312240785,-17.5667606180304,
12.7969105088962));
#177256=CARTESIAN_POINT('Ctrl Pts',(20.4508723801858,-17.7016336550456,
12.8081469295512));
#177257=CARTESIAN_POINT('Ctrl Pts',(20.5871342162755,-17.9245478486149,
12.8254113663581));
#177258=CARTESIAN_POINT('Ctrl Pts',(20.6290758426579,-18.0041319273194,
12.8313410094519));
#177259=CARTESIAN_POINT('Ctrl Pts',(20.6815953770312,-18.121309793168,12.8395443431179));
#177260=CARTESIAN_POINT('Ctrl Pts',(20.6963944633231,-18.1569010284677,
12.8419694631999));
#177261=CARTESIAN_POINT('Ctrl Pts',(20.712944126124,-18.1999846494188,12.844809751787));
#177262=CARTESIAN_POINT('Ctrl Pts',(20.7156353498323,-18.2071051844952,
12.8452760972875));
#177263=CARTESIAN_POINT('Ctrl Pts',(20.7197486797973,-18.2181684492128,
12.8459957315367));
#177264=CARTESIAN_POINT('Ctrl Pts',(20.7211975509218,-18.2221010627762,
12.846250574659));
#177265=CARTESIAN_POINT('Ctrl Pts',(20.7238565808022,-18.229384969042,12.8467207766399));
#177266=CARTESIAN_POINT('Ctrl Pts',(20.7250699473992,-18.2327349862536,
12.8469363208114));
#177267=CARTESIAN_POINT('Ctrl Pts',(20.7277860844522,-18.2402935864786,
12.8474210598012));
#177268=CARTESIAN_POINT('Ctrl Pts',(20.7292839858799,-18.2445038613987,
12.8476899634007));
#177269=CARTESIAN_POINT('Ctrl Pts',(20.7336431879201,-18.2568805874098,
12.8484772923799));
#177270=CARTESIAN_POINT('Ctrl Pts',(20.736467803333,-18.2650599886678,12.8489935927151));
#177271=CARTESIAN_POINT('Ctrl Pts',(20.7558510926441,-18.3223249176739,
12.8525817392031));
#177272=CARTESIAN_POINT('Ctrl Pts',(20.7706547855483,-18.3719907101684,
12.8555580424725));
#177273=CARTESIAN_POINT('Ctrl Pts',(20.7889978036788,-18.4429476385196,
12.859685062801));
#177274=CARTESIAN_POINT('Ctrl Pts',(20.7940565889579,-18.4638226003992,
12.8608841242494));
#177275=CARTESIAN_POINT('Ctrl Pts',(20.8292168204339,-18.6192042241958,
12.8697211025083));
#177276=CARTESIAN_POINT('Ctrl Pts',(20.8464361234239,-18.7562888512858,
12.8770516681324));
#177277=CARTESIAN_POINT('Ctrl Pts',(20.8526909284411,-18.984813333524,12.8896554717419));
#177278=CARTESIAN_POINT('Ctrl Pts',(20.8493361918441,-19.0756043067693,
12.8947578849793));
#177279=CARTESIAN_POINT('Ctrl Pts',(20.8380619449433,-19.1866195387204,
12.9012593001847));
#177280=CARTESIAN_POINT('Ctrl Pts',(20.8356513405907,-19.207312735762,12.9024821747734));
#177281=CARTESIAN_POINT('Ctrl Pts',(20.8317737298706,-19.2368049283457,
12.9042420604276));
#177282=CARTESIAN_POINT('Ctrl Pts',(20.8305558530335,-19.2456358635337,
12.9047712138997));
#177283=CARTESIAN_POINT('Ctrl Pts',(20.8283522580869,-19.260901262554,12.9056898093815));
#177284=CARTESIAN_POINT('Ctrl Pts',(20.8273925647315,-19.2673394035452,
12.9060784231051));
#177285=CARTESIAN_POINT('Ctrl Pts',(20.8254934735185,-19.2796886839866,
12.9068261815068));
#177286=CARTESIAN_POINT('Ctrl Pts',(20.8245586683405,-19.2856004743193,
12.9071851769834));
#177287=CARTESIAN_POINT('Ctrl Pts',(20.8220516913691,-19.3010303711591,
12.9081248975568));
#177288=CARTESIAN_POINT('Ctrl Pts',(20.8204395199626,-19.3105417556434,
12.9087068881774));
#177289=CARTESIAN_POINT('Ctrl Pts',(20.8146595317652,-19.3432823478781,
12.9107198218279));
#177290=CARTESIAN_POINT('Ctrl Pts',(20.8101684461189,-19.3664520183281,
12.9121609943188));
#177291=CARTESIAN_POINT('Ctrl Pts',(20.7711441683131,-19.5511904291212,
12.9237898335411));
#177292=CARTESIAN_POINT('Ctrl Pts',(20.7181975470318,-19.7082578337931,
12.934592027523));
#177293=CARTESIAN_POINT('Ctrl Pts',(20.5930493756557,-19.9727152551533,
12.9539265624109));
#177294=CARTESIAN_POINT('Ctrl Pts',(20.5282543265012,-20.0827441635174,
12.9623538755103));
#177295=CARTESIAN_POINT('Ctrl Pts',(20.4469595063022,-20.1960267228779,
12.9710015840332));
#177296=CARTESIAN_POINT('Ctrl Pts',(20.4398861615423,-20.2057085692402,
12.9717402867579));
#177297=CARTESIAN_POINT('Ctrl Pts',(20.4297252021208,-20.2193714550986,
12.9727815694726));
#177298=CARTESIAN_POINT('Ctrl Pts',(20.4267051993937,-20.2234021690459,
12.9730886146112));
#177299=CARTESIAN_POINT('Ctrl Pts',(20.4214803080055,-20.2303240706963,
12.9736155926085));
#177300=CARTESIAN_POINT('Ctrl Pts',(20.4192823122238,-20.2332204137115,
12.9738360030218));
#177301=CARTESIAN_POINT('Ctrl Pts',(20.4150096323128,-20.2388205898798,
12.9742619717701));
#177302=CARTESIAN_POINT('Ctrl Pts',(20.4129358810608,-20.241525076194,12.9744675953067));
#177303=CARTESIAN_POINT('Ctrl Pts',(20.4073307631139,-20.2487985591644,
12.9750203972164));
#177304=CARTESIAN_POINT('Ctrl Pts',(20.4037871880083,-20.2533581729778,
12.9753667199411));
#177305=CARTESIAN_POINT('Ctrl Pts',(20.3906100423283,-20.2701711246706,
12.9766431629238));
#177306=CARTESIAN_POINT('Ctrl Pts',(20.3808596222771,-20.2823328014786,
12.97756534501));
#177307=CARTESIAN_POINT('Ctrl Pts',(20.2843015346713,-20.4000807595963,
12.9864949130558));
#177308=CARTESIAN_POINT('Ctrl Pts',(20.1875821062503,-20.4971479439714,
12.9938782275807));
#177309=CARTESIAN_POINT('Ctrl Pts',(19.9630237698075,-20.6826265581204,
13.0096948169346));
#177310=CARTESIAN_POINT('Ctrl Pts',(19.8334828563456,-20.7676810568081,
13.0181143258019));
#177311=CARTESIAN_POINT('Ctrl Pts',(19.6768994536994,-20.8475426753486,
13.0283508671624));
#177312=CARTESIAN_POINT('Ctrl Pts',(19.6578075303315,-20.8569202115095,
13.0295990380894));
#177313=CARTESIAN_POINT('Ctrl Pts',(19.6304507546937,-20.8698492774063,
13.031388972863));
#177314=CARTESIAN_POINT('Ctrl Pts',(19.6222991765641,-20.8736384611988,
13.0319225008756));
#177315=CARTESIAN_POINT('Ctrl Pts',(19.6081915342117,-20.8800873182916,
13.0328462652825));
#177316=CARTESIAN_POINT('Ctrl Pts',(19.6022468120971,-20.8827716118845,
13.0332356475825));
#177317=CARTESIAN_POINT('Ctrl Pts',(19.5908383095093,-20.8878596906219,
13.0339831859697));
#177318=CARTESIAN_POINT('Ctrl Pts',(19.5853765738694,-20.8902679274934,
13.0343411847011));
#177319=CARTESIAN_POINT('Ctrl Pts',(19.571142355586,-20.8964724334231,13.0352745403183));
#177320=CARTESIAN_POINT('Ctrl Pts',(19.5623542891255,-20.9002324129473,
13.0358511294002));
#177321=CARTESIAN_POINT('Ctrl Pts',(19.5322726154318,-20.9128625461953,
13.0378261491551));
#177322=CARTESIAN_POINT('Ctrl Pts',(19.5108602236532,-20.921443886093,13.0392342994339));
#177323=CARTESIAN_POINT('Ctrl Pts',(19.326306323835,-20.9919286662724,13.0513951041409));
#177324=CARTESIAN_POINT('Ctrl Pts',(19.1562576504481,-21.0337807682103,
13.0628424167069));
#177325=CARTESIAN_POINT('Ctrl Pts',(18.8959417254216,-21.0646185923452,
13.0801628129264));
#177326=CARTESIAN_POINT('Ctrl Pts',(18.8082757853792,-21.0695144584377,
13.0859453007544));
#177327=CARTESIAN_POINT('Ctrl Pts',(18.6825553954879,-21.0687159529994,
13.0939733663515));
#177328=CARTESIAN_POINT('Ctrl Pts',(18.6445670799573,-21.0674515218346,
13.0963639261331));
#177329=CARTESIAN_POINT('Ctrl Pts',(18.599062751845,-21.0647087879691,13.0991692089537));
#177330=CARTESIAN_POINT('Ctrl Pts',(18.5914970589351,-21.0642119684073,
13.0996336854787));
#177331=CARTESIAN_POINT('Ctrl Pts',(18.5797601616791,-21.0633778870095,
13.1003510619821));
#177332=CARTESIAN_POINT('Ctrl Pts',(18.5755871019513,-21.0630688913225,
13.1006055010932));
#177333=CARTESIAN_POINT('Ctrl Pts',(18.5678619243686,-21.0624738422157,
13.1010753282678));
#177334=CARTESIAN_POINT('Ctrl Pts',(18.5643096431062,-21.0621911955862,
13.1012908992711));
#177335=CARTESIAN_POINT('Ctrl Pts',(18.5562959071147,-21.0615331947977,
13.1017761649565));
#177336=CARTESIAN_POINT('Ctrl Pts',(18.5518349322269,-21.0611526577067,
13.1020455655842));
#177337=CARTESIAN_POINT('Ctrl Pts',(18.5387170283904,-21.0599917246556,
13.1028357017344));
#177338=CARTESIAN_POINT('Ctrl Pts',(18.5300635387784,-21.0591721514543,
13.1033542894156));
#177339=CARTESIAN_POINT('Ctrl Pts',(18.4689434366683,-21.0530034145317,
13.1069999677989));
#177340=CARTESIAN_POINT('Ctrl Pts',(18.4166831321325,-21.0457481518896,
13.1100279928185));
#177341=CARTESIAN_POINT('Ctrl Pts',(18.3491993660454,-21.0337941039218,
13.1138841982832));
#177342=CARTESIAN_POINT('Ctrl Pts',(18.333685702231,-21.0308666863539,13.114766940754));
#177343=CARTESIAN_POINT('Ctrl Pts',(18.2683553846207,-21.0177804538025,
13.1184737002074));
#177344=CARTESIAN_POINT('Ctrl Pts',(18.2188789466605,-21.0060020544148,
13.121255128417));
#177345=CARTESIAN_POINT('Ctrl Pts',(18.0644203201235,-20.9632986698096,
13.1299802777983));
#177346=CARTESIAN_POINT('Ctrl Pts',(17.961387340135,-20.9260131934354,13.1358712571059));
#177347=CARTESIAN_POINT('Ctrl Pts',(17.8114224938407,-20.8581964004676,
13.1450223107367));
#177348=CARTESIAN_POINT('Ctrl Pts',(17.7620546089211,-20.8335035161518,
13.1481336779481));
#177349=CARTESIAN_POINT('Ctrl Pts',(17.6836215165351,-20.7903615710545,
13.1532834946455));
#177350=CARTESIAN_POINT('Ctrl Pts',(17.6539415157725,-20.7730825620969,
13.1552824397751));
#177351=CARTESIAN_POINT('Ctrl Pts',(17.6154867423497,-20.7494242696181,
13.1579451830577));
#177352=CARTESIAN_POINT('Ctrl Pts',(17.606321106399,-20.7436880919717,13.158585405537));
#177353=CARTESIAN_POINT('Ctrl Pts',(17.5913800202427,-20.7341773699217,
13.1596383772904));
#177354=CARTESIAN_POINT('Ctrl Pts',(17.5855782964891,-20.7304443160173,
13.1600495837561));
#177355=CARTESIAN_POINT('Ctrl Pts',(17.5743824819919,-20.7231628661379,
13.1608476792434));
#177356=CARTESIAN_POINT('Ctrl Pts',(17.5689861673104,-20.719618017182,13.1612344325455));
#177357=CARTESIAN_POINT('Ctrl Pts',(17.5565627299609,-20.7113754357007,
13.1621296703234));
#177358=CARTESIAN_POINT('Ctrl Pts',(17.5495473935714,-20.7066602145462,
13.1626388102793));
#177359=CARTESIAN_POINT('Ctrl Pts',(17.5307542287007,-20.6938646963093,
13.1640125822823));
#177360=CARTESIAN_POINT('Ctrl Pts',(17.5190297833328,-20.6857071157826,
13.1648801388415));
#177361=CARTESIAN_POINT('Ctrl Pts',(17.392421918462,-20.5957014657772,13.1743651173633));
#177362=CARTESIAN_POINT('Ctrl Pts',(17.285932606171,-20.5027010451042,13.1834322353885));
#177363=CARTESIAN_POINT('Ctrl Pts',(17.123405389796,-20.3293207814724,13.1990666158707));
#177364=CARTESIAN_POINT('Ctrl Pts',(17.0622207108439,-20.2543754223836,
13.2054947880728));
#177365=CARTESIAN_POINT('Ctrl Pts',(16.9686660544061,-20.1222738788584,
13.2160579265799));
#177366=CARTESIAN_POINT('Ctrl Pts',(16.933439688745,-20.067315691708,13.220252050226));
#177367=CARTESIAN_POINT('Ctrl Pts',(16.8942250341913,-19.9994207203129,
13.2251234910849));
#177368=CARTESIAN_POINT('Ctrl Pts',(16.8877510526217,-19.9879666666764,
13.2259350796216));
#177369=CARTESIAN_POINT('Ctrl Pts',(16.8788540500336,-19.9718773646439,
13.2270600778773));
#177370=CARTESIAN_POINT('Ctrl Pts',(16.8763409370398,-19.9672926384712,
13.2273789625167));
#177371=CARTESIAN_POINT('Ctrl Pts',(16.8720920943022,-19.9594727929224,
13.2279199303812));
#177372=CARTESIAN_POINT('Ctrl Pts',(16.8703477569948,-19.9562423988482,
13.2281425577202));
#177373=CARTESIAN_POINT('Ctrl Pts',(16.867022326837,-19.9500454237551,13.2285679871242));
#177374=CARTESIAN_POINT('Ctrl Pts',(16.8654398913212,-19.9470796051507,
13.2287708772906));
#177375=CARTESIAN_POINT('Ctrl Pts',(16.8612708347571,-19.9392208993858,
13.2293066266323));
#177376=CARTESIAN_POINT('Ctrl Pts',(16.858696304655,-19.9343215778614,13.2296387232001));
#177377=CARTESIAN_POINT('Ctrl Pts',(16.8496512073231,-19.9169436298722,
13.2308101487592));
#177378=CARTESIAN_POINT('Ctrl Pts',(16.8432855781525,-19.9044104052285,
13.2316431328683));
#177379=CARTESIAN_POINT('Ctrl Pts',(16.7641645765918,-19.7447097402592,
13.2421191975049));
#177380=CARTESIAN_POINT('Ctrl Pts',(16.7086313196221,-19.5896038629917,
13.2508474021997));
#177381=CARTESIAN_POINT('Ctrl Pts',(16.6409703150105,-19.2974349413105,
13.2671776847458));
#177382=CARTESIAN_POINT('Ctrl Pts',(16.6231411419796,-19.1626335726882,
13.2746743954839));
#177383=CARTESIAN_POINT('Ctrl Pts',(16.6177334381976,-19.0102153502626,
13.2835989597362));
#177384=CARTESIAN_POINT('Ctrl Pts',(16.6173369766507,-18.9933619238226,
13.2845914612895));
#177385=CARTESIAN_POINT('Ctrl Pts',(16.6170471058777,-18.9683224448112,
13.2860751509792));
#177386=CARTESIAN_POINT('Ctrl Pts',(16.6169998255314,-18.960138584867,13.2865615214586));
#177387=CARTESIAN_POINT('Ctrl Pts',(16.6170001372645,-18.9455564763432,
13.2874307944041));
#177388=CARTESIAN_POINT('Ctrl Pts',(16.6170292805235,-18.9391582980038,
13.2878131140335));
#177389=CARTESIAN_POINT('Ctrl Pts',(16.6171518843235,-18.9256683305771,
13.2886211575997));
#177390=CARTESIAN_POINT('Ctrl Pts',(16.6172519794772,-18.9185766942862,
13.2890470848809));
#177391=CARTESIAN_POINT('Ctrl Pts',(16.6176113756255,-18.8998005224859,
13.2901778747686));
#177392=CARTESIAN_POINT('Ctrl Pts',(16.6179318027047,-18.8881175247336,
13.2908846438824));
#177393=CARTESIAN_POINT('Ctrl Pts',(16.6198779960632,-18.8336263277381,
13.2941962880927));
#177394=CARTESIAN_POINT('Ctrl Pts',(16.6227060715058,-18.7908736445078,
13.2968385317458));
#177395=CARTESIAN_POINT('Ctrl Pts',(16.6340979511695,-18.6730661229858,
13.3042463160918));
#177396=CARTESIAN_POINT('Ctrl Pts',(16.6453836997484,-18.5983437757388,
13.3090901301051));
#177397=CARTESIAN_POINT('Ctrl Pts',(16.6815642400618,-18.4229141733201,
13.3207652578194));
#177398=CARTESIAN_POINT('Ctrl Pts',(16.7099064233513,-18.3231481995358,
13.3276519349119));
#177399=CARTESIAN_POINT('Ctrl Pts',(16.7454194046024,-18.225889667056,13.3344632333882));
#177400=CARTESIAN_POINT('Origin',(18.734,-18.952,0.));
#177401=CARTESIAN_POINT('',(16.743090036011,-18.2250592052755,14.3554399658108));
#177402=CARTESIAN_POINT('',(16.7454193947488,-18.2258896940418,14.1348940370926));
#177403=CARTESIAN_POINT('',(16.7454193692319,-18.2258897639242,0.));
#177404=CARTESIAN_POINT('',(16.6201365817634,-18.9515404579278,14.311091773925));
#177405=CARTESIAN_POINT('Ctrl Pts',(16.6203928623232,-18.9515314192714,
14.3109441064964));
#177406=CARTESIAN_POINT('Ctrl Pts',(16.6199115702051,-18.7039933214138,
14.3257760596012));
#177407=CARTESIAN_POINT('Ctrl Pts',(16.6606018499745,-18.4566059525848,
14.340608012706));
#177408=CARTESIAN_POINT('Ctrl Pts',(16.743090036011,-18.2250592052755,14.3554399658108));
#177409=CARTESIAN_POINT('Ctrl Pts',(16.6170000287542,-18.9516510797598,
14.3128990382682));
#177410=CARTESIAN_POINT('Ctrl Pts',(16.6169985638884,-18.9605388440599,
14.3123784727587));
#177411=CARTESIAN_POINT('Ctrl Pts',(16.6170530690528,-18.9694264496665,
14.311856218884));
#177412=CARTESIAN_POINT('Ctrl Pts',(16.617270741535,-18.9869375859922,14.3108237482288));
#177413=CARTESIAN_POINT('Ctrl Pts',(16.6174306466636,-18.9955609659129,
14.3103136432639));
#177414=CARTESIAN_POINT('Ctrl Pts',(16.6177963852562,-19.0103940122229,
14.3094332540418));
#177415=CARTESIAN_POINT('Ctrl Pts',(16.6179768689464,-19.0166042359689,
14.3090637645325));
#177416=CARTESIAN_POINT('Ctrl Pts',(16.6183911392992,-19.028982091129,14.3083255017697));
#177417=CARTESIAN_POINT('Ctrl Pts',(16.6186245665712,-19.0351496736629,
14.3079567433572));
#177418=CARTESIAN_POINT('Ctrl Pts',(16.6191442765092,-19.0474570442302,
14.3072190573059));
#177419=CARTESIAN_POINT('Ctrl Pts',(16.619430334278,-19.0535967816614,14.3068501402674));
#177420=CARTESIAN_POINT('Ctrl Pts',(16.6202771218832,-19.0702146333442,
14.3058491214672));
#177421=CARTESIAN_POINT('Ctrl Pts',(16.6208890190741,-19.0806898639952,
14.3052154202335));
#177422=CARTESIAN_POINT('Ctrl Pts',(16.6234852743548,-19.1201005142573,
14.3028208550529));
#177423=CARTESIAN_POINT('Ctrl Pts',(16.6259862441654,-19.1489976250017,
14.301043887867));
#177424=CARTESIAN_POINT('Ctrl Pts',(16.6533334749466,-19.4038925864202,
14.2851745675177));
#177425=CARTESIAN_POINT('Ctrl Pts',(16.7138477085442,-19.6245466791475,
14.2698452627864));
#177426=CARTESIAN_POINT('Ctrl Pts',(16.8322264942422,-19.883816958295,14.2513238062692));
#177427=CARTESIAN_POINT('Ctrl Pts',(16.8583594908963,-19.9353611754857,
14.247627510522));
#177428=CARTESIAN_POINT('Ctrl Pts',(16.8925972239178,-19.9965463788508,
14.2432767012153));
#177429=CARTESIAN_POINT('Ctrl Pts',(16.898718247857,-20.0072640561445,14.2425160201536));
#177430=CARTESIAN_POINT('Ctrl Pts',(16.9074985434946,-20.0223305075977,
14.241449398554));
#177431=CARTESIAN_POINT('Ctrl Pts',(16.9100801887588,-20.0267239131598,
14.2411386985434));
#177432=CARTESIAN_POINT('Ctrl Pts',(16.9145364058199,-20.0342451320219,
14.240607423729));
#177433=CARTESIAN_POINT('Ctrl Pts',(16.9164032337857,-20.0373774885019,
14.2403863509249));
#177434=CARTESIAN_POINT('Ctrl Pts',(16.9200225191191,-20.0434147736011,
14.2399606386637));
#177435=CARTESIAN_POINT('Ctrl Pts',(16.9217738674845,-20.0463203160777,
14.2397559267035));
#177436=CARTESIAN_POINT('Ctrl Pts',(16.9264840170099,-20.0540922862543,
14.23920876601));
#177437=CARTESIAN_POINT('Ctrl Pts',(16.9294555087507,-20.0589510454379,
14.2388671417719));
#177438=CARTESIAN_POINT('Ctrl Pts',(16.9403589057916,-20.0766188727872,
14.2376262872196));
#177439=CARTESIAN_POINT('Ctrl Pts',(16.9484080925125,-20.0893555084984,
14.2367344332985));
#177440=CARTESIAN_POINT('Ctrl Pts',(17.0411047119212,-20.2326240690977,
14.2267199622498));
#177441=CARTESIAN_POINT('Ctrl Pts',(17.1397702716753,-20.3535485650571,
14.2184099905279));
#177442=CARTESIAN_POINT('Ctrl Pts',(17.3441964430362,-20.5542679786293,
14.2028291012479));
#177443=CARTESIAN_POINT('Ctrl Pts',(17.4458690459048,-20.6370903846123,
14.1956355622444));
#177444=CARTESIAN_POINT('Ctrl Pts',(17.5686601993454,-20.7194732505057,
14.1870579580777));
#177445=CARTESIAN_POINT('Ctrl Pts',(17.5829040050208,-20.7287826339327,
14.1860649062725));
#177446=CARTESIAN_POINT('Ctrl Pts',(17.6055868815264,-20.7432203393623,
14.1844857174748));
#177447=CARTESIAN_POINT('Ctrl Pts',(17.6139524436912,-20.7484631743405,
14.1839037753907));
#177448=CARTESIAN_POINT('Ctrl Pts',(17.6282465562387,-20.7572828749356,
14.1829100644459));
#177449=CARTESIAN_POINT('Ctrl Pts',(17.6341565905712,-20.7608895516117,
14.1824993912247));
#177450=CARTESIAN_POINT('Ctrl Pts',(17.6458238516216,-20.7679313353851,
14.1816889728369));
#177451=CARTESIAN_POINT('Ctrl Pts',(17.6515799165101,-20.7713682161675,
14.1812892985924));
#177452=CARTESIAN_POINT('Ctrl Pts',(17.662760227534,-20.7779720153797,14.1805132297018));
#177453=CARTESIAN_POINT('Ctrl Pts',(17.668182439662,-20.7811422519363,14.1801369611862));
#177454=CARTESIAN_POINT('Ctrl Pts',(17.6809398095863,-20.7885251934992,
14.1792518907075));
#177455=CARTESIAN_POINT('Ctrl Pts',(17.6882862277516,-20.7927181354778,
14.1787423810995));
#177456=CARTESIAN_POINT('Ctrl Pts',(17.7081227339754,-20.8038826740534,
14.1773669647971));
#177457=CARTESIAN_POINT('Ctrl Pts',(17.7206585101674,-20.8107718021923,
14.1764981226869));
#177458=CARTESIAN_POINT('Ctrl Pts',(17.8364812946338,-20.8729031838007,
14.1684725470742));
#177459=CARTESIAN_POINT('Ctrl Pts',(17.9440997805178,-20.9196022592869,
14.1610125097963));
#177460=CARTESIAN_POINT('Ctrl Pts',(18.2100568997786,-21.0096608125125,
14.1426693604763));
#177461=CARTESIAN_POINT('Ctrl Pts',(18.3706639288621,-21.0440017959744,
14.1316435710508));
#177462=CARTESIAN_POINT('Ctrl Pts',(18.5648597694148,-21.0624656260514,
14.1192615733656));
#177463=CARTESIAN_POINT('Ctrl Pts',(18.5961610074516,-21.0647409286526,
14.1172965025599));
#177464=CARTESIAN_POINT('Ctrl Pts',(18.6346548631846,-21.0666798389272,
14.1149268088956));
#177465=CARTESIAN_POINT('Ctrl Pts',(18.6418085189274,-21.0670037852376,
14.1144884162702));
#177466=CARTESIAN_POINT('Ctrl Pts',(18.6530528192028,-21.0674558140129,
14.113802609786));
#177467=CARTESIAN_POINT('Ctrl Pts',(18.657142349113,-21.0676083402359,14.1135538628078));
#177468=CARTESIAN_POINT('Ctrl Pts',(18.664804734509,-21.0678718752243,14.1130891013304));
#177469=CARTESIAN_POINT('Ctrl Pts',(18.6683773879172,-21.0679856923264,
14.1128729378517));
#177470=CARTESIAN_POINT('Ctrl Pts',(18.6765563907379,-21.0682255232384,
14.1123792749819));
#177471=CARTESIAN_POINT('Ctrl Pts',(18.6811628664646,-21.0683455463821,
14.112102113721));
#177472=CARTESIAN_POINT('Ctrl Pts',(18.6954029530342,-21.0686700533648,
14.1112479187135));
#177473=CARTESIAN_POINT('Ctrl Pts',(18.7050377512107,-21.0688238100798,
14.1106736490053));
#177474=CARTESIAN_POINT('Ctrl Pts',(18.8024979972458,-21.0697135819577,
14.1048988257154));
#177475=CARTESIAN_POINT('Ctrl Pts',(18.8902987135775,-21.0650492912422,
14.0999755013231));
#177476=CARTESIAN_POINT('Ctrl Pts',(19.0081025781511,-21.0514051105892,
14.093453033427));
#177477=CARTESIAN_POINT('Ctrl Pts',(19.0385597936453,-21.0472034346202,
14.0917744866438));
#177478=CARTESIAN_POINT('Ctrl Pts',(19.176770223872,-21.0250593019557,14.084154294581));
#177479=CARTESIAN_POINT('Ctrl Pts',(19.2831250144684,-20.9994572429335,
14.0782720326108));
#177480=CARTESIAN_POINT('Ctrl Pts',(19.4393112133755,-20.948809056898,14.0691412443895));
#177481=CARTESIAN_POINT('Ctrl Pts',(19.4909139121867,-20.9298248167773,
14.0660414920822));
#177482=CARTESIAN_POINT('Ctrl Pts',(19.5733692925994,-20.8957903053402,
14.0609091886858));
#177483=CARTESIAN_POINT('Ctrl Pts',(19.6046985292448,-20.881959957136,14.0589157905539));
#177484=CARTESIAN_POINT('Ctrl Pts',(19.6454500505661,-20.8627758833888,
14.0562593901813));
#177485=CARTESIAN_POINT('Ctrl Pts',(19.6551872702009,-20.8581006473667,
14.0556198205059));
#177486=CARTESIAN_POINT('Ctrl Pts',(19.6710821685015,-20.8503186170072,
14.0545676489534));
#177487=CARTESIAN_POINT('Ctrl Pts',(19.6772612733218,-20.8472558483541,
14.0541565852843));
#177488=CARTESIAN_POINT('Ctrl Pts',(19.689196921702,-20.8412669319171,14.0533585713872));
#177489=CARTESIAN_POINT('Ctrl Pts',(19.6949552655867,-20.8383445272199,
14.0529717558436));
#177490=CARTESIAN_POINT('Ctrl Pts',(19.7082254701403,-20.8315332623007,
14.0520760889686));
#177491=CARTESIAN_POINT('Ctrl Pts',(19.7157275358983,-20.8276256536899,
14.0515665801786));
#177492=CARTESIAN_POINT('Ctrl Pts',(19.7358522184387,-20.8169894730245,
14.0501911675157));
#177493=CARTESIAN_POINT('Ctrl Pts',(19.7484302227906,-20.8101778465497,
14.0493223282512));
#177494=CARTESIAN_POINT('Ctrl Pts',(19.863127843729,-20.746551637817,14.0413133525316));
#177495=CARTESIAN_POINT('Ctrl Pts',(19.960431704408,-20.6815093911962,14.033871391778));
#177496=CARTESIAN_POINT('Ctrl Pts',(20.1792926898503,-20.5074199805855,
14.0156042039348));
#177497=CARTESIAN_POINT('Ctrl Pts',(20.2946012664589,-20.3916965138818,
14.0046385635982));
#177498=CARTESIAN_POINT('Ctrl Pts',(20.41557440637,-20.2384856072234,13.9922357529867));
#177499=CARTESIAN_POINT('Ctrl Pts',(20.4350579953202,-20.2126108297202,
13.9902062646671));
#177500=CARTESIAN_POINT('Ctrl Pts',(20.4581574237856,-20.1804227558167,
13.9877700342318));
#177501=CARTESIAN_POINT('Ctrl Pts',(20.4623434011426,-20.1745262288418,
13.9873272876515));
#177502=CARTESIAN_POINT('Ctrl Pts',(20.4688598443581,-20.165246551393,13.9866362040669));
#177503=CARTESIAN_POINT('Ctrl Pts',(20.4712107701972,-20.1618779337631,
13.9863865004224));
#177504=CARTESIAN_POINT('Ctrl Pts',(20.4755877109546,-20.1555672001771,
13.9859209181685));
#177505=CARTESIAN_POINT('Ctrl Pts',(20.4776160619388,-20.152626831729,13.9857048847962));
#177506=CARTESIAN_POINT('Ctrl Pts',(20.4822304714435,-20.1459012661219,
13.9852127724995));
#177507=CARTESIAN_POINT('Ctrl Pts',(20.4848116788647,-20.1421128016237,
13.984937023702));
#177508=CARTESIAN_POINT('Ctrl Pts',(20.4927119270671,-20.1304361973155,
13.9840914906566));
#177509=CARTESIAN_POINT('Ctrl Pts',(20.4979902005319,-20.1225204370791,
13.9835243900639));
#177510=CARTESIAN_POINT('Ctrl Pts',(20.5690653040157,-20.0143572906987,
13.9758540865189));
#177511=CARTESIAN_POINT('Ctrl Pts',(20.6262923367506,-19.9087161394295,
13.969271279574));
#177512=CARTESIAN_POINT('Ctrl Pts',(20.7178059936496,-19.6990270984464,
13.9568186765284));
#177513=CARTESIAN_POINT('Ctrl Pts',(20.7535835234111,-19.5960630069706,
13.9509553974396));
#177514=CARTESIAN_POINT('Ctrl Pts',(20.8003489699177,-19.418370751754,13.9407335518356));
#177515=CARTESIAN_POINT('Ctrl Pts',(20.8155537457217,-19.3449784356359,
13.9364855352));
#177516=CARTESIAN_POINT('Ctrl Pts',(20.8296676775589,-19.2523648181068,
13.9310153591968));
#177517=CARTESIAN_POINT('Ctrl Pts',(20.8322509242903,-19.2337535514502,
13.929910790735));
#177518=CARTESIAN_POINT('Ctrl Pts',(20.8356487967478,-19.2066261073567,
13.9282921535242));
#177519=CARTESIAN_POINT('Ctrl Pts',(20.8366601253209,-19.1981351529786,
13.9277842905433));
#177520=CARTESIAN_POINT('Ctrl Pts',(20.8383438635375,-19.183230384364,13.92689056471));
#177521=CARTESIAN_POINT('Ctrl Pts',(20.8390384638506,-19.1768191516539,
13.9265054066274));
#177522=CARTESIAN_POINT('Ctrl Pts',(20.8403308773127,-19.1643586258857,
13.9257553879369));
#177523=CARTESIAN_POINT('Ctrl Pts',(20.8409319507925,-19.1583097289032,
13.925390634115));
#177524=CARTESIAN_POINT('Ctrl Pts',(20.8423073805125,-19.1438347902302,
13.9245161659618));
#177525=CARTESIAN_POINT('Ctrl Pts',(20.8430572825163,-19.1354065791591,
13.924005686868));
#177526=CARTESIAN_POINT('Ctrl Pts',(20.8455851797949,-19.1049263812782,
13.9221547074298));
#177527=CARTESIAN_POINT('Ctrl Pts',(20.8470679493491,-19.0828519497904,
13.9208049852415));
#177528=CARTESIAN_POINT('Ctrl Pts',(20.8577336076008,-18.8755184134431,
13.9080373215584));
#177529=CARTESIAN_POINT('Ctrl Pts',(20.8428740606282,-18.689861664509,13.8958211252233));
#177530=CARTESIAN_POINT('Ctrl Pts',(20.7872334898909,-18.4301219667557,
13.8782833409733));
#177531=CARTESIAN_POINT('Ctrl Pts',(20.7659837045713,-18.3526934096555,
13.8730123855918));
#177532=CARTESIAN_POINT('Ctrl Pts',(20.7288885747899,-18.2424873828691,
13.8655997390942));
#177533=CARTESIAN_POINT('Ctrl Pts',(20.7165166755242,-18.20861815348,13.8633348077176));
#177534=CARTESIAN_POINT('Ctrl Pts',(20.7005444269591,-18.1681328046278,
13.8606572215011));
#177535=CARTESIAN_POINT('Ctrl Pts',(20.6977671458048,-18.1612008067393,
13.8601998304739));
#177536=CARTESIAN_POINT('Ctrl Pts',(20.6933858112382,-18.1504305739998,
13.859491018786));
#177537=CARTESIAN_POINT('Ctrl Pts',(20.6918070586786,-18.146582205526,13.8592381161906));
#177538=CARTESIAN_POINT('Ctrl Pts',(20.6888538588364,-18.1394434754006,
13.8587696972341));
#177539=CARTESIAN_POINT('Ctrl Pts',(20.6874824539807,-18.1361519643077,
13.8585540070002));
#177540=CARTESIAN_POINT('Ctrl Pts',(20.6843576357318,-18.1287051360699,
13.858066660091));
#177541=CARTESIAN_POINT('Ctrl Pts',(20.6825992608731,-18.1245519583559,
13.8577953085805));
#177542=CARTESIAN_POINT('Ctrl Pts',(20.6773530880157,-18.1122702748014,
13.8569941097287));
#177543=CARTESIAN_POINT('Ctrl Pts',(20.6738275549437,-18.1041578570673,
13.8564665012397));
#177544=CARTESIAN_POINT('Ctrl Pts',(20.6473672677725,-18.0443006020077,
13.8525837773986));
#177545=CARTESIAN_POINT('Ctrl Pts',(20.6224142823125,-17.9934671662867,
13.8493429340956));
#177546=CARTESIAN_POINT('Ctrl Pts',(20.5159451807352,-17.7969133354706,
13.8368048508807));
#177547=CARTESIAN_POINT('Ctrl Pts',(20.4193556676389,-17.6600491203108,
13.8280140456728));
#177548=CARTESIAN_POINT('Ctrl Pts',(20.2685601734049,-17.4924674541399,
13.8155119844931));
#177549=CARTESIAN_POINT('Ctrl Pts',(20.2276532489514,-17.4506308247862,
13.8122219975605));
#177550=CARTESIAN_POINT('Ctrl Pts',(20.1589897077629,-17.3859935659781,
13.8068037008979));
#177551=CARTESIAN_POINT('Ctrl Pts',(20.1322929944386,-17.3621106020858,
13.804720521714));
#177552=CARTESIAN_POINT('Ctrl Pts',(20.0966389796344,-17.3318072508283,
13.8019616021526));
#177553=CARTESIAN_POINT('Ctrl Pts',(20.0882184700461,-17.324762506023,13.8013116662425));
#177554=CARTESIAN_POINT('Ctrl Pts',(20.0743897808976,-17.3133748638122,
13.8002467811953));
#177555=CARTESIAN_POINT('Ctrl Pts',(20.0690143150772,-17.3089924289704,
13.7998334439103));
#177556=CARTESIAN_POINT('Ctrl Pts',(20.058604088043,-17.3005901426147,13.7990340764229));
#177557=CARTESIAN_POINT('Ctrl Pts',(20.05357231449,-17.2965666994596,13.7986481971558));
#177558=CARTESIAN_POINT('Ctrl Pts',(20.0419645395485,-17.2873715871934,
13.7977591032985));
#177559=CARTESIAN_POINT('Ctrl Pts',(20.0353761225506,-17.2822158301276,
13.7972552615765));
#177560=CARTESIAN_POINT('Ctrl Pts',(20.0176929791805,-17.2685461356653,
13.7959049842466));
#177561=CARTESIAN_POINT('Ctrl Pts',(20.0065442998312,-17.2601029675608,
13.7950557777646));
#177562=CARTESIAN_POINT('Ctrl Pts',(19.9144915569788,-17.1918137413675,
13.7880600319688));
#177563=CARTESIAN_POINT('Ctrl Pts',(19.8295097320171,-17.1377041814489,
13.7816925998755));
#177564=CARTESIAN_POINT('Ctrl Pts',(19.5902989928113,-17.0083440013616,
13.7640470659696));
#177565=CARTESIAN_POINT('Ctrl Pts',(19.4302591033687,-16.9454443031439,
13.7524857772771));
#177566=CARTESIAN_POINT('Ctrl Pts',(19.2257888824506,-16.8925284821273,
13.7389778823449));
#177567=CARTESIAN_POINT('Ctrl Pts',(19.1869053807888,-16.8836295233524,
13.7364660647257));
#177568=CARTESIAN_POINT('Ctrl Pts',(19.1402539044138,-16.8743316365259,
13.7335381860775));
#177569=CARTESIAN_POINT('Ctrl Pts',(19.1327086109033,-16.8728704919655,
13.7330672954573));
#177570=CARTESIAN_POINT('Ctrl Pts',(19.1210209907743,-16.8706731515228,
13.7323421731953));
#177571=CARTESIAN_POINT('Ctrl Pts',(19.1168842359302,-16.8699081768379,
13.7320863498469));
#177572=CARTESIAN_POINT('Ctrl Pts',(19.1092407733773,-16.8685182868598,
13.7316152309988));
#177573=CARTESIAN_POINT('Ctrl Pts',(19.105734795997,-16.86788989524,13.7313997444462));
#177574=CARTESIAN_POINT('Ctrl Pts',(19.0978461368141,-16.8664965161994,
13.730916249382));
#177575=CARTESIAN_POINT('Ctrl Pts',(19.0934626334226,-16.8657364959759,
13.7306485253506));
#177576=CARTESIAN_POINT('Ctrl Pts',(19.0822404270118,-16.8638271880139,
13.72996545517));
#177577=CARTESIAN_POINT('Ctrl Pts',(19.0753983528898,-16.8626976630058,
13.7295512049085));
#177578=CARTESIAN_POINT('Ctrl Pts',(19.0353995765776,-16.8562961935664,
13.7271417558337));
#177579=CARTESIAN_POINT('Ctrl Pts',(19.0021247723537,-16.851779644938,13.7251864795585));
#177580=CARTESIAN_POINT('Ctrl Pts',(18.9506106108374,-16.8460317795856,
13.722215708549));
#177581=CARTESIAN_POINT('Ctrl Pts',(18.9324407318121,-16.8442420411798,
13.7211786184165));
#177582=CARTESIAN_POINT('Ctrl Pts',(18.8831299528729,-16.840028230316,13.7183878330192));
#177583=CARTESIAN_POINT('Ctrl Pts',(18.851954305638,-16.838057851183,13.7166490020242));
#177584=CARTESIAN_POINT('Ctrl Pts',(18.7822810849243,-16.8352005438811,
13.7127985803021));
#177585=CARTESIAN_POINT('Ctrl Pts',(18.7437799226957,-16.8346725613945,
13.7106950087804));
#177586=CARTESIAN_POINT('Ctrl Pts',(18.5960098586888,-16.8366770974319,
13.7026493547095));
#177587=CARTESIAN_POINT('Ctrl Pts',(18.4870146104425,-16.8466188973424,
13.6967644233398));
#177588=CARTESIAN_POINT('Ctrl Pts',(18.3250242599343,-16.8741510180712,
13.6876274304945));
#177589=CARTESIAN_POINT('Ctrl Pts',(18.2711535560168,-16.8854835897332,
13.684524122855));
#177590=CARTESIAN_POINT('Ctrl Pts',(18.1845501981536,-16.9072583256948,
13.6793864578755));
#177591=CARTESIAN_POINT('Ctrl Pts',(18.1515216202109,-16.9164208832722,
13.6773913608685));
#177592=CARTESIAN_POINT('Ctrl Pts',(18.1083928298295,-16.9295209732093,
13.6747330177077));
#177593=CARTESIAN_POINT('Ctrl Pts',(18.0980786971841,-16.932740275435,13.6740932479001));
#177594=CARTESIAN_POINT('Ctrl Pts',(18.0812217041842,-16.9381437317735,
13.6730408310188));
#177595=CARTESIAN_POINT('Ctrl Pts',(18.0746639943558,-16.9402811820502,
13.6726297235628));
#177596=CARTESIAN_POINT('Ctrl Pts',(18.0619874554704,-16.9444816724802,
13.6718316846659));
#177597=CARTESIAN_POINT('Ctrl Pts',(18.0558673829804,-16.9465407389742,
13.6714448882269));
#177598=CARTESIAN_POINT('Ctrl Pts',(18.0417538798914,-16.9513611448833,
13.6705493530508));
#177599=CARTESIAN_POINT('Ctrl Pts',(18.0337674242931,-16.954142433484,13.6700399574625));
#177600=CARTESIAN_POINT('Ctrl Pts',(18.0123241714089,-16.9617544328562,
13.668665048468));
#177601=CARTESIAN_POINT('Ctrl Pts',(17.998899472983,-16.9666736745448,13.6677966030124));
#177602=CARTESIAN_POINT('Ctrl Pts',(17.8756712302297,-17.0132496851991,
13.6597526956773));
#177603=CARTESIAN_POINT('Ctrl Pts',(17.7694802222011,-17.0638329686308,
13.6522722424118));
#177604=CARTESIAN_POINT('Ctrl Pts',(17.5265488143714,-17.2054114947464,
13.633902001293));
#177605=CARTESIAN_POINT('Ctrl Pts',(17.3951038112648,-17.3040112030056,
13.6228709597717));
#177606=CARTESIAN_POINT('Ctrl Pts',(17.2538231638002,-17.4381540700932,
13.6105089084557));
#177607=CARTESIAN_POINT('Ctrl Pts',(17.2317792610491,-17.460026121755,13.6085649687121));
#177608=CARTESIAN_POINT('Ctrl Pts',(17.205268564518,-17.4875136949609,13.606217151333));
#177609=CARTESIAN_POINT('Ctrl Pts',(17.2003398493186,-17.4926760177962,
13.6057802224147));
#177610=CARTESIAN_POINT('Ctrl Pts',(17.1926298765882,-17.5008336252696,
13.60509619059));
#177611=CARTESIAN_POINT('Ctrl Pts',(17.1898310778336,-17.503812151355,13.6048477657558));
#177612=CARTESIAN_POINT('Ctrl Pts',(17.1846001254261,-17.5094114197576,
13.6043832775744));
#177613=CARTESIAN_POINT('Ctrl Pts',(17.1821660131123,-17.5120301876336,
13.6041670672029));
#177614=CARTESIAN_POINT('Ctrl Pts',(17.1766043188343,-17.5180442819201,
13.6036728681127));
#177615=CARTESIAN_POINT('Ctrl Pts',(17.1734812054159,-17.5214436740196,
13.6033952202802));
#177616=CARTESIAN_POINT('Ctrl Pts',(17.1638449915378,-17.5320014398754,
13.6025380296285));
#177617=CARTESIAN_POINT('Ctrl Pts',(17.1573697342568,-17.5391943960583,
13.6019612789278));
#177618=CARTESIAN_POINT('Ctrl Pts',(17.0888259491366,-17.6163935292043,
13.5958448821422));
#177619=CARTESIAN_POINT('Ctrl Pts',(17.0314058435558,-17.6904058048352,
13.5906201640413));
#177620=CARTESIAN_POINT('Ctrl Pts',(16.9052207571342,-17.8774357311332,
13.5782429453261));
#177621=CARTESIAN_POINT('Ctrl Pts',(16.8417781178672,-17.9935541008624,
13.5711935441839));
#177622=CARTESIAN_POINT('Ctrl Pts',(16.7738052627277,-18.1514291303372,
13.5616456907613));
#177623=CARTESIAN_POINT('Ctrl Pts',(16.7590846233678,-18.1884650609054,
13.5594100858738));
#177624=CARTESIAN_POINT('Ctrl Pts',(16.7454193670368,-18.225889769936,13.5571445045843));
#177625=CARTESIAN_POINT('',(16.6170007998506,-18.9500893124935,14.0892703911058));
#177626=CARTESIAN_POINT('Ctrl Pts',(16.7454194046024,-18.225889667056,13.3344632333882));
#177627=CARTESIAN_POINT('Ctrl Pts',(16.7539003524645,-18.2026631027393,
13.336089857378));
#177628=CARTESIAN_POINT('Ctrl Pts',(16.7627902765797,-18.1795795115226,
13.3377116760456));
#177629=CARTESIAN_POINT('Ctrl Pts',(16.7783264505047,-18.1412559718137,
13.3404079872272));
#177630=CARTESIAN_POINT('Ctrl Pts',(16.7847480723209,-18.1259359259581,
13.3414868650764));
#177631=CARTESIAN_POINT('Ctrl Pts',(16.8125073103354,-18.0618374645365,
13.3460009929237));
#177632=CARTESIAN_POINT('Ctrl Pts',(16.8355026388732,-18.0137930414874,
13.349385222995));
#177633=CARTESIAN_POINT('Ctrl Pts',(16.8643428909334,-17.9589505434368,
13.3532075465039));
#177634=CARTESIAN_POINT('Ctrl Pts',(16.8684462592698,-17.9512631838952,
13.3537423619827));
#177635=CARTESIAN_POINT('Ctrl Pts',(16.874731891055,-17.9396605383436,13.3545478473222));
#177636=CARTESIAN_POINT('Ctrl Pts',(16.8768792573934,-17.935726594463,13.35482065036));
#177637=CARTESIAN_POINT('Ctrl Pts',(16.8807565591158,-17.9286767618996,
13.3553089445088));
#177638=CARTESIAN_POINT('Ctrl Pts',(16.8824818761278,-17.9255584096634,
13.3555247232875));
#177639=CARTESIAN_POINT('Ctrl Pts',(16.8862483454407,-17.9187912591001,
13.3559925282457));
#177640=CARTESIAN_POINT('Ctrl Pts',(16.8882924278162,-17.9151441576208,
13.3562443630418));
#177641=CARTESIAN_POINT('Ctrl Pts',(16.8940655506734,-17.9049147822005,
13.356949974689));
#177642=CARTESIAN_POINT('Ctrl Pts',(16.8978191321277,-17.8983463303686,
13.3574022033368));
#177643=CARTESIAN_POINT('Ctrl Pts',(16.9204919363382,-17.8591599599498,
13.3600958513959));
#177644=CARTESIAN_POINT('Ctrl Pts',(16.9402459402481,-17.8270299474275,
13.3622866583483));
#177645=CARTESIAN_POINT('Ctrl Pts',(17.0081356277537,-17.7229463384696,
13.3693824529943));
#177646=CARTESIAN_POINT('Ctrl Pts',(17.0598276861012,-17.653412241126,13.374123014618));
#177647=CARTESIAN_POINT('Ctrl Pts',(17.2291757705467,-17.45259621933,13.3884176312927));
#177648=CARTESIAN_POINT('Ctrl Pts',(17.3590578341418,-17.3326683386654,
13.3978831087856));
#177649=CARTESIAN_POINT('Ctrl Pts',(17.5209471697267,-17.2168578287132,
13.4094500361173));
#177650=CARTESIAN_POINT('Ctrl Pts',(17.5398248787797,-17.2038120115654,
13.410794386808));
#177651=CARTESIAN_POINT('Ctrl Pts',(17.5668447374941,-17.1857812759897,
13.4127140830162));
#177652=CARTESIAN_POINT('Ctrl Pts',(17.5748146827075,-17.1805403240585,
13.4132797831267));
#177653=CARTESIAN_POINT('Ctrl Pts',(17.5878261061958,-17.1721095560344,
13.4142025594507));
#177654=CARTESIAN_POINT('Ctrl Pts',(17.5928461842817,-17.1688868361464,
13.4145584026044));
#177655=CARTESIAN_POINT('Ctrl Pts',(17.603386238513,-17.1621832192265,13.4153051747859));
#177656=CARTESIAN_POINT('Ctrl Pts',(17.6089088151235,-17.1587065464249,
13.4156962553992));
#177657=CARTESIAN_POINT('Ctrl Pts',(17.6220913770569,-17.1504924835205,
13.4166293504809));
#177658=CARTESIAN_POINT('Ctrl Pts',(17.6297656466736,-17.1457783616835,
13.4171722146517));
#177659=CARTESIAN_POINT('Ctrl Pts',(17.6557515255351,-17.1300433596053,
13.4190094146126));
#177660=CARTESIAN_POINT('Ctrl Pts',(17.6741994151492,-17.1192511246894,
13.4203120408752));
#177661=CARTESIAN_POINT('Ctrl Pts',(17.7757270925724,-17.0619016870768,
13.4274744457338));
#177662=CARTESIAN_POINT('Ctrl Pts',(17.8617020662172,-17.020717865647,13.4335232534566));
#177663=CARTESIAN_POINT('Ctrl Pts',(18.1086037907643,-16.9223038927295,
13.4507947272331));
#177664=CARTESIAN_POINT('Ctrl Pts',(18.2741027520591,-16.8785299435595,
13.4623042606654));
#177665=CARTESIAN_POINT('Ctrl Pts',(18.4794996029676,-16.8500313296989,
13.4755392909284));
#177666=CARTESIAN_POINT('Ctrl Pts',(18.516071976282,-16.8459253344735,13.4778537099786));
#177667=CARTESIAN_POINT('Ctrl Pts',(18.5598511689017,-16.8421629931504,
13.4805595846343));
#177668=CARTESIAN_POINT('Ctrl Pts',(18.5669702929428,-16.8415874594942,
13.4809975624706));
#177669=CARTESIAN_POINT('Ctrl Pts',(18.5785918334233,-16.8407071108761,
13.4817090635648));
#177670=CARTESIAN_POINT('Ctrl Pts',(18.5830924853179,-16.8403806486992,
13.4819837564659));
#177671=CARTESIAN_POINT('Ctrl Pts',(18.5911516255582,-16.8398219634576,
13.482474077201));
#177672=CARTESIAN_POINT('Ctrl Pts',(18.5947096753999,-16.8395843396214,
13.482690003241));
#177673=CARTESIAN_POINT('Ctrl Pts',(18.6024176333088,-16.8390891244443,
13.4831565833469));
#177674=CARTESIAN_POINT('Ctrl Pts',(18.6065676917752,-16.8388347687014,
13.4834070543531));
#177675=CARTESIAN_POINT('Ctrl Pts',(18.6181652197954,-16.8381582495792,
13.4841050025983));
#177676=CARTESIAN_POINT('Ctrl Pts',(18.6256142956396,-16.837763214544,13.4845509852218));
#177677=CARTESIAN_POINT('Ctrl Pts',(18.6689406698259,-16.8356951427539,
13.4871323550971));
#177678=CARTESIAN_POINT('Ctrl Pts',(18.704856114594,-16.8348958587633,13.4892219140928));
#177679=CARTESIAN_POINT('Ctrl Pts',(18.8205015405215,-16.8352660586759,
13.4958377363242));
#177680=CARTESIAN_POINT('Ctrl Pts',(18.9001547247206,-16.840024695492,13.5002239731848));
#177681=CARTESIAN_POINT('Ctrl Pts',(19.1643166047464,-16.870848103593,13.514724185321));
#177682=CARTESIAN_POINT('Ctrl Pts',(19.345600774252,-16.9167348744402,13.524680855757));
#177683=CARTESIAN_POINT('Ctrl Pts',(19.5390203102987,-16.9939097633066,
13.5367933177697));
#177684=CARTESIAN_POINT('Ctrl Pts',(19.5593680915753,-17.0023993910069,
13.538085782113));
#177685=CARTESIAN_POINT('Ctrl Pts',(19.5873252906305,-17.0145799775871,
13.5398884606527));
#177686=CARTESIAN_POINT('Ctrl Pts',(19.5950511931441,-17.0180012320284,
13.5403894968882));
#177687=CARTESIAN_POINT('Ctrl Pts',(19.6082967266698,-17.023961840106,13.5412535241017));
#177688=CARTESIAN_POINT('Ctrl Pts',(19.6138263266479,-17.0264788897479,
13.5416157469552));
#177689=CARTESIAN_POINT('Ctrl Pts',(19.6252042283873,-17.0317173043175,
13.5423642410518));
#177690=CARTESIAN_POINT('Ctrl Pts',(19.6310510747576,-17.0344416629785,
13.5427506127031));
#177691=CARTESIAN_POINT('Ctrl Pts',(19.644629325278,-17.040844188729,13.5436519867897));
#177692=CARTESIAN_POINT('Ctrl Pts',(19.652351008045,-17.0445426018729,13.5441676875279));
#177693=CARTESIAN_POINT('Ctrl Pts',(19.6769987557534,-17.0565323577941,
13.545823911042));
#177694=CARTESIAN_POINT('Ctrl Pts',(19.6938362474643,-17.0650027615292,
13.5469706590549));
#177695=CARTESIAN_POINT('Ctrl Pts',(19.7774011679847,-17.1084494123327,
13.5527406789516));
#177696=CARTESIAN_POINT('Ctrl Pts',(19.8423343265186,-17.1467416757843,
13.5574803603144));
#177697=CARTESIAN_POINT('Ctrl Pts',(19.9960274933769,-17.248799067349,13.5693363841238));
#177698=CARTESIAN_POINT('Ctrl Pts',(20.0821579942293,-17.3161291732635,
13.5765525554743));
#177699=CARTESIAN_POINT('Ctrl Pts',(20.1738253381538,-17.3999629311809,
13.5847586850779));
#177700=CARTESIAN_POINT('Ctrl Pts',(20.184836236259,-17.4102509002412,13.5857535790107));
#177701=CARTESIAN_POINT('Ctrl Pts',(20.2707592430541,-17.4922682344573,
13.5935857163402));
#177702=CARTESIAN_POINT('Ctrl Pts',(20.340427471791,-17.5693063638114,13.6003591315249));
#177703=CARTESIAN_POINT('Ctrl Pts',(20.4101260258063,-17.6587929804181,
13.6073671004742));
#177704=CARTESIAN_POINT('Ctrl Pts',(20.4160264505532,-17.6664768077909,
13.6079623337494));
#177705=CARTESIAN_POINT('Ctrl Pts',(20.4246614678704,-17.6778830008016,
13.6088360209613));
#177706=CARTESIAN_POINT('Ctrl Pts',(20.4274368628119,-17.6815741189699,
13.6091172361096));
#177707=CARTESIAN_POINT('Ctrl Pts',(20.4323396252473,-17.6881391288657,
13.6096146772753));
#177708=CARTESIAN_POINT('Ctrl Pts',(20.4344718103382,-17.6910093548351,
13.609831237707));
#177709=CARTESIAN_POINT('Ctrl Pts',(20.4390249884247,-17.6971711337458,
13.6102941681123));
#177710=CARTESIAN_POINT('Ctrl Pts',(20.441443720334,-17.7004642884526,13.6105403815742));
#177711=CARTESIAN_POINT('Ctrl Pts',(20.4480580007005,-17.7095246350391,
13.6112145576049));
#177712=CARTESIAN_POINT('Ctrl Pts',(20.4522340089326,-17.7153061186601,
13.6116411863517));
#177713=CARTESIAN_POINT('Ctrl Pts',(20.4743893825871,-17.7463080353882,
13.6139105344812));
#177714=CARTESIAN_POINT('Ctrl Pts',(20.4918438694643,-17.7719010739727,
13.615719409072));
#177715=CARTESIAN_POINT('Ctrl Pts',(20.5978754531955,-17.9349481219017,
13.6269059288837));
#177716=CARTESIAN_POINT('Ctrl Pts',(20.6708474847609,-18.0819078246826,
13.6355483597946));
#177717=CARTESIAN_POINT('Ctrl Pts',(20.7660118637535,-18.3466229109875,
13.6509435195264));
#177718=CARTESIAN_POINT('Ctrl Pts',(20.796527315069,-18.4605436339403,13.6575138956757));
#177719=CARTESIAN_POINT('Ctrl Pts',(20.8199515596796,-18.5904759727044,
13.6652483585029));
#177720=CARTESIAN_POINT('Ctrl Pts',(20.8223461923881,-18.6045756234303,
13.6660905375797));
#177721=CARTESIAN_POINT('Ctrl Pts',(20.8259293818693,-18.6270507732195,
13.667437990705));
#177722=CARTESIAN_POINT('Ctrl Pts',(20.8272109399408,-18.635411155505,13.6679403175115));
#177723=CARTESIAN_POINT('Ctrl Pts',(20.8293825006736,-18.6501674742287,
13.668828958476));
#177724=CARTESIAN_POINT('Ctrl Pts',(20.8302934088461,-18.6565602593672,
13.6692146055066));
#177725=CARTESIAN_POINT('Ctrl Pts',(20.8321166991622,-18.669789293524,13.6700140707878));
#177726=CARTESIAN_POINT('Ctrl Pts',(20.833024949567,-18.6766260261083,13.6704280148275));
#177727=CARTESIAN_POINT('Ctrl Pts',(20.8352700542355,-18.6941825088929,
13.6714930703164));
#177728=CARTESIAN_POINT('Ctrl Pts',(20.8365582807662,-18.7049081774827,
13.6721457087488));
#177729=CARTESIAN_POINT('Ctrl Pts',(20.8415887217315,-18.7496830985969,
13.6748786940828));
#177730=CARTESIAN_POINT('Ctrl Pts',(20.844586174763,-18.7838092388975,13.6769823067786));
#177731=CARTESIAN_POINT('Ctrl Pts',(20.8502353808129,-18.8728736752039,
13.6825292345993));
#177732=CARTESIAN_POINT('Ctrl Pts',(20.8515764257692,-18.9278664735895,
13.6860108052008));
#177733=CARTESIAN_POINT('Ctrl Pts',(20.8491826972318,-19.0921357874228,
13.6965697449011));
#177734=CARTESIAN_POINT('Ctrl Pts',(20.8391285296679,-19.2011310634843,
13.7037955397244));
#177735=CARTESIAN_POINT('Ctrl Pts',(20.8142524002979,-19.3465947782513,
13.713544165535));
#177736=CARTESIAN_POINT('Ctrl Pts',(20.8067752500602,-19.38415500747,13.7160696795729));
#177737=CARTESIAN_POINT('Ctrl Pts',(20.7910457636762,-19.453315066172,13.7207164573003));
#177738=CARTESIAN_POINT('Ctrl Pts',(20.7830729771046,-19.4849673063677,
13.7228417176583));
#177739=CARTESIAN_POINT('Ctrl Pts',(20.7735175281082,-19.5195099180314,
13.7251514085116));
#177740=CARTESIAN_POINT('Ctrl Pts',(20.7726567503308,-19.5225943471818,
13.7253575630732));
#177741=CARTESIAN_POINT('Ctrl Pts',(20.7592838654499,-19.5700969064179,
13.7285310649638));
#177742=CARTESIAN_POINT('Ctrl Pts',(20.7453286058861,-19.6141000401863,
13.7314516379822));
#177743=CARTESIAN_POINT('Ctrl Pts',(20.7273949441287,-19.6648282596846,
13.7347686199128));
#177744=CARTESIAN_POINT('Ctrl Pts',(20.7248058168856,-19.6720275929376,
13.7352381692315));
#177745=CARTESIAN_POINT('Ctrl Pts',(20.7205920439777,-19.6835479190047,
13.735987437124));
#177746=CARTESIAN_POINT('Ctrl Pts',(20.7189922226535,-19.6878778322058,
13.7362685712276));
#177747=CARTESIAN_POINT('Ctrl Pts',(20.7161250466301,-19.6955604519296,
13.7367664961684));
#177748=CARTESIAN_POINT('Ctrl Pts',(20.7148633254281,-19.6989152112827,
13.7369836186124));
#177749=CARTESIAN_POINT('Ctrl Pts',(20.7121611550301,-19.7060449384769,
13.7374443961343));
#177750=CARTESIAN_POINT('Ctrl Pts',(20.7107184205992,-19.7098189828746,
13.7376879120659));
#177751=CARTESIAN_POINT('Ctrl Pts',(20.7067732930654,-19.7200511064626,
13.7383471234583));
#177752=CARTESIAN_POINT('Ctrl Pts',(20.7042499732011,-19.7265011388612,
13.7387615821668));
#177753=CARTESIAN_POINT('Ctrl Pts',(20.6912698550748,-19.7592065371379,
13.7408581462147));
#177754=CARTESIAN_POINT('Ctrl Pts',(20.6803191778902,-19.785264371617,13.7425122201924));
#177755=CARTESIAN_POINT('Ctrl Pts',(20.6466749328626,-19.8610376362878,
13.7472956561698));
#177756=CARTESIAN_POINT('Ctrl Pts',(20.6225736085474,-19.9101050957269,
13.7503594737831));
#177757=CARTESIAN_POINT('Ctrl Pts',(20.5294284003924,-20.0825302940906,
13.7611898315668));
#177758=CARTESIAN_POINT('Ctrl Pts',(20.4499757946822,-20.1998345045874,
13.7687031809662));
#177759=CARTESIAN_POINT('Ctrl Pts',(20.3021585790556,-20.37697605724,13.7814809195929));
#177760=CARTESIAN_POINT('Ctrl Pts',(20.2406099228957,-20.4418999430942,
13.786537736569));
#177761=CARTESIAN_POINT('Ctrl Pts',(20.1651123771409,-20.5120621955398,
13.7925804196745));
#177762=CARTESIAN_POINT('Ctrl Pts',(20.1549867987538,-20.5212906660536,
13.7933876540355));
#177763=CARTESIAN_POINT('Ctrl Pts',(20.1385972027527,-20.5359394865182,
13.7946895717616));
#177764=CARTESIAN_POINT('Ctrl Pts',(20.1323895998671,-20.5414225753209,
13.7951816147904));
#177765=CARTESIAN_POINT('Ctrl Pts',(20.1213060435957,-20.5510973342095,
13.7960583544532));
#177766=CARTESIAN_POINT('Ctrl Pts',(20.1164428430365,-20.5553035043939,
13.79644244134));
#177767=CARTESIAN_POINT('Ctrl Pts',(20.1062656726431,-20.5640249841146,
13.7972449994028));
#177768=CARTESIAN_POINT('Ctrl Pts',(20.1009484110886,-20.5685363173577,
13.7976636277541));
#177769=CARTESIAN_POINT('Ctrl Pts',(20.0870716703492,-20.5801923614128,
13.7987544329902));
#177770=CARTESIAN_POINT('Ctrl Pts',(20.0784779469333,-20.587295800039,13.7994282817828));
#177771=CARTESIAN_POINT('Ctrl Pts',(20.0408170896054,-20.6179281477777,
13.8023744236567));
#177772=CARTESIAN_POINT('Ctrl Pts',(20.0111869455471,-20.6407512326211,
13.8046747616221));
#177773=CARTESIAN_POINT('Ctrl Pts',(19.9307600055691,-20.699373690697,13.8108768734502));
#177774=CARTESIAN_POINT('Ctrl Pts',(19.8789680575382,-20.7337396910258,
13.8148291357925));
#177775=CARTESIAN_POINT('Ctrl Pts',(19.7231172909987,-20.8275489928654,
13.8265844553654));
#177776=CARTESIAN_POINT('Ctrl Pts',(19.6154377901442,-20.8804970835454,
13.8345488982109));
#177777=CARTESIAN_POINT('Ctrl Pts',(19.4135659844437,-20.9593058001976,
13.8488180310605));
#177778=CARTESIAN_POINT('Ctrl Pts',(19.3209364219741,-20.9883193738169,
13.8551280801419));
#177779=CARTESIAN_POINT('Ctrl Pts',(19.2172086718811,-21.0131385966935,
13.8617177281017));
#177780=CARTESIAN_POINT('Ctrl Pts',(19.2077671315104,-21.0153292632683,
13.8623132357389));
#177781=CARTESIAN_POINT('Ctrl Pts',(19.1938042095478,-21.0184681036448,
13.8631872472829));
#177782=CARTESIAN_POINT('Ctrl Pts',(19.1892943905398,-21.0194664092496,
13.8634685152981));
#177783=CARTESIAN_POINT('Ctrl Pts',(19.1812876927908,-21.0212113243425,
13.8639660149026));
#177784=CARTESIAN_POINT('Ctrl Pts',(19.1777921572663,-21.0219638418914,
13.8641825811992));
#177785=CARTESIAN_POINT('Ctrl Pts',(19.1702986076366,-21.0235571957604,
13.8646454853417));
#177786=CARTESIAN_POINT('Ctrl Pts',(19.166300072379,-21.0243953142204,13.8648916668787));
#177787=CARTESIAN_POINT('Ctrl Pts',(19.1553171893943,-21.0266642266586,
13.8655656654203));
#177788=CARTESIAN_POINT('Ctrl Pts',(19.1483279269635,-21.0280713378125,
13.8659921497727));
#177789=CARTESIAN_POINT('Ctrl Pts',(19.1109706666151,-21.0353961071367,
13.8682593507968));
#177790=CARTESIAN_POINT('Ctrl Pts',(19.0804810831658,-21.0406831519165,
13.870066298496));
#177791=CARTESIAN_POINT('Ctrl Pts',(18.9878385464108,-21.0546631670935,
13.8754553235058));
#177792=CARTESIAN_POINT('Ctrl Pts',(18.9254019540112,-21.0612635787971,
13.8789505168442));
#177793=CARTESIAN_POINT('Ctrl Pts',(18.704030075372,-21.0747528409897,13.8911389494923));
#177794=CARTESIAN_POINT('Ctrl Pts',(18.5447211456008,-21.0665098111604,
13.8995812656302));
#177795=CARTESIAN_POINT('Ctrl Pts',(18.3258285304965,-21.0302289489533,
13.9120639289613));
#177796=CARTESIAN_POINT('Ctrl Pts',(18.2643148615901,-21.0171959442851,
13.9156661783047));
#177797=CARTESIAN_POINT('Ctrl Pts',(18.1914005345203,-20.9983211877463,
13.920089459441));
#177798=CARTESIAN_POINT('Ctrl Pts',(18.1793533099789,-20.995088745658,13.9208253388945));
#177799=CARTESIAN_POINT('Ctrl Pts',(18.1596261795417,-20.9896083371777,
13.9220389228766));
#177800=CARTESIAN_POINT('Ctrl Pts',(18.151929102011,-20.987422926173,13.9225145948675));
#177801=CARTESIAN_POINT('Ctrl Pts',(18.1381184264747,-20.9834169535159,
13.9233720419129));
#177802=CARTESIAN_POINT('Ctrl Pts',(18.1320002898861,-20.981612287198,13.9237532942526));
#177803=CARTESIAN_POINT('Ctrl Pts',(18.118993107782,-20.9777115723511,13.92456686861));
#177804=CARTESIAN_POINT('Ctrl Pts',(18.1121064272423,-20.9756079743864,
13.924999433884));
#177805=CARTESIAN_POINT('Ctrl Pts',(18.0936032231324,-20.9698526324287,
13.9261666158466));
#177806=CARTESIAN_POINT('Ctrl Pts',(18.0820073843388,-20.9661357693647,
13.9269033630824));
#177807=CARTESIAN_POINT('Ctrl Pts',(18.0250665895771,-20.9473410515868,
13.9305476833004));
#177808=CARTESIAN_POINT('Ctrl Pts',(17.980212055019,-20.9308318896352,13.9335022185114));
#177809=CARTESIAN_POINT('Ctrl Pts',(17.7804986855081,-20.8495496704731,
13.9470494161377));
#177810=CARTESIAN_POINT('Ctrl Pts',(17.633134541706,-20.7680226370081,13.958197698942));
#177811=CARTESIAN_POINT('Ctrl Pts',(17.4168216353448,-20.6122663317817,
13.9757560270314));
#177812=CARTESIAN_POINT('Ctrl Pts',(17.3408006318111,-20.5490107349291,
13.982190485097));
#177813=CARTESIAN_POINT('Ctrl Pts',(17.2624671798305,-20.473963910728,13.9888929466025));
#177814=CARTESIAN_POINT('Ctrl Pts',(17.2555127344352,-20.4672090285377,
13.9894886179829));
#177815=CARTESIAN_POINT('Ctrl Pts',(17.2453133412618,-20.4571652305694,
13.9903628230858));
#177816=CARTESIAN_POINT('Ctrl Pts',(17.2420324763639,-20.4539131960833,
13.9906441226462));
#177817=CARTESIAN_POINT('Ctrl Pts',(17.236230998062,-20.4481249286493,13.9911416571258));
#177818=CARTESIAN_POINT('Ctrl Pts',(17.2337061417771,-20.4455930252082,
13.991358226927));
#177819=CARTESIAN_POINT('Ctrl Pts',(17.2283104489712,-20.4401547848357,
13.9918211154224));
#177820=CARTESIAN_POINT('Ctrl Pts',(17.225441614127,-20.4372465400626,13.9920672779286));
#177821=CARTESIAN_POINT('Ctrl Pts',(17.2195717244196,-20.4312614612724,
13.9925710964168));
#177822=CARTESIAN_POINT('Ctrl Pts',(17.2165715832354,-20.4281837532667,
13.9928286817238));
#177823=CARTESIAN_POINT('Ctrl Pts',(17.2028281910154,-20.4139988633756,
13.9940091492461));
#177824=CARTESIAN_POINT('Ctrl Pts',(17.1921970585629,-20.4027830665149,
13.9949236799429));
#177825=CARTESIAN_POINT('Ctrl Pts',(17.1270839017022,-20.3325647599154,
14.0005412506516));
#177826=CARTESIAN_POINT('Ctrl Pts',(17.0758674040217,-20.2706119379657,
14.0050328569994));
#177827=CARTESIAN_POINT('Ctrl Pts',(16.9870844250608,-20.1498376664508,
14.0132735203915));
#177828=CARTESIAN_POINT('Ctrl Pts',(16.948665264207,-20.0917847940165,14.0170365238758));
#177829=CARTESIAN_POINT('Ctrl Pts',(16.8366942173446,-19.9029974988654,
14.0289657710074));
#177830=CARTESIAN_POINT('Ctrl Pts',(16.7741390010244,-19.7663108177587,
14.0371977909662));
#177831=CARTESIAN_POINT('Ctrl Pts',(16.7220478750258,-19.6107399544399,
14.0468105562725));
#177832=CARTESIAN_POINT('Ctrl Pts',(16.7176849721947,-19.5972622527926,
14.0476448783759));
#177833=CARTESIAN_POINT('Ctrl Pts',(16.7109454564642,-19.5757068140997,
14.0489821048932));
#177834=CARTESIAN_POINT('Ctrl Pts',(16.7084811540771,-19.5676567856875,
14.0494821324417));
#177835=CARTESIAN_POINT('Ctrl Pts',(16.7042134851154,-19.5534127694799,
14.0503680983448));
#177836=CARTESIAN_POINT('Ctrl Pts',(16.7023902813248,-19.547224801956,14.0507533824506));
#177837=CARTESIAN_POINT('Ctrl Pts',(16.6986719539726,-19.5343886454759,
14.0515534693251));
#177838=CARTESIAN_POINT('Ctrl Pts',(16.6967810570793,-19.5277393213656,
14.0519684046648));
#177839=CARTESIAN_POINT('Ctrl Pts',(16.6919990651489,-19.5106049375816,
14.0530389203583));
#177840=CARTESIAN_POINT('Ctrl Pts',(16.6891561702079,-19.5001067405812,
14.0536960580349));
#177841=CARTESIAN_POINT('Ctrl Pts',(16.6831808524464,-19.4773474686982,
14.0551235042638));
#177842=CARTESIAN_POINT('Ctrl Pts',(16.680077234064,-19.4650793306029,14.0558947171782));
#177843=CARTESIAN_POINT('Ctrl Pts',(16.6713661333626,-19.4292994480852,
14.0581493239078));
#177844=CARTESIAN_POINT('Ctrl Pts',(16.6660512435801,-19.4057191824863,
14.0596419383516));
#177845=CARTESIAN_POINT('Ctrl Pts',(16.6316557511639,-19.2399329757323,
14.07018533815));
#177846=CARTESIAN_POINT('Ctrl Pts',(16.6168699503902,-19.095183031562,14.079683056516));
#177847=CARTESIAN_POINT('Ctrl Pts',(16.6170008616905,-18.9500899223173,
14.0892704589852));
#177848=CARTESIAN_POINT('Ctrl Pts',(16.6170008622343,-18.9500893196667,
14.0892704988069));
#177849=CARTESIAN_POINT('Ctrl Pts',(16.6171115220882,-18.8274802096574,
14.0973722129365));
#177850=CARTESIAN_POINT('Ctrl Pts',(16.6278735782882,-18.7050980287736,
14.1054939065436));
#177851=CARTESIAN_POINT('Ctrl Pts',(16.6513555158941,-18.5719488797031,
14.1139585263025));
#177852=CARTESIAN_POINT('Ctrl Pts',(16.653648125981,-18.5595933258764,14.1147402671926));
#177853=CARTESIAN_POINT('Ctrl Pts',(16.6573287573147,-18.5406969010199,
14.1159293732425));
#177854=CARTESIAN_POINT('Ctrl Pts',(16.658637933201,-18.5341411915676,14.1163407091571));
#177855=CARTESIAN_POINT('Ctrl Pts',(16.6608486766872,-18.5233376087066,
14.1170164731497));
#177856=CARTESIAN_POINT('Ctrl Pts',(16.6617322884575,-18.51908616617,14.117281862338));
#177857=CARTESIAN_POINT('Ctrl Pts',(16.6634789761774,-18.5108099811438,
14.1177973993164));
#177858=CARTESIAN_POINT('Ctrl Pts',(16.6643407213338,-18.506784980344,14.1180476200037));
#177859=CARTESIAN_POINT('Ctrl Pts',(16.6659719864128,-18.4992728339622,
14.1185136513447));
#177860=CARTESIAN_POINT('Ctrl Pts',(16.666738581683,-18.495785159794,14.1187296198732));
#177861=CARTESIAN_POINT('Ctrl Pts',(16.6685067296667,-18.4878368283752,
14.1192209191906));
#177862=CARTESIAN_POINT('Ctrl Pts',(16.669513906797,-18.4833774743403,14.1194959240696));
#177863=CARTESIAN_POINT('Ctrl Pts',(16.6726472977603,-18.4697103152121,
14.120336915301));
#177864=CARTESIAN_POINT('Ctrl Pts',(16.6748207595074,-18.4605133103523,
14.1209002596648));
#177865=CARTESIAN_POINT('Ctrl Pts',(16.6956478234693,-18.3749475836915,
14.1261199387586));
#177866=CARTESIAN_POINT('Ctrl Pts',(16.7184739276668,-18.2996845882871,
14.1305523024423));
#177867=CARTESIAN_POINT('Ctrl Pts',(16.7454193947488,-18.2258896940418,
14.1348940370926));
#177868=CARTESIAN_POINT('Origin',(18.734,-18.952,0.));
#177869=CARTESIAN_POINT('',(16.7454193692319,-18.2258897639242,15.1555945373748));
#177870=CARTESIAN_POINT('',(16.7454193926287,-18.2258896998479,14.9318514575852));
#177871=CARTESIAN_POINT('',(16.7454193692319,-18.2258897639242,0.));
#177872=CARTESIAN_POINT('',(16.6156459649053,-18.9502594248307,15.110942953281));
#177873=CARTESIAN_POINT('Ctrl Pts',(16.6170007251258,-18.9502478064743,
15.1109437209775));
#177874=CARTESIAN_POINT('Ctrl Pts',(16.6170993834536,-18.8310488678702,
15.1181312937192));
#177875=CARTESIAN_POINT('Ctrl Pts',(16.6272689227094,-18.7122546433194,
15.1253188664609));
#177876=CARTESIAN_POINT('Ctrl Pts',(16.6472858251195,-18.5951905938001,
15.1325064392026));
#177877=CARTESIAN_POINT('Ctrl Pts',(16.6595036684846,-18.5237374692653,
15.1368935634506));
#177878=CARTESIAN_POINT('Ctrl Pts',(16.6754196380939,-18.4527731733662,
15.1412806876986));
#177879=CARTESIAN_POINT('Ctrl Pts',(16.6949811994244,-18.3827098008052,
15.1456678119466));
#177880=CARTESIAN_POINT('Ctrl Pts',(16.709735150403,-18.329865779477,15.1489767204226));
#177881=CARTESIAN_POINT('Ctrl Pts',(16.7265618805371,-18.277534314435,15.1522856288987));
#177882=CARTESIAN_POINT('Ctrl Pts',(16.7454193692319,-18.2258897639242,
15.1555945373748));
#177883=CARTESIAN_POINT('Ctrl Pts',(16.743090036011,-18.2250592052755,14.3554399658108));
#177884=CARTESIAN_POINT('Ctrl Pts',(16.7690653566902,-18.1521457215081,
14.3601105102452));
#177885=CARTESIAN_POINT('Ctrl Pts',(17.0725680384113,-17.4332647782197,
14.40717299024));
#177886=CARTESIAN_POINT('Ctrl Pts',(18.4531255181642,-16.4645434415688,
14.4966274057954));
#177887=CARTESIAN_POINT('Ctrl Pts',(20.6735252872927,-17.3694159533935,
14.6238032124768));
#177888=CARTESIAN_POINT('Ctrl Pts',(21.1145309858464,-19.7262111017336,
14.7509790191583));
#177889=CARTESIAN_POINT('Ctrl Pts',(19.3715472573024,-21.3727156171947,
14.8781548258396));
#177890=CARTESIAN_POINT('Ctrl Pts',(17.1752233382973,-20.8308254969318,
14.9981428038806));
#177891=CARTESIAN_POINT('Ctrl Pts',(16.6208559183895,-19.5344638852643,
15.075738846361));
#177892=CARTESIAN_POINT('Ctrl Pts',(16.6156459649053,-18.9502594248307,
15.110942953281));
#177893=CARTESIAN_POINT('Ctrl Pts',(16.7454193947488,-18.2258896940418,
14.1348940370926));
#177894=CARTESIAN_POINT('Ctrl Pts',(16.7604972189655,-18.184596424189,14.1373235333657));
#177895=CARTESIAN_POINT('Ctrl Pts',(16.7768648746395,-18.1437628265383,
14.1397244619261));
#177896=CARTESIAN_POINT('Ctrl Pts',(16.8230771617196,-18.0381372392333,
14.1459966961117));
#177897=CARTESIAN_POINT('Ctrl Pts',(16.8549327780734,-17.9743101323951,
14.1498507172934));
#177898=CARTESIAN_POINT('Ctrl Pts',(16.9337290477334,-17.8345657051403,
14.1586405472823));
#177899=CARTESIAN_POINT('Ctrl Pts',(16.982367371586,-17.7597685692748,14.1635988425243));
#177900=CARTESIAN_POINT('Ctrl Pts',(17.0559411059934,-17.6608874095257,
14.1706897752876));
#177901=CARTESIAN_POINT('Ctrl Pts',(17.0769686667388,-17.634008975664,14.1726760492236));
#177902=CARTESIAN_POINT('Ctrl Pts',(17.1055473192068,-17.5992438041695,
14.1753299172114));
#177903=CARTESIAN_POINT('Ctrl Pts',(17.1125234962165,-17.5908896444725,
14.1759743065694));
#177904=CARTESIAN_POINT('Ctrl Pts',(17.1240365196256,-17.5773166167404,
14.1770323875731));
#177905=CARTESIAN_POINT('Ctrl Pts',(17.1285351201684,-17.5720654616132,
14.1774445069301));
#177906=CARTESIAN_POINT('Ctrl Pts',(17.1372798227453,-17.5619585320599,
14.1782431354147));
#177907=CARTESIAN_POINT('Ctrl Pts',(17.1415225553785,-17.5570999340496,
14.1786295022534));
#177908=CARTESIAN_POINT('Ctrl Pts',(17.1513511825713,-17.5459478922079,
14.1795220507335));
#177909=CARTESIAN_POINT('Ctrl Pts',(17.1569525011313,-17.5396682428503,
14.1800288754498));
#177910=CARTESIAN_POINT('Ctrl Pts',(17.1720744880781,-17.5229170811656,
14.1813923634545));
#177911=CARTESIAN_POINT('Ctrl Pts',(17.1816628467637,-17.5125075057123,
14.1822518835076));
#177912=CARTESIAN_POINT('Ctrl Pts',(17.2658129781242,-17.4229686983819,
14.1897533296712));
#177913=CARTESIAN_POINT('Ctrl Pts',(17.34625215017,-17.3496082241773,14.1966547814615));
#177914=CARTESIAN_POINT('Ctrl Pts',(17.5089830018816,-17.2226749493561,
14.210092937947));
#177915=CARTESIAN_POINT('Ctrl Pts',(17.5900728316884,-17.1679986054793,
14.2165774440231));
#177916=CARTESIAN_POINT('Ctrl Pts',(17.7368988642659,-17.0831370273213,
14.2277551380599));
#177917=CARTESIAN_POINT('Ctrl Pts',(17.8009519285969,-17.0503475038104,
14.2324604151131));
#177918=CARTESIAN_POINT('Ctrl Pts',(17.8972652897789,-17.0070841781335,
14.2391770255881));
#177919=CARTESIAN_POINT('Ctrl Pts',(17.9283038549006,-16.9940223322516,
14.241289008369));
#177920=CARTESIAN_POINT('Ctrl Pts',(17.9664235875241,-16.9790406661045,
14.2438082312705));
#177921=CARTESIAN_POINT('Ctrl Pts',(17.9732182724655,-16.9764106578555,
14.2442544266867));
#177922=CARTESIAN_POINT('Ctrl Pts',(17.9839067519935,-16.9723368057187,
14.2449517087929));
#177923=CARTESIAN_POINT('Ctrl Pts',(17.9877913733167,-16.9708692800211,
14.2452041766294));
#177924=CARTESIAN_POINT('Ctrl Pts',(17.995020427257,-16.9681625794067,14.2456722022112));
#177925=CARTESIAN_POINT('Ctrl Pts',(17.9983636408144,-16.9669204379694,
14.2458879312512));
#177926=CARTESIAN_POINT('Ctrl Pts',(18.0059506754657,-16.9641233418396,
14.2463758901694));
#177927=CARTESIAN_POINT('Ctrl Pts',(18.0101963359913,-16.9625735289155,
14.2466478116417));
#177928=CARTESIAN_POINT('Ctrl Pts',(18.0228077880583,-16.9580156290841,
14.247452256275));
#177929=CARTESIAN_POINT('Ctrl Pts',(18.0311877202684,-16.9550465855451,
14.247982513526));
#177930=CARTESIAN_POINT('Ctrl Pts',(18.0942139625286,-16.9331620151875,
14.2519403909262));
#177931=CARTESIAN_POINT('Ctrl Pts',(18.1496012505542,-16.9164380746681,
14.255248677143));
#177932=CARTESIAN_POINT('Ctrl Pts',(18.3636338700943,-16.8612707309285,
14.2676340021751));
#177933=CARTESIAN_POINT('Ctrl Pts',(18.5258439248858,-16.8389459585693,
14.2762394491432));
#177934=CARTESIAN_POINT('Ctrl Pts',(18.7490749118662,-16.8342015245125,
14.2886071776783));
#177935=CARTESIAN_POINT('Ctrl Pts',(18.8091564934396,-16.8354820255666,
14.2919822494349));
#177936=CARTESIAN_POINT('Ctrl Pts',(18.8932432274277,-16.8408590982979,
14.2968207052173));
#177937=CARTESIAN_POINT('Ctrl Pts',(18.9173581669781,-16.8428167392094,
14.2982214758417));
#177938=CARTESIAN_POINT('Ctrl Pts',(18.9594161826665,-16.8469577075536,
14.3006904980823));
#177939=CARTESIAN_POINT('Ctrl Pts',(18.977374937732,-16.8489583651079,14.3017530750738));
#177940=CARTESIAN_POINT('Ctrl Pts',(19.0037768069369,-16.8522423120571,
14.3033282949119));
#177941=CARTESIAN_POINT('Ctrl Pts',(19.01224158611,-16.8533472202056,14.3038353154866));
#177942=CARTESIAN_POINT('Ctrl Pts',(19.0270865299337,-16.8553763227179,
14.3047280687395));
#177943=CARTESIAN_POINT('Ctrl Pts',(19.0334696257948,-16.8562785251909,
14.3051131014711));
#177944=CARTESIAN_POINT('Ctrl Pts',(19.0458676187016,-16.8580886859364,
14.3058632563624));
#177945=CARTESIAN_POINT('Ctrl Pts',(19.0518829247914,-16.8589934429909,
14.306228273523));
#177946=CARTESIAN_POINT('Ctrl Pts',(19.066272109426,-16.8612211697439,14.3071039899289));
#177947=CARTESIAN_POINT('Ctrl Pts',(19.0746420552448,-16.8625685321894,
14.3076154588562));
#177948=CARTESIAN_POINT('Ctrl Pts',(19.1049271193319,-16.8676305171145,
14.3094737797347));
#177949=CARTESIAN_POINT('Ctrl Pts',(19.1267908895736,-16.8716398564208,
14.3108299491941));
#177950=CARTESIAN_POINT('Ctrl Pts',(19.3294007880085,-16.9121018499462,
14.3235376178334));
#177951=CARTESIAN_POINT('Ctrl Pts',(19.5046902285641,-16.9716727409204,
14.3356765760265));
#177952=CARTESIAN_POINT('Ctrl Pts',(19.7426185366837,-17.0889564753652,
14.3531919332245));
#177953=CARTESIAN_POINT('Ctrl Pts',(19.8131220253681,-17.1288872980212,
14.3585128420122));
#177954=CARTESIAN_POINT('Ctrl Pts',(19.911632341301,-17.1924020726889,14.3659860246247));
#177955=CARTESIAN_POINT('Ctrl Pts',(19.9415884070687,-17.2128239305798,
14.368263613347));
#177956=CARTESIAN_POINT('Ctrl Pts',(19.977076867882,-17.2383766921879,14.3709540979527));
#177957=CARTESIAN_POINT('Ctrl Pts',(19.9831234246218,-17.2427792376527,
14.3714122243153));
#177958=CARTESIAN_POINT('Ctrl Pts',(19.9924983380312,-17.2496815055131,
14.3721219252348));
#177959=CARTESIAN_POINT('Ctrl Pts',(19.9958428000915,-17.2521591039025,
14.37237498762));
#177960=CARTESIAN_POINT('Ctrl Pts',(20.0020387373891,-17.2567774559933,
14.3728435516808));
#177961=CARTESIAN_POINT('Ctrl Pts',(20.0048920845525,-17.2589155298896,
14.3730592281751));
#177962=CARTESIAN_POINT('Ctrl Pts',(20.0113396306019,-17.2637722971219,
14.3735463525865));
#177963=CARTESIAN_POINT('Ctrl Pts',(20.014930548973,-17.2664952571287,14.3738174965195));
#177964=CARTESIAN_POINT('Ctrl Pts',(20.0257640529109,-17.2747648196623,
14.3746351320544));
#177965=CARTESIAN_POINT('Ctrl Pts',(20.032979617025,-17.2803468721445,14.3751791907405));
#177966=CARTESIAN_POINT('Ctrl Pts',(20.0884681320401,-17.3238497285166,
14.3793609724962));
#177967=CARTESIAN_POINT('Ctrl Pts',(20.1351119679583,-17.3638111044263,
14.3828641416323));
#177968=CARTESIAN_POINT('Ctrl Pts',(20.2872061039383,-17.5060398419072,
14.3945010096608));
#177969=CARTESIAN_POINT('Ctrl Pts',(20.3837338277971,-17.6172218003159,
14.4022872173824));
#177970=CARTESIAN_POINT('Ctrl Pts',(20.5211938675895,-17.8134787008976,
14.4154842761584));
#177971=CARTESIAN_POINT('Ctrl Pts',(20.5693505080626,-17.8928596401075,
14.4206926499907));
#177972=CARTESIAN_POINT('Ctrl Pts',(20.6218690755522,-17.9938332639764,
14.4273222592249));
#177973=CARTESIAN_POINT('Ctrl Pts',(20.6313137059699,-18.0126737551051,
14.4285591331837));
#177974=CARTESIAN_POINT('Ctrl Pts',(20.6443687957487,-18.0397169988001,
14.430335654894));
#177975=CARTESIAN_POINT('Ctrl Pts',(20.6482110792106,-18.0478069063957,
14.4308672368226));
#177976=CARTESIAN_POINT('Ctrl Pts',(20.6547602422308,-18.061824983953,14.4317886996085));
#177977=CARTESIAN_POINT('Ctrl Pts',(20.6574913145826,-18.0677417636292,
14.4321777378722));
#177978=CARTESIAN_POINT('Ctrl Pts',(20.6626744817152,-18.0791085643564,
14.4329253651094));
#177979=CARTESIAN_POINT('Ctrl Pts',(20.665130906204,-18.0845565512354,14.4332838003344));
#177980=CARTESIAN_POINT('Ctrl Pts',(20.6714720453677,-18.0987806934464,
14.4342199500857));
#177981=CARTESIAN_POINT('Ctrl Pts',(20.6753201734384,-18.1075729213761,
14.4347989114098));
#177982=CARTESIAN_POINT('Ctrl Pts',(20.6883060613078,-18.1378011210538,
14.4367906461468));
#177983=CARTESIAN_POINT('Ctrl Pts',(20.6971493581847,-18.1593610373518,
14.4382133627017));
#177984=CARTESIAN_POINT('Ctrl Pts',(20.7678865584375,-18.3402677991235,
14.4501731097673));
#177985=CARTESIAN_POINT('Ctrl Pts',(20.8106148009925,-18.506399219495,14.4613733882527));
#177986=CARTESIAN_POINT('Ctrl Pts',(20.8446793196122,-18.7652813297502,
14.4786282131894));
#177987=CARTESIAN_POINT('Ctrl Pts',(20.8507199765435,-18.8554102135709,
14.4845832112794));
#177988=CARTESIAN_POINT('Ctrl Pts',(20.8511062741943,-18.9842805476592,
14.492816667076));
#177989=CARTESIAN_POINT('Ctrl Pts',(20.8501648843296,-19.0229057614886,
14.49524767335));
#177990=CARTESIAN_POINT('Ctrl Pts',(20.8477729847385,-19.0690930749978,
14.4980939188358));
#177991=CARTESIAN_POINT('Ctrl Pts',(20.8473379911583,-19.0766978684573,
14.4985605793421));
#177992=CARTESIAN_POINT('Ctrl Pts',(20.8465999734401,-19.0884841591562,
14.4992805940618));
#177993=CARTESIAN_POINT('Ctrl Pts',(20.8463255636522,-19.0926672930147,
14.499535505224));
#177994=CARTESIAN_POINT('Ctrl Pts',(20.8457949436417,-19.1004042133233,
14.5000057705053));
#177995=CARTESIAN_POINT('Ctrl Pts',(20.8455421897163,-19.1039581385761,
14.5002213103369));
#177996=CARTESIAN_POINT('Ctrl Pts',(20.844952295327,-19.111966758852,14.5007059614379));
#177997=CARTESIAN_POINT('Ctrl Pts',(20.8446100268816,-19.1164210216253,
14.5009747819627));
#177998=CARTESIAN_POINT('Ctrl Pts',(20.8435639095311,-19.1294933131671,
14.501761642187));
#177999=CARTESIAN_POINT('Ctrl Pts',(20.842821348907,-19.1381082717019,14.5022775606373));
#178000=CARTESIAN_POINT('Ctrl Pts',(20.837275220557,-19.1981507254997,14.5058563523392));
#178001=CARTESIAN_POINT('Ctrl Pts',(20.830643309437,-19.2493963689155,14.5088242487981));
#178002=CARTESIAN_POINT('Ctrl Pts',(20.8185587282442,-19.3218354773013,
14.5129602891302));
#178003=CARTESIAN_POINT('Ctrl Pts',(20.8146434089476,-19.3432625994992,
14.5141762367099));
#178004=CARTESIAN_POINT('Ctrl Pts',(20.8014003700517,-19.409903629592,14.5179447994881));
#178005=CARTESIAN_POINT('Ctrl Pts',(20.7909238627403,-19.45487621983,14.5204691498698));
#178006=CARTESIAN_POINT('Ctrl Pts',(20.7507051162463,-19.6051064020344,
14.5289363649793));
#178007=CARTESIAN_POINT('Ctrl Pts',(20.7142828981661,-19.7083902818046,
14.5348247068131));
#178008=CARTESIAN_POINT('Ctrl Pts',(20.6477506739108,-19.8587994047399,
14.5439696281747));
#178009=CARTESIAN_POINT('Ctrl Pts',(20.623495817134,-19.9083115150446,14.5470774800121));
#178010=CARTESIAN_POINT('Ctrl Pts',(20.5810528673916,-19.9870178315409,
14.5522219968268));
#178011=CARTESIAN_POINT('Ctrl Pts',(20.5640366493465,-20.0168154168468,
14.554219263986));
#178012=CARTESIAN_POINT('Ctrl Pts',(20.5407177316318,-20.0554386606359,
14.5568800886423));
#178013=CARTESIAN_POINT('Ctrl Pts',(20.5350601990483,-20.0646490877286,
14.557520113803));
#178014=CARTESIAN_POINT('Ctrl Pts',(20.5256770207777,-20.0796657479039,
14.558572843665));
#178015=CARTESIAN_POINT('Ctrl Pts',(20.5219930462509,-20.0854978829294,
14.5589840069489));
#178016=CARTESIAN_POINT('Ctrl Pts',(20.514805789859,-20.0967538727245,14.5597820776845));
#178017=CARTESIAN_POINT('Ctrl Pts',(20.5113060650999,-20.1021799162912,
14.5601688497291));
#178018=CARTESIAN_POINT('Ctrl Pts',(20.5031665841764,-20.1146736759997,
14.5610642169183));
#178019=CARTESIAN_POINT('Ctrl Pts',(20.4985092254094,-20.1217297421348,
14.5615734681397));
#178020=CARTESIAN_POINT('Ctrl Pts',(20.4858668763241,-20.140636039178,14.5629477350517));
#178021=CARTESIAN_POINT('Ctrl Pts',(20.4778040714258,-20.1524334761901,
14.5638156785344));
#178022=CARTESIAN_POINT('Ctrl Pts',(20.4027425002855,-20.2599108981909,
14.5718202652279));
#178023=CARTESIAN_POINT('Ctrl Pts',(20.3280628686515,-20.3499585909559,
14.5792584515377));
#178024=CARTESIAN_POINT('Ctrl Pts',(20.132580043701,-20.5495285974901,14.5975057692211));
#178025=CARTESIAN_POINT('Ctrl Pts',(20.0058105119725,-20.6521828818894,
14.6084546158184));
#178026=CARTESIAN_POINT('Ctrl Pts',(19.840960588158,-20.7568253574901,14.620863600959));
#178027=CARTESIAN_POINT('Ctrl Pts',(19.8129751083141,-20.7736940749651,
14.6229114294141));
#178028=CARTESIAN_POINT('Ctrl Pts',(19.7783138859935,-20.793507556201,14.6253665621806));
#178029=CARTESIAN_POINT('Ctrl Pts',(19.7720005560008,-20.7970735544335,
14.6258105193929));
#178030=CARTESIAN_POINT('Ctrl Pts',(19.7620781585256,-20.8026110367418,
14.6265030697708));
#178031=CARTESIAN_POINT('Ctrl Pts',(19.7584815253384,-20.804604521816,14.6267530389589));
#178032=CARTESIAN_POINT('Ctrl Pts',(19.7517502413733,-20.8083098346129,
14.6272188513599));
#178033=CARTESIAN_POINT('Ctrl Pts',(19.7486171014945,-20.8100241907691,
14.6274348509351));
#178034=CARTESIAN_POINT('Ctrl Pts',(19.7414581823612,-20.8139178193558,
14.6279265434622));
#178035=CARTESIAN_POINT('Ctrl Pts',(19.7374296717057,-20.8160919639559,
14.6282019084627));
#178036=CARTESIAN_POINT('Ctrl Pts',(19.7250361554935,-20.8227287954197,
14.6290450966787));
#178037=CARTESIAN_POINT('Ctrl Pts',(19.7166480653741,-20.8271484407077,
14.6296102577913));
#178038=CARTESIAN_POINT('Ctrl Pts',(19.6008140007761,-20.8871901352769,
14.6373429775697));
#178039=CARTESIAN_POINT('Ctrl Pts',(19.4888054128516,-20.9335662313437,
14.6439804893635));
#178040=CARTESIAN_POINT('Ctrl Pts',(19.2028073969266,-21.0241835424842,
14.6603064431349));
#178041=CARTESIAN_POINT('Ctrl Pts',(19.0260361519297,-21.0563842011585,
14.6699251200044));
#178042=CARTESIAN_POINT('Ctrl Pts',(18.8258763563366,-21.067114455345,14.6815960702804));
#178043=CARTESIAN_POINT('Ctrl Pts',(18.8044107241675,-21.0679377835882,
14.6828564248385));
#178044=CARTESIAN_POINT('Ctrl Pts',(18.7739144021392,-21.0686429289018,
14.684660813919));
#178045=CARTESIAN_POINT('Ctrl Pts',(18.7648908277235,-21.0687938494076,
14.6851964272703));
#178046=CARTESIAN_POINT('Ctrl Pts',(18.7493378521133,-21.0689545059572,
14.6861226616634));
#178047=CARTESIAN_POINT('Ctrl Pts',(18.7428088152758,-21.0689917414342,
14.6865124162515));
#178048=CARTESIAN_POINT('Ctrl Pts',(18.7303180253181,-21.0690051925921,
14.6872598749605));
#178049=CARTESIAN_POINT('Ctrl Pts',(18.7243563316378,-21.068986429085,14.6876174178959));
#178050=CARTESIAN_POINT('Ctrl Pts',(18.7088771923154,-21.0688723237703,
14.6885478437945));
#178051=CARTESIAN_POINT('Ctrl Pts',(18.6993602465184,-21.0687379794065,
14.6891219436901));
#178052=CARTESIAN_POINT('Ctrl Pts',(18.6670303135176,-21.0680635107621,
14.6910793565644));
#178053=CARTESIAN_POINT('Ctrl Pts',(18.6442259007042,-21.0672187280819,
14.6924721559598));
#178054=CARTESIAN_POINT('Ctrl Pts',(18.4439242820799,-21.0565537158359,
14.7048164569888));
#178055=CARTESIAN_POINT('Ctrl Pts',(18.2683373930392,-21.0247817708654,
14.7164925038476));
#178056=CARTESIAN_POINT('Ctrl Pts',(18.0173335129665,-20.9458345030525,
14.7338754485258));
#178057=CARTESIAN_POINT('Ctrl Pts',(17.9374624474419,-20.9152923066633,
14.739501754004));
#178058=CARTESIAN_POINT('Ctrl Pts',(17.8255729443369,-20.8645505134323,
14.74734295224));
#178059=CARTESIAN_POINT('Ctrl Pts',(17.7919077579063,-20.8481940268046,
14.7496960751315));
#178060=CARTESIAN_POINT('Ctrl Pts',(17.751991916602,-20.8274749010043,14.7524633792915));
#178061=CARTESIAN_POINT('Ctrl Pts',(17.7453107263114,-20.8239614056363,
14.7529257930619));
#178062=CARTESIAN_POINT('Ctrl Pts',(17.7349616584056,-20.8184481886917,
14.7536406770263));
#178063=CARTESIAN_POINT('Ctrl Pts',(17.7312807435791,-20.8164732614186,
14.7538946696059));
#178064=CARTESIAN_POINT('Ctrl Pts',(17.7244699982195,-20.8127930778915,
14.7543640846775));
#178065=CARTESIAN_POINT('Ctrl Pts',(17.7213386562089,-20.8110908278804,
14.7545796874812));
#178066=CARTESIAN_POINT('Ctrl Pts',(17.7142752508495,-20.8072279010215,
14.7550655450462));
#178067=CARTESIAN_POINT('Ctrl Pts',(17.710345759237,-20.805062633852,14.7553355025786));
#178068=CARTESIAN_POINT('Ctrl Pts',(17.6987856735437,-20.7986446892405,
14.756128789491));
#178069=CARTESIAN_POINT('Ctrl Pts',(17.6911743769557,-20.7943571955166,
14.7566499452989));
#178070=CARTESIAN_POINT('Ctrl Pts',(17.6369037680884,-20.7633421219217,
14.7603592304453));
#178071=CARTESIAN_POINT('Ctrl Pts',(17.5912470088454,-20.7348900885347,
14.763444330768));
#178072=CARTESIAN_POINT('Ctrl Pts',(17.4071720841302,-20.6101995480509,
14.7759434078619));
#178073=CARTESIAN_POINT('Ctrl Pts',(17.2794066333268,-20.4993409289175,
14.7848132778786));
#178074=CARTESIAN_POINT('Ctrl Pts',(17.1115465626614,-20.3143267011366,
14.7986576589763));
#178075=CARTESIAN_POINT('Ctrl Pts',(17.060471157986,-20.2510721018573,14.803248767792));
#178076=CARTESIAN_POINT('Ctrl Pts',(17.0017259930104,-20.169087141203,14.8091326216188));
#178077=CARTESIAN_POINT('Ctrl Pts',(16.9905152035284,-20.1529725520273,
14.8102859077259));
#178078=CARTESIAN_POINT('Ctrl Pts',(16.9746597467292,-20.1294916668556,
14.8119628559975));
#178079=CARTESIAN_POINT('Ctrl Pts',(16.9698336794635,-20.1222486668776,
14.8124796554925));
#178080=CARTESIAN_POINT('Ctrl Pts',(16.9614964409842,-20.1095672917066,
14.8133837561062));
#178081=CARTESIAN_POINT('Ctrl Pts',(16.957965271981,-20.1041421548521,14.813770301005));
#178082=CARTESIAN_POINT('Ctrl Pts',(16.9511894776933,-20.0936269431713,
14.81451910815));
#178083=CARTESIAN_POINT('Ctrl Pts',(16.9479416283479,-20.0885390128369,
14.8148812452003));
#178084=CARTESIAN_POINT('Ctrl Pts',(16.9402801644432,-20.0764229744615,
14.815743212904));
#178085=CARTESIAN_POINT('Ctrl Pts',(16.9358860544753,-20.0693827051681,
14.816243759427));
#178086=CARTESIAN_POINT('Ctrl Pts',(16.9204544008849,-20.0443312629719,
14.8180238565611));
#178087=CARTESIAN_POINT('Ctrl Pts',(16.9096454486403,-20.026181385203,14.8193117372901));
#178088=CARTESIAN_POINT('Ctrl Pts',(16.8022349832156,-19.8395241725488,
14.8325423885839));
#178089=CARTESIAN_POINT('Ctrl Pts',(16.7290069376686,-19.6586727857104,
14.8453728731502));
#178090=CARTESIAN_POINT('Ctrl Pts',(16.6631797526465,-19.398055295425,14.8631017321562));
#178091=CARTESIAN_POINT('Ctrl Pts',(16.6487382168833,-19.3247554843099,
14.8679934972455));
#178092=CARTESIAN_POINT('Ctrl Pts',(16.6333272062598,-19.2166767412335,
14.8749433504138));
#178093=CARTESIAN_POINT('Ctrl Pts',(16.6292914350924,-19.1823956121774,
14.8771093014166));
#178094=CARTESIAN_POINT('Ctrl Pts',(16.6254128237801,-19.1406888023454,
14.8796857585881));
#178095=CARTESIAN_POINT('Ctrl Pts',(16.6247685436926,-19.1333450061363,
14.8801372228181));
#178096=CARTESIAN_POINT('Ctrl Pts',(16.623822466253,-19.1218732017602,14.8808388637963));
#178097=CARTESIAN_POINT('Ctrl Pts',(16.6234943983514,-19.1177475028299,
14.8810904753447));
#178098=CARTESIAN_POINT('Ctrl Pts',(16.622906023878,-19.1100631372184,14.881557733176));
#178099=CARTESIAN_POINT('Ctrl Pts',(16.6226426178642,-19.106504810681,14.8817735456592));
#178100=CARTESIAN_POINT('Ctrl Pts',(16.6220645668639,-19.098418333969,14.8822627418272));
#178101=CARTESIAN_POINT('Ctrl Pts',(16.6217554883487,-19.093889838036,14.8825358105878));
#178102=CARTESIAN_POINT('Ctrl Pts',(16.6209918952332,-19.0821461257066,
14.8832417434411));
#178103=CARTESIAN_POINT('Ctrl Pts',(16.6205597666391,-19.0749294441844,
14.883673383521));
#178104=CARTESIAN_POINT('Ctrl Pts',(16.6180743366898,-19.029524866141,14.8863762676856));
#178105=CARTESIAN_POINT('Ctrl Pts',(16.6170190193761,-18.9912868187921,
14.8885955085252));
#178106=CARTESIAN_POINT('Ctrl Pts',(16.6169207098347,-18.7909008080633,
14.9000236618683));
#178107=CARTESIAN_POINT('Ctrl Pts',(16.6354677289579,-18.629276688061,14.9085853047104));
#178108=CARTESIAN_POINT('Ctrl Pts',(16.6916958548057,-18.3880942781729,
14.9221735828745));
#178109=CARTESIAN_POINT('Ctrl Pts',(16.7161208887108,-18.3061287994777,
14.926935560901));
#178110=CARTESIAN_POINT('Ctrl Pts',(16.7454193926287,-18.2258896998479,
14.9318514575852));
#178111=CARTESIAN_POINT('Origin',(18.734,-18.952,0.));
#178112=CARTESIAN_POINT('',(16.7454193691905,-18.2258897640378,15.9575278689401));
#178113=CARTESIAN_POINT('',(16.7454193749215,-18.2258897483422,15.7328935260819));
#178114=CARTESIAN_POINT('',(16.7454193692319,-18.2258897639242,0.));
#178115=CARTESIAN_POINT('',(16.6170004656572,-18.9534041339617,15.9109437209775));
#178116=CARTESIAN_POINT('Ctrl Pts',(16.7454193691904,-18.2258897640378,
15.9575278689401));
#178117=CARTESIAN_POINT('Ctrl Pts',(16.7400018536359,-18.240726583525,15.9565689505998));
#178118=CARTESIAN_POINT('Ctrl Pts',(16.7347506147815,-18.2556234021838,
15.9556045111451));
#178119=CARTESIAN_POINT('Ctrl Pts',(16.6996529154685,-18.3588596237815,
15.9489084765267));
#178120=CARTESIAN_POINT('Ctrl Pts',(16.6755084838295,-18.449016641622,15.9429915915783));
#178121=CARTESIAN_POINT('Ctrl Pts',(16.6304385517586,-18.6764384866331,
15.92794103383));
#178122=CARTESIAN_POINT('Ctrl Pts',(16.6169140929087,-18.8147188280224,
15.9186647458253));
#178123=CARTESIAN_POINT('Ctrl Pts',(16.6170004105498,-18.9533184338415,
15.9096291502085));
#178124=CARTESIAN_POINT('Ctrl Pts',(16.7454193692319,-18.2258897639242,
15.1555945373748));
#178125=CARTESIAN_POINT('Ctrl Pts',(16.7703664756571,-18.1575677238728,
15.1599719862091));
#178126=CARTESIAN_POINT('Ctrl Pts',(16.7988694213885,-18.0904486586419,
15.1643494350433));
#178127=CARTESIAN_POINT('Ctrl Pts',(16.8307867059135,-18.0249249452108,
15.1687268838775));
#178128=CARTESIAN_POINT('Ctrl Pts',(16.8626811668449,-17.95944808685,15.1731012024607));
#178129=CARTESIAN_POINT('Ctrl Pts',(16.897984912061,-17.89556474928,15.1774755210439));
#178130=CARTESIAN_POINT('Ctrl Pts',(16.9365084077469,-17.8336472042422,
15.1818498396271));
#178131=CARTESIAN_POINT('Ctrl Pts',(16.9750170641353,-17.771753509918,15.1862224732175));
#178132=CARTESIAN_POINT('Ctrl Pts',(17.0167427546477,-17.7118245143087,
15.1905951068078));
#178133=CARTESIAN_POINT('Ctrl Pts',(17.061450917826,-17.6542062691942,15.1949677403982));
#178134=CARTESIAN_POINT('Ctrl Pts',(17.1061566074958,-17.596591211847,15.1993401320697));
#178135=CARTESIAN_POINT('Ctrl Pts',(17.1538441452889,-17.5412870313143,
15.2037125237412));
#178136=CARTESIAN_POINT('Ctrl Pts',(17.2042377414628,-17.4886079020457,
15.2080849154128));
#178137=CARTESIAN_POINT('Ctrl Pts',(17.254681022044,-17.435876835001,15.2124616179433));
#178138=CARTESIAN_POINT('Ctrl Pts',(17.3078353564725,-17.3857763388251,
15.2168383204739));
#178139=CARTESIAN_POINT('Ctrl Pts',(17.3633875710639,-17.3385841919562,
15.2212150230044));
#178140=CARTESIAN_POINT('Ctrl Pts',(17.4189660949095,-17.2913696951198,
15.2255937983196));
#178141=CARTESIAN_POINT('Ctrl Pts',(17.476944377479,-17.2470665850251,15.2299725736349));
#178142=CARTESIAN_POINT('Ctrl Pts',(17.5369777562186,-17.2059110137532,
15.2343513489501));
#178143=CARTESIAN_POINT('Ctrl Pts',(17.5971223014476,-17.1646792328712,
15.2387382326392));
#178144=CARTESIAN_POINT('Ctrl Pts',(17.6593291342759,-17.126606889442,15.2431251163283));
#178145=CARTESIAN_POINT('Ctrl Pts',(17.7232266804942,-17.0918854076764,
15.2475120000174));
#178146=CARTESIAN_POINT('Ctrl Pts',(17.7823156149067,-17.0597768920889,
15.2515687486396));
#178147=CARTESIAN_POINT('Ctrl Pts',(17.8428498273126,-17.030533487829,15.2556254972618));
#178148=CARTESIAN_POINT('Ctrl Pts',(17.9045214391032,-17.0042694444527,
15.2596822458839));
#178149=CARTESIAN_POINT('Ctrl Pts',(17.9712319856141,-16.9758594737004,
15.2640704548148));
#178150=CARTESIAN_POINT('Ctrl Pts',(18.0395340178847,-16.9508253061037,
15.2684586637457));
#178151=CARTESIAN_POINT('Ctrl Pts',(18.1090523123262,-16.9293459545263,
15.2728468726766));
#178152=CARTESIAN_POINT('Ctrl Pts',(18.1784674300925,-16.9078984818679,
15.2772285687779));
#178153=CARTESIAN_POINT('Ctrl Pts',(18.2490947695204,-16.8899954929979,
15.2816102648792));
#178154=CARTESIAN_POINT('Ctrl Pts',(18.3205388114184,-16.8757681137367,
15.2859919609805));
#178155=CARTESIAN_POINT('Ctrl Pts',(18.3918989008814,-16.8615574527783,
15.2903685082401));
#178156=CARTESIAN_POINT('Ctrl Pts',(18.464073315643,-16.8510139151847,15.2947450554998));
#178157=CARTESIAN_POINT('Ctrl Pts',(18.5366526876881,-16.84421845574,15.2991216027594));
#178158=CARTESIAN_POINT('Ctrl Pts',(18.6091860309502,-16.8374273058768,
15.3034953744764));
#178159=CARTESIAN_POINT('Ctrl Pts',(18.6821233428399,-16.8343795627893,
15.3078691461934));
#178160=CARTESIAN_POINT('Ctrl Pts',(18.7550478100786,-16.8351046342129,
15.3122429179104));
#178161=CARTESIAN_POINT('Ctrl Pts',(18.8279500861569,-16.8358294849948,
15.3166153586739));
#178162=CARTESIAN_POINT('Ctrl Pts',(18.9008390432801,-16.840324866202,15.3209877994375));
#178163=CARTESIAN_POINT('Ctrl Pts',(18.973297213937,-16.8485680796845,15.3253602402011));
#178164=CARTESIAN_POINT('Ctrl Pts',(19.0457572373573,-16.856811503947,15.3297327927684));
#178165=CARTESIAN_POINT('Ctrl Pts',(19.1177859733816,-16.8688028942383,
15.3341053453358));
#178166=CARTESIAN_POINT('Ctrl Pts',(19.1889721056856,-16.8844678036248,
15.3384778979031));
#178167=CARTESIAN_POINT('Ctrl Pts',(19.2602321176428,-16.9001489706452,
15.3428549884705));
#178168=CARTESIAN_POINT('Ctrl Pts',(19.3306473077957,-16.9195111648159,
15.3472320790378));
#178169=CARTESIAN_POINT('Ctrl Pts',(19.3998183959356,-16.9424291842202,
15.3516091696051));
#178170=CARTESIAN_POINT('Ctrl Pts',(19.469027260974,-16.9653597200056,15.3559886506641));
#178171=CARTESIAN_POINT('Ctrl Pts',(19.5369902214648,-16.9918497721618,
15.360368131723));
#178172=CARTESIAN_POINT('Ctrl Pts',(19.6033275197911,-17.0217257543722,
15.364747612782));
#178173=CARTESIAN_POINT('Ctrl Pts',(19.6697824005334,-17.0516546915606,
15.3691348564417));
#178174=CARTESIAN_POINT('Ctrl Pts',(19.7346054355421,-17.0849813228797,
15.3735221001015));
#178175=CARTESIAN_POINT('Ctrl Pts',(19.7974415556907,-17.1214861219783,
15.3779093437612));
#178176=CARTESIAN_POINT('Ctrl Pts',(19.8401640625164,-17.1463058677706,
15.3808922466959));
#178177=CARTESIAN_POINT('Ctrl Pts',(19.8819686426658,-17.1725938434287,
15.3838751496307));
#178178=CARTESIAN_POINT('Ctrl Pts',(19.9227521494642,-17.2002701900281,
15.3868580525654));
#178179=CARTESIAN_POINT('Ctrl Pts',(19.9827495924521,-17.2409854241402,
15.3912462614963));
#178180=CARTESIAN_POINT('Ctrl Pts',(20.0407699602753,-17.2848661041391,
15.3956344704272));
#178181=CARTESIAN_POINT('Ctrl Pts',(20.0964596300331,-17.3316936226349,
15.4000226793581));
#178182=CARTESIAN_POINT('Ctrl Pts',(20.1520666470875,-17.3784516413291,
15.4044043754594));
#178183=CARTESIAN_POINT('Ctrl Pts',(20.2053494667964,-17.4281475084506,
15.4087860715606));
#178184=CARTESIAN_POINT('Ctrl Pts',(20.2559837460593,-17.4805196308713,
15.4131677676619));
#178185=CARTESIAN_POINT('Ctrl Pts',(20.3065585260145,-17.5328302118802,
15.4175443149215));
#178186=CARTESIAN_POINT('Ctrl Pts',(20.354490614394,-17.5878104559203,15.4219208621811));
#178187=CARTESIAN_POINT('Ctrl Pts',(20.3994903578935,-17.6451599685639,
15.4262974094408));
#178188=CARTESIAN_POINT('Ctrl Pts',(20.4444615632096,-17.7024731109801,
15.4306711811577));
#178189=CARTESIAN_POINT('Ctrl Pts',(20.4865038163907,-17.7621521621709,
15.4350449528747));
#178190=CARTESIAN_POINT('Ctrl Pts',(20.5253667770628,-17.8238625659807,
15.4394187245917));
#178191=CARTESIAN_POINT('Ctrl Pts',(20.5642179116054,-17.8855541911073,
15.4437911653552));
#178192=CARTESIAN_POINT('Ctrl Pts',(20.599891417462,-17.9492755337059,15.4481636061188));
#178193=CARTESIAN_POINT('Ctrl Pts',(20.6321804129387,-18.0146632835871,
15.4525360468823));
#178194=CARTESIAN_POINT('Ctrl Pts',(20.6644702340486,-18.0800527054402,
15.4569085994496));
#178195=CARTESIAN_POINT('Ctrl Pts',(20.6933751611692,-18.1471081857717,
15.461281152017));
#178196=CARTESIAN_POINT('Ctrl Pts',(20.7187351546652,-18.2154435759318,
15.4656537045843));
#178197=CARTESIAN_POINT('Ctrl Pts',(20.744121467719,-18.2838498871373,15.4700307951516));
#178198=CARTESIAN_POINT('Ctrl Pts',(20.7659553334552,-18.3535383070817,
15.4744078857189));
#178199=CARTESIAN_POINT('Ctrl Pts',(20.7841259040682,-18.4241053348739,
15.4787849762863));
#178200=CARTESIAN_POINT('Ctrl Pts',(20.8023063983042,-18.4947109019391,
15.4831644573452));
#178201=CARTESIAN_POINT('Ctrl Pts',(20.8168195180768,-18.5661955591485,
15.4875439384041));
#178202=CARTESIAN_POINT('Ctrl Pts',(20.8276056664123,-18.6381460314631,
15.4919234194631));
#178203=CARTESIAN_POINT('Ctrl Pts',(20.8384109331234,-18.710224035507,15.4963106631228));
#178204=CARTESIAN_POINT('Ctrl Pts',(20.8454759896221,-18.7827690229248,
15.5006979067825));
#178205=CARTESIAN_POINT('Ctrl Pts',(20.8487932306453,-18.8553636113216,
15.5050851504422));
#178206=CARTESIAN_POINT('Ctrl Pts',(20.8510486348925,-18.9047209362348,
15.5080680533771));
#178207=CARTESIAN_POINT('Ctrl Pts',(20.8515726338748,-18.9541011550575,
15.511050956312));
#178208=CARTESIAN_POINT('Ctrl Pts',(20.8503765449711,-19.0033743116382,
15.5140338592469));
#178209=CARTESIAN_POINT('Ctrl Pts',(20.8486169543561,-19.0758610503894,
15.5184220681777));
#178210=CARTESIAN_POINT('Ctrl Pts',(20.8431255714046,-19.148398777627,15.5228102771086));
#178211=CARTESIAN_POINT('Ctrl Pts',(20.8338948009669,-19.2205718244197,
15.5271984860395));
#178212=CARTESIAN_POINT('Ctrl Pts',(20.824677730523,-19.2926377544445,15.5315801821408));
#178213=CARTESIAN_POINT('Ctrl Pts',(20.8117323505351,-19.364339603947,15.5359618782421));
#178214=CARTESIAN_POINT('Ctrl Pts',(20.7951030586573,-19.4352630563093,
15.5403435743433));
#178215=CARTESIAN_POINT('Ctrl Pts',(20.7784933075209,-19.5061031679707,
15.544720121603));
#178216=CARTESIAN_POINT('Ctrl Pts',(20.7582083534313,-19.5761662321966,
15.5490966688626));
#178217=CARTESIAN_POINT('Ctrl Pts',(20.7343439967237,-19.6450460985904,
15.5534732161222));
#178218=CARTESIAN_POINT('Ctrl Pts',(20.7104947744443,-19.713882282374,15.5578469878392));
#178219=CARTESIAN_POINT('Ctrl Pts',(20.6830708110599,-19.7815363024755,
15.5622207595562));
#178220=CARTESIAN_POINT('Ctrl Pts',(20.6522179108565,-19.8476165733558,
15.5665945312731));
#178221=CARTESIAN_POINT('Ctrl Pts',(20.6213743992941,-19.9136767357877,
15.5709669720367));
#178222=CARTESIAN_POINT('Ctrl Pts',(20.5871042264084,-19.9781636629362,
15.5753394128002));
#178223=CARTESIAN_POINT('Ctrl Pts',(20.5496008974363,-20.0407067471218,
15.5797118535638));
#178224=CARTESIAN_POINT('Ctrl Pts',(20.5120966094999,-20.1032514305409,
15.5840844061311));
#178225=CARTESIAN_POINT('Ctrl Pts',(20.471359251126,-20.1638517596412,15.5884569586985));
#178226=CARTESIAN_POINT('Ctrl Pts',(20.4276268858003,-20.2221641514759,
15.5928295112658));
#178227=CARTESIAN_POINT('Ctrl Pts',(20.3838491333763,-20.2805370621104,
15.5972066018331));
#178228=CARTESIAN_POINT('Ctrl Pts',(20.3370704580455,-20.3366169078809,
15.6015836924004));
#178229=CARTESIAN_POINT('Ctrl Pts',(20.287570140387,-20.3900920759457,15.6059607829678));
#178230=CARTESIAN_POINT('Ctrl Pts',(20.2380427887679,-20.4435964487845,
15.6103402640267));
#178231=CARTESIAN_POINT('Ctrl Pts',(20.1857911812168,-20.494492974896,15.6147197450856));
#178232=CARTESIAN_POINT('Ctrl Pts',(20.1311305579277,-20.5425078447165,
15.6190992261446));
#178233=CARTESIAN_POINT('Ctrl Pts',(20.0763730490507,-20.5906078205715,
15.6234864698043));
#178234=CARTESIAN_POINT('Ctrl Pts',(20.0191983762087,-20.6358156407823,
15.627873713464));
#178235=CARTESIAN_POINT('Ctrl Pts',(19.959953375359,-20.6778989893519,15.6322609571237));
#178236=CARTESIAN_POINT('Ctrl Pts',(19.9196724836153,-20.7065116112378,
15.6352438600586));
#178237=CARTESIAN_POINT('Ctrl Pts',(19.8784351648856,-20.7336807873357,
15.6382267629934));
#178238=CARTESIAN_POINT('Ctrl Pts',(19.8363568176097,-20.7593456909704,
15.6412096659283));
#178239=CARTESIAN_POINT('Ctrl Pts',(19.7744545085683,-20.7971018505909,
15.6455978748592));
#178240=CARTESIAN_POINT('Ctrl Pts',(19.7104893778662,-20.8317477625258,
15.6499860837901));
#178241=CARTESIAN_POINT('Ctrl Pts',(19.644806826183,-20.8630520467477,15.654374292721));
#178242=CARTESIAN_POINT('Ctrl Pts',(19.579221758297,-20.8943098702214,15.6587559888223));
#178243=CARTESIAN_POINT('Ctrl Pts',(19.5119247612699,-20.9222357055049,
15.6631376849236));
#178244=CARTESIAN_POINT('Ctrl Pts',(19.4432882414188,-20.9466426222722,
15.6675193810248));
#178245=CARTESIAN_POINT('Ctrl Pts',(19.3747323749407,-20.97102085897,15.6718959282845));
#178246=CARTESIAN_POINT('Ctrl Pts',(19.3048405647327,-20.9918882305585,
15.6762724755441));
#178247=CARTESIAN_POINT('Ctrl Pts',(19.234006173908,-21.0091054484527,15.6806490228038));
#178248=CARTESIAN_POINT('Ctrl Pts',(19.1632167052245,-21.0263117474376,
15.6850227945208));
#178249=CARTESIAN_POINT('Ctrl Pts',(19.0914863095564,-21.0398723720885,
15.6893965662378));
#178250=CARTESIAN_POINT('Ctrl Pts',(19.0192231694669,-21.0496979629106,
15.6937703379548));
#178251=CARTESIAN_POINT('Ctrl Pts',(18.9469820192935,-21.0595205637724,
15.6981427787183));
#178252=CARTESIAN_POINT('Ctrl Pts',(18.8742089242411,-21.0656103223221,
15.7025152194819));
#178253=CARTESIAN_POINT('Ctrl Pts',(18.8013202474328,-21.0679293429332,
15.7068876602454));
#178254=CARTESIAN_POINT('Ctrl Pts',(18.728429706853,-21.0702484228418,15.7112602128128));
#178255=CARTESIAN_POINT('Ctrl Pts',(18.6554240608469,-21.0687965600418,
15.7156327653801));
#178256=CARTESIAN_POINT('Ctrl Pts',(18.582721067549,-21.0635879533177,15.7200053179475));
#178257=CARTESIAN_POINT('Ctrl Pts',(18.5099426203423,-21.0583739409051,
15.7243824085148));
#178258=CARTESIAN_POINT('Ctrl Pts',(18.4374679351483,-21.0493954347148,
15.7287594990822));
#178259=CARTESIAN_POINT('Ctrl Pts',(18.3657101983337,-21.0367185953957,
15.7331365896495));
#178260=CARTESIAN_POINT('Ctrl Pts',(18.2939132719558,-21.0240348327841,
15.7375160707085));
#178261=CARTESIAN_POINT('Ctrl Pts',(18.2228345439085,-21.0076488240848,
15.7418955517674));
#178262=CARTESIAN_POINT('Ctrl Pts',(18.1528748782415,-20.9876774284894,
15.7462750328264));
#178263=CARTESIAN_POINT('Ctrl Pts',(18.0827912095367,-20.9676706337294,
15.7506622764861));
#178264=CARTESIAN_POINT('Ctrl Pts',(18.0138310210261,-20.9440659176032,
15.7550495201458));
#178265=CARTESIAN_POINT('Ctrl Pts',(17.9463773894235,-20.9170291660199,
15.7594367638056));
#178266=CARTESIAN_POINT('Ctrl Pts',(17.9005154197516,-20.8986467801989,
15.7624196667403));
#178267=CARTESIAN_POINT('Ctrl Pts',(17.8553494637696,-20.8786788808127,
15.765402569675));
#178268=CARTESIAN_POINT('Ctrl Pts',(17.8109931300721,-20.8571895753615,
15.7683854726098));
#178269=CARTESIAN_POINT('Ctrl Pts',(17.7457396290593,-20.8255762228108,
15.7727736815407));
#178270=CARTESIAN_POINT('Ctrl Pts',(17.6819847879021,-20.7905448456105,
15.7771618904716));
#178271=CARTESIAN_POINT('Ctrl Pts',(17.6201101194241,-20.7522606294508,
15.7815500994025));
#178272=CARTESIAN_POINT('Ctrl Pts',(17.558327283213,-20.7140332334155,15.7859317955037));
#178273=CARTESIAN_POINT('Ctrl Pts',(17.4984194869967,-20.6725628338802,
15.790313491605));
#178274=CARTESIAN_POINT('Ctrl Pts',(17.4407454860729,-20.6280613837826,
15.7946951877063));
#178275=CARTESIAN_POINT('Ctrl Pts',(17.38313925669,-20.5836122264304,15.7990717349659));
#178276=CARTESIAN_POINT('Ctrl Pts',(17.3277619882547,-20.5361393871241,
15.8034482822256));
#178277=CARTESIAN_POINT('Ctrl Pts',(17.2749437204166,-20.4858982277218,
15.8078248294852));
#178278=CARTESIAN_POINT('Ctrl Pts',(17.2221589491563,-20.4356889305326,
15.8121986012022));
#178279=CARTESIAN_POINT('Ctrl Pts',(17.1719303071397,-20.3827151282831,
15.8165723729191));
#178280=CARTESIAN_POINT('Ctrl Pts',(17.1245538730402,-20.3272716693127,
15.8209461446361));
#178281=CARTESIAN_POINT('Ctrl Pts',(17.0771918557487,-20.2718450819731,
15.8253185853997));
#178282=CARTESIAN_POINT('Ctrl Pts',(17.0326806364326,-20.2139506964276,
15.8296910261632));
#178283=CARTESIAN_POINT('Ctrl Pts',(16.9912774487785,-20.1539180959882,
15.8340634669268));
#178284=CARTESIAN_POINT('Ctrl Pts',(16.9498732024403,-20.0938839605086,
15.8384360194941));
#178285=CARTESIAN_POINT('Ctrl Pts',(16.9115774177713,-20.0317118998147,
15.8428085720614));
#178286=CARTESIAN_POINT('Ctrl Pts',(16.8766042803955,-19.9677608679187,
15.8471811246288));
#178287=CARTESIAN_POINT('Ctrl Pts',(16.8415948465786,-19.9037434652296,
15.8515582151961));
#178288=CARTESIAN_POINT('Ctrl Pts',(16.8099151769008,-19.8379438292392,
15.8559353057634));
#178289=CARTESIAN_POINT('Ctrl Pts',(16.7817332906702,-19.7707451957982,
15.8603123963308));
#178290=CARTESIAN_POINT('Ctrl Pts',(16.7535360132656,-19.7035098626894,
15.8646918773897));
#178291=CARTESIAN_POINT('Ctrl Pts',(16.7288404860623,-19.6348744651307,
15.8690713584486));
#178292=CARTESIAN_POINT('Ctrl Pts',(16.7077654290805,-19.5652393200137,
15.8734508395076));
#178293=CARTESIAN_POINT('Ctrl Pts',(16.6866530167017,-19.4954807470694,
15.8778380831673));
#178294=CARTESIAN_POINT('Ctrl Pts',(16.6691740053291,-19.4247193565783,
15.882225326827));
#178295=CARTESIAN_POINT('Ctrl Pts',(16.6553962633247,-19.3533670463298,
15.8866125704867));
#178296=CARTESIAN_POINT('Ctrl Pts',(16.6460287263818,-19.3048543508531,
15.8895954734216));
#178297=CARTESIAN_POINT('Ctrl Pts',(16.6383710944438,-19.2560686843218,
15.8925783763564));
#178298=CARTESIAN_POINT('Ctrl Pts',(16.6324309574258,-19.207140273759,15.8955612792912));
#178299=CARTESIAN_POINT('Ctrl Pts',(16.6222201199426,-19.1230344615427,
15.9006887598533));
#178300=CARTESIAN_POINT('Ctrl Pts',(16.617056776629,-19.0383036553196,15.9058162404154));
#178301=CARTESIAN_POINT('Ctrl Pts',(16.6170004656572,-18.9534041339617,
15.9109437209775));
#178302=CARTESIAN_POINT('',(16.6170004208928,-18.9533349381466,15.6876313477606));
#178303=CARTESIAN_POINT('Ctrl Pts',(16.7454193926287,-18.2258896998479,
14.9318514575852));
#178304=CARTESIAN_POINT('Ctrl Pts',(16.7539898784969,-18.2024179187845,
14.933289470365));
#178305=CARTESIAN_POINT('Ctrl Pts',(16.7629774004005,-18.1790938469297,
14.9347402968244));
#178306=CARTESIAN_POINT('Ctrl Pts',(16.7777126709423,-18.1427842604912,
14.9370362380879));
#178307=CARTESIAN_POINT('Ctrl Pts',(16.7831788110695,-18.129694155967,14.9378716791207));
#178308=CARTESIAN_POINT('Ctrl Pts',(16.7921001473088,-18.1089193795933,
14.9392103624449));
#178309=CARTESIAN_POINT('Ctrl Pts',(16.7954704382948,-18.101198550981,14.9397107178972));
#178310=CARTESIAN_POINT('Ctrl Pts',(16.8015031078548,-18.0876005617751,
14.9405970648266));
#178311=CARTESIAN_POINT('Ctrl Pts',(16.8041464536433,-18.0817150379637,
14.9409824002202));
#178312=CARTESIAN_POINT('Ctrl Pts',(16.8096767348037,-18.0695507221011,
14.941782396109));
#178313=CARTESIAN_POINT('Ctrl Pts',(16.8125675896862,-18.0632738060156,
14.9421971882002));
#178314=CARTESIAN_POINT('Ctrl Pts',(16.8200827102869,-18.0471642848501,
14.9432669153005));
#178315=CARTESIAN_POINT('Ctrl Pts',(16.8247519940797,-18.0373530143986,
14.9439234032379));
#178316=CARTESIAN_POINT('Ctrl Pts',(16.8446948431519,-17.9962665451481,
14.9466939011902));
#178317=CARTESIAN_POINT('Ctrl Pts',(16.8606622630466,-17.9653359690922,
14.9488319833083));
#178318=CARTESIAN_POINT('Ctrl Pts',(16.904394922929,-17.8855130233668,14.9544918278066));
#178319=CARTESIAN_POINT('Ctrl Pts',(16.9333566758698,-17.8373108233625,
14.958053815934));
#178320=CARTESIAN_POINT('Ctrl Pts',(17.0332350965844,-17.6851475752947,
14.9697636289789));
#178321=CARTESIAN_POINT('Ctrl Pts',(17.111503950185,-17.5863432978684,14.9781230573006));
#178322=CARTESIAN_POINT('Ctrl Pts',(17.2668972608481,-17.4225228703116,
14.993000550841));
#178323=CARTESIAN_POINT('Ctrl Pts',(17.3407869996825,-17.3549236006907,
14.9995201462719));
#178324=CARTESIAN_POINT('Ctrl Pts',(17.4267853808941,-17.2867754164596,
15.0062995425205));
#178325=CARTESIAN_POINT('Ctrl Pts',(17.4344245246477,-17.2808068435704,
15.0068951742375));
#178326=CARTESIAN_POINT('Ctrl Pts',(17.445764031804,-17.2720718978711,15.0077693324552));
#178327=CARTESIAN_POINT('Ctrl Pts',(17.4494327578829,-17.2692649229632,
15.0080506243749));
#178328=CARTESIAN_POINT('Ctrl Pts',(17.4559575636467,-17.2643065100323,
15.0085481504069));
#178329=CARTESIAN_POINT('Ctrl Pts',(17.458809932902,-17.2621502792693,15.0087647193588));
#178330=CARTESIAN_POINT('Ctrl Pts',(17.4649328356691,-17.2575460405312,
15.0092276116425));
#178331=CARTESIAN_POINT('Ctrl Pts',(17.4682049867318,-17.2551002759807,
15.0094737787569));
#178332=CARTESIAN_POINT('Ctrl Pts',(17.4772061297981,-17.2484129081427,
15.0101476971184));
#178333=CARTESIAN_POINT('Ctrl Pts',(17.4829495580454,-17.2441906995523,
15.0105741162415));
#178334=CARTESIAN_POINT('Ctrl Pts',(17.5137221087292,-17.2218071938327,
15.0128403481282));
#178335=CARTESIAN_POINT('Ctrl Pts',(17.5391269881891,-17.204165914299,15.014646426112));
#178336=CARTESIAN_POINT('Ctrl Pts',(17.6171834029864,-17.1524608758435,
15.020031900505));
#178337=CARTESIAN_POINT('Ctrl Pts',(17.6709725467387,-17.1201719094805,
15.0235245474624));
#178338=CARTESIAN_POINT('Ctrl Pts',(17.8443350931063,-17.0263166707742,
15.0343589181434));
#178339=CARTESIAN_POINT('Ctrl Pts',(17.9683762754242,-16.9737227332602,
15.0415276660066));
#178340=CARTESIAN_POINT('Ctrl Pts',(18.1354764545173,-16.9209600364709,
15.0512527095806));
#178341=CARTESIAN_POINT('Ctrl Pts',(18.1747299561353,-16.9098025216839,
15.0535399420459));
#178342=CARTESIAN_POINT('Ctrl Pts',(18.2613894649474,-16.8878561283963,
15.058620684093));
#178343=CARTESIAN_POINT('Ctrl Pts',(18.3088928166469,-16.8775521239902,
15.0614259917412));
#178344=CARTESIAN_POINT('Ctrl Pts',(18.3691073314938,-16.8666460311403,
15.0650250106284));
#178345=CARTESIAN_POINT('Ctrl Pts',(18.3815281410285,-16.8645107393646,
15.0657696551922));
#178346=CARTESIAN_POINT('Ctrl Pts',(18.4012400690407,-16.8613029570123,
15.0669552616516));
#178347=CARTESIAN_POINT('Ctrl Pts',(18.408519118623,-16.8601573933581,15.0673939008005));
#178348=CARTESIAN_POINT('Ctrl Pts',(18.4220931019255,-16.8580937091542,
15.0682134771367));
#178349=CARTESIAN_POINT('Ctrl Pts',(18.4283864969468,-16.8571659127048,
15.0685941026791));
#178350=CARTESIAN_POINT('Ctrl Pts',(18.4423736159789,-16.8551682495619,
15.0694415068844));
#178351=CARTESIAN_POINT('Ctrl Pts',(18.4500692114948,-16.8541123380093,
15.069908721841));
#178352=CARTESIAN_POINT('Ctrl Pts',(18.4724466377461,-16.851167316905,15.0712702319319));
#178353=CARTESIAN_POINT('Ctrl Pts',(18.4871424631253,-16.8493898452894,
15.0721680353832));
#178354=CARTESIAN_POINT('Ctrl Pts',(18.6040634087039,-16.8364908184537,
15.0793414001929));
#178355=CARTESIAN_POINT('Ctrl Pts',(18.7069418159813,-16.8326781665324,
15.0858477816265));
#178356=CARTESIAN_POINT('Ctrl Pts',(18.965368629394,-16.8419222242805,15.1026338888025));
#178357=CARTESIAN_POINT('Ctrl Pts',(19.1199577291818,-16.8646589701208,
15.1131041057439));
#178358=CARTESIAN_POINT('Ctrl Pts',(19.3214646282975,-16.9174646787792,
15.126560009598));
#178359=CARTESIAN_POINT('Ctrl Pts',(19.3717727497202,-16.9326695224225,
15.1298978648114));
#178360=CARTESIAN_POINT('Ctrl Pts',(19.4296851269129,-16.9525534015036,
15.1336748205914));
#178361=CARTESIAN_POINT('Ctrl Pts',(19.4378857908484,-16.955425609842,15.1342080917586));
#178362=CARTESIAN_POINT('Ctrl Pts',(19.4502843211664,-16.9598539687521,
15.1350117163951));
#178363=CARTESIAN_POINT('Ctrl Pts',(19.4544952026125,-16.9613730378522,
15.1352841886319));
#178364=CARTESIAN_POINT('Ctrl Pts',(19.4620494556115,-16.9641253337935,
15.135772129925));
#178365=CARTESIAN_POINT('Ctrl Pts',(19.4653945443353,-16.9653536501286,
15.1359878848015));
#178366=CARTESIAN_POINT('Ctrl Pts',(19.472661416482,-16.968042887147,15.1364559127081));
#178367=CARTESIAN_POINT('Ctrl Pts',(19.4765819616605,-16.9695069874646,
15.1367079928655));
#178368=CARTESIAN_POINT('Ctrl Pts',(19.487595219813,-16.9736570659245,15.1374149860329));
#178369=CARTESIAN_POINT('Ctrl Pts',(19.4946779603429,-16.9763695779007,
15.1378683410873));
#178370=CARTESIAN_POINT('Ctrl Pts',(19.5371983186418,-16.9929163730567,
15.1405829201818));
#178371=CARTESIAN_POINT('Ctrl Pts',(19.5722747537141,-17.0076666850721,
15.1427926120918));
#178372=CARTESIAN_POINT('Ctrl Pts',(19.6869971606401,-17.0595919727712,
15.1499806666271));
#178373=CARTESIAN_POINT('Ctrl Pts',(19.7647300150421,-17.1007815328418,
15.1547896820693));
#178374=CARTESIAN_POINT('Ctrl Pts',(19.9882626432145,-17.23768638006,15.1690493655377));
#178375=CARTESIAN_POINT('Ctrl Pts',(20.1250233222925,-17.346667222233,15.1784223751174));
#178376=CARTESIAN_POINT('Ctrl Pts',(20.2630319169469,-17.4876628575787,
15.1898859632073));
#178377=CARTESIAN_POINT('Ctrl Pts',(20.2789076767094,-17.5044219957036,
15.1912382672544));
#178378=CARTESIAN_POINT('Ctrl Pts',(20.3009669070879,-17.528484937568,15.1931673748106));
#178379=CARTESIAN_POINT('Ctrl Pts',(20.3073801376038,-17.5355765608708,
15.1937344020104));
#178380=CARTESIAN_POINT('Ctrl Pts',(20.3177190137002,-17.5471659450041,
15.1946587518003));
#178381=CARTESIAN_POINT('Ctrl Pts',(20.321674106934,-17.5516373450142,15.1950148328205));
#178382=CARTESIAN_POINT('Ctrl Pts',(20.3299107460889,-17.561028961372,15.195761622865));
#178383=CARTESIAN_POINT('Ctrl Pts',(20.3341885660916,-17.5659523488508,
15.196152481349));
#178384=CARTESIAN_POINT('Ctrl Pts',(20.3443064351711,-17.5777063820968,
15.1970841584231));
#178385=CARTESIAN_POINT('Ctrl Pts',(20.3501258395364,-17.5845545604108,
15.1976258199015));
#178386=CARTESIAN_POINT('Ctrl Pts',(20.3695622157234,-17.6077243391253,
15.1994547284389));
#178387=CARTESIAN_POINT('Ctrl Pts',(20.3829765887197,-17.6242135065956,
15.2007501645598));
#178388=CARTESIAN_POINT('Ctrl Pts',(20.4545184434044,-17.714910408525,15.2078448722442));
#178389=CARTESIAN_POINT('Ctrl Pts',(20.5078810142697,-17.7927259127434,
15.2138291957854));
#178390=CARTESIAN_POINT('Ctrl Pts',(20.6403914491075,-18.0166399543896,
15.2307281692643));
#178391=CARTESIAN_POINT('Ctrl Pts',(20.7078162865442,-18.168882804642,15.2419109716618));
#178392=CARTESIAN_POINT('Ctrl Pts',(20.769161436931,-18.3675594989172,15.2552398700389));
#178393=CARTESIAN_POINT('Ctrl Pts',(20.7803558491844,-18.4080505025665,
15.2578907606393));
#178394=CARTESIAN_POINT('Ctrl Pts',(20.792106572206,-18.4560749532719,15.2609373330676));
#178395=CARTESIAN_POINT('Ctrl Pts',(20.7938361672691,-18.4633086022078,
15.2613936389829));
#178396=CARTESIAN_POINT('Ctrl Pts',(20.7965741903848,-18.4750326150644,
15.2621288594024));
#178397=CARTESIAN_POINT('Ctrl Pts',(20.7976061437692,-18.4795173426932,
15.2624090739161));
#178398=CARTESIAN_POINT('Ctrl Pts',(20.7994135294787,-18.4874908777551,
15.2629054110361));
#178399=CARTESIAN_POINT('Ctrl Pts',(20.8001947580573,-18.4909783141237,
15.263121862514));
#178400=CARTESIAN_POINT('Ctrl Pts',(20.8018524619569,-18.498467228507,15.2635852994625));
#178401=CARTESIAN_POINT('Ctrl Pts',(20.8027261536057,-18.5024692654762,
15.2638321245483));
#178402=CARTESIAN_POINT('Ctrl Pts',(20.8050989856604,-18.5134917056192,
15.2645097029506));
#178403=CARTESIAN_POINT('Ctrl Pts',(20.8065740581177,-18.5205173124898,
15.264939099931));
#178404=CARTESIAN_POINT('Ctrl Pts',(20.8143549360015,-18.5585374801061,
15.2672500908868));
#178405=CARTESIAN_POINT('Ctrl Pts',(20.8200016235565,-18.5896646818428,
15.2690963516887));
#178406=CARTESIAN_POINT('Ctrl Pts',(20.8505127930543,-18.7823525349615,
15.2803089243486));
#178407=CARTESIAN_POINT('Ctrl Pts',(20.8572959209056,-18.9462309529907,
15.2889470804902));
#178408=CARTESIAN_POINT('Ctrl Pts',(20.8364521778122,-19.2260284817361,
15.3043057680651));
#178409=CARTESIAN_POINT('Ctrl Pts',(20.818085161711,-19.3418467941423,15.310841027446));
#178410=CARTESIAN_POINT('Ctrl Pts',(20.7868423563593,-19.4694278260755,
15.3185359648139));
#178411=CARTESIAN_POINT('Ctrl Pts',(20.7833021630712,-19.4832757521026,
15.3193776637806));
#178412=CARTESIAN_POINT('Ctrl Pts',(20.7774449089722,-19.5052570850802,
15.3207244921903));
#178413=CARTESIAN_POINT('Ctrl Pts',(20.7752188322162,-19.5134144405317,
15.3212266787146));
#178414=CARTESIAN_POINT('Ctrl Pts',(20.7712067808673,-19.52777706159,15.3221151562499));
#178415=CARTESIAN_POINT('Ctrl Pts',(20.7694411640473,-19.5339879371094,
15.3225007809202));
#178416=CARTESIAN_POINT('Ctrl Pts',(20.765730681969,-19.546816791544,15.3233002830423));
#178417=CARTESIAN_POINT('Ctrl Pts',(20.7637818324674,-19.5534335294864,
15.3237142866932));
#178418=CARTESIAN_POINT('Ctrl Pts',(20.7586966803705,-19.5703923897565,
15.3247796707361));
#178419=CARTESIAN_POINT('Ctrl Pts',(20.7555134858669,-19.5807201403548,
15.325432579931));
#178420=CARTESIAN_POINT('Ctrl Pts',(20.7419000498259,-19.6237159947741,
15.328168187452));
#178421=CARTESIAN_POINT('Ctrl Pts',(20.7307563656462,-19.6561511115615,
15.3302742074545));
#178422=CARTESIAN_POINT('Ctrl Pts',(20.6996742239813,-19.7399386847355,
15.3358289959565));
#178423=CARTESIAN_POINT('Ctrl Pts',(20.678511633313,-19.7908064221735,15.3393161552602));
#178424=CARTESIAN_POINT('Ctrl Pts',(20.6094731179962,-19.9400546181705,
15.3498858328151));
#178425=CARTESIAN_POINT('Ctrl Pts',(20.5559342362382,-20.0356067170176,
15.3571167414476));
#178426=CARTESIAN_POINT('Ctrl Pts',(20.4696764998539,-20.1649476915121,
15.3673864091129));
#178427=CARTESIAN_POINT('Ctrl Pts',(20.4428466986765,-20.2024631831195,
15.3704265460418));
#178428=CARTESIAN_POINT('Ctrl Pts',(20.4015473052407,-20.2563968172339,
15.3748628270667));
#178429=CARTESIAN_POINT('Ctrl Pts',(20.3880145998484,-20.2735145936583,
15.3762810095849));
#178430=CARTESIAN_POINT('Ctrl Pts',(20.3415255029232,-20.3304864629098,
15.3810282506029));
#178431=CARTESIAN_POINT('Ctrl Pts',(20.3073715064803,-20.3693447809194,
15.3843123436245));
#178432=CARTESIAN_POINT('Ctrl Pts',(20.2658813861545,-20.413199243317,15.3880359756918));
#178433=CARTESIAN_POINT('Ctrl Pts',(20.2598985749258,-20.4194458609474,
15.3885667885746));
#178434=CARTESIAN_POINT('Ctrl Pts',(20.2507673997294,-20.4288634389345,
15.3893674502862));
#178435=CARTESIAN_POINT('Ctrl Pts',(20.2476470881257,-20.4320613012977,
15.3896393950357));
#178436=CARTESIAN_POINT('Ctrl Pts',(20.2420203092301,-20.4377915202144,
15.3901267748702));
#178437=CARTESIAN_POINT('Ctrl Pts',(20.2395175646328,-20.4403274363343,
15.3903424928276));
#178438=CARTESIAN_POINT('Ctrl Pts',(20.23405649581,-20.4458330158099,15.3908108816896));
#178439=CARTESIAN_POINT('Ctrl Pts',(20.2310957600289,-20.4488002056881,
15.3910633573256));
#178440=CARTESIAN_POINT('Ctrl Pts',(20.2227314768663,-20.4571330764128,
15.3917725791028));
#178441=CARTESIAN_POINT('Ctrl Pts',(20.2173077001495,-20.4624784866368,
15.3922277514971));
#178442=CARTESIAN_POINT('Ctrl Pts',(20.1842244755602,-20.4947336564113,
15.3949765615158));
#178443=CARTESIAN_POINT('Ctrl Pts',(20.1558604345399,-20.5209141120957,
15.3972171441048));
#178444=CARTESIAN_POINT('Ctrl Pts',(20.0589544815258,-20.6055716758488,
15.4045580810294));
#178445=CARTESIAN_POINT('Ctrl Pts',(19.9873951814078,-20.6604515687314,
15.4094807701987));
#178446=CARTESIAN_POINT('Ctrl Pts',(19.7703838425376,-20.8058842291388,
15.4236858474793));
#178447=CARTESIAN_POINT('Ctrl Pts',(19.617205868654,-20.8835586278959,15.4329071198529));
#178448=CARTESIAN_POINT('Ctrl Pts',(19.4344668356363,-20.9498932474798,
15.4442004818327));
#178449=CARTESIAN_POINT('Ctrl Pts',(19.4124498592442,-20.9574767366913,
15.4455644109655));
#178450=CARTESIAN_POINT('Ctrl Pts',(19.3811909128918,-20.9676698590786,
15.4475072847831));
#178451=CARTESIAN_POINT('Ctrl Pts',(19.3720489314345,-20.9705823280256,
15.4480762603632));
#178452=CARTESIAN_POINT('Ctrl Pts',(19.3571816552308,-20.9752076841959,
15.4490029216618));
#178453=CARTESIAN_POINT('Ctrl Pts',(19.3514682853889,-20.9769586722245,
15.4493593532819));
#178454=CARTESIAN_POINT('Ctrl Pts',(19.3395085365729,-20.9805686788854,
15.4501061775866));
#178455=CARTESIAN_POINT('Ctrl Pts',(19.3332608417802,-20.9824230876476,
15.450496716635));
#178456=CARTESIAN_POINT('Ctrl Pts',(19.3184050206524,-20.9867579767451,
15.4514263441498));
#178457=CARTESIAN_POINT('Ctrl Pts',(19.3097895677072,-20.98921270906,15.4519662656662));
#178458=CARTESIAN_POINT('Ctrl Pts',(19.2808413694828,-20.9972623885439,
15.4537832264802));
#178459=CARTESIAN_POINT('Ctrl Pts',(19.2604411623725,-21.0026080496847,
15.4550683098663));
#178460=CARTESIAN_POINT('Ctrl Pts',(19.1497844519941,-21.029844440252,15.4620661600873));
#178461=CARTESIAN_POINT('Ctrl Pts',(19.0582528190898,-21.0460798449994,
15.4679583697048));
#178462=CARTESIAN_POINT('Ctrl Pts',(18.8138452422157,-21.0730219504027,
15.4839175569266));
#178463=CARTESIAN_POINT('Ctrl Pts',(18.6603709972031,-21.0732459581053,
15.4941952255566));
#178464=CARTESIAN_POINT('Ctrl Pts',(18.504928816888,-21.0565727218587,15.5043123765119));
#178465=CARTESIAN_POINT('Ctrl Pts',(18.5016396530041,-21.0562121133199,
15.5045263010876));
#178466=CARTESIAN_POINT('Ctrl Pts',(18.4463584969669,-21.0500201466498,
15.508119005645));
#178467=CARTESIAN_POINT('Ctrl Pts',(18.3945945228599,-21.0422705749683,
15.5114427770827));
#178468=CARTESIAN_POINT('Ctrl Pts',(18.334640634137,-21.0310085027146,15.51520555058));
#178469=CARTESIAN_POINT('Ctrl Pts',(18.3261244042237,-21.0293545103693,
15.515737968209));
#178470=CARTESIAN_POINT('Ctrl Pts',(18.3132323169734,-21.026768316934,15.5165405642306));
#178471=CARTESIAN_POINT('Ctrl Pts',(18.308848970586,-21.0258745417867,15.5168128534451));
#178472=CARTESIAN_POINT('Ctrl Pts',(18.3009792698467,-21.0242438911216,
15.517300599761));
#178473=CARTESIAN_POINT('Ctrl Pts',(18.2974919301759,-21.0235121053444,
15.5175163416602));
#178474=CARTESIAN_POINT('Ctrl Pts',(18.2899105488846,-21.0219012277284,
15.5179844940444));
#178475=CARTESIAN_POINT('Ctrl Pts',(18.2858172758937,-21.0210187963508,
15.5182367108281));
#178476=CARTESIAN_POINT('Ctrl Pts',(18.274307120353,-21.0185016665517,15.518944473656));
#178477=CARTESIAN_POINT('Ctrl Pts',(18.2668962910998,-21.0168391730474,
15.5193984562993));
#178478=CARTESIAN_POINT('Ctrl Pts',(18.2222370765169,-21.0065678980349,
15.522124791579));
#178479=CARTESIAN_POINT('Ctrl Pts',(18.1852159989921,-20.9969907259359,
15.5243450917027));
#178480=CARTESIAN_POINT('Ctrl Pts',(18.0632993635277,-20.9619017332701,
15.5315853686935));
#178481=CARTESIAN_POINT('Ctrl Pts',(17.9797430098427,-20.9320614146232,
15.5364331799524));
#178482=CARTESIAN_POINT('Ctrl Pts',(17.7392675851407,-20.8287407235072,
15.550669209331));
#178483=CARTESIAN_POINT('Ctrl Pts',(17.5892360359658,-20.7411777446196,
15.5599856754051));
#178484=CARTESIAN_POINT('Ctrl Pts',(17.4330672552499,-20.6222700422172,
15.5713889394683));
#178485=CARTESIAN_POINT('Ctrl Pts',(17.4148286011103,-20.6079030098277,
15.5727489053254));
#178486=CARTESIAN_POINT('Ctrl Pts',(17.3894007872719,-20.5871861660199,
15.5746870842445));
#178487=CARTESIAN_POINT('Ctrl Pts',(17.3820124270668,-20.5810826984707,
15.5752553941233));
#178488=CARTESIAN_POINT('Ctrl Pts',(17.3700863783538,-20.5710936713861,
15.5761812654653));
#178489=CARTESIAN_POINT('Ctrl Pts',(17.3655231949928,-20.5672386563803,
15.5765375771153));
#178490=CARTESIAN_POINT('Ctrl Pts',(17.3563662784197,-20.5594361616393,
15.5772567650024));
#178491=CARTESIAN_POINT('Ctrl Pts',(17.3517730494286,-20.5554881790995,
15.5776196601031));
#178492=CARTESIAN_POINT('Ctrl Pts',(17.3407758110547,-20.5459534441586,
15.5784937145474));
#178493=CARTESIAN_POINT('Ctrl Pts',(17.3343884149842,-20.5403477675266,
15.5790056581806));
#178494=CARTESIAN_POINT('Ctrl Pts',(17.3141046862124,-20.522329101273,15.5806452238866));
#178495=CARTESIAN_POINT('Ctrl Pts',(17.3003387035503,-20.5097713056291,
15.5817789174205));
#178496=CARTESIAN_POINT('Ctrl Pts',(17.2684734255031,-20.4799225576682,
15.5844535762565));
#178497=CARTESIAN_POINT('Ctrl Pts',(17.2505117783673,-20.462489356358,15.5860005246433));
#178498=CARTESIAN_POINT('Ctrl Pts',(17.1883633529826,-20.3999914731401,
15.5914949787602));
#178499=CARTESIAN_POINT('Ctrl Pts',(17.1458897746575,-20.3532767985085,
15.5955120527167));
#178500=CARTESIAN_POINT('Ctrl Pts',(17.0460471666817,-20.2330859220675,
15.6056165632377));
#178501=CARTESIAN_POINT('Ctrl Pts',(16.9913226606222,-20.1575868650647,
15.6117716441221));
#178502=CARTESIAN_POINT('Ctrl Pts',(16.8765740252499,-19.9750611031889,
15.6260169947454));
#178503=CARTESIAN_POINT('Ctrl Pts',(16.8205080328898,-19.865915016324,15.6340846131507));
#178504=CARTESIAN_POINT('Ctrl Pts',(16.7706163236359,-19.7437719914218,
15.642232947836));
#178505=CARTESIAN_POINT('Ctrl Pts',(16.7671005791807,-19.7349974604127,
15.6428135502771));
#178506=CARTESIAN_POINT('Ctrl Pts',(16.7619716143272,-19.7219441213306,
15.6436699197268));
#178507=CARTESIAN_POINT('Ctrl Pts',(16.7603133509283,-19.7176833001007,
15.6439482954824));
#178508=CARTESIAN_POINT('Ctrl Pts',(16.7573845202505,-19.7100850856542,
15.6444426143378));
#178509=CARTESIAN_POINT('Ctrl Pts',(16.7561085836893,-19.7067498246512,
15.6446588761142));
#178510=CARTESIAN_POINT('Ctrl Pts',(16.7533801739178,-19.69956340522,15.6451232922391));
#178511=CARTESIAN_POINT('Ctrl Pts',(16.7519304948998,-19.6957112463241,
15.6453712789052));
#178512=CARTESIAN_POINT('Ctrl Pts',(16.7479520837355,-19.6850453566173,
15.6460553299809));
#178513=CARTESIAN_POINT('Ctrl Pts',(16.7454471631092,-19.6782227199235,
15.6464899947657));
#178514=CARTESIAN_POINT('Ctrl Pts',(16.7317897365044,-19.6404235417277,
15.6488828422822));
#178515=CARTESIAN_POINT('Ctrl Pts',(16.7213252060677,-19.609201153953,15.6508026668322));
#178516=CARTESIAN_POINT('Ctrl Pts',(16.6636029018366,-19.4226428511168,
15.6620104021434));
#178517=CARTESIAN_POINT('Ctrl Pts',(16.6336098822308,-19.2625187434697,
15.6705925842714));
#178518=CARTESIAN_POINT('Ctrl Pts',(16.618771005776,-19.0515351732291,15.6821718102302));
#178519=CARTESIAN_POINT('Ctrl Pts',(16.617031386799,-19.0024419403517,15.6848816867355));
#178520=CARTESIAN_POINT('Ctrl Pts',(16.6170004208928,-18.9533349381466,
15.6876313477606));
#178521=CARTESIAN_POINT('Ctrl Pts',(16.6170004192074,-18.9533322627481,
15.6876314975649));
#178522=CARTESIAN_POINT('Ctrl Pts',(16.6169565169202,-18.8835704055676,
15.6915376931939));
#178523=CARTESIAN_POINT('Ctrl Pts',(16.62036089015,-18.8138535640072,15.6955212326732));
#178524=CARTESIAN_POINT('Ctrl Pts',(16.6282125589666,-18.734158587401,15.7002202348787));
#178525=CARTESIAN_POINT('Ctrl Pts',(16.6293001576506,-18.7238899479628,
15.7008284385311));
#178526=CARTESIAN_POINT('Ctrl Pts',(16.6312632475932,-18.7065663360107,
15.7018593087927));
#178527=CARTESIAN_POINT('Ctrl Pts',(16.6320992366459,-18.6995070050852,
15.7022807358949));
#178528=CARTESIAN_POINT('Ctrl Pts',(16.6337047671108,-18.6865103049005,
15.7030591555859));
#178529=CARTESIAN_POINT('Ctrl Pts',(16.6344639731179,-18.6805717144542,
15.7034158195831));
#178530=CARTESIAN_POINT('Ctrl Pts',(16.6360832810977,-18.6683187506339,
15.7041537754714));
#178531=CARTESIAN_POINT('Ctrl Pts',(16.6369467236812,-18.6620048869433,
15.7045351694354));
#178532=CARTESIAN_POINT('Ctrl Pts',(16.6389488845612,-18.6478409232857,
15.7053933353336));
#178533=CARTESIAN_POINT('Ctrl Pts',(16.6401032377709,-18.639993162409,15.7058705976374));
#178534=CARTESIAN_POINT('Ctrl Pts',(16.6431522412091,-18.6200441629729,
15.7070884153629));
#178535=CARTESIAN_POINT('Ctrl Pts',(16.6451078418647,-18.6079526631919,
15.7078308924383));
#178536=CARTESIAN_POINT('Ctrl Pts',(16.6571524976023,-18.5373722396685,
15.7121907850031));
#178537=CARTESIAN_POINT('Ctrl Pts',(16.6695919036022,-18.4793163395534,
15.7158823634575));
#178538=CARTESIAN_POINT('Ctrl Pts',(16.6997698414317,-18.3626461002099,
15.7235211131819));
#178539=CARTESIAN_POINT('Ctrl Pts',(16.7176452909224,-18.3041241696756,
15.7274691240795));
#178540=CARTESIAN_POINT('Ctrl Pts',(16.7404566265233,-18.2395907584607,
15.7319399041205));
#178541=CARTESIAN_POINT('Ctrl Pts',(16.7429205066429,-18.232733338599,15.7324164674271));
#178542=CARTESIAN_POINT('Ctrl Pts',(16.7454193749215,-18.2258897483422,
15.7328935260819));
#178543=CARTESIAN_POINT('Origin',(18.734,-18.952,0.));
#178544=CARTESIAN_POINT('',(16.7454192974512,-18.2258899605083,16.7554728927777));
#178545=CARTESIAN_POINT('',(16.7454193692319,-18.2258897639242,16.5356516076535));
#178546=CARTESIAN_POINT('',(16.7454193692319,-18.2258897639242,0.));
#178547=CARTESIAN_POINT('Ctrl Pts',(16.7454192974512,-18.2258899605083,
16.7554728927777));
#178548=CARTESIAN_POINT('Ctrl Pts',(16.7246695920637,-18.2827166967783,
16.7521869458714));
#178549=CARTESIAN_POINT('Ctrl Pts',(16.7063536199304,-18.3404386255704,
16.7488940241178));
#178550=CARTESIAN_POINT('Ctrl Pts',(16.6648838452894,-18.493651950924,16.7401350888319));
#178551=CARTESIAN_POINT('Ctrl Pts',(16.645861750119,-18.5900612109107,16.7345998833666));
#178552=CARTESIAN_POINT('Ctrl Pts',(16.6317631855524,-18.70199076929,16.7279812705224));
#178553=CARTESIAN_POINT('Ctrl Pts',(16.6300811167997,-18.7165651764132,
16.7271159336786));
#178554=CARTESIAN_POINT('Ctrl Pts',(16.6277432519347,-18.7388535224522,
16.7257867711579));
#178555=CARTESIAN_POINT('Ctrl Pts',(16.6269780369073,-18.7465557149213,
16.7253263933704));
#178556=CARTESIAN_POINT('Ctrl Pts',(16.6257184973669,-18.7599814909001,
16.7245219962028));
#178557=CARTESIAN_POINT('Ctrl Pts',(16.625205197225,-18.7657032448873,16.7241785780139));
#178558=CARTESIAN_POINT('Ctrl Pts',(16.6241033853643,-18.7785735781056,
16.7234047182599));
#178559=CARTESIAN_POINT('Ctrl Pts',(16.6235279049427,-18.7857231757729,
16.7229738710155));
#178560=CARTESIAN_POINT('Ctrl Pts',(16.6220830309384,-18.8048914690991,
16.7218161189399));
#178561=CARTESIAN_POINT('Ctrl Pts',(16.6212799114272,-18.8169147602251,
16.7210871425985));
#178562=CARTESIAN_POINT('Ctrl Pts',(16.6181723376229,-18.8702856926723,
16.7178385079915));
#178563=CARTESIAN_POINT('Ctrl Pts',(16.6169788916296,-18.9116865673218,
16.7152843363529));
#178564=CARTESIAN_POINT('Ctrl Pts',(16.6170878342108,-19.1225723393612,
16.7020917135601));
#178565=CARTESIAN_POINT('Ctrl Pts',(16.6375272228444,-19.2914052006955,
16.6908605394253));
#178566=CARTESIAN_POINT('Ctrl Pts',(16.7025602568232,-19.5567378422221,
16.6728475754346));
#178567=CARTESIAN_POINT('Ctrl Pts',(16.7346397976448,-19.6555760008162,
16.6660710230332));
#178568=CARTESIAN_POINT('Ctrl Pts',(16.7775028814751,-19.7606419935097,
16.6590602329866));
#178569=CARTESIAN_POINT('Ctrl Pts',(16.7812238449539,-19.7695867812862,
16.6584650042628));
#178570=CARTESIAN_POINT('Ctrl Pts',(16.7868091127715,-19.7827574707192,
16.6575913224019));
#178571=CARTESIAN_POINT('Ctrl Pts',(16.7886259927884,-19.7870031733232,
16.6573101081016));
#178572=CARTESIAN_POINT('Ctrl Pts',(16.7918742110331,-19.7945254916574,
16.6568126678403));
#178573=CARTESIAN_POINT('Ctrl Pts',(16.7932999703058,-19.7978044571216,
16.6565961074699));
#178574=CARTESIAN_POINT('Ctrl Pts',(16.7963728344805,-19.8048227613399,
16.6561331765346));
#178575=CARTESIAN_POINT('Ctrl Pts',(16.7980224549729,-19.808560938065,16.6558869624849));
#178576=CARTESIAN_POINT('Ctrl Pts',(16.8025810936737,-19.8188107470481,
16.6552127833076));
#178577=CARTESIAN_POINT('Ctrl Pts',(16.8055122409406,-19.825312561095,16.6547861520224));
#178578=CARTESIAN_POINT('Ctrl Pts',(16.8213484140837,-19.8599715103299,
16.65251676682));
#178579=CARTESIAN_POINT('Ctrl Pts',(16.8348380827748,-19.8878592805146,
16.6507078589996));
#178580=CARTESIAN_POINT('Ctrl Pts',(16.9233519936901,-20.0610449154679,
16.6395212075378));
#178581=CARTESIAN_POINT('Ctrl Pts',(17.0143947885187,-20.1975509179192,
16.6308786888292));
#178582=CARTESIAN_POINT('Ctrl Pts',(17.196466169748,-20.4119804038316,16.6154835501062));
#178583=CARTESIAN_POINT('Ctrl Pts',(17.2800216251338,-20.4952091871193,
16.608913302389));
#178584=CARTESIAN_POINT('Ctrl Pts',(17.380992329486,-20.5802701785601,16.6011789840365));
#178585=CARTESIAN_POINT('Ctrl Pts',(17.3920227713541,-20.5893730893443,
16.6003368065505));
#178586=CARTESIAN_POINT('Ctrl Pts',(17.409722114742,-20.6036805445389,16.598989355451));
#178587=CARTESIAN_POINT('Ctrl Pts',(17.4163315616311,-20.6089581835253,
16.5984870290645));
#178588=CARTESIAN_POINT('Ctrl Pts',(17.4280424983855,-20.6181949771008,
16.5975983885361));
#178589=CARTESIAN_POINT('Ctrl Pts',(17.4331308375226,-20.6221706854176,
16.5972127415187));
#178590=CARTESIAN_POINT('Ctrl Pts',(17.4436912521112,-20.6303443929479,
16.5964132759632));
#178591=CARTESIAN_POINT('Ctrl Pts',(17.4491658059688,-20.6345390510522,
16.5959993316345));
#178592=CARTESIAN_POINT('Ctrl Pts',(17.4632677541215,-20.6452351458732,
16.5949342747658));
#178593=CARTESIAN_POINT('Ctrl Pts',(17.4719245142755,-20.6516973735035,
16.5942816352357));
#178594=CARTESIAN_POINT('Ctrl Pts',(17.5082358322577,-20.6783732399568,
16.591548639891));
#178595=CARTESIAN_POINT('Ctrl Pts',(17.5363282210755,-20.6979795111006,
16.5894450180728));
#178596=CARTESIAN_POINT('Ctrl Pts',(17.6107288172203,-20.747264617646,16.5838980606411));
#178597=CARTESIAN_POINT('Ctrl Pts',(17.65773750538,-20.7758342643689,16.5804164690477));
#178598=CARTESIAN_POINT('Ctrl Pts',(17.8013465148784,-20.8556263858028,
16.5698574889258));
#178599=CARTESIAN_POINT('Ctrl Pts',(17.9008524232842,-20.9012299985079,
16.5626316748121));
#178600=CARTESIAN_POINT('Ctrl Pts',(18.0393939197642,-20.9521700144381,
16.5528807854854));
#178601=CARTESIAN_POINT('Ctrl Pts',(18.0757162153561,-20.9644165205872,
16.550353032336));
#178602=CARTESIAN_POINT('Ctrl Pts',(18.1433460128919,-20.985191624372,16.5457179372652));
#178603=CARTESIAN_POINT('Ctrl Pts',(18.1745562879807,-20.9939998016045,
16.5436063985128));
#178604=CARTESIAN_POINT('Ctrl Pts',(18.2120838153806,-21.0036657907865,
16.5411087272298));
#178605=CARTESIAN_POINT('Ctrl Pts',(18.2182171631365,-21.0052162787845,
16.5407018266001));
#178606=CARTESIAN_POINT('Ctrl Pts',(18.2665317275001,-21.0171998718105,
16.5375072608297));
#178607=CARTESIAN_POINT('Ctrl Pts',(18.3090215578563,-21.0263603873719,
16.5347619590204));
#178608=CARTESIAN_POINT('Ctrl Pts',(18.3591553016936,-21.0355635070149,
16.5316205812639));
#178609=CARTESIAN_POINT('Ctrl Pts',(18.3665514941911,-21.0368805805222,
16.5311596175139));
#178610=CARTESIAN_POINT('Ctrl Pts',(18.3785117016488,-21.0389447656501,
16.5304183816415));
#178611=CARTESIAN_POINT('Ctrl Pts',(18.3830713522644,-21.0397163289763,
16.5301367754393));
#178612=CARTESIAN_POINT('Ctrl Pts',(18.3911615310593,-21.0410580588519,
16.5296389017171));
#178613=CARTESIAN_POINT('Ctrl Pts',(18.3946910093723,-21.0416342260313,
16.5294222976174));
#178614=CARTESIAN_POINT('Ctrl Pts',(18.4022522865027,-21.0428488986275,
16.5289595602004));
#178615=CARTESIAN_POINT('Ctrl Pts',(18.406284465869,-21.0434846859682,16.5287135818993));
#178616=CARTESIAN_POINT('Ctrl Pts',(18.4173486414224,-21.0451964845796,
16.5280407131526));
#178617=CARTESIAN_POINT('Ctrl Pts',(18.4243843361549,-21.0462487316264,
16.5276151479222));
#178618=CARTESIAN_POINT('Ctrl Pts',(18.461834575018,-21.0516568740241,16.5253615574399));
#178619=CARTESIAN_POINT('Ctrl Pts',(18.4923376455223,-21.0553859694736,
16.523566822637));
#178620=CARTESIAN_POINT('Ctrl Pts',(18.5846792262413,-21.0646395112173,
16.5182275421597));
#178621=CARTESIAN_POINT('Ctrl Pts',(18.6466926646594,-21.0681098622425,
16.5147680059268));
#178622=CARTESIAN_POINT('Ctrl Pts',(18.8556388020453,-21.0705999193564,
16.5032794219685));
#178623=CARTESIAN_POINT('Ctrl Pts',(19.0022847612066,-21.0570619012732,
16.4954668615935));
#178624=CARTESIAN_POINT('Ctrl Pts',(19.2195938395234,-21.0139078096739,
16.4830959578587));
#178625=CARTESIAN_POINT('Ctrl Pts',(19.2920097291687,-20.9954991035761,
16.4788410329755));
#178626=CARTESIAN_POINT('Ctrl Pts',(19.3758190961901,-20.9694065653792,
16.4736906390922));
#178627=CARTESIAN_POINT('Ctrl Pts',(19.3883045083419,-20.9653918150907,
16.4729174212191));
#178628=CARTESIAN_POINT('Ctrl Pts',(19.4085312642726,-20.9586797854283,
16.4716547581577));
#178629=CARTESIAN_POINT('Ctrl Pts',(19.4162957788978,-20.9560530569173,
16.4711676383336));
#178630=CARTESIAN_POINT('Ctrl Pts',(19.4300950343634,-20.951295290973,16.4702975271425));
#178631=CARTESIAN_POINT('Ctrl Pts',(19.4361357656776,-20.9491818451356,
16.4699151228316));
#178632=CARTESIAN_POINT('Ctrl Pts',(19.44884398157,-20.9446708922582,16.4691074187185));
#178633=CARTESIAN_POINT('Ctrl Pts',(19.4555091875467,-20.9422672416602,
16.4686819181977));
#178634=CARTESIAN_POINT('Ctrl Pts',(19.4731068882467,-20.9358210273962,
16.467553465513));
#178635=CARTESIAN_POINT('Ctrl Pts',(19.4840181638137,-20.9317215982123,
16.466848620884));
#178636=CARTESIAN_POINT('Ctrl Pts',(19.5345545425301,-20.9122570365838,
16.4635596353019));
#178637=CARTESIAN_POINT('Ctrl Pts',(19.5737427897822,-20.8957918774756,
16.4609387457589));
#178638=CARTESIAN_POINT('Ctrl Pts',(19.6803243755859,-20.8471863477512,
16.4536089749656));
#178639=CARTESIAN_POINT('Ctrl Pts',(19.7465497052036,-20.812645673675,16.4488238339975));
#178640=CARTESIAN_POINT('Ctrl Pts',(19.8888734742627,-20.7285634160326,
16.4380545960301));
#178641=CARTESIAN_POINT('Ctrl Pts',(19.9638932674497,-20.6774772302302,
16.4320430114774));
#178642=CARTESIAN_POINT('Ctrl Pts',(20.1201754941372,-20.5556702515601,
16.4189701264334));
#178643=CARTESIAN_POINT('Ctrl Pts',(20.1998034725076,-20.4832303688943,
16.4119383050303));
#178644=CARTESIAN_POINT('Ctrl Pts',(20.2802157596568,-20.3980286880123,
16.4047004456004));
#178645=CARTESIAN_POINT('Ctrl Pts',(20.2867920040622,-20.3909646076896,
16.4041074892436));
#178646=CARTESIAN_POINT('Ctrl Pts',(20.2964385206063,-20.3804593554748,
16.4032364942098));
#178647=CARTESIAN_POINT('Ctrl Pts',(20.2995461201574,-20.3770528437594,
16.4029557183089));
#178648=CARTESIAN_POINT('Ctrl Pts',(20.3050431785446,-20.3709873537681,
16.4024587622354));
#178649=CARTESIAN_POINT('Ctrl Pts',(20.3074370541459,-20.3683324526115,
16.4022422500809));
#178650=CARTESIAN_POINT('Ctrl Pts',(20.3125557152281,-20.3626266641098,
16.4017790994339));
#178651=CARTESIAN_POINT('Ctrl Pts',(20.3152783791295,-20.3595739482974,
16.4015326191452));
#178652=CARTESIAN_POINT('Ctrl Pts',(20.3227373011253,-20.3511618712906,
16.4008569593889));
#178653=CARTESIAN_POINT('Ctrl Pts',(20.3274553248212,-20.3457863125969,
16.4004291235405));
#178654=CARTESIAN_POINT('Ctrl Pts',(20.3526454098058,-20.3167904779122,
16.3981417303946));
#178655=CARTESIAN_POINT('Ctrl Pts',(20.3726208588295,-20.2927415583613,
16.3963166586658));
#178656=CARTESIAN_POINT('Ctrl Pts',(20.4938881886454,-20.1399840740441,
16.3851021957151));
#178657=CARTESIAN_POINT('Ctrl Pts',(20.5805004428922,-20.0003134258405,
16.3764475570268));
#178658=CARTESIAN_POINT('Ctrl Pts',(20.6999637618455,-19.7459808249813,
16.3610664055762));
#178659=CARTESIAN_POINT('Ctrl Pts',(20.7408830393391,-19.6359840904026,
16.3545261415905));
#178660=CARTESIAN_POINT('Ctrl Pts',(20.7763480645627,-19.509411619263,16.3468255708633));
#178661=CARTESIAN_POINT('Ctrl Pts',(20.7800651782993,-19.4956088679742,
16.3459838010905));
#178662=CARTESIAN_POINT('Ctrl Pts',(20.7857582392627,-19.4735828139439,
16.3446368805025));
#178663=CARTESIAN_POINT('Ctrl Pts',(20.7878252239812,-19.4653833366579,
16.344134673243));
#178664=CARTESIAN_POINT('Ctrl Pts',(20.7913838268615,-19.4509012751989,
16.3432461714996));
#178665=CARTESIAN_POINT('Ctrl Pts',(20.7928959373918,-19.4446238027058,
16.3428605434722));
#178666=CARTESIAN_POINT('Ctrl Pts',(20.795963893721,-19.4316263948014,16.3420610466401));
#178667=CARTESIAN_POINT('Ctrl Pts',(20.7975156612635,-19.4249055842003,
16.3416470516966));
#178668=CARTESIAN_POINT('Ctrl Pts',(20.8014142116704,-19.4076361032048,
16.3405817158572));
#178669=CARTESIAN_POINT('Ctrl Pts',(20.803713097208,-19.397076925514,16.3399288464261));
#178670=CARTESIAN_POINT('Ctrl Pts',(20.8129681953377,-19.3529436891469,
16.3371936247649));
#178671=CARTESIAN_POINT('Ctrl Pts',(20.81918876568,-19.3192222686824,16.33508795909));
#178672=CARTESIAN_POINT('Ctrl Pts',(20.8332586100318,-19.23098823302,16.3295343279965));
#178673=CARTESIAN_POINT('Ctrl Pts',(20.8398041894306,-19.1762967732665,
16.3260479917225));
#178674=CARTESIAN_POINT('Ctrl Pts',(20.8529620952653,-19.0124045270463,
16.315479895195));
#178675=CARTESIAN_POINT('Ctrl Pts',(20.8532530398053,-18.9028863096366,
16.3082497393259));
#178676=CARTESIAN_POINT('Ctrl Pts',(20.8362310514469,-18.6756725496535,
16.2931984531219));
#178677=CARTESIAN_POINT('Ctrl Pts',(20.8174699425562,-18.5584370576244,
16.285405373538));
#178678=CARTESIAN_POINT('Ctrl Pts',(20.7867038640797,-18.4341326998506,
16.2774959409879));
#178679=CARTESIAN_POINT('Ctrl Pts',(20.7843534156278,-18.4249036397557,
16.2769109240264));
#178680=CARTESIAN_POINT('Ctrl Pts',(20.7807789197147,-18.4112541397232,
16.2760493247114));
#178681=CARTESIAN_POINT('Ctrl Pts',(20.7796026961359,-18.4068214585382,
16.2757700880254));
#178682=CARTESIAN_POINT('Ctrl Pts',(20.7774846398149,-18.398942780428,16.2752748258948));
#178683=CARTESIAN_POINT('Ctrl Pts',(20.7765484816545,-18.3954953171535,
16.2750584769984));
#178684=CARTESIAN_POINT('Ctrl Pts',(20.7745173849428,-18.3880898425376,
16.2745945271954));
#178685=CARTESIAN_POINT('Ctrl Pts',(20.7734196581763,-18.3841326541823,
16.2743470905249));
#178686=CARTESIAN_POINT('Ctrl Pts',(20.7703587304061,-18.3732216923779,
16.2736661061644));
#178687=CARTESIAN_POINT('Ctrl Pts',(20.7683714114672,-18.3662746617194,
16.2732339375138));
#178688=CARTESIAN_POINT('Ctrl Pts',(20.7573053281698,-18.3283270092134,
16.2708803157118));
#178689=CARTESIAN_POINT('Ctrl Pts',(20.7475529738977,-18.29752530341,16.268995754699));
#178690=CARTESIAN_POINT('Ctrl Pts',(20.6843927193559,-18.1128416537301,
16.2577860268716));
#178691=CARTESIAN_POINT('Ctrl Pts',(20.6140714909384,-17.9653077440627,
16.2491772491913));
#178692=CARTESIAN_POINT('Ctrl Pts',(20.4654113158115,-17.7282476763719,
16.2338590457182));
#178693=CARTESIAN_POINT('Ctrl Pts',(20.3952164074734,-17.6345366516259,
16.2273331984634));
#178694=CARTESIAN_POINT('Ctrl Pts',(20.3081688892259,-17.5364133593976,
16.219648855837));
#178695=CARTESIAN_POINT('Ctrl Pts',(20.2985772719514,-17.5258193753807,
16.2188072917872));
#178696=CARTESIAN_POINT('Ctrl Pts',(20.283141426536,-17.5091135431319,16.2174606388905));
#178697=CARTESIAN_POINT('Ctrl Pts',(20.2773664646587,-17.5029380829562,
16.2169584917476));
#178698=CARTESIAN_POINT('Ctrl Pts',(20.2671163414441,-17.4921078893121,
16.2160700600332));
#178699=CARTESIAN_POINT('Ctrl Pts',(20.262656562493,-17.4874386992094,16.2156844415814));
#178700=CARTESIAN_POINT('Ctrl Pts',(20.2533882317986,-17.4778236250631,
16.2148849289276));
#178701=CARTESIAN_POINT('Ctrl Pts',(20.2485767326516,-17.4728807003799,
16.2144709084111));
#178702=CARTESIAN_POINT('Ctrl Pts',(20.2361643841556,-17.4602533776872,
16.2134054316305));
#178703=CARTESIAN_POINT('Ctrl Pts',(20.2285287562794,-17.4526035840792,
16.2127524460503));
#178704=CARTESIAN_POINT('Ctrl Pts',(20.1964160069067,-17.4209202648625,
16.2100160989504));
#178705=CARTESIAN_POINT('Ctrl Pts',(20.1714162540278,-17.3974260940714,
16.2079093999838));
#178706=CARTESIAN_POINT('Ctrl Pts',(20.1047998787551,-17.3378027188554,
16.2023523939175));
#178707=CARTESIAN_POINT('Ctrl Pts',(20.0623259134757,-17.3026744963841,
16.1988636577931));
#178708=CARTESIAN_POINT('Ctrl Pts',(19.931579391767,-17.2028689848442,16.1882909511582));
#178709=CARTESIAN_POINT('Ctrl Pts',(19.8396177042695,-17.1433370314395,
16.1810586003525));
#178710=CARTESIAN_POINT('Ctrl Pts',(19.6394021637277,-17.0347219378359,
16.1660121017659));
#178711=CARTESIAN_POINT('Ctrl Pts',(19.5307614638837,-16.9870862760845,
16.1582260025326));
#178712=CARTESIAN_POINT('Ctrl Pts',(19.4096763404152,-16.9456995868945,
16.1503221520732));
#178713=CARTESIAN_POINT('Ctrl Pts',(19.400635464455,-16.9426774699008,16.1497365788605));
#178714=CARTESIAN_POINT('Ctrl Pts',(19.3872134494329,-16.9382914219884,
16.1488743208427));
#178715=CARTESIAN_POINT('Ctrl Pts',(19.3828479385061,-16.9368805491264,
16.1485949759355));
#178716=CARTESIAN_POINT('Ctrl Pts',(19.3750749336323,-16.934396299578,16.1480995950186));
#178717=CARTESIAN_POINT('Ctrl Pts',(19.3716692813514,-16.9333173476821,
16.147883234957));
#178718=CARTESIAN_POINT('Ctrl Pts',(19.3643440047434,-16.9310169990452,
16.1474193427833));
#178719=CARTESIAN_POINT('Ctrl Pts',(19.3604235654339,-16.9297983849795,
16.1471719744778));
#178720=CARTESIAN_POINT('Ctrl Pts',(19.3495984891982,-16.9264680618227,
16.1464913710623));
#178721=CARTESIAN_POINT('Ctrl Pts',(19.3426864810158,-16.9243802368974,
16.1460595124438));
#178722=CARTESIAN_POINT('Ctrl Pts',(19.3048667972504,-16.9131673341792,
16.143710706958));
#178723=CARTESIAN_POINT('Ctrl Pts',(19.2737627214024,-16.9047130149783,
16.1418304743107));
#178724=CARTESIAN_POINT('Ctrl Pts',(19.084302385453,-16.8578348231362,16.130620460864));
#178725=CARTESIAN_POINT('Ctrl Pts',(18.9221229484456,-16.8370859915432,
16.1220083890275));
#178726=CARTESIAN_POINT('Ctrl Pts',(18.6422407540804,-16.8337601729077,
16.1066856179914));
#178727=CARTESIAN_POINT('Ctrl Pts',(18.5254286060972,-16.842058667023,16.1001586842392));
#178728=CARTESIAN_POINT('Ctrl Pts',(18.3957845843667,-16.8621426916598,
16.0924731185701));
#178729=CARTESIAN_POINT('Ctrl Pts',(18.3816846916261,-16.8644734384523,
16.0916315388002));
#178730=CARTESIAN_POINT('Ctrl Pts',(18.3592822550857,-16.8684100451873,
16.0902848654482));
#178731=CARTESIAN_POINT('Ctrl Pts',(18.3509637154792,-16.8699232267453,
16.0897827137114));
#178732=CARTESIAN_POINT('Ctrl Pts',(18.3363089489912,-16.8726797939313,
16.0888942766458));
#178733=CARTESIAN_POINT('Ctrl Pts',(18.3299688924155,-16.8739024194961,
16.0885086574623));
#178734=CARTESIAN_POINT('Ctrl Pts',(18.3168673832569,-16.8764911556537,
16.0877091460186));
#178735=CARTESIAN_POINT('Ctrl Pts',(18.3101068235671,-16.8778613459722,
16.0872951274571));
#178736=CARTESIAN_POINT('Ctrl Pts',(18.2927708472212,-16.881463196703,16.0862296614504));
#178737=CARTESIAN_POINT('Ctrl Pts',(18.2822057020248,-16.8837428291913,
16.0855766847489));
#178738=CARTESIAN_POINT('Ctrl Pts',(18.2381843929082,-16.8935946634145,
16.0828404236966));
#178739=CARTESIAN_POINT('Ctrl Pts',(18.2048988366685,-16.9018982004212,
16.0807338037345));
#178740=CARTESIAN_POINT('Ctrl Pts',(18.1187106915936,-16.9256377596298,
16.0751770557398));
#178741=CARTESIAN_POINT('Ctrl Pts',(18.0661856584287,-16.9423363349094,
16.0716885031325));
#178742=CARTESIAN_POINT('Ctrl Pts',(17.8184620016038,-17.031876164015,16.0547573725747));
#178743=CARTESIAN_POINT('Ctrl Pts',(17.6341000533558,-17.1312055117576,
16.0405669002422));
#178744=CARTESIAN_POINT('Ctrl Pts',(17.4635919109797,-17.2585500366682,
16.027150434105));
#178745=CARTESIAN_POINT('Ctrl Pts',(17.4599737511049,-17.2612703915826,
16.0268656545933));
#178746=CARTESIAN_POINT('Ctrl Pts',(17.4399959236207,-17.2763914940188,
16.0252928906516));
#178747=CARTESIAN_POINT('Ctrl Pts',(17.4238078904053,-17.2890186040663,
16.0240172019346));
#178748=CARTESIAN_POINT('Ctrl Pts',(17.4027810234203,-17.3059178066909,
16.0223613078333));
#178749=CARTESIAN_POINT('Ctrl Pts',(17.3977750186683,-17.3099788818406,
16.0219671635049));
#178750=CARTESIAN_POINT('Ctrl Pts',(17.3897442068621,-17.316554851155,16.0213351100327));
#178751=CARTESIAN_POINT('Ctrl Pts',(17.3867077693656,-17.3190553842454,
16.0210961889251));
#178752=CARTESIAN_POINT('Ctrl Pts',(17.3810359129483,-17.3237527981171,
16.0206500373336));
#178753=CARTESIAN_POINT('Ctrl Pts',(17.3783988647879,-17.3259476227316,
16.0204426643857));
#178754=CARTESIAN_POINT('Ctrl Pts',(17.3721624817998,-17.3311639015387,
16.0199523607955));
#178755=CARTESIAN_POINT('Ctrl Pts',(17.3685678277111,-17.3341909667995,
16.0196698390166));
#178756=CARTESIAN_POINT('Ctrl Pts',(17.3573349023048,-17.3437143436269,
16.0187871603079));
#178757=CARTESIAN_POINT('Ctrl Pts',(17.3497325578077,-17.3502530783282,
16.0181900230108));
#178758=CARTESIAN_POINT('Ctrl Pts',(17.3319067038273,-17.365806707011,16.016789671789));
#178759=CARTESIAN_POINT('Ctrl Pts',(17.3217231164897,-17.3748669053311,
16.015989523897));
#178760=CARTESIAN_POINT('Ctrl Pts',(17.2863072542557,-17.4069940449287,
16.0132033315157));
#178761=CARTESIAN_POINT('Ctrl Pts',(17.2615457343291,-17.4305742299714,
16.0112489914483));
#178762=CARTESIAN_POINT('Ctrl Pts',(17.183673151494,-17.5084145709385,16.0050398775088));
#178763=CARTESIAN_POINT('Ctrl Pts',(17.1329038446143,-17.5649366684851,
16.0008918747454));
#178764=CARTESIAN_POINT('Ctrl Pts',(16.977365602455,-17.7580482698994,15.9874070852766));
#178765=CARTESIAN_POINT('Ctrl Pts',(16.8861986078455,-17.9046660899658,
15.9781418734426));
#178766=CARTESIAN_POINT('Ctrl Pts',(16.8039952049217,-18.0817643010186,
15.9667990944902));
#178767=CARTESIAN_POINT('Ctrl Pts',(16.7945621974466,-18.1029949187229,
15.9654383085152));
#178768=CARTESIAN_POINT('Ctrl Pts',(16.7817332916145,-18.1331986902603,
15.9634991581719));
#178769=CARTESIAN_POINT('Ctrl Pts',(16.7780458573277,-18.1420467466132,
15.9629307106105));
#178770=CARTESIAN_POINT('Ctrl Pts',(16.7721580878062,-18.1564492469223,
15.9620046758582));
#178771=CARTESIAN_POINT('Ctrl Pts',(16.7699209242609,-18.1619885619307,
15.9616483393663));
#178772=CARTESIAN_POINT('Ctrl Pts',(16.7652917993662,-18.1735916806907,
15.9609015251491));
#178773=CARTESIAN_POINT('Ctrl Pts',(16.7629043418377,-18.1796572032372,
15.9605109002237));
#178774=CARTESIAN_POINT('Ctrl Pts',(16.7572996251138,-18.1940916825968,
15.959580720751));
#178775=CARTESIAN_POINT('Ctrl Pts',(16.7541074642866,-18.2024701921705,
15.9590403305058));
#178776=CARTESIAN_POINT('Ctrl Pts',(16.74909993319,-18.2158687493782,15.9581753499659));
#178777=CARTESIAN_POINT('Ctrl Pts',(16.7472501565826,-18.2208758306612,
15.9578519244208));
#178778=CARTESIAN_POINT('Ctrl Pts',(16.7454193691904,-18.2258897640378,
15.9575278689401));
#178779=CARTESIAN_POINT('Ctrl Pts',(16.7454193749215,-18.2258897483422,
15.7328935260819));
#178780=CARTESIAN_POINT('Ctrl Pts',(16.7986491770761,-18.0801105736236,
15.7430556214707));
#178781=CARTESIAN_POINT('Ctrl Pts',(16.8677533973363,-17.9406091845295,
15.7534873781281));
#178782=CARTESIAN_POINT('Ctrl Pts',(16.969167748649,-17.782329829287,15.7654348139467));
#178783=CARTESIAN_POINT('Ctrl Pts',(16.9874713599678,-17.7551712038437,
15.7674874144511));
#178784=CARTESIAN_POINT('Ctrl Pts',(17.0105923652516,-17.7225254090454,
15.7699474626286));
#178785=CARTESIAN_POINT('Ctrl Pts',(17.0148163996346,-17.7166258068677,
15.7703917328071));
#178786=CARTESIAN_POINT('Ctrl Pts',(17.0214824326368,-17.7074159329509,
15.7710846623438));
#178787=CARTESIAN_POINT('Ctrl Pts',(17.0239038427826,-17.7040909279055,
15.7713347001544));
#178788=CARTESIAN_POINT('Ctrl Pts',(17.0284457747782,-17.6978921339815,
15.7718005722054));
#178789=CARTESIAN_POINT('Ctrl Pts',(17.0305638546939,-17.695016685123,15.772016563221));
#178790=CARTESIAN_POINT('Ctrl Pts',(17.0354125014323,-17.6884690546978,
15.772508148056));
#178791=CARTESIAN_POINT('Ctrl Pts',(17.0381476990232,-17.6848003652934,
15.7727834144827));
#178792=CARTESIAN_POINT('Ctrl Pts',(17.0465812188346,-17.6735647907638,
15.7736260010112));
#178793=CARTESIAN_POINT('Ctrl Pts',(17.0523185392419,-17.6660271389598,
15.7741906645266));
#178794=CARTESIAN_POINT('Ctrl Pts',(17.1322503964098,-17.5624630114758,
15.7819443981977));
#178795=CARTESIAN_POINT('Ctrl Pts',(17.2145286866137,-17.472935972836,15.7886001887928));
#178796=CARTESIAN_POINT('Ctrl Pts',(17.3839443253859,-17.3177474013176,
15.8011019253958));
#178797=CARTESIAN_POINT('Ctrl Pts',(17.4693525423884,-17.2507952223934,
15.8069418417311));
#178798=CARTESIAN_POINT('Ctrl Pts',(17.6043744854454,-17.1607592486249,
15.815974350041));
#178799=CARTESIAN_POINT('Ctrl Pts',(17.6503661690858,-17.1325675768534,
15.819017893463));
#178800=CARTESIAN_POINT('Ctrl Pts',(17.7169507811347,-17.0951737790149,
15.8234134095805));
#178801=CARTESIAN_POINT('Ctrl Pts',(17.7366928450442,-17.084496020637,15.8247152664774));
#178802=CARTESIAN_POINT('Ctrl Pts',(17.7717696322091,-17.066239103077,15.827028240413));
#178803=CARTESIAN_POINT('Ctrl Pts',(17.787033602579,-17.0585280414747,15.8280347113196));
#178804=CARTESIAN_POINT('Ctrl Pts',(17.8097464193935,-17.047397298406,15.8295329891039));
#178805=CARTESIAN_POINT('Ctrl Pts',(17.8171246364199,-17.0438344681445,
15.8300198003622));
#178806=CARTESIAN_POINT('Ctrl Pts',(17.8300552996081,-17.037682756556,15.8308732092417));
#178807=CARTESIAN_POINT('Ctrl Pts',(17.8355986797496,-17.0350749632634,
15.8312391455504));
#178808=CARTESIAN_POINT('Ctrl Pts',(17.8466659908122,-17.0299270769396,
15.8319699261856));
#178809=CARTESIAN_POINT('Ctrl Pts',(17.8521897007478,-17.0273866465295,
15.8323347544759));
#178810=CARTESIAN_POINT('Ctrl Pts',(17.8654310342758,-17.0213657449341,
15.8332095758929));
#178811=CARTESIAN_POINT('Ctrl Pts',(17.8731586980037,-17.0179077259414,
15.833720335174));
#178812=CARTESIAN_POINT('Ctrl Pts',(17.9011813969711,-17.0055691831373,
15.8355733863613));
#178813=CARTESIAN_POINT('Ctrl Pts',(17.9215942224466,-16.9969612422103,
15.8369249270421));
#178814=CARTESIAN_POINT('Ctrl Pts',(18.1138494702251,-16.919419468248,15.8496742686148));
#178815=CARTESIAN_POINT('Ctrl Pts',(18.2938744716083,-16.8730020674608,
15.8618670521711));
#178816=CARTESIAN_POINT('Ctrl Pts',(18.5574429208237,-16.8408420172486,
15.8793982076665));
#178817=CARTESIAN_POINT('Ctrl Pts',(18.6377919029663,-16.8356573626097,
15.8846844324742));
#178818=CARTESIAN_POINT('Ctrl Pts',(18.7543545483081,-16.8347898969838,
15.8921155935479));
#178819=CARTESIAN_POINT('Ctrl Pts',(18.7904670296205,-16.8354450720657,
15.8943844030806));
#178820=CARTESIAN_POINT('Ctrl Pts',(18.8340114125223,-16.8373504935855,
15.8970659420626));
#178821=CARTESIAN_POINT('Ctrl Pts',(18.8414737359984,-16.8377166184473,
15.897523558883));
#178822=CARTESIAN_POINT('Ctrl Pts',(18.8530883143883,-16.8383481171297,
15.8982326436105));
#178823=CARTESIAN_POINT('Ctrl Pts',(18.8572419037747,-16.8385862349207,
15.8984855952612));
#178824=CARTESIAN_POINT('Ctrl Pts',(18.8649540831465,-16.839051173689,15.8989540587022));
#178825=CARTESIAN_POINT('Ctrl Pts',(18.8685127684244,-16.8392747386586,
15.8991697446558));
#178826=CARTESIAN_POINT('Ctrl Pts',(18.8765702921974,-16.8398013724336,
15.8996570230034));
#178827=CARTESIAN_POINT('Ctrl Pts',(18.8810687257854,-16.8401098226303,
15.8999283105961));
#178828=CARTESIAN_POINT('Ctrl Pts',(18.892678665158,-16.8409431724365,15.9006266019916));
#178829=CARTESIAN_POINT('Ctrl Pts',(18.8997886321025,-16.8414896397551,
15.901052425327));
#178830=CARTESIAN_POINT('Ctrl Pts',(18.9433826825752,-16.8450619081063,
15.9036529345329));
#178831=CARTESIAN_POINT('Ctrl Pts',(18.9797883547807,-16.8489979368472,
15.9057800223777));
#178832=CARTESIAN_POINT('Ctrl Pts',(19.185121235868,-16.876603307102,15.917615682844));
#178833=CARTESIAN_POINT('Ctrl Pts',(19.3508153104973,-16.9196779860824,
15.9265900374109));
#178834=CARTESIAN_POINT('Ctrl Pts',(19.5983240232338,-17.0171268399761,
15.9412221850858));
#178835=CARTESIAN_POINT('Ctrl Pts',(19.6846181101444,-17.0580326567271,
15.9465711712111));
#178836=CARTESIAN_POINT('Ctrl Pts',(19.7865220539972,-17.1150612543843,
15.9533710312598));
#178837=CARTESIAN_POINT('Ctrl Pts',(19.8050299233889,-17.1257904054752,
15.9546262694712));
#178838=CARTESIAN_POINT('Ctrl Pts',(19.8310970183237,-17.1414342566027,
15.9564245901129));
#178839=CARTESIAN_POINT('Ctrl Pts',(19.8387927267763,-17.1461198251769,
15.9569593294526));
#178840=CARTESIAN_POINT('Ctrl Pts',(19.8520109046996,-17.1542838902018,
15.9578845281662));
#178841=CARTESIAN_POINT('Ctrl Pts',(19.8575476708812,-17.1577390869102,
15.9582741262711));
#178842=CARTESIAN_POINT('Ctrl Pts',(19.8681139866999,-17.1644010393384,
15.9590216164507));
#178843=CARTESIAN_POINT('Ctrl Pts',(19.8731461410982,-17.167603562244,15.9593793489408));
#178844=CARTESIAN_POINT('Ctrl Pts',(19.8861869817092,-17.1759805538481,
15.9603109947769));
#178845=CARTESIAN_POINT('Ctrl Pts',(19.8941742976707,-17.1811878958225,
15.9608861314053));
#178846=CARTESIAN_POINT('Ctrl Pts',(19.9212431739136,-17.1990972391178,
15.9628508781781));
#178847=CARTESIAN_POINT('Ctrl Pts',(19.9401529739022,-17.2120547761967,
15.9642500715595));
#178848=CARTESIAN_POINT('Ctrl Pts',(20.1027579186037,-17.3274009560412,
15.9765203133115));
#178849=CARTESIAN_POINT('Ctrl Pts',(20.2333152106197,-17.4470580130278,
15.9881037093106));
#178850=CARTESIAN_POINT('Ctrl Pts',(20.4033972526729,-17.6472939897339,
16.005461150955));
#178851=CARTESIAN_POINT('Ctrl Pts',(20.4552225885771,-17.7164678633397,
16.0111503512296));
#178852=CARTESIAN_POINT('Ctrl Pts',(20.523373185568,-17.8200766578057,16.0190669076583));
#178853=CARTESIAN_POINT('Ctrl Pts',(20.5432243806693,-17.8520843690389,
16.0214352013854));
#178854=CARTESIAN_POINT('Ctrl Pts',(20.5660252556376,-17.8911373096204,
16.0242179034205));
#178855=CARTESIAN_POINT('Ctrl Pts',(20.5698031132852,-17.8976883201116,
16.0246811579534));
#178856=CARTESIAN_POINT('Ctrl Pts',(20.5756146825765,-17.9078918472713,
16.0253970579462));
#178857=CARTESIAN_POINT('Ctrl Pts',(20.5776727713038,-17.9115303047537,
16.025651232608));
#178858=CARTESIAN_POINT('Ctrl Pts',(20.5814655527914,-17.9182820826468,
16.0261208154473));
#178859=CARTESIAN_POINT('Ctrl Pts',(20.583203145719,-17.9213936602332,16.0263364050088));
#178860=CARTESIAN_POINT('Ctrl Pts',(20.5871085834648,-17.9284289608655,
16.0268220199729));
#178861=CARTESIAN_POINT('Ctrl Pts',(20.5892718222449,-17.9323551791434,
16.0270917494463));
#178862=CARTESIAN_POINT('Ctrl Pts',(20.5956052439299,-17.9439370486092,
16.0278837453882));
#178863=CARTESIAN_POINT('Ctrl Pts',(20.59974068688,-17.951611728663,16.0284038488457));
#178864=CARTESIAN_POINT('Ctrl Pts',(20.6288254360826,-18.00639580176,16.0320846675931));
#178865=CARTESIAN_POINT('Ctrl Pts',(20.6520371413981,-18.0544114111279,
16.03514414567));
#178866=CARTESIAN_POINT('Ctrl Pts',(20.6801852874549,-18.1187310408185,
16.039092696787));
#178867=CARTESIAN_POINT('Ctrl Pts',(20.6867721725102,-18.134286605865,16.0400364071153));
#178868=CARTESIAN_POINT('Ctrl Pts',(20.7495007617665,-18.2875082992728,
16.0492372743885));
#178869=CARTESIAN_POINT('Ctrl Pts',(20.7911801703704,-18.4306500657084,
16.0571187250839));
#178870=CARTESIAN_POINT('Ctrl Pts',(20.8284373449654,-18.6376433294357,
16.0687552454186));
#178871=CARTESIAN_POINT('Ctrl Pts',(20.8367007241814,-18.698747715629,16.0722142940749));
#178872=CARTESIAN_POINT('Ctrl Pts',(20.8456567395971,-18.7971534085797,
16.0778852771615));
#178873=CARTESIAN_POINT('Ctrl Pts',(20.8480505818683,-18.8342649508023,
16.0800463668223));
#178874=CARTESIAN_POINT('Ctrl Pts',(20.8498893595605,-18.8825375860425,
16.0828940127973));
#178875=CARTESIAN_POINT('Ctrl Pts',(20.8502252205033,-18.8936594668152,
16.0835526097752));
#178876=CARTESIAN_POINT('Ctrl Pts',(20.8506288006009,-18.911749822692,16.0846281253856));
#178877=CARTESIAN_POINT('Ctrl Pts',(20.8507498188059,-18.918716984696,16.0850433696457));
#178878=CARTESIAN_POINT('Ctrl Pts',(20.8509163824109,-18.9321155,16.0858439534821));
#178879=CARTESIAN_POINT('Ctrl Pts',(20.8509670217873,-18.9385467212361,
16.0862291288333));
#178880=CARTESIAN_POINT('Ctrl Pts',(20.8510158621944,-18.9532711374946,
16.0871130964528));
#178881=CARTESIAN_POINT('Ctrl Pts',(20.8509946383011,-18.9615642522578,
16.0876124921698));
#178882=CARTESIAN_POINT('Ctrl Pts',(20.8508088196149,-18.9835928991429,
16.0889431612529));
#178883=CARTESIAN_POINT('Ctrl Pts',(20.8505592658744,-18.9973271459202,
16.08977708036));
#178884=CARTESIAN_POINT('Ctrl Pts',(20.8476429745416,-19.1018246375468,
16.0961555521935));
#178885=CARTESIAN_POINT('Ctrl Pts',(20.8392732291846,-19.1923224709446,
16.1018785383048));
#178886=CARTESIAN_POINT('Ctrl Pts',(20.8032181634376,-19.4207978880447,
16.1168162314853));
#178887=CARTESIAN_POINT('Ctrl Pts',(20.7675482784219,-19.5570716755587,
16.1262081025575));
#178888=CARTESIAN_POINT('Ctrl Pts',(20.6997977488651,-19.739566946158,16.13894990623));
#178889=CARTESIAN_POINT('Ctrl Pts',(20.6790045776565,-19.7896040096614,
16.1424575174684));
#178890=CARTESIAN_POINT('Ctrl Pts',(20.6445449312534,-19.8643027986768,
16.1476622344254));
#178891=CARTESIAN_POINT('Ctrl Pts',(20.6322688247292,-19.8895787848243,
16.1494175510262));
#178892=CARTESIAN_POINT('Ctrl Pts',(20.6163493386294,-19.9207609362137,
16.1515689305592));
#178893=CARTESIAN_POINT('Ctrl Pts',(20.6131759743504,-19.9269022744061,
16.1519919527315));
#178894=CARTESIAN_POINT('Ctrl Pts',(20.6081015785714,-19.9366057961958,
16.1526591092862));
#178895=CARTESIAN_POINT('Ctrl Pts',(20.6062203725,-19.9401782117273,16.1529044612158));
#178896=CARTESIAN_POINT('Ctrl Pts',(20.6026495583884,-19.9469123976665,
16.1533664272689));
#178897=CARTESIAN_POINT('Ctrl Pts',(20.6009621605159,-19.9500752188442,
16.1535831695517));
#178898=CARTESIAN_POINT('Ctrl Pts',(20.5970812099536,-19.957305306156,16.1540781339038));
#178899=CARTESIAN_POINT('Ctrl Pts',(20.5948823710689,-19.9613696822472,
16.1543560161919));
#178900=CARTESIAN_POINT('Ctrl Pts',(20.5889996413363,-19.9721588717554,
16.1550928017429));
#178901=CARTESIAN_POINT('Ctrl Pts',(20.5852924546031,-19.9788709970271,
16.1555502615088));
#178902=CARTESIAN_POINT('Ctrl Pts',(20.5587909112841,-20.0262439172689,
16.158773553888));
#178903=CARTESIAN_POINT('Ctrl Pts',(20.5346936962701,-20.0661655092835,
16.1614617893916));
#178904=CARTESIAN_POINT('Ctrl Pts',(20.5068125481072,-20.1090848941097,
16.1643570633199));
#178905=CARTESIAN_POINT('Ctrl Pts',(20.5043167135478,-20.1128998738619,
16.1646144609876));
#178906=CARTESIAN_POINT('Ctrl Pts',(20.4889698185111,-20.1361936099222,
16.1661865588864));
#178907=CARTESIAN_POINT('Ctrl Pts',(20.4758094094793,-20.1554673266876,
16.167489344523));
#178908=CARTESIAN_POINT('Ctrl Pts',(20.436056947628,-20.2116672095203,16.1713059271141));
#178909=CARTESIAN_POINT('Ctrl Pts',(20.4085896483035,-20.2479587472541,
16.1737939101594));
#178910=CARTESIAN_POINT('Ctrl Pts',(20.3112066886066,-20.3683562640255,
16.1822246657831));
#178911=CARTESIAN_POINT('Ctrl Pts',(20.2359567760231,-20.4479181008005,
16.1881126735045));
#178912=CARTESIAN_POINT('Ctrl Pts',(20.1140502965276,-20.5582960729378,
16.1972568180917));
#178913=CARTESIAN_POINT('Ctrl Pts',(20.0717731692527,-20.593672378155,16.2003642246821));
#178914=CARTESIAN_POINT('Ctrl Pts',(20.0010165044206,-20.6483298996806,
16.2055080701845));
#178915=CARTESIAN_POINT('Ctrl Pts',(19.9733622000711,-20.6686383112002,
16.2075051247608));
#178916=CARTESIAN_POINT('Ctrl Pts',(19.9363628901784,-20.6944492275682,
16.2101657063372));
#178917=CARTESIAN_POINT('Ctrl Pts',(19.9274509035291,-20.7005653446864,
16.2108057064886));
#178918=CARTESIAN_POINT('Ctrl Pts',(19.9127752657263,-20.7104724784298,
16.2118584056923));
#178919=CARTESIAN_POINT('Ctrl Pts',(19.9070391598751,-20.7143040918499,
16.2122695635035));
#178920=CARTESIAN_POINT('Ctrl Pts',(19.8958978603225,-20.7216677803985,
16.213067631105));
#178921=CARTESIAN_POINT('Ctrl Pts',(19.8904950265313,-20.7252032999569,
16.2134544055281));
#178922=CARTESIAN_POINT('Ctrl Pts',(19.8779803863855,-20.733311134783,16.2143497891331));
#178923=CARTESIAN_POINT('Ctrl Pts',(19.8708572297515,-20.7378656498345,
16.2148590544676));
#178924=CARTESIAN_POINT('Ctrl Pts',(19.8516216643262,-20.7500030656846,
16.2162333841592));
#178925=CARTESIAN_POINT('Ctrl Pts',(19.8394596045894,-20.7575060940593,
16.2171013767246));
#178926=CARTESIAN_POINT('Ctrl Pts',(19.727145564418,-20.825234739053,16.2251096917076));
#178927=CARTESIAN_POINT('Ctrl Pts',(19.6222596816702,-20.8771839983641,
16.2325518830783));
#178928=CARTESIAN_POINT('Ctrl Pts',(19.3623085969813,-20.9801547196364,
16.2508154736745));
#178929=CARTESIAN_POINT('Ctrl Pts',(19.2045739197855,-21.0224452483299,
16.2617770490455));
#178930=CARTESIAN_POINT('Ctrl Pts',(19.011448730543,-21.0509912763467,16.274181337372));
#178931=CARTESIAN_POINT('Ctrl Pts',(18.979237897354,-21.0549980545058,16.2762152488124));
#178932=CARTESIAN_POINT('Ctrl Pts',(18.939746573596,-21.0589906750871,16.2786560395557));
#178933=CARTESIAN_POINT('Ctrl Pts',(18.9325436234497,-21.0596816150739,
16.2790990792166));
#178934=CARTESIAN_POINT('Ctrl Pts',(18.9212451285424,-21.0607069840108,
16.2797905178954));
#178935=CARTESIAN_POINT('Ctrl Pts',(18.9171519907479,-21.0610664360155,
16.2800402858223));
#178936=CARTESIAN_POINT('Ctrl Pts',(18.9094985884157,-21.0617160957521,
16.2805059236637));
#178937=CARTESIAN_POINT('Ctrl Pts',(18.9059386752022,-21.0620092064753,
16.2807219487286));
#178938=CARTESIAN_POINT('Ctrl Pts',(18.897809885945,-21.0626577935262,16.2812139588645));
#178939=CARTESIAN_POINT('Ctrl Pts',(18.8932405956802,-21.0630074452023,
16.2814896143374));
#178940=CARTESIAN_POINT('Ctrl Pts',(18.8791897186696,-21.0640367673506,
16.2823345769834));
#178941=CARTESIAN_POINT('Ctrl Pts',(18.8697045101551,-21.0646674264054,
16.2829012057517));
#178942=CARTESIAN_POINT('Ctrl Pts',(18.7843093456043,-21.0697677441233,
16.2879711841856));
#178943=CARTESIAN_POINT('Ctrl Pts',(18.7082054014633,-21.070208796356,16.2922673244558));
#178944=CARTESIAN_POINT('Ctrl Pts',(18.5898140850792,-21.0645110947877,
16.2988269208558));
#178945=CARTESIAN_POINT('Ctrl Pts',(18.547463081989,-21.0611934155097,16.3011484938636));
#178946=CARTESIAN_POINT('Ctrl Pts',(18.3965607709308,-21.0447910546901,
16.3094124856806));
#178947=CARTESIAN_POINT('Ctrl Pts',(18.2889612781282,-21.0245779311487,
16.3152990669983));
#178948=CARTESIAN_POINT('Ctrl Pts',(18.1302306184801,-20.9818237747983,
16.3244398954967));
#178949=CARTESIAN_POINT('Ctrl Pts',(18.0776353880004,-20.9654316165808,
16.327545401422));
#178950=CARTESIAN_POINT('Ctrl Pts',(17.9934267495775,-20.9355362666617,
16.3326863811211));
#178951=CARTESIAN_POINT('Ctrl Pts',(17.9613968965364,-20.9232810831048,
16.3346825280834));
#178952=CARTESIAN_POINT('Ctrl Pts',(17.9196834611983,-20.9061479896563,
16.3373420718212));
#178953=CARTESIAN_POINT('Ctrl Pts',(17.9097185865706,-20.9019656242518,
16.3379819651689));
#178954=CARTESIAN_POINT('Ctrl Pts',(17.8934466770621,-20.8949891122312,
16.3390345334454));
#178955=CARTESIAN_POINT('Ctrl Pts',(17.8871204257654,-20.89224007895,16.3394456678857));
#178956=CARTESIAN_POINT('Ctrl Pts',(17.8748983853308,-20.8868579039729,
16.3402437221114));
#178957=CARTESIAN_POINT('Ctrl Pts',(17.8690009795193,-20.8842286060475,
16.340630506699));
#178958=CARTESIAN_POINT('Ctrl Pts',(17.855408603304,-20.8780938859998,16.341525960443));
#178959=CARTESIAN_POINT('Ctrl Pts',(17.8477224607239,-20.8745692757786,
16.3420352860753));
#178960=CARTESIAN_POINT('Ctrl Pts',(17.827101021306,-20.8649630285519,16.3434098840022));
#178961=CARTESIAN_POINT('Ctrl Pts',(17.8142060342502,-20.8587963580319,
16.3442780862837));
#178962=CARTESIAN_POINT('Ctrl Pts',(17.6962262732674,-20.8009005808381,
16.3523026058879));
#178963=CARTESIAN_POINT('Ctrl Pts',(17.5955586507501,-20.7406729997485,
16.3597622111443));
#178964=CARTESIAN_POINT('Ctrl Pts',(17.3674340186021,-20.5771018086952,
16.3780996966685));
#178965=CARTESIAN_POINT('Ctrl Pts',(17.2459722416748,-20.4666722654724,
16.3891199719299));
#178966=CARTESIAN_POINT('Ctrl Pts',(17.1177574528905,-20.3196400550649,
16.4015037911325));
#178967=CARTESIAN_POINT('Ctrl Pts',(17.0976052224759,-20.2954625668438,
16.403474683421));
#178968=CARTESIAN_POINT('Ctrl Pts',(17.0735333296601,-20.2652367671559,
16.4058503994211));
#178969=CARTESIAN_POINT('Ctrl Pts',(17.0690967018619,-20.2596075027145,
16.4062891921075));
#178970=CARTESIAN_POINT('Ctrl Pts',(17.0621710199215,-20.2507276928364,
16.406975483563));
#178971=CARTESIAN_POINT('Ctrl Pts',(17.0596627075544,-20.2474923351964,
16.4072243185171));
#178972=CARTESIAN_POINT('Ctrl Pts',(17.0549819727073,-20.2414185664612,
16.4076891548603));
#178973=CARTESIAN_POINT('Ctrl Pts',(17.0528073784729,-20.2385819620404,
16.4079053057623));
#178974=CARTESIAN_POINT('Ctrl Pts',(17.0478470215855,-20.2320774766881,
16.4083988232835));
#178975=CARTESIAN_POINT('Ctrl Pts',(17.0450660427117,-20.2284060097705,
16.4086758525205));
#178976=CARTESIAN_POINT('Ctrl Pts',(17.0378179745889,-20.2187718987769,
16.4093988612888));
#178977=CARTESIAN_POINT('Ctrl Pts',(17.0333702961248,-20.2127946386531,
16.409843516853));
#178978=CARTESIAN_POINT('Ctrl Pts',(17.0039151561351,-20.1727702473765,
16.4127958625758));
#178979=CARTESIAN_POINT('Ctrl Pts',(16.9798982063689,-20.1380021079905,
16.4152399444127));
#178980=CARTESIAN_POINT('Ctrl Pts',(16.9164802357213,-20.0400496880174,
16.4218683513697));
#178981=CARTESIAN_POINT('Ctrl Pts',(16.8793454306222,-19.9754686764816,
16.4259561035331));
#178982=CARTESIAN_POINT('Ctrl Pts',(16.7951472797133,-19.8093431575168,
16.4361043561752));
#178983=CARTESIAN_POINT('Ctrl Pts',(16.7525863070628,-19.7057812498675,
16.4421169529417));
#178984=CARTESIAN_POINT('Ctrl Pts',(16.6925866262591,-19.518963755382,16.4530200327051));
#178985=CARTESIAN_POINT('Ctrl Pts',(16.6716050219941,-19.4371195556745,
16.457812439815));
#178986=CARTESIAN_POINT('Ctrl Pts',(16.6528673353179,-19.3403009414751,
16.4636013834646));
#178987=CARTESIAN_POINT('Ctrl Pts',(16.650308712979,-19.3263279241678,16.4644395951184));
#178988=CARTESIAN_POINT('Ctrl Pts',(16.6465902583539,-19.30480018066,16.4657356113839));
#178989=CARTESIAN_POINT('Ctrl Pts',(16.6453303598907,-19.2972629854671,
16.4661902323967));
#178990=CARTESIAN_POINT('Ctrl Pts',(16.6431068637625,-19.2835034500645,
16.4670218085244));
#178991=CARTESIAN_POINT('Ctrl Pts',(16.6421301613061,-19.2772832937722,
16.4673983427374));
#178992=CARTESIAN_POINT('Ctrl Pts',(16.6400580229959,-19.2636914158526,
16.4682224921851));
#178993=CARTESIAN_POINT('Ctrl Pts',(16.6389737394915,-19.2563181022256,
16.4686704557581));
#178994=CARTESIAN_POINT('Ctrl Pts',(16.6361094461845,-19.2360992763592,
16.4699013252763));
#178995=CARTESIAN_POINT('Ctrl Pts',(16.6344085230222,-19.2232430509384,
16.4706867196878));
#178996=CARTESIAN_POINT('Ctrl Pts',(16.6263685201593,-19.1578589105123,
16.4746955627278));
#178997=CARTESIAN_POINT('Ctrl Pts',(16.6218825847585,-19.105126054127,16.4779768409725));
#178998=CARTESIAN_POINT('Ctrl Pts',(16.617766361128,-19.0183299141281,16.4834601044147));
#178999=CARTESIAN_POINT('Ctrl Pts',(16.6169742106524,-18.9843434164516,
16.4856276621907));
#179000=CARTESIAN_POINT('Ctrl Pts',(16.6171022081763,-18.8197312259874,
16.4962188776041));
#179001=CARTESIAN_POINT('Ctrl Pts',(16.6292932871456,-18.6894054728747,
16.5049104190834));
#179002=CARTESIAN_POINT('Ctrl Pts',(16.6709615320031,-18.4676530475529,
16.5197603279542));
#179003=CARTESIAN_POINT('Ctrl Pts',(16.6947819253757,-18.375533519513,16.5259401150738));
#179004=CARTESIAN_POINT('Ctrl Pts',(16.7277657538437,-18.276125045736,16.5324111806187));
#179005=CARTESIAN_POINT('Ctrl Pts',(16.7308789356263,-18.2669534220978,
16.5330062673888));
#179006=CARTESIAN_POINT('Ctrl Pts',(16.7355692054842,-18.253440996125,16.5338797814061));
#179007=CARTESIAN_POINT('Ctrl Pts',(16.7370976771306,-18.2490836207518,
16.5341609683186));
#179008=CARTESIAN_POINT('Ctrl Pts',(16.7398349366889,-18.241361213979,16.5346583782767));
#179009=CARTESIAN_POINT('Ctrl Pts',(16.7410380033782,-18.2379942124689,
16.5348749355805));
#179010=CARTESIAN_POINT('Ctrl Pts',(16.7432997980327,-18.2317144243437,
16.5352782381891));
#179011=CARTESIAN_POINT('Ctrl Pts',(16.7443563829228,-18.2288009389497,
16.5354651111096));
#179012=CARTESIAN_POINT('Ctrl Pts',(16.7454193692319,-18.2258897639242,
16.5356516076535));
#179013=CARTESIAN_POINT('Origin',(18.734,-18.952,0.));
#179014=CARTESIAN_POINT('',(16.7454193574352,-18.2258897962317,17.5536949220328));
#179015=CARTESIAN_POINT('',(16.7454193703768,-18.2258897607889,17.3329785739071));
#179016=CARTESIAN_POINT('',(16.7454193692319,-18.2258897639242,0.));
#179017=CARTESIAN_POINT('',(16.6170009798014,-18.9502127592998,17.5117108725788));
#179018=CARTESIAN_POINT('Ctrl Pts',(16.7454193574352,-18.2258897962317,
17.5536949220328));
#179019=CARTESIAN_POINT('Ctrl Pts',(16.7413714151833,-18.2369757988282,
17.5529503472539));
#179020=CARTESIAN_POINT('Ctrl Pts',(16.7374153734205,-18.2480978513274,
17.5522096669621));
#179021=CARTESIAN_POINT('Ctrl Pts',(16.7284957195804,-18.2738552394198,
17.5505098130367));
#179022=CARTESIAN_POINT('Ctrl Pts',(16.7235995003856,-18.2885110414992,
17.5495540496509));
#179023=CARTESIAN_POINT('Ctrl Pts',(16.7171006505231,-18.3086967106174,
17.5482545722139));
#179024=CARTESIAN_POINT('Ctrl Pts',(16.7153595931654,-18.3141810462808,
17.5479032140515));
#179025=CARTESIAN_POINT('Ctrl Pts',(16.7126241636862,-18.322921057949,17.5473460619894));
#179026=CARTESIAN_POINT('Ctrl Pts',(16.7116152609576,-18.3261721046219,
17.547139427821));
#179027=CARTESIAN_POINT('Ctrl Pts',(16.7095441547532,-18.3329032629761,
17.5467128847844));
#179028=CARTESIAN_POINT('Ctrl Pts',(16.7084830809009,-18.336383683007,17.5464930479701));
#179029=CARTESIAN_POINT('Ctrl Pts',(16.7059703217907,-18.3447025915504,
17.5459692588079));
#179030=CARTESIAN_POINT('Ctrl Pts',(16.7045269600696,-18.3495436120295,
17.545665792097));
#179031=CARTESIAN_POINT('Ctrl Pts',(16.6996912337203,-18.3659771875174,
17.5446400284771));
#179032=CARTESIAN_POINT('Ctrl Pts',(16.6963806855563,-18.3775938388039,
17.5439223413945));
#179033=CARTESIAN_POINT('Ctrl Pts',(16.6886497495818,-18.4056297446831,
17.5422066455205));
#179034=CARTESIAN_POINT('Ctrl Pts',(16.6843273312696,-18.4220753909503,
17.541213684684));
#179035=CARTESIAN_POINT('Ctrl Pts',(16.668771959161,-18.4842994252448,17.5375011482999));
#179036=CARTESIAN_POINT('Ctrl Pts',(16.6588701449653,-18.5303990672132,
17.5348407975409));
#179037=CARTESIAN_POINT('Ctrl Pts',(16.6283221116876,-18.7000293569035,
17.525255197217));
#179038=CARTESIAN_POINT('Ctrl Pts',(16.6171065838711,-18.8249907791413,
17.5185706197638));
#179039=CARTESIAN_POINT('Ctrl Pts',(16.6170007560361,-18.95021085035,17.5117113679171));
#179040=CARTESIAN_POINT('Ctrl Pts',(16.6170007544058,-18.9502127804554,
17.5117112621906));
#179041=CARTESIAN_POINT('Ctrl Pts',(16.6169304738018,-19.0334616382956,
17.5071510906457));
#179042=CARTESIAN_POINT('Ctrl Pts',(16.6217706589722,-19.1166375130435,
17.5025270065186));
#179043=CARTESIAN_POINT('Ctrl Pts',(16.6354867191127,-19.233244553671,17.4958023784479));
#179044=CARTESIAN_POINT('Ctrl Pts',(16.640299115908,-19.2670760339661,17.4938228290134));
#179045=CARTESIAN_POINT('Ctrl Pts',(16.6476157596072,-19.3108798684298,
17.491216464112));
#179046=CARTESIAN_POINT('Ctrl Pts',(16.6493769145509,-19.3209722816618,
17.4906129592889));
#179047=CARTESIAN_POINT('Ctrl Pts',(16.6524780889849,-19.3380124286009,
17.4895887495204));
#179048=CARTESIAN_POINT('Ctrl Pts',(16.6537798228097,-19.3449670134176,
17.4891692578465));
#179049=CARTESIAN_POINT('Ctrl Pts',(16.6564245658922,-19.358715221747,17.4883369899524));
#179050=CARTESIAN_POINT('Ctrl Pts',(16.6577660954574,-19.3655090420839,
17.4879242654479));
#179051=CARTESIAN_POINT('Ctrl Pts',(16.6604207587197,-19.3786142129694,
17.4871252735954));
#179052=CARTESIAN_POINT('Ctrl Pts',(16.6617294358375,-19.3849263956566,
17.4867391528484));
#179053=CARTESIAN_POINT('Ctrl Pts',(16.6648077221552,-19.3994401798843,
17.4858483391349));
#179054=CARTESIAN_POINT('Ctrl Pts',(16.6665972917148,-19.4076373951692,
17.4853430110984));
#179055=CARTESIAN_POINT('Ctrl Pts',(16.6715178229252,-19.429550193613,17.4839861569912));
#179056=CARTESIAN_POINT('Ctrl Pts',(16.6747368134473,-19.4432453884597,
17.4831318174468));
#179057=CARTESIAN_POINT('Ctrl Pts',(16.7030023345249,-19.5583384343218,
17.4758975009352));
#179058=CARTESIAN_POINT('Ctrl Pts',(16.7353809208197,-19.6577718654768,
17.4692788495735));
#179059=CARTESIAN_POINT('Ctrl Pts',(16.8068986778427,-19.8323811165516,
17.4570149658523));
#179060=CARTESIAN_POINT('Ctrl Pts',(16.8434657138016,-19.9083834675659,
17.45144184036));
#179061=CARTESIAN_POINT('Ctrl Pts',(16.9296233906247,-20.0630939097261,
17.4397430179211));
#179062=CARTESIAN_POINT('Ctrl Pts',(16.9800719491005,-20.1411356371382,
17.4336307215776));
#179063=CARTESIAN_POINT('Ctrl Pts',(17.0539803422169,-20.2404809713889,
17.4257741628426));
#179064=CARTESIAN_POINT('Ctrl Pts',(17.0730217096313,-20.2649358772608,
17.4238340413425));
#179065=CARTESIAN_POINT('Ctrl Pts',(17.0970989611475,-20.2944957605528,
17.4214901795506));
#179066=CARTESIAN_POINT('Ctrl Pts',(17.1016316456187,-20.3000035003857,
17.4210535170314));
#179067=CARTESIAN_POINT('Ctrl Pts',(17.1088046138549,-20.3086302567729,
17.4203698082325));
#179068=CARTESIAN_POINT('Ctrl Pts',(17.1114261896776,-20.3117646588463,
17.4201214420577));
#179069=CARTESIAN_POINT('Ctrl Pts',(17.116358709412,-20.3176274892084,17.4196570034692));
#179070=CARTESIAN_POINT('Ctrl Pts',(17.118667463459,-20.3203576217125,17.4194407843878));
#179071=CARTESIAN_POINT('Ctrl Pts',(17.1239738343295,-20.3266003305954,
17.4189464868741));
#179072=CARTESIAN_POINT('Ctrl Pts',(17.1269760293182,-20.3301089512796,
17.4186687498332));
#179073=CARTESIAN_POINT('Ctrl Pts',(17.1363107954761,-20.3409463693886,
17.4178110092996));
#179074=CARTESIAN_POINT('Ctrl Pts',(17.1426823022761,-20.3482416711482,
17.4172338030958));
#179075=CARTESIAN_POINT('Ctrl Pts',(17.2191980624413,-20.4346471793953,
17.4103960435262));
#179076=CARTESIAN_POINT('Ctrl Pts',(17.2951338106021,-20.5084503707135,
17.4045386166813));
#179077=CARTESIAN_POINT('Ctrl Pts',(17.5054690018733,-20.6842682445332,
17.3895655348813));
#179078=CARTESIAN_POINT('Ctrl Pts',(17.6470724835729,-20.7764526196379,
17.3805829394062));
#179079=CARTESIAN_POINT('Ctrl Pts',(17.822655576485,-20.8629918486194,17.3693878594998));
#179080=CARTESIAN_POINT('Ctrl Pts',(17.8474436531446,-20.8746170320157,
17.36780778385));
#179081=CARTESIAN_POINT('Ctrl Pts',(17.890732859955,-20.8939037486668,17.3650446455047));
#179082=CARTESIAN_POINT('Ctrl Pts',(17.9091304099634,-20.9017896700504,
17.3638692028871));
#179083=CARTESIAN_POINT('Ctrl Pts',(17.9357223705074,-20.9127443234659,
17.3621674562089));
#179084=CARTESIAN_POINT('Ctrl Pts',(17.94382864892,-20.916025129215,17.3616483353886));
#179085=CARTESIAN_POINT('Ctrl Pts',(17.9580051965668,-20.9216607463205,
17.3607397532174));
#179086=CARTESIAN_POINT('Ctrl Pts',(17.9640664729106,-20.9240379694504,
17.3603510531793));
#179087=CARTESIAN_POINT('Ctrl Pts',(17.9757188816356,-20.9285461154423,
17.3596033232956));
#179088=CARTESIAN_POINT('Ctrl Pts',(17.9813082786803,-20.9306813721396,
17.3592444435844));
#179089=CARTESIAN_POINT('Ctrl Pts',(17.9959234141704,-20.9361937461023,
17.3583054597131));
#179090=CARTESIAN_POINT('Ctrl Pts',(18.0049632171588,-20.9395329514456,
17.3577240938987));
#179091=CARTESIAN_POINT('Ctrl Pts',(18.036161112823,-20.9508156402387,17.3557155218438));
#179092=CARTESIAN_POINT('Ctrl Pts',(18.0584280752299,-20.9584509912777,
17.354278145317));
#179093=CARTESIAN_POINT('Ctrl Pts',(18.2402544669451,-21.017429548226,17.3425060558339));
#179094=CARTESIAN_POINT('Ctrl Pts',(18.4052411676596,-21.0500183426998,
17.3315368351925));
#179095=CARTESIAN_POINT('Ctrl Pts',(18.6971294514733,-21.0723777872687,
17.3121910022218));
#179096=CARTESIAN_POINT('Ctrl Pts',(18.8225689067809,-21.0708495821324,
17.3039194491839));
#179097=CARTESIAN_POINT('Ctrl Pts',(18.9590204336079,-21.0570409003437,
17.2954142426233));
#179098=CARTESIAN_POINT('Ctrl Pts',(18.9708823738012,-21.055739086411,17.2946791143928));
#179099=CARTESIAN_POINT('Ctrl Pts',(18.9877249183501,-21.0537464009877,
17.2936419606708));
#179100=CARTESIAN_POINT('Ctrl Pts',(18.9927147954818,-21.0531380069029,
17.2933355170668));
#179101=CARTESIAN_POINT('Ctrl Pts',(19.0013083959076,-21.0520591488736,
17.2928092441102));
#179102=CARTESIAN_POINT('Ctrl Pts',(19.0049131460946,-21.0515971697787,
17.2925889405603));
#179103=CARTESIAN_POINT('Ctrl Pts',(19.011898612675,-21.0506836335322,17.2921629209678));
#179104=CARTESIAN_POINT('Ctrl Pts',(19.0152794271839,-21.05023318933,17.2919571409472));
#179105=CARTESIAN_POINT('Ctrl Pts',(19.0243947358565,-21.0489962803707,
17.2914033745344));
#179106=CARTESIAN_POINT('Ctrl Pts',(19.0301271663692,-21.0481944579716,
17.2910562491542));
#179107=CARTESIAN_POINT('Ctrl Pts',(19.0513721364507,-21.0451339335721,
17.289773709563));
#179108=CARTESIAN_POINT('Ctrl Pts',(19.0668631684812,-21.0427264001738,
17.2888463317429));
#179109=CARTESIAN_POINT('Ctrl Pts',(19.2155428960719,-21.0179249394503,
17.280008389634));
#179110=CARTESIAN_POINT('Ctrl Pts',(19.3463463229008,-20.9830025742286,
17.2727063784694));
#179111=CARTESIAN_POINT('Ctrl Pts',(19.6191655652255,-20.8813828491795,
17.2568966641222));
#179112=CARTESIAN_POINT('Ctrl Pts',(19.7588984006038,-20.8109276533858,
17.2484018466449));
#179113=CARTESIAN_POINT('Ctrl Pts',(19.9074405477088,-20.7141517712137,
17.2380772478022));
#179114=CARTESIAN_POINT('Ctrl Pts',(19.9250887823573,-20.7022711355029,
17.2368288459338));
#179115=CARTESIAN_POINT('Ctrl Pts',(19.9499355347727,-20.6849946895212,
17.2350386370128));
#179116=CARTESIAN_POINT('Ctrl Pts',(19.9572837000914,-20.6798156162987,
17.2345050692874));
#179117=CARTESIAN_POINT('Ctrl Pts',(19.9699061409286,-20.6707982888845,
17.2335812578259));
#179118=CARTESIAN_POINT('Ctrl Pts',(19.9751961130677,-20.6669821440746,
17.233191868419));
#179119=CARTESIAN_POINT('Ctrl Pts',(19.9852929633915,-20.6596271690569,
17.2324443315621));
#179120=CARTESIAN_POINT('Ctrl Pts',(19.9901026833484,-20.6560923321479,
17.2320863415411));
#179121=CARTESIAN_POINT('Ctrl Pts',(20.0025749704088,-20.6468445053715,
17.2311530420332));
#179122=CARTESIAN_POINT('Ctrl Pts',(20.0102138480243,-20.6410999266948,
17.2305765006436));
#179123=CARTESIAN_POINT('Ctrl Pts',(20.0361512259079,-20.6213181420612,
17.2286018182644));
#179124=CARTESIAN_POINT('Ctrl Pts',(20.0542586234261,-20.6070341313103,
17.2271939621623));
#179125=CARTESIAN_POINT('Ctrl Pts',(20.2073751973753,-20.4821362645431,
17.2150307346349));
#179126=CARTESIAN_POINT('Ctrl Pts',(20.328435538637,-20.3555325794204,17.2035802962184));
#179127=CARTESIAN_POINT('Ctrl Pts',(20.4849024782737,-20.1451964155519,
17.1862589416547));
#179128=CARTESIAN_POINT('Ctrl Pts',(20.5328183961388,-20.0716568609642,
17.1804785067545));
#179129=CARTESIAN_POINT('Ctrl Pts',(20.5947618329447,-19.9622958974445,
17.1724528915946));
#179130=CARTESIAN_POINT('Ctrl Pts',(20.6125941671862,-19.9287378202598,
17.1700628187077));
#179131=CARTESIAN_POINT('Ctrl Pts',(20.6328908004931,-19.8879274571345,
17.1672580293692));
#179132=CARTESIAN_POINT('Ctrl Pts',(20.6362304114609,-19.8811210593469,
17.166793579358));
#179133=CARTESIAN_POINT('Ctrl Pts',(20.6413564020617,-19.8705303828504,
17.1660762348604));
#179134=CARTESIAN_POINT('Ctrl Pts',(20.6431682084479,-19.8667585808596,
17.1658218014577));
#179135=CARTESIAN_POINT('Ctrl Pts',(20.6465022958226,-19.8597646541829,
17.1653519795243));
#179136=CARTESIAN_POINT('Ctrl Pts',(20.6480276112758,-19.8565440854293,
17.1651364080874));
#179137=CARTESIAN_POINT('Ctrl Pts',(20.6514510223034,-19.8492684228995,
17.1646511347528));
#179138=CARTESIAN_POINT('Ctrl Pts',(20.6533443846704,-19.8452111617896,
17.1643817269502));
#179139=CARTESIAN_POINT('Ctrl Pts',(20.6588757726999,-19.8332592238418,
17.1635915503718));
#179140=CARTESIAN_POINT('Ctrl Pts',(20.6624781135022,-19.8253480013949,
17.1630729297659));
#179141=CARTESIAN_POINT('Ctrl Pts',(20.6876008168352,-19.7692617560708,
17.1594257598493));
#179142=CARTESIAN_POINT('Ctrl Pts',(20.7073641585449,-19.7203149204864,
17.1563963707161));
#179143=CARTESIAN_POINT('Ctrl Pts',(20.7307032603142,-19.6556479020907,
17.1525281198126));
#179144=CARTESIAN_POINT('Ctrl Pts',(20.735957063009,-19.6405580701476,17.1516347921442));
#179145=CARTESIAN_POINT('Ctrl Pts',(20.7571454890679,-19.5774078138515,
17.1479295510806));
#179146=CARTESIAN_POINT('Ctrl Pts',(20.7715246361901,-19.5288416622487,
17.1451596034167));
#179147=CARTESIAN_POINT('Ctrl Pts',(20.8114258098308,-19.3738539000839,
17.1364459819417));
#179148=CARTESIAN_POINT('Ctrl Pts',(20.8304479895602,-19.2659484962345,
17.1305551319957));
#179149=CARTESIAN_POINT('Ctrl Pts',(20.8463898655661,-19.1021421846975,
17.1214043793214));
#179150=CARTESIAN_POINT('Ctrl Pts',(20.8495851592457,-19.0470389728025,
17.118293184714));
#179151=CARTESIAN_POINT('Ctrl Pts',(20.8512712123662,-18.9575442512807,
17.1131436281628));
#179152=CARTESIAN_POINT('Ctrl Pts',(20.8510825804375,-18.9232028484331,
17.1111447653357));
#179153=CARTESIAN_POINT('Ctrl Pts',(20.8497365137264,-18.8780749468508,
17.1084821160901));
#179154=CARTESIAN_POINT('Ctrl Pts',(20.8493313558287,-18.8672700909863,
17.1078419032162));
#179155=CARTESIAN_POINT('Ctrl Pts',(20.8485321309317,-18.8495770398198,
17.1067889431909));
#179156=CARTESIAN_POINT('Ctrl Pts',(20.8481871265019,-18.842686744097,17.1063777387798));
#179157=CARTESIAN_POINT('Ctrl Pts',(20.8474540544223,-18.8293515327965,
17.1055796443721));
#179158=CARTESIAN_POINT('Ctrl Pts',(20.8470701697673,-18.8229064569063,
17.1051928900797));
#179159=CARTESIAN_POINT('Ctrl Pts',(20.8461156360282,-18.8080278144545,
17.1042976457736));
#179160=CARTESIAN_POINT('Ctrl Pts',(20.8455239500489,-18.7995957503937,
17.1037885002504));
#179161=CARTESIAN_POINT('Ctrl Pts',(20.8437966519874,-18.7769254371075,
17.1024147036412));
#179162=CARTESIAN_POINT('Ctrl Pts',(20.8425674281465,-18.7626949536508,
17.1015471278806));
#179163=CARTESIAN_POINT('Ctrl Pts',(20.8276355885117,-18.6080958002519,
17.0920634644556));
#179164=CARTESIAN_POINT('Ctrl Pts',(20.8000852563815,-18.4694459136423,
17.0829978303278));
#179165=CARTESIAN_POINT('Ctrl Pts',(20.7307945966785,-18.2421892491328,
17.0673675450501));
#179166=CARTESIAN_POINT('Ctrl Pts',(20.6963316889671,-18.1518284542033,
17.060942004802));
#179167=CARTESIAN_POINT('Ctrl Pts',(20.635269890882,-18.0196575505104,17.0514409668087));
#179168=CARTESIAN_POINT('Ctrl Pts',(20.6131815916944,-17.9759022483213,
17.0482790106928));
#179169=CARTESIAN_POINT('Ctrl Pts',(20.5769516840405,-17.9099310052912,
17.0435261713027));
#179170=CARTESIAN_POINT('Ctrl Pts',(20.563882076425,-17.8871476944359,17.0418876090633));
#179171=CARTESIAN_POINT('Ctrl Pts',(20.5469189535631,-17.8588122001037,
17.0398589504759));
#179172=CARTESIAN_POINT('Ctrl Pts',(20.5434188770552,-17.853028649946,17.0394453733763));
#179173=CARTESIAN_POINT('Ctrl Pts',(20.5378019121738,-17.8438467210566,
17.0387896907196));
#179174=CARTESIAN_POINT('Ctrl Pts',(20.535703017919,-17.8404374674221,17.0385464365064));
#179175=CARTESIAN_POINT('Ctrl Pts',(20.5317021285747,-17.8339798900203,
17.0380860939183));
#179176=CARTESIAN_POINT('Ctrl Pts',(20.5298020686265,-17.8309304928456,
17.0378688905139));
#179177=CARTESIAN_POINT('Ctrl Pts',(20.525408345417,-17.8239188607269,17.0373698538717));
#179178=CARTESIAN_POINT('Ctrl Pts',(20.5229092968791,-17.8199600513604,
17.0370883803241));
#179179=CARTESIAN_POINT('Ctrl Pts',(20.5161716320798,-17.8093647645656,
17.0363357253899));
#179180=CARTESIAN_POINT('Ctrl Pts',(20.511909039558,-17.8027435191116,17.0358660879167));
#179181=CARTESIAN_POINT('Ctrl Pts',(20.4795855399492,-17.7531444593571,
17.0323522518052));
#179182=CARTESIAN_POINT('Ctrl Pts',(20.4500044352946,-17.711172380623,17.0294022813644));
#179183=CARTESIAN_POINT('Ctrl Pts',(20.4053569830019,-17.6524781588698,
17.0252478948409));
#179184=CARTESIAN_POINT('Ctrl Pts',(20.3915070883327,-17.6348585946878,
17.0239968303872));
#179185=CARTESIAN_POINT('Ctrl Pts',(20.3484520641552,-17.5818396882788,
17.0202092363147));
#179186=CARTESIAN_POINT('Ctrl Pts',(20.3183729706973,-17.5471664592261,
17.0176999688148));
#179187=CARTESIAN_POINT('Ctrl Pts',(20.2128851959383,-17.4332684728602,
17.0092478755073));
#179188=CARTESIAN_POINT('Ctrl Pts',(20.1324765156178,-17.3589182613142,
17.0033596732591));
#179189=CARTESIAN_POINT('Ctrl Pts',(20.0034493180968,-17.2569410477388,
16.994215076586));
#179190=CARTESIAN_POINT('Ctrl Pts',(19.9588953967741,-17.2244708267689,
16.9911074109248));
#179191=CARTESIAN_POINT('Ctrl Pts',(19.8846332442519,-17.1746679440795,
16.9859631747503));
#179192=CARTESIAN_POINT('Ctrl Pts',(19.855679797452,-17.1562549359242,16.9839659964122));
#179193=CARTESIAN_POINT('Ctrl Pts',(19.8170337188935,-17.1329772405272,
16.9813052732521));
#179194=CARTESIAN_POINT('Ctrl Pts',(19.8077321153054,-17.1274712461177,
16.9806652584713));
#179195=CARTESIAN_POINT('Ctrl Pts',(19.7924259804511,-17.118568509827,16.9796125412864));
#179196=CARTESIAN_POINT('Ctrl Pts',(19.786446216972,-17.1151294155816,16.9792013802263));
#179197=CARTESIAN_POINT('Ctrl Pts',(19.7748369760338,-17.1085279823513,
16.9784033106653));
#179198=CARTESIAN_POINT('Ctrl Pts',(19.769209622997,-17.1053620480574,16.9780165375546));
#179199=CARTESIAN_POINT('Ctrl Pts',(19.7561804757564,-17.0981101553555,
16.9771211633197));
#179200=CARTESIAN_POINT('Ctrl Pts',(19.7487685488852,-17.0940427157634,
16.9766119060867));
#179201=CARTESIAN_POINT('Ctrl Pts',(19.7287642138754,-17.0832203569117,
16.9752376125887));
#179202=CARTESIAN_POINT('Ctrl Pts',(19.7161276161237,-17.0765484475575,
16.9743696483561));
#179203=CARTESIAN_POINT('Ctrl Pts',(19.5995634299499,-17.0165056710283,
16.9663634959402));
#179204=CARTESIAN_POINT('Ctrl Pts',(19.4914690089998,-16.9717042529663,
16.9589236278741));
#179205=CARTESIAN_POINT('Ctrl Pts',(19.2253472622209,-16.8863943993965,
16.940669498441));
#179206=CARTESIAN_POINT('Ctrl Pts',(19.0652449898105,-16.8547576559061,
16.9297153297797));
#179207=CARTESIAN_POINT('Ctrl Pts',(18.870625616796,-16.8391621396681,16.9173083171974));
#179208=CARTESIAN_POINT('Ctrl Pts',(18.8380929695566,-16.8373096427298,
16.9152663165047));
#179209=CARTESIAN_POINT('Ctrl Pts',(18.7982882165433,-16.8359639635512,
16.9128171881611));
#179210=CARTESIAN_POINT('Ctrl Pts',(18.7910465536276,-16.8357563522717,
16.9123736142436));
#179211=CARTESIAN_POINT('Ctrl Pts',(18.7796942477205,-16.8354892077068,
16.911681528221));
#179212=CARTESIAN_POINT('Ctrl Pts',(18.7755843338242,-16.8354044689614,
16.9114316430668));
#179213=CARTESIAN_POINT('Ctrl Pts',(18.7679029855719,-16.8352684759644,
16.9109659035768));
#179214=CARTESIAN_POINT('Ctrl Pts',(18.7643317075639,-16.8352142892998,
16.9107498933849));
#179215=CARTESIAN_POINT('Ctrl Pts',(18.7561808611843,-16.8351112491809,
16.9102580684049));
#179216=CARTESIAN_POINT('Ctrl Pts',(18.75160126969,-16.8350682178783,16.9099825822549));
#179217=CARTESIAN_POINT('Ctrl Pts',(18.7375304072785,-16.8349816673078,
16.9091386543664));
#179218=CARTESIAN_POINT('Ctrl Pts',(18.7280388039128,-16.8349871147156,
16.9085728815195));
#179219=CARTESIAN_POINT('Ctrl Pts',(18.6430927357192,-16.8356071789726,
16.9035382645834));
#179220=CARTESIAN_POINT('Ctrl Pts',(18.5677126421295,-16.8401918211874,
16.8992734412857));
#179221=CARTESIAN_POINT('Ctrl Pts',(18.4499500110904,-16.8537009554024,
16.8927111952766));
#179222=CARTESIAN_POINT('Ctrl Pts',(18.4073278166062,-16.8599128238263,
16.8903571658276));
#179223=CARTESIAN_POINT('Ctrl Pts',(18.2572736260032,-16.8864800209564,
16.8820606563415));
#179224=CARTESIAN_POINT('Ctrl Pts',(18.1512626662309,-16.9138495804539,
16.8761738091633));
#179225=CARTESIAN_POINT('Ctrl Pts',(17.995737716435,-16.9671343761917,16.8670323627783));
#179226=CARTESIAN_POINT('Ctrl Pts',(17.9443513733083,-16.9870121766752,
16.8639265027801));
#179227=CARTESIAN_POINT('Ctrl Pts',(17.8623237772519,-17.0224804674919,
16.8587849891377));
#179228=CARTESIAN_POINT('Ctrl Pts',(17.8311833444689,-17.0368532813996,
16.8567886730124));
#179229=CARTESIAN_POINT('Ctrl Pts',(17.7907073085509,-17.0567415225125,
16.8541289357708));
#179230=CARTESIAN_POINT('Ctrl Pts',(17.781044427072,-17.0615816685984,16.8534890224442));
#179231=CARTESIAN_POINT('Ctrl Pts',(17.765275619888,-17.0696319022643,16.8524364296291));
#179232=CARTESIAN_POINT('Ctrl Pts',(17.7591474991179,-17.0727982599548,
16.8520252907696));
#179233=CARTESIAN_POINT('Ctrl Pts',(17.747313090532,-17.0789864829095,16.8512272339164));
#179234=CARTESIAN_POINT('Ctrl Pts',(17.7416049319149,-17.0820046203462,
16.8508404511521));
#179235=CARTESIAN_POINT('Ctrl Pts',(17.7284538608288,-17.0890353038905,
16.8499450102998));
#179236=CARTESIAN_POINT('Ctrl Pts',(17.7210210398499,-17.0930664024755,
16.8494356957957));
#179237=CARTESIAN_POINT('Ctrl Pts',(17.7010895643663,-17.1040310283788,
16.84806114753));
#179238=CARTESIAN_POINT('Ctrl Pts',(17.6886368158597,-17.1110466910775,
16.8471929841115));
#179239=CARTESIAN_POINT('Ctrl Pts',(17.5748400110784,-17.1766847385948,
16.839171510024));
#179240=CARTESIAN_POINT('Ctrl Pts',(17.4784677450456,-17.2434839586772,
16.8317151784735));
#179241=CARTESIAN_POINT('Ctrl Pts',(17.2619561354151,-17.4218067422182,
16.8133920003601));
#179242=CARTESIAN_POINT('Ctrl Pts',(17.1482518540488,-17.5399774970377,
16.8023832044535));
#179243=CARTESIAN_POINT('Ctrl Pts',(17.0301039703484,-17.6952463971379,
16.7899955315845));
#179244=CARTESIAN_POINT('Ctrl Pts',(17.0114991784074,-17.7208694354002,
16.7880124611225));
#179245=CARTESIAN_POINT('Ctrl Pts',(16.9893874427833,-17.7528054419641,
16.7856241526983));
#179246=CARTESIAN_POINT('Ctrl Pts',(16.9853298243766,-17.7587300460031,
16.7851845272729));
#179247=CARTESIAN_POINT('Ctrl Pts',(16.9790047132035,-17.7680670093458,
16.7844972263259));
#179248=CARTESIAN_POINT('Ctrl Pts',(16.9767168904267,-17.7714654361251,
16.784248208229));
#179249=CARTESIAN_POINT('Ctrl Pts',(16.9724517498487,-17.7778409244991,
16.7837832155224));
#179250=CARTESIAN_POINT('Ctrl Pts',(16.9704721279198,-17.780816318075,16.783567090291));
#179251=CARTESIAN_POINT('Ctrl Pts',(16.9659610004637,-17.7876339636287,
16.7830738731386));
#179252=CARTESIAN_POINT('Ctrl Pts',(16.9634344849883,-17.7914794579568,
16.7827971170523));
#179253=CARTESIAN_POINT('Ctrl Pts',(16.9568582374412,-17.8015603297506,
16.7820752899555));
#179254=CARTESIAN_POINT('Ctrl Pts',(16.9528287407576,-17.8078089197858,
16.7816315358764));
#179255=CARTESIAN_POINT('Ctrl Pts',(16.9262822845475,-17.8494549280485,
16.7786973474529));
#179256=CARTESIAN_POINT('Ctrl Pts',(16.9047872114559,-17.8854963304429,
16.7762696353254));
#179257=CARTESIAN_POINT('Ctrl Pts',(16.8738142378991,-17.941124484184,16.7726519437717));
#179258=CARTESIAN_POINT('Ctrl Pts',(16.8635446403685,-17.9602554880022,
16.7714302374583));
#179259=CARTESIAN_POINT('Ctrl Pts',(16.8457278215645,-17.9947076192241,
16.7692640336148));
#179260=CARTESIAN_POINT('Ctrl Pts',(16.8380683858714,-18.0099682299352,
16.768316156312));
#179261=CARTESIAN_POINT('Ctrl Pts',(16.7987610397288,-18.0907057371168,
16.7633540382376));
#179262=CARTESIAN_POINT('Ctrl Pts',(16.7703355293929,-18.1576524547246,
16.7594186555602));
#179263=CARTESIAN_POINT('Ctrl Pts',(16.7454192974512,-18.2258899605083,
16.7554728927777));
#179264=CARTESIAN_POINT('',(16.6170000778107,-18.9514260221329,17.2909082085163));
#179265=CARTESIAN_POINT('Ctrl Pts',(16.7454193692319,-18.2258897639242,
16.5356516076535));
#179266=CARTESIAN_POINT('Ctrl Pts',(16.7457579316466,-18.2249625511863,
16.5357110070265));
#179267=CARTESIAN_POINT('Ctrl Pts',(16.7460971434404,-18.2240355728191,
16.5357703682188));
#179268=CARTESIAN_POINT('Ctrl Pts',(16.7488929534975,-18.2164118714529,
16.5362583814801));
#179269=CARTESIAN_POINT('Ctrl Pts',(16.7513827741478,-18.2097272603787,
16.5366850874225));
#179270=CARTESIAN_POINT('Ctrl Pts',(16.7648702365569,-18.1740685038746,
16.5389555844351));
#179271=CARTESIAN_POINT('Ctrl Pts',(16.7764699452589,-18.1453242589646,
16.5407654901067));
#179272=CARTESIAN_POINT('Ctrl Pts',(16.8532263795245,-17.9665380260565,
16.5519560730976));
#179273=CARTESIAN_POINT('Ctrl Pts',(16.9349647273724,-17.8242016348003,
16.5606012080705));
#179274=CARTESIAN_POINT('Ctrl Pts',(17.1022875653794,-17.598098072237,16.5759957187365));
#179275=CARTESIAN_POINT('Ctrl Pts',(17.1800410103599,-17.5095222650219,
16.58256213577));
#179276=CARTESIAN_POINT('Ctrl Pts',(17.2750386749844,-17.4179447995518,
16.590292142767));
#179277=CARTESIAN_POINT('Ctrl Pts',(17.2854344416404,-17.4081245794737,
16.591134269601));
#179278=CARTESIAN_POINT('Ctrl Pts',(17.3021355858462,-17.3926652592262,
16.5924816547495));
#179279=CARTESIAN_POINT('Ctrl Pts',(17.3083767594504,-17.3869572187501,
16.5929839662928));
#179280=CARTESIAN_POINT('Ctrl Pts',(17.3194429380778,-17.3769574558901,
16.5938725894741));
#179281=CARTESIAN_POINT('Ctrl Pts',(17.3242537156038,-17.3726500991246,
16.5942582340704));
#179282=CARTESIAN_POINT('Ctrl Pts',(17.3342433738404,-17.3637878116787,
16.5950577033534));
#179283=CARTESIAN_POINT('Ctrl Pts',(17.3394249519492,-17.359236049751,16.5954716538736));
#179284=CARTESIAN_POINT('Ctrl Pts',(17.3527797460429,-17.3476196460923,
16.5965367450822));
#179285=CARTESIAN_POINT('Ctrl Pts',(17.3609848905063,-17.3405921645117,
16.5971894129516));
#179286=CARTESIAN_POINT('Ctrl Pts',(17.3954326586002,-17.3115427138292,
16.5999226832476));
#179287=CARTESIAN_POINT('Ctrl Pts',(17.4221529057372,-17.2900975897885,
16.6020265575377));
#179288=CARTESIAN_POINT('Ctrl Pts',(17.4930983435437,-17.2359355321594,
16.6075743393707));
#179289=CARTESIAN_POINT('Ctrl Pts',(17.538096974659,-17.2042788219609,16.6110565170793));
#179290=CARTESIAN_POINT('Ctrl Pts',(17.6611866045542,-17.1246657032057,
16.6204782806145));
#179291=CARTESIAN_POINT('Ctrl Pts',(17.7412413669288,-17.0799670751409,
16.6265050358633));
#179292=CARTESIAN_POINT('Ctrl Pts',(17.8723898346,-17.017524021557,16.6361026784844));
#179293=CARTESIAN_POINT('Ctrl Pts',(17.9217074221706,-16.996303110698,16.639652561429));
#179294=CARTESIAN_POINT('Ctrl Pts',(18.0061489782579,-16.9637145194573,
16.645587331596));
#179295=CARTESIAN_POINT('Ctrl Pts',(18.0408609965526,-16.9513489079362,
16.6479873598333));
#179296=CARTESIAN_POINT('Ctrl Pts',(18.1208694487278,-16.9251796859873,
16.6534054177813));
#179297=CARTESIAN_POINT('Ctrl Pts',(18.166344442657,-16.9119760836724,16.6564034619504));
#179298=CARTESIAN_POINT('Ctrl Pts',(18.2196941097344,-16.8984085587801,
16.6597974543887));
#179299=CARTESIAN_POINT('Ctrl Pts',(18.2271711786098,-16.8965504369703,
16.6602703428091));
#179300=CARTESIAN_POINT('Ctrl Pts',(18.2391594155229,-16.8936406414161,
16.6610238999646));
#179301=CARTESIAN_POINT('Ctrl Pts',(18.2436640998979,-16.8925629023622,
16.6613060095215));
#179302=CARTESIAN_POINT('Ctrl Pts',(18.2516628015271,-16.890676956991,16.6618050353246));
#179303=CARTESIAN_POINT('Ctrl Pts',(18.2551553772695,-16.8898628346593,
16.662022288459));
#179304=CARTESIAN_POINT('Ctrl Pts',(18.262578318197,-16.8881524164112,16.6624826492754));
#179305=CARTESIAN_POINT('Ctrl Pts',(18.2665091707841,-16.8872584724516,
16.6627256213737));
#179306=CARTESIAN_POINT('Ctrl Pts',(18.2771600196659,-16.8848682604252,
16.6633818228253));
#179307=CARTESIAN_POINT('Ctrl Pts',(18.2838848677486,-16.8833935204877,
16.6637938345701));
#179308=CARTESIAN_POINT('Ctrl Pts',(18.3177490238762,-16.8761401661215,
16.6658575410414));
#179309=CARTESIAN_POINT('Ctrl Pts',(18.3449942703993,-16.8708624181691,
16.667482244176));
#179310=CARTESIAN_POINT('Ctrl Pts',(18.4247162617235,-16.8570397014274,
16.6721533891327));
#179311=CARTESIAN_POINT('Ctrl Pts',(18.4774228910061,-16.8499333875376,
16.6751378899842));
#179312=CARTESIAN_POINT('Ctrl Pts',(18.6704674242955,-16.8312759601424,
16.6858683621127));
#179313=CARTESIAN_POINT('Ctrl Pts',(18.8115927598804,-16.8317433080845,
16.6933518959393));
#179314=CARTESIAN_POINT('Ctrl Pts',(19.0430308398618,-16.8556622025063,
16.7062219698052));
#179315=CARTESIAN_POINT('Ctrl Pts',(19.1337087864596,-16.8710477869865,
16.7114143335807));
#179316=CARTESIAN_POINT('Ctrl Pts',(19.2364858658513,-16.8954527946891,
16.7176070908601));
#179317=CARTESIAN_POINT('Ctrl Pts',(19.2498461121305,-16.8987632313086,
16.7184180563041));
#179318=CARTESIAN_POINT('Ctrl Pts',(19.2712106903153,-16.9042786844685,
16.7197248421897));
#179319=CARTESIAN_POINT('Ctrl Pts',(19.2792361207256,-16.906400948003,16.720217990276));
#179320=CARTESIAN_POINT('Ctrl Pts',(19.2934578943537,-16.9102514249627,
16.721096000627));
#179321=CARTESIAN_POINT('Ctrl Pts',(19.2996592653873,-16.9119607912364,
16.7214802470044));
#179322=CARTESIAN_POINT('Ctrl Pts',(19.3125582726307,-16.9155796531408,
16.7222824324488));
#179323=CARTESIAN_POINT('Ctrl Pts',(19.3192544605672,-16.9174939866115,
16.7227005251823));
#179324=CARTESIAN_POINT('Ctrl Pts',(19.3366078024684,-16.9225477914207,
16.7237883917691));
#179325=CARTESIAN_POINT('Ctrl Pts',(19.3472498035017,-16.9257381458365,
16.7244598207519));
#179326=CARTESIAN_POINT('Ctrl Pts',(19.3932464610423,-16.9399229822027,
16.7273808223348));
#179327=CARTESIAN_POINT('Ctrl Pts',(19.4283326608282,-16.9517595878086,
16.7296578511468));
#179328=CARTESIAN_POINT('Ctrl Pts',(19.520606171892,-16.9856091004283,16.7357809459443));
#179329=CARTESIAN_POINT('Ctrl Pts',(19.577175806304,-17.0091938088539,16.7396759213215));
#179330=CARTESIAN_POINT('Ctrl Pts',(19.7735717689237,-17.1012685187257,
16.7536844023944));
#179331=CARTESIAN_POINT('Ctrl Pts',(19.9067736508129,-17.1826745555084,
16.7641302935602));
#179332=CARTESIAN_POINT('Ctrl Pts',(20.0425288699526,-17.287758870077,16.7752910035534));
#179333=CARTESIAN_POINT('Ctrl Pts',(20.0551025450465,-17.2977223849462,
16.7763295833007));
#179334=CARTESIAN_POINT('Ctrl Pts',(20.1049633123591,-17.338163668473,16.780464122607));
#179335=CARTESIAN_POINT('Ctrl Pts',(20.141321947888,-17.3697693492074,16.7835157651995));
#179336=CARTESIAN_POINT('Ctrl Pts',(20.1822398024961,-17.4078658054716,
16.786963012381));
#179337=CARTESIAN_POINT('Ctrl Pts',(20.1878770983402,-17.413172419222,16.7874382343839));
#179338=CARTESIAN_POINT('Ctrl Pts',(20.1968483347533,-17.4217107120478,
16.7881947875875));
#179339=CARTESIAN_POINT('Ctrl Pts',(20.2002009138202,-17.4249225833077,
16.7884775774023));
#179340=CARTESIAN_POINT('Ctrl Pts',(20.2061253709757,-17.4306358873811,
16.7889773728589));
#179341=CARTESIAN_POINT('Ctrl Pts',(20.2087014888055,-17.4331328594372,
16.7891947190711));
#179342=CARTESIAN_POINT('Ctrl Pts',(20.2141542441453,-17.4384450412243,
16.7896547982651));
#179343=CARTESIAN_POINT('Ctrl Pts',(20.2170291983152,-17.4412619031539,
16.7898973981151));
#179344=CARTESIAN_POINT('Ctrl Pts',(20.2247797112398,-17.4488992515652,
16.7905515404179));
#179345=CARTESIAN_POINT('Ctrl Pts',(20.2296399630892,-17.453735300043,16.7909618782856));
#179346=CARTESIAN_POINT('Ctrl Pts',(20.2538070883146,-17.4780168628845,
16.7930034478209));
#179347=CARTESIAN_POINT('Ctrl Pts',(20.2727595998508,-17.497813310003,16.794608376622));
#179348=CARTESIAN_POINT('Ctrl Pts',(20.3266669183098,-17.5563555408519,
16.7992046181021));
#179349=CARTESIAN_POINT('Ctrl Pts',(20.360581867575,-17.5960340951197,16.8021363322757));
#179350=CARTESIAN_POINT('Ctrl Pts',(20.4796153933748,-17.7461980123186,
16.8127466170172));
#179351=CARTESIAN_POINT('Ctrl Pts',(20.5552265603972,-17.8637593465706,
16.8201606503024));
#179352=CARTESIAN_POINT('Ctrl Pts',(20.6617591792953,-18.0720223132515,
16.8330840696799));
#179353=CARTESIAN_POINT('Ctrl Pts',(20.6991033001663,-18.1589161504293,
16.8384165267062));
#179354=CARTESIAN_POINT('Ctrl Pts',(20.7351175527663,-18.2610521829524,
16.8447649157734));
#179355=CARTESIAN_POINT('Ctrl Pts',(20.7395894900493,-18.2741422496332,
16.8455798672138));
#179356=CARTESIAN_POINT('Ctrl Pts',(20.746545628087,-18.2951755627874,16.846891852208));
#179357=CARTESIAN_POINT('Ctrl Pts',(20.7491118760681,-18.3030914006092,
16.8473861790022));
#179358=CARTESIAN_POINT('Ctrl Pts',(20.7535799444679,-18.3171557148462,
16.848265547018));
#179359=CARTESIAN_POINT('Ctrl Pts',(20.7555005328611,-18.3232981527626,
16.8486499657966));
#179360=CARTESIAN_POINT('Ctrl Pts',(20.7594384278194,-18.3360969627027,
16.8494517650095));
#179361=CARTESIAN_POINT('Ctrl Pts',(20.7614509958386,-18.3427547013591,
16.8498692954058));
#179362=CARTESIAN_POINT('Ctrl Pts',(20.7665811782359,-18.3600327179641,
16.8509540754894));
#179363=CARTESIAN_POINT('Ctrl Pts',(20.7696483469128,-18.3706676427868,
16.8516229627504));
#179364=CARTESIAN_POINT('Ctrl Pts',(20.7825082896349,-18.4166075116827,
16.854517792768));
#179365=CARTESIAN_POINT('Ctrl Pts',(20.7914665648738,-18.4521376183938,
16.8567705860487));
#179366=CARTESIAN_POINT('Ctrl Pts',(20.8127333699572,-18.5467825422329,
16.8628119273177));
#179367=CARTESIAN_POINT('Ctrl Pts',(20.8234420278755,-18.6062189063305,
16.8666477812295));
#179368=CARTESIAN_POINT('Ctrl Pts',(20.8539096070944,-18.8296972741524,
16.8812045005653));
#179369=CARTESIAN_POINT('Ctrl Pts',(20.8569895064341,-18.9953986078187,
16.8923178090366));
#179370=CARTESIAN_POINT('Ctrl Pts',(20.8402747663553,-19.1648899587749,
16.9033404905975));
#179371=CARTESIAN_POINT('Ctrl Pts',(20.8397506016606,-19.1700136010275,
16.9036733163694));
#179372=CARTESIAN_POINT('Ctrl Pts',(20.8385402686491,-19.1814326919621,
16.9044141620626));
#179373=CARTESIAN_POINT('Ctrl Pts',(20.8378445375761,-19.1877270998669,
16.9048219020755));
#179374=CARTESIAN_POINT('Ctrl Pts',(20.8319910254868,-19.2385936639612,
16.9081114066809));
#179375=CARTESIAN_POINT('Ctrl Pts',(20.8254451925663,-19.2829983820863,
16.9109488191941));
#179376=CARTESIAN_POINT('Ctrl Pts',(20.8161485353515,-19.3346277269972,
16.9141824039571));
#179377=CARTESIAN_POINT('Ctrl Pts',(20.8147646143112,-19.3420834840355,
16.9146477509915));
#179378=CARTESIAN_POINT('Ctrl Pts',(20.8124775967123,-19.3540460213231,
16.9153916170681));
#179379=CARTESIAN_POINT('Ctrl Pts',(20.8115998471143,-19.3585574983769,
16.9156715200884));
#179380=CARTESIAN_POINT('Ctrl Pts',(20.8100119342341,-19.3665796393241,
16.9161680605031));
#179381=CARTESIAN_POINT('Ctrl Pts',(20.8093075464648,-19.3700913975676,
16.9163850228345));
#179382=CARTESIAN_POINT('Ctrl Pts',(20.8077872269704,-19.3775725061254,
16.9168463485946));
#179383=CARTESIAN_POINT('Ctrl Pts',(20.8069688120972,-19.3815412965269,
16.9170905682988));
#179384=CARTESIAN_POINT('Ctrl Pts',(20.8047097734705,-19.3923393549919,
16.9177536780116));
#179385=CARTESIAN_POINT('Ctrl Pts',(20.8032467497388,-19.3991639579512,
16.9181713062858));
#179386=CARTESIAN_POINT('Ctrl Pts',(20.7955436669008,-19.4342492116117,
16.9203113336856));
#179387=CARTESIAN_POINT('Ctrl Pts',(20.7887579865491,-19.4623884771996,
16.9220042938675));
#179388=CARTESIAN_POINT('Ctrl Pts',(20.7669925003292,-19.545159912836,16.9269383504506));
#179389=CARTESIAN_POINT('Ctrl Pts',(20.7503942898981,-19.5993423806615,
16.9301088958517));
#179390=CARTESIAN_POINT('Ctrl Pts',(20.6842689006648,-19.7878345898215,
16.9411316553532));
#179391=CARTESIAN_POINT('Ctrl Pts',(20.6233265152133,-19.9177200611084,
16.9487391883837));
#179392=CARTESIAN_POINT('Ctrl Pts',(20.5287380642251,-20.0755094955522,
16.9589508547083));
#179393=CARTESIAN_POINT('Ctrl Pts',(20.506721953469,-20.1099356347493,16.9612417048194));
#179394=CARTESIAN_POINT('Ctrl Pts',(20.4565623206211,-20.1835828464794,
16.9663073414754));
#179395=CARTESIAN_POINT('Ctrl Pts',(20.4280464712532,-20.2225208723823,
16.9690932490908));
#179396=CARTESIAN_POINT('Ctrl Pts',(20.3904563072864,-20.2703321145388,
16.972670343423));
#179397=CARTESIAN_POINT('Ctrl Pts',(20.3825980338955,-20.2801459161364,
16.9734131972958));
#179398=CARTESIAN_POINT('Ctrl Pts',(20.370000609189,-20.2955941350155,16.9745965841451));
#179399=CARTESIAN_POINT('Ctrl Pts',(20.3653185987138,-20.3012749239152,
16.9750348091776));
#179400=CARTESIAN_POINT('Ctrl Pts',(20.3565353225848,-20.3118193265516,
16.9758540025463));
#179401=CARTESIAN_POINT('Ctrl Pts',(20.3524415674669,-20.3166891093673,
16.9762346616875));
#179402=CARTESIAN_POINT('Ctrl Pts',(20.3432950899046,-20.3274703882299,
16.9770826379979));
#179403=CARTESIAN_POINT('Ctrl Pts',(20.3382316379539,-20.3333726233566,
16.9775503943819));
#179404=CARTESIAN_POINT('Ctrl Pts',(20.3234078905989,-20.3504605605342,
16.9789150281003));
#179405=CARTESIAN_POINT('Ctrl Pts',(20.313562464884,-20.3615714894902,16.9798154384965));
#179406=CARTESIAN_POINT('Ctrl Pts',(20.2335265870203,-20.4500034041803,
16.9870893252779));
#179407=CARTESIAN_POINT('Ctrl Pts',(20.1578298999202,-20.5221264019524,
16.9937011742737));
#179408=CARTESIAN_POINT('Ctrl Pts',(19.947192608373,-20.69501811552,17.0114031389657));
#179409=CARTESIAN_POINT('Ctrl Pts',(19.8050215000256,-20.7858096987755,
17.0227380649217));
#179410=CARTESIAN_POINT('Ctrl Pts',(19.6178491272122,-20.8760780578777,
17.0360339347626));
#179411=CARTESIAN_POINT('Ctrl Pts',(19.5816031288803,-20.8923182868501,
17.0385365138317));
#179412=CARTESIAN_POINT('Ctrl Pts',(19.5381637633804,-20.9103317198838,
17.0414334940262));
#179413=CARTESIAN_POINT('Ctrl Pts',(19.5313937441473,-20.9130980862233,
17.041882090998));
#179414=CARTESIAN_POINT('Ctrl Pts',(19.5203752769399,-20.9175339624139,
17.0426073443738));
#179415=CARTESIAN_POINT('Ctrl Pts',(19.5161355923517,-20.9192248853812,
17.0428852452359));
#179416=CARTESIAN_POINT('Ctrl Pts',(19.508569916496,-20.9222139963249,17.043379045138));
#179417=CARTESIAN_POINT('Ctrl Pts',(19.5052460858614,-20.923517492325,17.0435952602193));
#179418=CARTESIAN_POINT('Ctrl Pts',(19.4980785171377,-20.9263074742307,
17.0440599397931));
#179419=CARTESIAN_POINT('Ctrl Pts',(19.4942337430918,-20.9277911427286,
17.0443082346788));
#179420=CARTESIAN_POINT('Ctrl Pts',(19.4835744358103,-20.9318687660506,
17.0449940057983));
#179421=CARTESIAN_POINT('Ctrl Pts',(19.4767507216162,-20.9344387845927,
17.0454300708023));
#179422=CARTESIAN_POINT('Ctrl Pts',(19.438712247109,-20.9485412579937,17.047845277202));
#179423=CARTESIAN_POINT('Ctrl Pts',(19.4072403424395,-20.9593724284508,
17.0497852111968));
#179424=CARTESIAN_POINT('Ctrl Pts',(19.2210809313221,-21.0185685993613,
17.0609920754098));
#179425=CARTESIAN_POINT('Ctrl Pts',(19.0614935560465,-21.0497876801291,
17.0695592837018));
#179426=CARTESIAN_POINT('Ctrl Pts',(18.7836239819198,-21.0716293086547,
17.0848192198537));
#179427=CARTESIAN_POINT('Ctrl Pts',(18.6668143820672,-21.0711441191033,
17.0913306623629));
#179428=CARTESIAN_POINT('Ctrl Pts',(18.5364141023222,-21.0598076140108,
17.0989987893772));
#179429=CARTESIAN_POINT('Ctrl Pts',(18.5221937291252,-21.0584261708781,
17.0998401416315));
#179430=CARTESIAN_POINT('Ctrl Pts',(18.4995830679418,-21.0559983771151,
17.1011865188859));
#179431=CARTESIAN_POINT('Ctrl Pts',(18.4911830299834,-21.0550455023247,
17.1016886040876));
#179432=CARTESIAN_POINT('Ctrl Pts',(18.4763779343099,-21.0532761742023,
17.1025769635994));
#179433=CARTESIAN_POINT('Ctrl Pts',(18.469970446441,-21.0524806788977,17.1029625721368));
#179434=CARTESIAN_POINT('Ctrl Pts',(18.4567247734735,-21.0507746515551,
17.1037621009545));
#179435=CARTESIAN_POINT('Ctrl Pts',(18.4498872070014,-21.0498599830203,
17.1041761477307));
#179436=CARTESIAN_POINT('Ctrl Pts',(18.4323464890353,-21.0474262152985,
17.1052417694463));
#179437=CARTESIAN_POINT('Ctrl Pts',(18.4216503789837,-21.045858536745,17.1058948745054));
#179438=CARTESIAN_POINT('Ctrl Pts',(18.377048252512,-21.0389720530882,17.1086323803955));
#179439=CARTESIAN_POINT('Ctrl Pts',(18.3432636531629,-21.0329112886132,
17.1107401434045));
#179440=CARTESIAN_POINT('Ctrl Pts',(18.2556228290471,-21.0149795443641,
17.1163006257816));
#179441=CARTESIAN_POINT('Ctrl Pts',(18.2020593553583,-21.0018213693875,
17.1197918341491));
#179442=CARTESIAN_POINT('Ctrl Pts',(18.0413674195267,-20.9556238690923,
17.1305393375562));
#179443=CARTESIAN_POINT('Ctrl Pts',(17.9362970231054,-20.9161575271391,
17.1379542076809));
#179444=CARTESIAN_POINT('Ctrl Pts',(17.7301970838325,-20.8194668160528,
17.1529889026018));
#179445=CARTESIAN_POINT('Ctrl Pts',(17.6297255448464,-20.7618720390721,
17.1605809871905));
#179446=CARTESIAN_POINT('Ctrl Pts',(17.5265614332745,-20.6909286316569,
17.1683149651159));
#179447=CARTESIAN_POINT('Ctrl Pts',(17.5187086993475,-20.6854496649405,
17.1689031869773));
#179448=CARTESIAN_POINT('Ctrl Pts',(17.5071418491718,-20.6772620676196,
17.1697685805832));
#179449=CARTESIAN_POINT('Ctrl Pts',(17.5033990733629,-20.6745944051054,
17.1700484399808));
#179450=CARTESIAN_POINT('Ctrl Pts',(17.4968473584393,-20.6698924207961,
17.1705380032819));
#179451=CARTESIAN_POINT('Ctrl Pts',(17.4940347034429,-20.6678633663296,
17.1707480641273));
#179452=CARTESIAN_POINT('Ctrl Pts',(17.4912141761505,-20.6658180756104,
17.170958598793));
#179453=CARTESIAN_POINT('Ctrl Pts',(17.4912013661276,-20.6658087862697,
17.1709595549785));
#179454=CARTESIAN_POINT('Ctrl Pts',(17.4911759712835,-20.6657903704615,
17.1709614505352));
#179455=CARTESIAN_POINT('Ctrl Pts',(17.4911633862972,-20.6657812438819,
17.1709623899187));
#179456=CARTESIAN_POINT('Ctrl Pts',(17.4911384362608,-20.6657631498002,
17.1709642522647));
#179457=CARTESIAN_POINT('Ctrl Pts',(17.4911260712267,-20.665754182317,17.170965175226));
#179458=CARTESIAN_POINT('Ctrl Pts',(17.4911015560354,-20.6657364027807,
17.1709670051054));
#179459=CARTESIAN_POINT('Ctrl Pts',(17.4910894058864,-20.6657275907405,
17.1709679120229));
#179460=CARTESIAN_POINT('Ctrl Pts',(17.491065316964,-20.6657101195721,17.1709697100762));
#179461=CARTESIAN_POINT('Ctrl Pts',(17.4910533776243,-20.6657014600397,
17.1709706012544));
#179462=CARTESIAN_POINT('Ctrl Pts',(17.4910297034798,-20.6656842889455,
17.1709723683399));
#179463=CARTESIAN_POINT('Ctrl Pts',(17.4910179695274,-20.6656757780083,
17.1709732441836));
#179464=CARTESIAN_POINT('Ctrl Pts',(17.4909947029493,-20.6656589017967,
17.1709749808399));
#179465=CARTESIAN_POINT('Ctrl Pts',(17.4909831701517,-20.6656505364037,
17.1709758416654));
#179466=CARTESIAN_POINT('Ctrl Pts',(17.4909603023359,-20.6656339487263,
17.17097754855));
#179467=CARTESIAN_POINT('Ctrl Pts',(17.4909489668599,-20.6656257261157,
17.1709783946435));
#179468=CARTESIAN_POINT('Ctrl Pts',(17.4909264872925,-20.665609419382,17.1709800725417));
#179469=CARTESIAN_POINT('Ctrl Pts',(17.4909153440214,-20.6656013358597,
17.1709809042852));
#179470=CARTESIAN_POINT('Ctrl Pts',(17.4908932467853,-20.6655853058121,
17.170982553639));
#179471=CARTESIAN_POINT('Ctrl Pts',(17.4908822922737,-20.6655773588959,
17.17098337129));
#179472=CARTESIAN_POINT('Ctrl Pts',(17.4908605676019,-20.6655615984825,
17.1709849928286));
#179473=CARTESIAN_POINT('Ctrl Pts',(17.4908497975491,-20.6655537850687,
17.1709857967083));
#179474=CARTESIAN_POINT('Ctrl Pts',(17.4908284382772,-20.6655382891242,
17.1709873909669));
#179475=CARTESIAN_POINT('Ctrl Pts',(17.4908178489378,-20.6655306065115,
17.1709881813549));
#179476=CARTESIAN_POINT('Ctrl Pts',(17.4907968468906,-20.6655153691357,
17.1709897489441));
#179477=CARTESIAN_POINT('Ctrl Pts',(17.4907864342944,-20.6655078144587,
17.170990526137));
#179478=CARTESIAN_POINT('Ctrl Pts',(17.4907663390662,-20.6654932344378,
17.1709920260355));
#179479=CARTESIAN_POINT('Ctrl Pts',(17.4907566562433,-20.6654862089751,
17.1709927487556));
#179480=CARTESIAN_POINT('Ctrl Pts',(17.4907373266925,-20.6654721839885,
17.1709941914991));
#179481=CARTESIAN_POINT('Ctrl Pts',(17.4907276802347,-20.6654651846616,
17.1709949115024));
#179482=CARTESIAN_POINT('Ctrl Pts',(17.4907084234582,-20.6654512119816,
17.170996348809));
#179483=CARTESIAN_POINT('Ctrl Pts',(17.4906988130375,-20.6654442385553,
17.1709970661199));
#179484=CARTESIAN_POINT('Ctrl Pts',(17.4906796287385,-20.6654303179722,
17.1709984980117));
#179485=CARTESIAN_POINT('Ctrl Pts',(17.4906700543764,-20.6654233704649,
17.1709992126287));
#179486=CARTESIAN_POINT('Ctrl Pts',(17.4906509412146,-20.6654095010115,
17.1710006392058));
#179487=CARTESIAN_POINT('Ctrl Pts',(17.4906414025766,-20.6654025791834,
17.1710013511538));
#179488=CARTESIAN_POINT('Ctrl Pts',(17.4873373597135,-20.6630049183732,
17.1712479589786));
#179489=CARTESIAN_POINT('Ctrl Pts',(17.4840497265218,-20.6606046599071,
17.171493191571));
#179490=CARTESIAN_POINT('Ctrl Pts',(17.4772529883802,-20.6556123329168,
17.1719999110107));
#179491=CARTESIAN_POINT('Ctrl Pts',(17.4737449279074,-20.6530188670642,
17.1722613008812));
#179492=CARTESIAN_POINT('Ctrl Pts',(17.4648423050744,-20.6463946096127,
17.1729243398703));
#179493=CARTESIAN_POINT('Ctrl Pts',(17.4594588676324,-20.6423488551926,
17.1733249935635));
#179494=CARTESIAN_POINT('Ctrl Pts',(17.4439818599249,-20.6306016164573,
17.1744763053273));
#179495=CARTESIAN_POINT('Ctrl Pts',(17.4339379676857,-20.6228347964638,
17.1752227885969));
#179496=CARTESIAN_POINT('Ctrl Pts',(17.3996937386464,-20.5958583930604,
17.1777679174922));
#179497=CARTESIAN_POINT('Ctrl Pts',(17.3758434070302,-20.5762088770927,
17.1795406027697));
#179498=CARTESIAN_POINT('Ctrl Pts',(17.2566649370767,-20.4735599519278,
17.1884481052951));
#179499=CARTESIAN_POINT('Ctrl Pts',(17.168471074874,-20.3826599018042,17.1952181982076));
#179500=CARTESIAN_POINT('Ctrl Pts',(17.0582611819491,-20.2465885634445,
17.2047514608429));
#179501=CARTESIAN_POINT('Ctrl Pts',(17.0289287054711,-20.2077037028477,
17.207414428955));
#179502=CARTESIAN_POINT('Ctrl Pts',(16.9490752892469,-20.0938823813317,
17.2151111645563));
#179503=CARTESIAN_POINT('Ctrl Pts',(16.9019802721141,-20.0166841986583,
17.2202202571225));
#179504=CARTESIAN_POINT('Ctrl Pts',(16.8535788962364,-19.9245707345212,
17.2263207580136));
#179505=CARTESIAN_POINT('Ctrl Pts',(16.8473133867772,-19.9123598134969,
17.2271294148033));
#179506=CARTESIAN_POINT('Ctrl Pts',(16.8374546784434,-19.8926771824009,
17.2284331886303));
#179507=CARTESIAN_POINT('Ctrl Pts',(16.833785805529,-19.8852436607635,17.2289256531454));
#179508=CARTESIAN_POINT('Ctrl Pts',(16.8273484107973,-19.8720054750239,
17.2298028772209));
#179509=CARTESIAN_POINT('Ctrl Pts',(16.8245624875533,-19.866209353122,17.2301870246928));
#179510=CARTESIAN_POINT('Ctrl Pts',(16.8188122844454,-19.8541050898976,
17.2309894394178));
#179511=CARTESIAN_POINT('Ctrl Pts',(16.8158526654903,-19.8477948316081,
17.231407862504));
#179512=CARTESIAN_POINT('Ctrl Pts',(16.8082461371726,-19.8313662678132,
17.2324975416901));
#179513=CARTESIAN_POINT('Ctrl Pts',(16.8036478411164,-19.8212258098082,
17.2331704632612));
#179514=CARTESIAN_POINT('Ctrl Pts',(16.784012823794,-19.7770011164761,17.2361069458593));
#179515=CARTESIAN_POINT('Ctrl Pts',(16.7697980192573,-19.7425612764889,
17.2383983247988));
#179516=CARTESIAN_POINT('Ctrl Pts',(16.7344380958012,-19.6500402388165,
17.2445700205905));
#179517=CARTESIAN_POINT('Ctrl Pts',(16.7149163225501,-19.5913809174453,
17.2485002146646));
#179518=CARTESIAN_POINT('Ctrl Pts',(16.6441980815093,-19.3431153339715,
17.2651780990222));
#179519=CARTESIAN_POINT('Ctrl Pts',(16.6169468519359,-19.1477387709714,
17.2785137881608));
#179520=CARTESIAN_POINT('Ctrl Pts',(16.6170000778107,-18.9514260221329,
17.2909082085163));
#179521=CARTESIAN_POINT('Ctrl Pts',(16.6170000784481,-18.9514236762823,
17.290908356624));
#179522=CARTESIAN_POINT('Ctrl Pts',(16.6170043638442,-18.9356822047961,
17.2919022109546));
#179523=CARTESIAN_POINT('Ctrl Pts',(16.6171842237133,-18.9199407054316,
17.292888940478));
#179524=CARTESIAN_POINT('Ctrl Pts',(16.6177851449884,-18.8933322805094,
17.2945431869397));
#179525=CARTESIAN_POINT('Ctrl Pts',(16.6181143695764,-18.8824642249398,
17.2952149993387));
#179526=CARTESIAN_POINT('Ctrl Pts',(16.6187085001638,-18.8668317574946,
17.2961753157442));
#179527=CARTESIAN_POINT('Ctrl Pts',(16.6189057980431,-18.8620651532563,
17.2964673281209));
#179528=CARTESIAN_POINT('Ctrl Pts',(16.6192791185133,-18.8537280713092,
17.2969766202679));
#179529=CARTESIAN_POINT('Ctrl Pts',(16.6194480741293,-18.8501573184082,
17.2971942817453));
#179530=CARTESIAN_POINT('Ctrl Pts',(16.6197955281146,-18.8431880877566,
17.2976181686609));
#179531=CARTESIAN_POINT('Ctrl Pts',(16.6199731786413,-18.8397895708806,
17.297824440825));
#179532=CARTESIAN_POINT('Ctrl Pts',(16.620344944467,-18.832992030622,17.2982361298109));
#179533=CARTESIAN_POINT('Ctrl Pts',(16.6205390638674,-18.8295930460491,
17.2984415466401));
#179534=CARTESIAN_POINT('Ctrl Pts',(16.6210263182057,-18.8214082324557,
17.2989351641012));
#179535=CARTESIAN_POINT('Ctrl Pts',(16.6213275158666,-18.8166228766968,
17.2992229156209));
#179536=CARTESIAN_POINT('Ctrl Pts',(16.6224923795772,-18.7990673690464,
17.300275579228));
#179537=CARTESIAN_POINT('Ctrl Pts',(16.6234556132615,-18.7863038009819,
17.3010351230314));
#179538=CARTESIAN_POINT('Ctrl Pts',(16.6267051710482,-18.7478907611317,
17.3033056967415));
#179539=CARTESIAN_POINT('Ctrl Pts',(16.6293438413026,-18.7222726522791,
17.3047993492989));
#179540=CARTESIAN_POINT('Ctrl Pts',(16.6519756108748,-18.5359691574001,
17.3155522149559));
#179541=CARTESIAN_POINT('Ctrl Pts',(16.6898786703323,-18.3779977387511,
17.324109604356));
#179542=CARTESIAN_POINT('Ctrl Pts',(16.7454193703768,-18.2258897607889,
17.3329785739071));
#179543=CARTESIAN_POINT('Origin',(18.734,-18.952,0.));
#179544=CARTESIAN_POINT('',(16.7454193588142,-18.2258897924551,18.356854558525));
#179545=CARTESIAN_POINT('',(16.7454193851305,-18.225889720383,18.1318062882837));
#179546=CARTESIAN_POINT('',(16.7454193692319,-18.2258897639242,0.));
#179547=CARTESIAN_POINT('Ctrl Pts',(16.7454193588142,-18.2258897924551,
18.356854558525));
#179548=CARTESIAN_POINT('Ctrl Pts',(16.7400764561234,-18.2405222721369,
18.3558520701171));
#179549=CARTESIAN_POINT('Ctrl Pts',(16.7348944425785,-18.2552154073299,
18.35484548685));
#179550=CARTESIAN_POINT('Ctrl Pts',(16.6860061191413,-18.3988716263901,
18.3450068903525));
#179551=CARTESIAN_POINT('Ctrl Pts',(16.6546780349517,-18.5317066270795,
18.3359031807386));
#179552=CARTESIAN_POINT('Ctrl Pts',(16.6262469177696,-18.7406855078547,
18.3221216440023));
#179553=CARTESIAN_POINT('Ctrl Pts',(16.6200989575309,-18.8152457073574,
18.3173148331482));
#179554=CARTESIAN_POINT('Ctrl Pts',(16.6176490865155,-18.8988371634596,
18.3121557706889));
#179555=CARTESIAN_POINT('Ctrl Pts',(16.6174451484326,-18.9076937611231,
18.3116120637845));
#179556=CARTESIAN_POINT('Ctrl Pts',(16.6172222392193,-18.9210041511307,
18.3107995602777));
#179557=CARTESIAN_POINT('Ctrl Pts',(16.6171617203416,-18.9254570198558,
18.3105285218209));
#179558=CARTESIAN_POINT('Ctrl Pts',(16.6170816556373,-18.933129653031,18.3100628795151));
#179559=CARTESIAN_POINT('Ctrl Pts',(16.6170554040053,-18.9363492920891,
18.3098679033127));
#179560=CARTESIAN_POINT('Ctrl Pts',(16.6170125976594,-18.943639116196,18.3094273992575));
#179561=CARTESIAN_POINT('Ctrl Pts',(16.6170004354112,-18.9477092868115,
18.3091821201468));
#179562=CARTESIAN_POINT('Ctrl Pts',(16.6169992761218,-18.9588398470706,
18.3085131347873));
#179563=CARTESIAN_POINT('Ctrl Pts',(16.6170338608354,-18.9659002604124,
18.3080907283311));
#179564=CARTESIAN_POINT('Ctrl Pts',(16.6174008059016,-19.0029597443722,
18.3058831704996));
#179565=CARTESIAN_POINT('Ctrl Pts',(16.6183355231144,-19.0329510574179,
18.3041297180233));
#179566=CARTESIAN_POINT('Ctrl Pts',(16.6230423596418,-19.1226663565822,
18.2989567809465));
#179567=CARTESIAN_POINT('Ctrl Pts',(16.6287092893136,-19.1822633632961,
18.2956161958563));
#179568=CARTESIAN_POINT('Ctrl Pts',(16.6597465950646,-19.4070599465742,
18.2831216880128));
#179569=CARTESIAN_POINT('Ctrl Pts',(16.7021117943599,-19.5692828192729,
18.274274328893));
#179570=CARTESIAN_POINT('Ctrl Pts',(16.7847365639451,-19.7799918556394,
18.2615097814227));
#179571=CARTESIAN_POINT('Ctrl Pts',(16.8086669656977,-19.8342075908473,
18.2581084339116));
#179572=CARTESIAN_POINT('Ctrl Pts',(16.840246159529,-19.898327240206,18.2539094836516));
#179573=CARTESIAN_POINT('Ctrl Pts',(16.8457498264668,-19.9092617858095,
18.2531871018665));
#179574=CARTESIAN_POINT('Ctrl Pts',(16.8549745014493,-19.9272000109042,
18.251991292269));
#179575=CARTESIAN_POINT('Ctrl Pts',(16.8586406286716,-19.9342316993587,
18.2515197954675));
#179576=CARTESIAN_POINT('Ctrl Pts',(16.865323900166,-19.946876496004,18.2506668833291));
#179577=CARTESIAN_POINT('Ctrl Pts',(16.868327058848,-19.9524969183725,18.2502859672664));
#179578=CARTESIAN_POINT('Ctrl Pts',(16.8748002255645,-19.9644809801034,
18.2494698479992));
#179579=CARTESIAN_POINT('Ctrl Pts',(16.8782776236858,-19.9708405156567,
18.2490343845758));
#179580=CARTESIAN_POINT('Ctrl Pts',(16.8877882472654,-19.9880235085378,
18.2478512706386));
#179581=CARTESIAN_POINT('Ctrl Pts',(16.8938838843996,-19.9988119301249,
18.24710138825));
#179582=CARTESIAN_POINT('Ctrl Pts',(16.9256761857397,-20.0539440310081,
18.2432323067795));
#179583=CARTESIAN_POINT('Ctrl Pts',(16.9528804660932,-20.0973943243011,
18.2400587086051));
#179584=CARTESIAN_POINT('Ctrl Pts',(17.0774362911812,-20.2811502978823,
18.2260766991341));
#179585=CARTESIAN_POINT('Ctrl Pts',(17.1899783146709,-20.4103635560819,
18.2147047805777));
#179586=CARTESIAN_POINT('Ctrl Pts',(17.3851539398323,-20.5862502501211,
18.1974264899812));
#179587=CARTESIAN_POINT('Ctrl Pts',(17.4574774253475,-20.643346703788,18.1914504276524));
#179588=CARTESIAN_POINT('Ctrl Pts',(17.5412586625768,-20.701042761103,18.1851656348704));
#179589=CARTESIAN_POINT('Ctrl Pts',(17.5492592032924,-20.7064719236629,
18.1845715961144));
#179590=CARTESIAN_POINT('Ctrl Pts',(17.5611326974641,-20.7144110141467,
18.1836993211302));
#179591=CARTESIAN_POINT('Ctrl Pts',(17.5649769819699,-20.7169633073778,
18.183418336287));
#179592=CARTESIAN_POINT('Ctrl Pts',(17.5718145255215,-20.7214707413266,
18.1829211495414));
#179593=CARTESIAN_POINT('Ctrl Pts',(17.5748044194671,-20.7234308872347,
18.1827046145));
#179594=CARTESIAN_POINT('Ctrl Pts',(17.5812240289241,-20.7276163083607,
18.1822415689968));
#179595=CARTESIAN_POINT('Ctrl Pts',(17.5846552194365,-20.7298392194033,
18.1819952159324));
#179596=CARTESIAN_POINT('Ctrl Pts',(17.5940985110213,-20.7359183305948,
18.1813202637702));
#179597=CARTESIAN_POINT('Ctrl Pts',(17.6001237855358,-20.7397541073622,
18.1808930036154));
#179598=CARTESIAN_POINT('Ctrl Pts',(17.6325054773727,-20.7601391942149,
18.1786142384344));
#179599=CARTESIAN_POINT('Ctrl Pts',(17.6592064858268,-20.7761372377348,
18.1767969117996));
#179600=CARTESIAN_POINT('Ctrl Pts',(17.8286695253085,-20.8726583177353,
18.1655817017695));
#179601=CARTESIAN_POINT('Ctrl Pts',(17.9800402216489,-20.9369706988151,
18.1569209978717));
#179602=CARTESIAN_POINT('Ctrl Pts',(18.2497879157544,-21.0162106765199,
18.1415316232652));
#179603=CARTESIAN_POINT('Ctrl Pts',(18.3647797420225,-21.0398453399555,
18.1349895654155));
#179604=CARTESIAN_POINT('Ctrl Pts',(18.4953200974181,-21.0555506284855,
18.1272869755072));
#179605=CARTESIAN_POINT('Ctrl Pts',(18.5095292563648,-21.0571142992307,
18.1264451805726));
#179606=CARTESIAN_POINT('Ctrl Pts',(18.5321672418979,-21.0593737314639,
18.1250982272442));
#179607=CARTESIAN_POINT('Ctrl Pts',(18.5405864377595,-21.0601631096962,
18.1245960126324));
#179608=CARTESIAN_POINT('Ctrl Pts',(18.5554424106275,-21.0614662549967,
18.1237075023239));
#179609=CARTESIAN_POINT('Ctrl Pts',(18.5618772682622,-21.062001056276,18.1233218731251));
#179610=CARTESIAN_POINT('Ctrl Pts',(18.5751908607504,-21.0630462416032,
18.1225223782265));
#179611=CARTESIAN_POINT('Ctrl Pts',(18.5820698370767,-21.0635524622274,
18.1221083864093));
#179612=CARTESIAN_POINT('Ctrl Pts',(18.5997320080844,-21.0647654584667,
18.1210430678004));
#179613=CARTESIAN_POINT('Ctrl Pts',(18.6105182650633,-21.0654232965734,
18.1203902125689));
#179614=CARTESIAN_POINT('Ctrl Pts',(18.6555453131005,-21.0678235566071,
18.1176551284641));
#179615=CARTESIAN_POINT('Ctrl Pts',(18.6898192841759,-21.0688165506296,
18.1155495890787));
#179616=CARTESIAN_POINT('Ctrl Pts',(18.7791606103171,-21.0692343218607,
18.1099963704284));
#179617=CARTESIAN_POINT('Ctrl Pts',(18.8342054418855,-21.0673436375107,
18.1065103274133));
#179618=CARTESIAN_POINT('Ctrl Pts',(18.9981749486223,-21.05529737631,18.09594279428));
#179619=CARTESIAN_POINT('Ctrl Pts',(19.1064471683049,-21.0388463998676,
18.0887129066814));
#179620=CARTESIAN_POINT('Ctrl Pts',(19.2565111520279,-21.0039918660478,
18.0785361397149));
#179621=CARTESIAN_POINT('Ctrl Pts',(19.2997372543213,-20.9924975024954,
18.0755876314039));
#179622=CARTESIAN_POINT('Ctrl Pts',(19.3667237620158,-20.9723924665874,
18.071017384995));
#179623=CARTESIAN_POINT('Ctrl Pts',(19.3907490064471,-20.9647110799636,
18.0693780886127));
#179624=CARTESIAN_POINT('Ctrl Pts',(19.461861411588,-20.9405659528622,18.0645357239251));
#179625=CARTESIAN_POINT('Ctrl Pts',(19.5085137468885,-20.9228643042607,
18.0613716945036));
#179626=CARTESIAN_POINT('Ctrl Pts',(19.5617050572443,-20.9005005550611,
18.0578132669912));
#179627=CARTESIAN_POINT('Ctrl Pts',(19.568892553094,-20.8974317011809,18.0573334962332));
#179628=CARTESIAN_POINT('Ctrl Pts',(19.5803423593787,-20.8924678212796,
18.0565711066511));
#179629=CARTESIAN_POINT('Ctrl Pts',(19.584615607449,-20.8905984225786,18.0562869942557));
#179630=CARTESIAN_POINT('Ctrl Pts',(19.5921674256897,-20.8872649847555,
18.0557856979716));
#179631=CARTESIAN_POINT('Ctrl Pts',(19.5954484924717,-20.8858067088761,
18.055568166356));
#179632=CARTESIAN_POINT('Ctrl Pts',(19.6023887945438,-20.8827009103173,
18.0551086141341));
#179633=CARTESIAN_POINT('Ctrl Pts',(19.6060470528497,-20.8810513320856,
18.0548667219678));
#179634=CARTESIAN_POINT('Ctrl Pts',(19.6158937875347,-20.8765775173519,
18.0542164921772));
#179635=CARTESIAN_POINT('Ctrl Pts',(19.6220734394534,-20.8737338113788,
18.0538093345541));
#179636=CARTESIAN_POINT('Ctrl Pts',(19.6524932152291,-20.8595573958998,
18.0518090854611));
#179637=CARTESIAN_POINT('Ctrl Pts',(19.6765318660155,-20.8477950409794,
18.0502410366366));
#179638=CARTESIAN_POINT('Ctrl Pts',(19.7451561995693,-20.81258835296,18.0457830247411));
#179639=CARTESIAN_POINT('Ctrl Pts',(19.7891384359692,-20.7880036592014,
18.0429484655315));
#179640=CARTESIAN_POINT('Ctrl Pts',(19.9451426672729,-20.6933425118803,
18.0328291654504));
#179641=CARTESIAN_POINT('Ctrl Pts',(20.0514209257145,-20.6143913048451,
18.0257917938663));
#179642=CARTESIAN_POINT('Ctrl Pts',(20.2269455796162,-20.456529724716,18.0128052365207));
#179643=CARTESIAN_POINT('Ctrl Pts',(20.2990060227302,-20.381422366323,18.0069649199435));
#179644=CARTESIAN_POINT('Ctrl Pts',(20.3742145569046,-20.2905002207869,
18.0000501829558));
#179645=CARTESIAN_POINT('Ctrl Pts',(20.3830666934791,-20.2795788714724,
17.999222132289));
#179646=CARTESIAN_POINT('Ctrl Pts',(20.3970253758706,-20.2620022698628,
17.9978930734479));
#179647=CARTESIAN_POINT('Ctrl Pts',(20.4022023703073,-20.2554033130414,
17.9973948865358));
#179648=CARTESIAN_POINT('Ctrl Pts',(20.4112884544689,-20.2436787491711,
17.9965110564187));
#179649=CARTESIAN_POINT('Ctrl Pts',(20.4152136257635,-20.2385656973833,
17.9961260571739));
#179650=CARTESIAN_POINT('Ctrl Pts',(20.4233078818155,-20.2279215704402,
17.9953254445956));
#179651=CARTESIAN_POINT('Ctrl Pts',(20.4274732910753,-20.2223878085526,
17.9949096931681));
#179652=CARTESIAN_POINT('Ctrl Pts',(20.4381457778705,-20.2080636054719,
17.9938346876592));
#179653=CARTESIAN_POINT('Ctrl Pts',(20.4446119661486,-20.1992430827485,
17.9931738511512));
#179654=CARTESIAN_POINT('Ctrl Pts',(20.4717394018219,-20.1616307773585,
17.9903603677151));
#179655=CARTESIAN_POINT('Ctrl Pts',(20.4917433502846,-20.1323740603814,
17.988182706553));
#179656=CARTESIAN_POINT('Ctrl Pts',(20.5423282426543,-20.0542521105974,
17.982392237566));
#179657=CARTESIAN_POINT('Ctrl Pts',(20.5716626651955,-20.0046185190729,
17.9787368537524));
#179658=CARTESIAN_POINT('Ctrl Pts',(20.6747978948891,-19.812633956754,17.9647006140863));
#179659=CARTESIAN_POINT('Ctrl Pts',(20.7343682062156,-19.6632713748046,
17.9539384240938));
#179660=CARTESIAN_POINT('Ctrl Pts',(20.7802679302856,-19.4948449269851,
17.9425841917919));
#179661=CARTESIAN_POINT('Ctrl Pts',(20.7838843496348,-19.4810247860628,
17.941658449567));
#179662=CARTESIAN_POINT('Ctrl Pts',(20.7893293716988,-19.4593220110097,
17.9402149344421));
#179663=CARTESIAN_POINT('Ctrl Pts',(20.7912531015821,-19.4514638405245,
17.9396943574825));
#179664=CARTESIAN_POINT('Ctrl Pts',(20.8031618681265,-19.4015818605624,
17.9364038514231));
#179665=CARTESIAN_POINT('Ctrl Pts',(20.8119046449392,-19.3592684119933,
17.9336753441514));
#179666=CARTESIAN_POINT('Ctrl Pts',(20.8206391076489,-19.3093268433427,
17.9305508082306));
#179667=CARTESIAN_POINT('Ctrl Pts',(20.8218918270728,-19.3019327947099,
17.9300906599337));
#179668=CARTESIAN_POINT('Ctrl Pts',(20.8238528448074,-19.2899725369792,
17.9293504768193));
#179669=CARTESIAN_POINT('Ctrl Pts',(20.8245855183514,-19.2854104678857,
17.9290691139141));
#179670=CARTESIAN_POINT('Ctrl Pts',(20.8258587018256,-19.2773136296906,
17.9285715093585));
#179671=CARTESIAN_POINT('Ctrl Pts',(20.8264051975035,-19.2737798567443,
17.9283549324757));
#179672=CARTESIAN_POINT('Ctrl Pts',(20.8275567517551,-19.2662066352444,
17.9278920752393));
#179673=CARTESIAN_POINT('Ctrl Pts',(20.8281590729452,-19.2621668265642,
17.9276459508316));
#179674=CARTESIAN_POINT('Ctrl Pts',(20.8297799980859,-19.2510751824092,
17.9269722700017));
#179675=CARTESIAN_POINT('Ctrl Pts',(20.8307747101782,-19.2440198334942,
17.9265460441383));
#179676=CARTESIAN_POINT('Ctrl Pts',(20.8358902188534,-19.2063619344694,
17.9242826813485));
#179677=CARTESIAN_POINT('Ctrl Pts',(20.8393769454466,-19.1756752769556,
17.9224791780782));
#179678=CARTESIAN_POINT('Ctrl Pts',(20.8478921652947,-19.0826234025755,
17.9171042078029));
#179679=CARTESIAN_POINT('Ctrl Pts',(20.8508293052481,-19.020098421261,17.9136190929229));
#179680=CARTESIAN_POINT('Ctrl Pts',(20.8513435470224,-18.8232739646198,
17.9028009703775));
#179681=CARTESIAN_POINT('Ctrl Pts',(20.838922338549,-18.689289591568,17.8956413110103));
#179682=CARTESIAN_POINT('Ctrl Pts',(20.8063008072433,-18.5173525007892,
17.885930685782));
#179683=CARTESIAN_POINT('Ctrl Pts',(20.7975521954345,-18.4775517128178,
17.8836471978451));
#179684=CARTESIAN_POINT('Ctrl Pts',(20.7757746400694,-18.3905355966297,
17.8785505438787));
#179685=CARTESIAN_POINT('Ctrl Pts',(20.7622451211399,-18.3434713306558,
17.8757248687069));
#179686=CARTESIAN_POINT('Ctrl Pts',(20.7431874442101,-18.284905961505,17.872102839793));
#179687=CARTESIAN_POINT('Ctrl Pts',(20.7391702955488,-18.272926574217,17.8713563295306));
#179688=CARTESIAN_POINT('Ctrl Pts',(20.7326385841842,-18.2540120232031,
17.8701684105764));
#179689=CARTESIAN_POINT('Ctrl Pts',(20.7301945530111,-18.2470526896566,
17.8697293400971));
#179690=CARTESIAN_POINT('Ctrl Pts',(20.7255751912979,-18.2341158036487,
17.8689093634801));
#179691=CARTESIAN_POINT('Ctrl Pts',(20.7234091864662,-18.2281349922804,
17.8685287715346));
#179692=CARTESIAN_POINT('Ctrl Pts',(20.7185415086301,-18.2148811520463,
17.8676819566234));
#179693=CARTESIAN_POINT('Ctrl Pts',(20.7158267510827,-18.2076130564834,
17.8672153003799));
#179694=CARTESIAN_POINT('Ctrl Pts',(20.7078319260588,-18.1865626361052,
17.8658570104972));
#179695=CARTESIAN_POINT('Ctrl Pts',(20.7024476855498,-18.1728206096663,
17.8649618939631));
#179696=CARTESIAN_POINT('Ctrl Pts',(20.6590069999302,-18.0652729936997,
17.8578889607705));
#179697=CARTESIAN_POINT('Ctrl Pts',(20.6144157506655,-17.9742637670155,
17.8514877320934));
#179698=CARTESIAN_POINT('Ctrl Pts',(20.4930092039418,-17.765746095288,17.8358363724378));
#179699=CARTESIAN_POINT('Ctrl Pts',(20.4106900314191,-17.6519928230237,
17.8264608633022));
#179700=CARTESIAN_POINT('Ctrl Pts',(20.3067311664855,-17.5347910863474,
17.8162460962281));
#179701=CARTESIAN_POINT('Ctrl Pts',(20.2955726167858,-17.5225051906479,
17.8151681766725));
#179702=CARTESIAN_POINT('Ctrl Pts',(20.2480212819138,-17.4713710638967,
17.8106556317554));
#179703=CARTESIAN_POINT('Ctrl Pts',(20.2103112464261,-17.4337679284982,
17.8072720231526));
#179704=CARTESIAN_POINT('Ctrl Pts',(20.164822881924,-17.391708104282,17.8034503206394));
#179705=CARTESIAN_POINT('Ctrl Pts',(20.1583887795724,-17.3858322152769,
17.8029155386089));
#179706=CARTESIAN_POINT('Ctrl Pts',(20.148590524906,-17.3769943706839,17.8021100935373));
#179707=CARTESIAN_POINT('Ctrl Pts',(20.1452530339559,-17.3740031810754,
17.801837297632));
#179708=CARTESIAN_POINT('Ctrl Pts',(20.1392445749264,-17.3686524748473,
17.8013490110623));
#179709=CARTESIAN_POINT('Ctrl Pts',(20.1365771372497,-17.3662890946283,
17.8011332327703));
#179710=CARTESIAN_POINT('Ctrl Pts',(20.130767376258,-17.3611677094757,17.8006654229155));
#179711=CARTESIAN_POINT('Ctrl Pts',(20.1276228571509,-17.3584122827174,
17.8004135827683));
#179712=CARTESIAN_POINT('Ctrl Pts',(20.1187653325902,-17.3506970270839,
17.7997079411251));
#179713=CARTESIAN_POINT('Ctrl Pts',(20.1130338065887,-17.3457584236439,
17.7992556880434));
#179714=CARTESIAN_POINT('Ctrl Pts',(20.0785729936607,-17.3163854799728,
17.7965615891902));
#179715=CARTESIAN_POINT('Ctrl Pts',(20.0492194797488,-17.2926900501522,
17.7943703755856));
#179716=CARTESIAN_POINT('Ctrl Pts',(19.9504458439372,-17.2172247554472,
17.7872726040437));
#179717=CARTESIAN_POINT('Ctrl Pts',(19.8784794425841,-17.1689254594074,
17.7825305768209));
#179718=CARTESIAN_POINT('Ctrl Pts',(19.6518050088679,-17.0361900637981,
17.7682366619213));
#179719=CARTESIAN_POINT('Ctrl Pts',(19.4893704272039,-16.9665271114053,
17.7587731110688));
#179720=CARTESIAN_POINT('Ctrl Pts',(19.2981408099133,-16.9114214610588,
17.7472083749291));
#179721=CARTESIAN_POINT('Ctrl Pts',(19.2759885527132,-16.9054262839702,
17.745863894274));
#179722=CARTESIAN_POINT('Ctrl Pts',(19.2444966582213,-16.8974506195116,
17.7439440442451));
#179723=CARTESIAN_POINT('Ctrl Pts',(19.2352338795538,-16.8951712301748,
17.7433783224094));
#179724=CARTESIAN_POINT('Ctrl Pts',(19.2201538561888,-16.8915682451773,
17.7424555202888));
#179725=CARTESIAN_POINT('Ctrl Pts',(19.2143457991763,-16.890206484572,17.7420996732026));
#179726=CARTESIAN_POINT('Ctrl Pts',(19.2021723961485,-16.8874065307825,
17.7413529006346));
#179727=CARTESIAN_POINT('Ctrl Pts',(19.1958060094738,-16.8859731865765,
17.740961823602));
#179728=CARTESIAN_POINT('Ctrl Pts',(19.1806378159044,-16.8826317936806,
17.7400287516068));
#179729=CARTESIAN_POINT('Ctrl Pts',(19.1718303136823,-16.8807504437117,
17.7394859070532));
#179730=CARTESIAN_POINT('Ctrl Pts',(19.1420842674372,-16.8745946660899,
17.7376488428849));
#179731=CARTESIAN_POINT('Ctrl Pts',(19.1210936109959,-16.8705812111768,
17.7363463344652));
#179732=CARTESIAN_POINT('Ctrl Pts',(19.0709954331502,-16.8617863637605,
17.7332220376431));
#179733=CARTESIAN_POINT('Ctrl Pts',(19.0418422794558,-16.8572943016439,
17.7313914479273));
#179734=CARTESIAN_POINT('Ctrl Pts',(18.8436279823292,-16.8309796108381,
17.7188582851884));
#179735=CARTESIAN_POINT('Ctrl Pts',(18.6725798007028,-16.8290408593784,
17.7075426535115));
#179736=CARTESIAN_POINT('Ctrl Pts',(18.4039839765343,-16.8585009795282,
17.689739829831));
#179737=CARTESIAN_POINT('Ctrl Pts',(18.3056615492848,-16.876384518382,17.683234611176));
#179738=CARTESIAN_POINT('Ctrl Pts',(18.1995667849229,-16.9035459200741,
17.6764681908364));
#179739=CARTESIAN_POINT('Ctrl Pts',(18.1901918094478,-16.9060147510222,
17.6758725433633));
#179740=CARTESIAN_POINT('Ctrl Pts',(18.1763750406761,-16.9097549747216,
17.6749983664912));
#179741=CARTESIAN_POINT('Ctrl Pts',(18.1719200731995,-16.9109766058771,
17.6747170715071));
#179742=CARTESIAN_POINT('Ctrl Pts',(18.1640238597279,-16.9131697018239,
17.6742195420543));
#179743=CARTESIAN_POINT('Ctrl Pts',(18.1605810440586,-16.9141353119289,
17.6740029727291));
#179744=CARTESIAN_POINT('Ctrl Pts',(18.1532100918069,-16.9162228091859,
17.6735400818566));
#179745=CARTESIAN_POINT('Ctrl Pts',(18.1492827620527,-16.9173473415853,
17.6732939165151));
#179746=CARTESIAN_POINT('Ctrl Pts',(18.1385116718984,-16.9204652449808,
17.6726200081316));
#179747=CARTESIAN_POINT('Ctrl Pts',(18.1316746130291,-16.9224818450536,
17.6721935971473));
#179748=CARTESIAN_POINT('Ctrl Pts',(18.0952336816106,-16.933430518794,17.6699274868392));
#179749=CARTESIAN_POINT('Ctrl Pts',(18.0658163244966,-16.9429763658007,
17.6681215180021));
#179750=CARTESIAN_POINT('Ctrl Pts',(17.9774217710695,-16.9738167432209,
17.6627364893235));
#179751=CARTESIAN_POINT('Ctrl Pts',(17.9191687176525,-16.997090604706,17.6592441620421));
#179752=CARTESIAN_POINT('Ctrl Pts',(17.7219681153042,-17.0862277143227,
17.647350561704));
#179753=CARTESIAN_POINT('Ctrl Pts',(17.5892207147139,-17.1646008704155,
17.6391831950194));
#179754=CARTESIAN_POINT('Ctrl Pts',(17.4622383317729,-17.2595654092346,
17.6302908518846));
#179755=CARTESIAN_POINT('Ctrl Pts',(17.4583592365505,-17.2624872811987,
17.6300181201842));
#179756=CARTESIAN_POINT('Ctrl Pts',(17.4040578853205,-17.3036826054145,
17.6261847470864));
#179757=CARTESIAN_POINT('Ctrl Pts',(17.3553710716627,-17.3441824037655,
17.6225575686703));
#179758=CARTESIAN_POINT('Ctrl Pts',(17.2993260861164,-17.3952224825379,
17.6181059983586));
#179759=CARTESIAN_POINT('Ctrl Pts',(17.2901524789185,-17.4037268316399,
17.6173680341071));
#179760=CARTESIAN_POINT('Ctrl Pts',(17.2752275868538,-17.4178108839172,
17.6161517061893));
#179761=CARTESIAN_POINT('Ctrl Pts',(17.2694315774682,-17.4233428997032,
17.6156753909468));
#179762=CARTESIAN_POINT('Ctrl Pts',(17.2590771665387,-17.433338636389,17.6148172408564));
#179763=CARTESIAN_POINT('Ctrl Pts',(17.254507253845,-17.4377903333131,17.6144359323341));
#179764=CARTESIAN_POINT('Ctrl Pts',(17.2456933740911,-17.4464542051588,
17.6136954856038));
#179765=CARTESIAN_POINT('Ctrl Pts',(17.24144698857,-17.450663841767,17.6133364610283));
#179766=CARTESIAN_POINT('Ctrl Pts',(17.2299424509366,-17.4621658654195,
17.6123574797289));
#179767=CARTESIAN_POINT('Ctrl Pts',(17.2227196055798,-17.4694931962907,
17.6117359722909));
#179768=CARTESIAN_POINT('Ctrl Pts',(17.1934253779375,-17.4996477505744,
17.6091867183149));
#179769=CARTESIAN_POINT('Ctrl Pts',(17.1718164019722,-17.5229165675612,
17.6072390961125));
#179770=CARTESIAN_POINT('Ctrl Pts',(17.1176161436062,-17.5839788094522,
17.6021745282846));
#179771=CARTESIAN_POINT('Ctrl Pts',(17.0858244741928,-17.622452872298,17.5990267722717));
#179772=CARTESIAN_POINT('Ctrl Pts',(17.0102418961657,-17.7208034929502,
17.5910887415768));
#179773=CARTESIAN_POINT('Ctrl Pts',(16.9681834221041,-17.7819242594128,
17.586247892214));
#179774=CARTESIAN_POINT('Ctrl Pts',(16.855520092246,-17.9656028583405,17.5720554976599));
#179775=CARTESIAN_POINT('Ctrl Pts',(16.7938830445993,-18.0931634557097,
17.5626092881251));
#179776=CARTESIAN_POINT('Ctrl Pts',(16.7454193574352,-18.2258897962317,
17.5536949220328));
#179777=CARTESIAN_POINT('Ctrl Pts',(16.7454193703768,-18.2258897607889,
17.3329785739071));
#179778=CARTESIAN_POINT('Ctrl Pts',(16.7466515045255,-18.2225153446616,
17.333175326203));
#179779=CARTESIAN_POINT('Ctrl Pts',(16.7478923195581,-18.2191438132461,
17.333372211731));
#179780=CARTESIAN_POINT('Ctrl Pts',(16.7755868005906,-18.1444796378743,
17.3377392514039));
#179781=CARTESIAN_POINT('Ctrl Pts',(16.8058521666827,-18.074665433262,17.3419652870829));
#179782=CARTESIAN_POINT('Ctrl Pts',(16.8590249439553,-17.96812504875,17.3487665315314));
#179783=CARTESIAN_POINT('Ctrl Pts',(16.8794133282801,-17.9302127035193,
17.3512600777808));
#179784=CARTESIAN_POINT('Ctrl Pts',(16.9067979234565,-17.882814048789,17.3544842221763));
#179785=CARTESIAN_POINT('Ctrl Pts',(16.9127377637891,-17.8727271496805,
17.3551766433149));
#179786=CARTESIAN_POINT('Ctrl Pts',(16.9224123738061,-17.8566052618435,
17.3562937204443));
#179787=CARTESIAN_POINT('Ctrl Pts',(16.926094421276,-17.8505387994598,17.3567164491273));
#179788=CARTESIAN_POINT('Ctrl Pts',(16.9331536611214,-17.8390389088988,
17.3575223994155));
#179789=CARTESIAN_POINT('Ctrl Pts',(16.9365251229351,-17.8336020424348,
17.3579054070299));
#179790=CARTESIAN_POINT('Ctrl Pts',(16.944261717024,-17.821251250412,17.3587800270841));
#179791=CARTESIAN_POINT('Ctrl Pts',(16.9486423462773,-17.8143471963686,
17.3592722101097));
#179792=CARTESIAN_POINT('Ctrl Pts',(16.9601171048081,-17.7964920050116,
17.3605537035385));
#179793=CARTESIAN_POINT('Ctrl Pts',(16.9672725992034,-17.7855808936593,
17.3613452949648));
#179794=CARTESIAN_POINT('Ctrl Pts',(17.0151698612886,-17.7139963283021,
17.3665957660338));
#179795=CARTESIAN_POINT('Ctrl Pts',(17.0589249661821,-17.6554076387175,
17.3711685695935));
#179796=CARTESIAN_POINT('Ctrl Pts',(17.2322419388608,-17.4467832936557,
17.3885131931583));
#179797=CARTESIAN_POINT('Ctrl Pts',(17.3796158935411,-17.312920191456,17.4019442721551));
#179798=CARTESIAN_POINT('Ctrl Pts',(17.5667165808522,-17.1856672732093,
17.4164433210276));
#179799=CARTESIAN_POINT('Ctrl Pts',(17.5903146959775,-17.1702968927357,
17.4182290118084));
#179800=CARTESIAN_POINT('Ctrl Pts',(17.6243045917675,-17.1491116261031,
17.4207331565202));
#179801=CARTESIAN_POINT('Ctrl Pts',(17.6344487020055,-17.1429070380755,
17.4214720965235));
#179802=CARTESIAN_POINT('Ctrl Pts',(17.6501569297104,-17.1334801278939,
17.4226028199757));
#179803=CARTESIAN_POINT('Ctrl Pts',(17.6556841793829,-17.1301972336046,
17.4229981334577));
#179804=CARTESIAN_POINT('Ctrl Pts',(17.664878208137,-17.1247929680169,17.4236513618647));
#179805=CARTESIAN_POINT('Ctrl Pts',(17.6685365104961,-17.1226573593757,
17.4239101495242));
#179806=CARTESIAN_POINT('Ctrl Pts',(17.6756376041958,-17.1185404785403,
17.4244102530051));
#179807=CARTESIAN_POINT('Ctrl Pts',(17.6790796072533,-17.116557888886,17.42465165181));
#179808=CARTESIAN_POINT('Ctrl Pts',(17.6855404550577,-17.1128606263513,
17.4251028549123));
#179809=CARTESIAN_POINT('Ctrl Pts',(17.6885579020581,-17.1111437119853,
17.4253127990916));
#179810=CARTESIAN_POINT('Ctrl Pts',(17.6955747901981,-17.1071739502924,
17.4257992113402));
#179811=CARTESIAN_POINT('Ctrl Pts',(17.6995773391968,-17.1049266853319,
17.4260753189192));
#179812=CARTESIAN_POINT('Ctrl Pts',(17.7119250203324,-17.0980467001937,
17.426923047579));
#179813=CARTESIAN_POINT('Ctrl Pts',(17.7202943316885,-17.0934573107749,
17.4274919647424));
#179814=CARTESIAN_POINT('Ctrl Pts',(17.8321453290519,-17.0331031169082,
17.4350237496617));
#179815=CARTESIAN_POINT('Ctrl Pts',(17.9400816610013,-16.9859865882986,
17.4414867714133));
#179816=CARTESIAN_POINT('Ctrl Pts',(18.1551743551717,-16.9127177939142,
17.4538602737133));
#179817=CARTESIAN_POINT('Ctrl Pts',(18.2615520578762,-16.88548042931,17.4597628205106));
#179818=CARTESIAN_POINT('Ctrl Pts',(18.4445804020308,-16.8534943880991,
17.4700911316911));
#179819=CARTESIAN_POINT('Ctrl Pts',(18.5202503258121,-16.8444424532063,
17.4744073521615));
#179820=CARTESIAN_POINT('Ctrl Pts',(18.6151569645426,-16.8382533811421,
17.4799597314741));
#179821=CARTESIAN_POINT('Ctrl Pts',(18.6340908163362,-16.8372738815052,
17.4810741218581));
#179822=CARTESIAN_POINT('Ctrl Pts',(18.6616106321383,-16.8362206089504,
17.4827045319267));
#179823=CARTESIAN_POINT('Ctrl Pts',(18.6701882559294,-16.8359445399092,
17.4832142160233));
#179824=CARTESIAN_POINT('Ctrl Pts',(18.6852186295816,-16.8355522621957,
17.4841100475738));
#179825=CARTESIAN_POINT('Ctrl Pts',(18.6916707133093,-16.8354133896715,
17.4844954798152));
#179826=CARTESIAN_POINT('Ctrl Pts',(18.7041920260279,-16.8352011609536,
17.4852452171841));
#179827=CARTESIAN_POINT('Ctrl Pts',(18.7102611399795,-16.8351244000574,
17.485609411694));
#179828=CARTESIAN_POINT('Ctrl Pts',(18.72475721061,-16.8350034043338,17.4864812235093));
#179829=CARTESIAN_POINT('Ctrl Pts',(18.7331842175177,-16.8349833853972,
17.4869895951325));
#179830=CARTESIAN_POINT('Ctrl Pts',(18.763515990459,-16.8350924347028,17.4888251480344));
#179831=CARTESIAN_POINT('Ctrl Pts',(18.7854177358851,-16.8355111638474,
17.4901613522644));
#179832=CARTESIAN_POINT('Ctrl Pts',(18.9947964672482,-16.8427659744034,
17.5030428288233));
#179833=CARTESIAN_POINT('Ctrl Pts',(19.1805560049646,-16.8741544315639,
17.5154073934769));
#179834=CARTESIAN_POINT('Ctrl Pts',(19.4350194118993,-16.9528811045889,
17.5329896172734));
#179835=CARTESIAN_POINT('Ctrl Pts',(19.5089809406485,-16.9803735673585,
17.5381663683722));
#179836=CARTESIAN_POINT('Ctrl Pts',(19.6139340063293,-17.0262072150448,
17.5454645850971));
#179837=CARTESIAN_POINT('Ctrl Pts',(19.6462636334707,-17.0413097797935,
17.5477054087737));
#179838=CARTESIAN_POINT('Ctrl Pts',(19.6848613524739,-17.0605436533822,
17.5503584071934));
#179839=CARTESIAN_POINT('Ctrl Pts',(19.6915070832152,-17.0638992049767,
17.5508143836669));
#179840=CARTESIAN_POINT('Ctrl Pts',(19.7018338065578,-17.0691819037774,
17.5515214844195));
#179841=CARTESIAN_POINT('Ctrl Pts',(19.705526985108,-17.0710849092871,17.5517740793255));
#179842=CARTESIAN_POINT('Ctrl Pts',(19.7123799698784,-17.0746416556055,
17.5522422196273));
#179843=CARTESIAN_POINT('Ctrl Pts',(19.715541168978,-17.076292492791,17.5524579370719));
#179844=CARTESIAN_POINT('Ctrl Pts',(19.7226966992806,-17.0800522875018,
17.5529457159732));
#179845=CARTESIAN_POINT('Ctrl Pts',(19.7266884516894,-17.082166039391,17.553217469976));
#179846=CARTESIAN_POINT('Ctrl Pts',(19.7385050018084,-17.0884717603059,
17.5540209603089));
#179847=CARTESIAN_POINT('Ctrl Pts',(19.74631034441,-17.0927002469667,17.5545504387007));
#179848=CARTESIAN_POINT('Ctrl Pts',(19.8044399739556,-17.1246661156217,
17.5584859616396));
#179849=CARTESIAN_POINT('Ctrl Pts',(19.8536476315465,-17.1543956803151,
17.561774189942));
#179850=CARTESIAN_POINT('Ctrl Pts',(20.037248612114,-17.2757896791421,17.5741112745422));
#179851=CARTESIAN_POINT('Ctrl Pts',(20.1621260780778,-17.3808220014613,
17.582688730169));
#179852=CARTESIAN_POINT('Ctrl Pts',(20.3154026043149,-17.5432636854615,
17.595054128838));
#179853=CARTESIAN_POINT('Ctrl Pts',(20.3551330743223,-17.5891724486943,
17.5984623859429));
#179854=CARTESIAN_POINT('Ctrl Pts',(20.4156835815707,-17.6655390328142,
17.6040575963685));
#179855=CARTESIAN_POINT('Ctrl Pts',(20.4377764966462,-17.6949451493129,
17.6061954618015));
#179856=CARTESIAN_POINT('Ctrl Pts',(20.4655156953497,-17.7339420225283,
17.6090166814668));
#179857=CARTESIAN_POINT('Ctrl Pts',(20.4718688613332,-17.7430237167468,
17.6096727281285));
#179858=CARTESIAN_POINT('Ctrl Pts',(20.4820942338171,-17.7578877892823,
17.6107451127868));
#179859=CARTESIAN_POINT('Ctrl Pts',(20.4860098085027,-17.7636401844462,
17.6111597949147));
#179860=CARTESIAN_POINT('Ctrl Pts',(20.4934913881546,-17.7747487696926,
17.6119600129509));
#179861=CARTESIAN_POINT('Ctrl Pts',(20.497061477942,-17.7801021256826,17.6123453885218));
#179862=CARTESIAN_POINT('Ctrl Pts',(20.5051884284862,-17.7924096946163,
17.6132308327424));
#179863=CARTESIAN_POINT('Ctrl Pts',(20.5097288172126,-17.7993746097782,
17.6137315116673));
#179864=CARTESIAN_POINT('Ctrl Pts',(20.5217003406142,-17.8179774458804,
17.6150678302696));
#179865=CARTESIAN_POINT('Ctrl Pts',(20.529058746483,-17.8296614844087,17.6159061514545));
#179866=CARTESIAN_POINT('Ctrl Pts',(20.5853756301151,-17.9210549176534,
17.6224569015313));
#179867=CARTESIAN_POINT('Ctrl Pts',(20.6291100596633,-18.0038474687044,
17.6283591228187));
#179868=CARTESIAN_POINT('Ctrl Pts',(20.7242878481568,-18.2171191058028,
17.6434622106105));
#179869=CARTESIAN_POINT('Ctrl Pts',(20.7685233588595,-18.3503307934482,
17.6528245653269));
#179870=CARTESIAN_POINT('Ctrl Pts',(20.8108081481427,-18.5381041227205,
17.6654112154109));
#179871=CARTESIAN_POINT('Ctrl Pts',(20.8204287032005,-18.5897046895771,
17.6688053168593));
#179872=CARTESIAN_POINT('Ctrl Pts',(20.8321550558771,-18.6688200752065,
17.6738624423594));
#179873=CARTESIAN_POINT('Ctrl Pts',(20.8356573148347,-18.6961050864414,
17.6755801270848));
#179874=CARTESIAN_POINT('Ctrl Pts',(20.8393681027406,-18.730276579246,17.6776920510488));
#179875=CARTESIAN_POINT('Ctrl Pts',(20.8400760121589,-18.7371047758992,
17.6781121037737));
#179876=CARTESIAN_POINT('Ctrl Pts',(20.8411464659194,-18.7479436695925,
17.6787756540179));
#179877=CARTESIAN_POINT('Ctrl Pts',(20.841530794977,-18.7519520965744,17.6790203472518));
#179878=CARTESIAN_POINT('Ctrl Pts',(20.8422358736238,-18.7595334588964,
17.679481794289));
#179879=CARTESIAN_POINT('Ctrl Pts',(20.842558974962,-18.7631060679842,17.6796986721527));
#179880=CARTESIAN_POINT('Ctrl Pts',(20.8432791355801,-18.7713012097062,
17.6801948741122));
#179881=CARTESIAN_POINT('Ctrl Pts',(20.843670080889,-18.7759242340723,17.6804738523526));
#179882=CARTESIAN_POINT('Ctrl Pts',(20.8446719124212,-18.7882537333393,
17.6812154689609));
#179883=CARTESIAN_POINT('Ctrl Pts',(20.84525579639,-18.7959624145724,17.6816766336076));
#179884=CARTESIAN_POINT('Ctrl Pts',(20.8491537415796,-18.8514596625095,
17.68497974839));
#179885=CARTESIAN_POINT('Ctrl Pts',(20.8508874253925,-18.8993492732169,
17.6877397177811));
#179886=CARTESIAN_POINT('Ctrl Pts',(20.8510584794881,-18.9757496549838,
17.6920566198715));
#179887=CARTESIAN_POINT('Ctrl Pts',(20.8505471657019,-19.0042383898969,
17.6936472203223));
#179888=CARTESIAN_POINT('Ctrl Pts',(20.847800356483,-19.0762349394366,17.6976371171893));
#179889=CARTESIAN_POINT('Ctrl Pts',(20.8447967734533,-19.1197004703986,
17.7000183932679));
#179890=CARTESIAN_POINT('Ctrl Pts',(20.8295552981277,-19.271827811454,17.7083422034416));
#179891=CARTESIAN_POINT('Ctrl Pts',(20.8102457159763,-19.3796034112313,
17.7142292781981));
#179892=CARTESIAN_POINT('Ctrl Pts',(20.7636353481383,-19.5586256004974,
17.7245156238653));
#179893=CARTESIAN_POINT('Ctrl Pts',(20.7406603971605,-19.630768425109,17.7288049481863));
#179894=CARTESIAN_POINT('Ctrl Pts',(20.7071864373007,-19.7191904556225,
17.7343249090456));
#179895=CARTESIAN_POINT('Ctrl Pts',(20.7002616627995,-19.7367680872222,
17.7354354344716));
#179896=CARTESIAN_POINT('Ctrl Pts',(20.689855121965,-19.7621809578871,17.7370612128874));
#179897=CARTESIAN_POINT('Ctrl Pts',(20.6865594278932,-19.7700917551782,
17.7375701815309));
#179898=CARTESIAN_POINT('Ctrl Pts',(20.6806985941754,-19.7839225972379,
17.7384651852554));
#179899=CARTESIAN_POINT('Ctrl Pts',(20.6781542394562,-19.7898513687653,
17.7388505092289));
#179900=CARTESIAN_POINT('Ctrl Pts',(20.6731622762336,-19.8013383011216,
17.739600354872));
#179901=CARTESIAN_POINT('Ctrl Pts',(20.6707177706073,-19.8068977477676,
17.739964767424));
#179902=CARTESIAN_POINT('Ctrl Pts',(20.6648187837648,-19.8201584339587,
17.7408376157691));
#179903=CARTESIAN_POINT('Ctrl Pts',(20.6613421204035,-19.8278496388554,
17.7413468099521));
#179904=CARTESIAN_POINT('Ctrl Pts',(20.6486422351825,-19.8555029966078,
17.7431883536538));
#179905=CARTESIAN_POINT('Ctrl Pts',(20.6391543619873,-19.8753414067305,
17.7445298030286));
#179906=CARTESIAN_POINT('Ctrl Pts',(20.546150700172,-20.0622662882698,17.7573680597733));
#179907=CARTESIAN_POINT('Ctrl Pts',(20.4411877427197,-20.2177263778437,
17.7696761038217));
#179908=CARTESIAN_POINT('Ctrl Pts',(20.2645491232413,-20.4167207417302,
17.7872412860787));
#179909=CARTESIAN_POINT('Ctrl Pts',(20.2085645656554,-20.4730682112223,
17.792453739437));
#179910=CARTESIAN_POINT('Ctrl Pts',(20.1229116573689,-20.5500914579864,
17.7997953650747));
#179911=CARTESIAN_POINT('Ctrl Pts',(20.0956732934613,-20.5733630359375,
17.8020453620333));
#179912=CARTESIAN_POINT('Ctrl Pts',(20.0620678708746,-20.6006298198979,
17.8047077196299));
#179913=CARTESIAN_POINT('Ctrl Pts',(20.0562551773457,-20.6052954371458,
17.8051642364927));
#179914=CARTESIAN_POINT('Ctrl Pts',(20.0471627086368,-20.612514973446,17.8058719908874));
#179915=CARTESIAN_POINT('Ctrl Pts',(20.0438999142413,-20.6150900431874,
17.8061247033619));
#179916=CARTESIAN_POINT('Ctrl Pts',(20.0378236904137,-20.6198565590691,
17.8065929499846));
#179917=CARTESIAN_POINT('Ctrl Pts',(20.035012334783,-20.6220504849644,17.8068086568785));
#179918=CARTESIAN_POINT('Ctrl Pts',(20.0286295762563,-20.6270055636558,
17.8072962700323));
#179919=CARTESIAN_POINT('Ctrl Pts',(20.0250548865612,-20.6297623963926,
17.8075678697158));
#179920=CARTESIAN_POINT('Ctrl Pts',(20.0144344388798,-20.6378989383835,
17.8083704811578));
#179921=CARTESIAN_POINT('Ctrl Pts',(20.0073635778774,-20.6432459275507,
17.8088992423076));
#179922=CARTESIAN_POINT('Ctrl Pts',(19.9544767104081,-20.6827192962727,
17.8128143714169));
#179923=CARTESIAN_POINT('Ctrl Pts',(19.9073253625779,-20.7150262344839,
17.8160842988135));
#179924=CARTESIAN_POINT('Ctrl Pts',(19.7306682855228,-20.8258361038753,
17.8277759492938));
#179925=CARTESIAN_POINT('Ctrl Pts',(19.5941512185764,-20.8922976198795,
17.8357917844943));
#179926=CARTESIAN_POINT('Ctrl Pts',(19.3644865811762,-20.9750596947134,
17.8492377569215));
#179927=CARTESIAN_POINT('Ctrl Pts',(19.2753073994552,-21.0007233294688,
17.854443600253));
#179928=CARTESIAN_POINT('Ctrl Pts',(19.1641540333276,-21.024944863132,17.8610701470341));
#179929=CARTESIAN_POINT('Ctrl Pts',(19.1435029939371,-21.0291230461215,
17.8623066882897));
#179930=CARTESIAN_POINT('Ctrl Pts',(19.1139908572965,-21.0346368240366,
17.8640828148199));
#179931=CARTESIAN_POINT('Ctrl Pts',(19.1051779063292,-21.0362255517487,
17.8646143392516));
#179932=CARTESIAN_POINT('Ctrl Pts',(19.0899348902619,-21.0388736950105,
17.8655357340878));
#179933=CARTESIAN_POINT('Ctrl Pts',(19.0835094783748,-21.0399594316208,
17.8659247622379));
#179934=CARTESIAN_POINT('Ctrl Pts',(19.0711818117254,-21.0419840054912,
17.8666723923177));
#179935=CARTESIAN_POINT('Ctrl Pts',(19.0652803853635,-21.0429275507541,
17.8670308406058));
#179936=CARTESIAN_POINT('Ctrl Pts',(19.0498904980835,-21.0453213626032,
17.8679670738101));
#179937=CARTESIAN_POINT('Ctrl Pts',(19.0403961078368,-21.0467320960606,
17.8685461059613));
#179938=CARTESIAN_POINT('Ctrl Pts',(19.0078136709391,-21.0513471354881,
17.8705383381295));
#179939=CARTESIAN_POINT('Ctrl Pts',(18.9846831165729,-21.054234579819,17.8719614879708));
#179940=CARTESIAN_POINT('Ctrl Pts',(18.7917146376176,-21.0750933695887,
17.8839119490064));
#179941=CARTESIAN_POINT('Ctrl Pts',(18.6203522476481,-21.0728297787518,
17.8951011276923));
#179942=CARTESIAN_POINT('Ctrl Pts',(18.3616208282738,-21.0379496625969,
17.9123532607126));
#179943=CARTESIAN_POINT('Ctrl Pts',(18.2729391681754,-21.0201579118172,
17.9183162923573));
#179944=CARTESIAN_POINT('Ctrl Pts',(18.1483250731119,-20.986740307303,17.9265592874871));
#179945=CARTESIAN_POINT('Ctrl Pts',(18.111267320365,-20.9757064222499,17.9289921545961));
#179946=CARTESIAN_POINT('Ctrl Pts',(18.0672904376315,-20.9612897757907,
17.9318402829592));
#179947=CARTESIAN_POINT('Ctrl Pts',(18.0600636219527,-20.9588773769331,
17.9323070428516));
#179948=CARTESIAN_POINT('Ctrl Pts',(18.04888037833,-20.955077053035,17.9330271776082));
#179949=CARTESIAN_POINT('Ctrl Pts',(18.0449148704866,-20.9537163288986,
17.9332821102341));
#179950=CARTESIAN_POINT('Ctrl Pts',(18.0375868131264,-20.9511774227121,
17.9337523954949));
#179951=CARTESIAN_POINT('Ctrl Pts',(18.0342232235184,-20.9500025419751,
17.9339679339679));
#179952=CARTESIAN_POINT('Ctrl Pts',(18.0266492252338,-20.9473355192997,
17.9344525573917));
#179953=CARTESIAN_POINT('Ctrl Pts',(18.0224405761324,-20.9458385441875,
17.9347213517472));
#179954=CARTESIAN_POINT('Ctrl Pts',(18.010101128324,-20.9414054772473,17.9355080643364));
#179955=CARTESIAN_POINT('Ctrl Pts',(18.0019834257658,-20.9384328506507,
17.9360238625153));
#179956=CARTESIAN_POINT('Ctrl Pts',(17.9455370956563,-20.9173697215983,
17.9395997087794));
#179957=CARTESIAN_POINT('Ctrl Pts',(17.8978616510936,-20.8975655957638,
17.9425649579697));
#179958=CARTESIAN_POINT('Ctrl Pts',(17.8310733338241,-20.8669127709695,
17.9467037787142));
#179959=CARTESIAN_POINT('Ctrl Pts',(17.8113349880038,-20.8574807284121,
17.9479249836257));
#179960=CARTESIAN_POINT('Ctrl Pts',(17.668446349898,-20.7864598601494,17.956775147596));
#179961=CARTESIAN_POINT('Ctrl Pts',(17.5514174744097,-20.713291793051,17.96409853679));
#179962=CARTESIAN_POINT('Ctrl Pts',(17.3704328114168,-20.5739143045383,
17.9766927937852));
#179963=CARTESIAN_POINT('Ctrl Pts',(17.3021869452797,-20.5139955608119,
17.9817933023191));
#179964=CARTESIAN_POINT('Ctrl Pts',(17.2232621482439,-20.4351702387793,
17.9882924139172));
#179965=CARTESIAN_POINT('Ctrl Pts',(17.2087435238608,-20.4202354887054,
17.9895150355767));
#179966=CARTESIAN_POINT('Ctrl Pts',(17.1883296515957,-20.3986069368003,
17.9912746205168));
#179967=CARTESIAN_POINT('Ctrl Pts',(17.1822523882909,-20.3920860395782,
17.9918037299412));
#179968=CARTESIAN_POINT('Ctrl Pts',(17.1718088761005,-20.3807372962285,
17.992722273466));
#179969=CARTESIAN_POINT('Ctrl Pts',(17.1674233463173,-20.3759273000759,
17.9931108795393));
#179970=CARTESIAN_POINT('Ctrl Pts',(17.1590478684073,-20.3666556501768,
17.993858640533));
#179971=CARTESIAN_POINT('Ctrl Pts',(17.1550545170895,-20.3621971444584,
17.9942176463347));
#179972=CARTESIAN_POINT('Ctrl Pts',(17.1446737499578,-20.3505078313432,
17.9951574325588));
#179973=CARTESIAN_POINT('Ctrl Pts',(17.1383168160314,-20.34325024887,17.9957394788501));
#179974=CARTESIAN_POINT('Ctrl Pts',(17.1165781276013,-20.3180866396199,
17.9977528008678));
#179975=CARTESIAN_POINT('Ctrl Pts',(17.1014468249146,-20.2999674625156,
17.999194311331));
#179976=CARTESIAN_POINT('Ctrl Pts',(16.9829318738435,-20.1531270860759,
18.0108161510283));
#179977=CARTESIAN_POINT('Ctrl Pts',(16.8946445712035,-20.0129890624413,
18.0216100112015));
#179978=CARTESIAN_POINT('Ctrl Pts',(16.7685612740643,-19.7488853971694,
18.0409499369832));
#179979=CARTESIAN_POINT('Ctrl Pts',(16.7241006235977,-19.628968966997,18.0493910386296));
#179980=CARTESIAN_POINT('Ctrl Pts',(16.6875909744737,-19.4942557998273,
18.0580465183784));
#179981=CARTESIAN_POINT('Ctrl Pts',(16.6845683633358,-19.4827176592795,
18.0587812922149));
#179982=CARTESIAN_POINT('Ctrl Pts',(16.6804108697193,-19.4662819679077,
18.0598180364087));
#179983=CARTESIAN_POINT('Ctrl Pts',(16.6791957303449,-19.4614052150545,
18.0601244202281));
#179984=CARTESIAN_POINT('Ctrl Pts',(16.6771318954958,-19.4529948170774,
18.0606506231147));
#179985=CARTESIAN_POINT('Ctrl Pts',(16.6762749145155,-19.4494632442821,
18.0608709160458));
#179986=CARTESIAN_POINT('Ctrl Pts',(16.6746311948224,-19.4426126360486,
18.0612969407393));
#179987=CARTESIAN_POINT('Ctrl Pts',(16.6738433837153,-19.4392939063317,
18.0615027363578));
#179988=CARTESIAN_POINT('Ctrl Pts',(16.671740039967,-19.4303370938981,18.0620565989928));
#179989=CARTESIAN_POINT('Ctrl Pts',(16.6704395975657,-19.4246954468276,
18.0624038044609));
#179990=CARTESIAN_POINT('Ctrl Pts',(16.6657019231818,-19.4037500214372,
18.0636869528289));
#179991=CARTESIAN_POINT('Ctrl Pts',(16.6624115604242,-19.3884130909542,
18.0646148494973));
#179992=CARTESIAN_POINT('Ctrl Pts',(16.6325545372761,-19.2412904073253,
18.073416765317));
#179993=CARTESIAN_POINT('Ctrl Pts',(16.6184239747238,-19.1072739496514,
18.0806878981142));
#179994=CARTESIAN_POINT('Ctrl Pts',(16.6170404620212,-18.9665205574997,
18.0883318251222));
#179995=CARTESIAN_POINT('Ctrl Pts',(16.6170066729076,-18.9602331678495,
18.0886732576158));
#179996=CARTESIAN_POINT('Ctrl Pts',(16.616866854777,-18.8081072288272,18.0969354855539));
#179997=CARTESIAN_POINT('Ctrl Pts',(16.6318021057098,-18.6626640217989,
18.1048962014557));
#179998=CARTESIAN_POINT('Ctrl Pts',(16.6664676958402,-18.4963942861878,
18.1147554600943));
#179999=CARTESIAN_POINT('Ctrl Pts',(16.6717720455133,-18.4729570065316,
18.1161622425507));
#180000=CARTESIAN_POINT('Ctrl Pts',(16.679780444546,-18.4401743679251,18.1181559718257));
#180001=CARTESIAN_POINT('Ctrl Pts',(16.6821518244031,-18.4307490823287,
18.1187322238881));
#180002=CARTESIAN_POINT('Ctrl Pts',(16.6860916186233,-18.4155335575623,
18.1196675317744));
#180003=CARTESIAN_POINT('Ctrl Pts',(16.6876199074586,-18.40973300111,18.1200252863472));
#180004=CARTESIAN_POINT('Ctrl Pts',(16.6908553251563,-18.3976615878375,
18.1207723192251));
#180005=CARTESIAN_POINT('Ctrl Pts',(16.6925667172145,-18.3913919479573,
18.1211617325887));
#180006=CARTESIAN_POINT('Ctrl Pts',(16.6966783608368,-18.376597557661,18.122084030321));
#180007=CARTESIAN_POINT('Ctrl Pts',(16.6991032760193,-18.3680798418789,
18.1226177126458));
#180008=CARTESIAN_POINT('Ctrl Pts',(16.7073169332177,-18.3399013139651,
18.1243922870873));
#180009=CARTESIAN_POINT('Ctrl Pts',(16.7133375992237,-18.3203098304095,
18.1256407199589));
#180010=CARTESIAN_POINT('Ctrl Pts',(16.7277680334014,-18.2756714939648,
18.1285197261513));
#180011=CARTESIAN_POINT('Ctrl Pts',(16.736362351287,-18.2506939993404,18.1301558666793));
#180012=CARTESIAN_POINT('Ctrl Pts',(16.7454193851305,-18.225889720383,18.1318062882837));
#180013=CARTESIAN_POINT('Origin',(18.734,-18.952,0.));
#180014=CARTESIAN_POINT('',(16.7477768045735,-18.2267292102227,19.1554367670381));
#180015=CARTESIAN_POINT('',(16.7454194046824,-18.2258896668369,18.9348454761515));
#180016=CARTESIAN_POINT('',(16.7454193692319,-18.2258897639242,0.));
#180017=CARTESIAN_POINT('',(16.6180378855072,-18.9538841874204,19.1109437209775));
#180018=CARTESIAN_POINT('Ctrl Pts',(16.6180378855072,-18.9538841874204,
19.1109437209775));
#180019=CARTESIAN_POINT('Ctrl Pts',(16.620150035447,-18.7070537460865,19.125774736331));
#180020=CARTESIAN_POINT('Ctrl Pts',(16.6645218904389,-18.4595580919697,
19.1406057516845));
#180021=CARTESIAN_POINT('Ctrl Pts',(16.7477768045735,-18.2267292102227,
19.1554367670381));
#180022=CARTESIAN_POINT('Ctrl Pts',(16.617000874469,-18.9539241884034,19.1115401934235));
#180023=CARTESIAN_POINT('Ctrl Pts',(16.6170652114638,-19.0247079855457,
19.1069028320399));
#180024=CARTESIAN_POINT('Ctrl Pts',(16.6206796002688,-19.0954439547243,
19.1022147600423));
#180025=CARTESIAN_POINT('Ctrl Pts',(16.6387701735723,-19.2736020781264,
19.0903935332217));
#180026=CARTESIAN_POINT('Ctrl Pts',(16.6579618430164,-19.3803535572353,
19.083293761929));
#180027=CARTESIAN_POINT('Ctrl Pts',(16.6882113661698,-19.4965887500812,
19.0758470398698));
#180028=CARTESIAN_POINT('Ctrl Pts',(16.6912765006865,-19.5079755038791,
19.0751207163271));
#180029=CARTESIAN_POINT('Ctrl Pts',(16.6957773496905,-19.5241559699026,
19.0740937428757));
#180030=CARTESIAN_POINT('Ctrl Pts',(16.6971350986209,-19.5289708838746,
19.0737887897188));
#180031=CARTESIAN_POINT('Ctrl Pts',(16.6995074993299,-19.537271254882,19.0732642610191));
#180032=CARTESIAN_POINT('Ctrl Pts',(16.700514067425,-19.5407589828398,19.0730442195897));
#180033=CARTESIAN_POINT('Ctrl Pts',(16.7024856521041,-19.5475250899387,
19.0726180632995));
#180034=CARTESIAN_POINT('Ctrl Pts',(16.703449635275,-19.5508037200546,19.0724118875206));
#180035=CARTESIAN_POINT('Ctrl Pts',(16.7060774471599,-19.5596619284184,
19.0718556859131));
#180036=CARTESIAN_POINT('Ctrl Pts',(16.7077563760127,-19.5652370484889,
19.0715065346915));
#180037=CARTESIAN_POINT('Ctrl Pts',(16.7141061795218,-19.5860116654419,
19.0702086337591));
#180038=CARTESIAN_POINT('Ctrl Pts',(16.7189253847574,-19.6011657467373,
19.0692681703082));
#180039=CARTESIAN_POINT('Ctrl Pts',(16.7615366618779,-19.7301087741614,
19.0613084815078));
#180040=CARTESIAN_POINT('Ctrl Pts',(16.8087671369662,-19.8405667096365,
19.0547667093754));
#180041=CARTESIAN_POINT('Ctrl Pts',(16.8870989036541,-19.987778871475,19.0457035422698));
#180042=CARTESIAN_POINT('Ctrl Pts',(16.9104596223258,-20.0283744664809,
19.043165895331));
#180043=CARTESIAN_POINT('Ctrl Pts',(16.9827337657313,-20.1448544928694,
19.0356933589462));
#180044=CARTESIAN_POINT('Ctrl Pts',(17.0351732310353,-20.2184205215897,
19.0307219844509));
#180045=CARTESIAN_POINT('Ctrl Pts',(17.1225202872451,-20.3257312918419,
19.0228503161085));
#180046=CARTESIAN_POINT('Ctrl Pts',(17.1541589179061,-20.3620021851008,
19.0200699604294));
#180047=CARTESIAN_POINT('Ctrl Pts',(17.1951341025899,-20.4058647071823,
19.0165371051478));
#180048=CARTESIAN_POINT('Ctrl Pts',(17.2033372655788,-20.414498691187,19.0158330775069));
#180049=CARTESIAN_POINT('Ctrl Pts',(17.2158470417529,-20.427444925191,19.0147640720485));
#180050=CARTESIAN_POINT('Ctrl Pts',(17.2201002307986,-20.4318086428753,
19.0144014173986));
#180051=CARTESIAN_POINT('Ctrl Pts',(17.2288317491846,-20.4406900285331,
19.0136584936779));
#180052=CARTESIAN_POINT('Ctrl Pts',(17.2333117158644,-20.4452059927581,
19.0132781544879));
#180053=CARTESIAN_POINT('Ctrl Pts',(17.2430281277644,-20.4549125851703,
19.0124550181459));
#180054=CARTESIAN_POINT('Ctrl Pts',(17.2482714600792,-20.4600961726571,
19.0120119170828));
#180055=CARTESIAN_POINT('Ctrl Pts',(17.2625641643284,-20.4740791374711,
19.0108069560384));
#180056=CARTESIAN_POINT('Ctrl Pts',(17.2716652206148,-20.4828250394491,
19.0100427772123));
#180057=CARTESIAN_POINT('Ctrl Pts',(17.3163414301034,-20.5249958610594,
19.0063059103351));
#180058=CARTESIAN_POINT('Ctrl Pts',(17.3529848115367,-20.5572626678642,
19.003284353189));
#180059=CARTESIAN_POINT('Ctrl Pts',(17.4081689160612,-20.6025669603666,
18.9987923241326));
#180060=CARTESIAN_POINT('Ctrl Pts',(17.4258573728964,-20.6166207270723,
18.9973608634575));
#180061=CARTESIAN_POINT('Ctrl Pts',(17.543364938576,-20.7069527132475,18.9879074241703));
#180062=CARTESIAN_POINT('Ctrl Pts',(17.6495718321833,-20.7744929229256,
18.9796023670809));
#180063=CARTESIAN_POINT('Ctrl Pts',(17.8347824117938,-20.8703259939516,
18.9658293618443));
#180064=CARTESIAN_POINT('Ctrl Pts',(17.9106203525734,-20.9040795704709,
18.9603734206604));
#180065=CARTESIAN_POINT('Ctrl Pts',(18.0226614618614,-20.9462513868634,
18.9527370823941));
#180066=CARTESIAN_POINT('Ctrl Pts',(18.0574095816186,-20.9583067798161,
18.9504257082238));
#180067=CARTESIAN_POINT('Ctrl Pts',(18.0996138954436,-20.9717276251687,
18.9477008309405));
#180068=CARTESIAN_POINT('Ctrl Pts',(18.1067835335827,-20.9739656074384,
18.9472407656497));
#180069=CARTESIAN_POINT('Ctrl Pts',(18.117951200504,-20.9773864463134,18.9465287203413));
#180070=CARTESIAN_POINT('Ctrl Pts',(18.12194098629,-20.978595703316,18.9462752369095));
#180071=CARTESIAN_POINT('Ctrl Pts',(18.1293490443409,-20.980817125907,18.9458062888669));
#180072=CARTESIAN_POINT('Ctrl Pts',(18.1327662697539,-20.9818324340824,
18.9455906469487));
#180073=CARTESIAN_POINT('Ctrl Pts',(18.1405004681003,-20.9841091339077,
18.9451041015624));
#180074=CARTESIAN_POINT('Ctrl Pts',(18.1448188939874,-20.9853654004266,
18.944833498997));
#180075=CARTESIAN_POINT('Ctrl Pts',(18.1559582180083,-20.9885674572621,
18.9441381404782));
#180076=CARTESIAN_POINT('Ctrl Pts',(18.1627850135225,-20.9904927647988,
18.943714548472));
#180077=CARTESIAN_POINT('Ctrl Pts',(18.2043241014246,-21.0019826472857,
18.9411519389684));
#180078=CARTESIAN_POINT('Ctrl Pts',(18.2392683215349,-21.0106952964831,
18.9390589412509));
#180079=CARTESIAN_POINT('Ctrl Pts',(18.289725807202,-21.0219167361447,18.9361041378621));
#180080=CARTESIAN_POINT('Ctrl Pts',(18.3050692561207,-21.0251505713877,
18.9352144701453));
#180081=CARTESIAN_POINT('Ctrl Pts',(18.321324888878,-21.028388463878,18.9342799220557));
#180082=CARTESIAN_POINT('Ctrl Pts',(18.3222023410887,-21.0285626618005,
18.9342295013104));
#180083=CARTESIAN_POINT('Ctrl Pts',(18.3453897870997,-21.0331507202427,
18.9328977330889));
#180084=CARTESIAN_POINT('Ctrl Pts',(18.3677699226102,-21.0372054574691,
18.931628080751));
#180085=CARTESIAN_POINT('Ctrl Pts',(18.5377453444319,-21.0651798041144,
18.9220759273548));
#180086=CARTESIAN_POINT('Ctrl Pts',(18.6874375397328,-21.0737633457977,
18.914148898755));
#180087=CARTESIAN_POINT('Ctrl Pts',(18.895486284219,-21.0636497386645,18.9026000437049));
#180088=CARTESIAN_POINT('Ctrl Pts',(18.9540349283439,-21.0583537951738,
18.8992952396136));
#180089=CARTESIAN_POINT('Ctrl Pts',(19.0479101787959,-21.0459056572862,
18.8938547420006));
#180090=CARTESIAN_POINT('Ctrl Pts',(19.0834080489576,-21.0402754349872,
18.8917646646156));
#180091=CARTESIAN_POINT('Ctrl Pts',(19.1295530010521,-21.0317470157421,
18.8889978805677));
#180092=CARTESIAN_POINT('Ctrl Pts',(19.1403461580014,-21.0296651845554,
18.8883471655341));
#180093=CARTESIAN_POINT('Ctrl Pts',(19.157924918173,-21.026132301998,18.8872813244757));
#180094=CARTESIAN_POINT('Ctrl Pts',(19.1647205497051,-21.0247317599582,
18.8868678158903));
#180095=CARTESIAN_POINT('Ctrl Pts',(19.1778116031673,-21.0219666070966,
18.8860683420336));
#180096=CARTESIAN_POINT('Ctrl Pts',(19.1841079308838,-21.0206066186528,
18.8856825289033));
#180097=CARTESIAN_POINT('Ctrl Pts',(19.1985605790557,-21.017415780284,18.8847939093201));
#180098=CARTESIAN_POINT('Ctrl Pts',(19.2067124191574,-21.0155653231005,
18.8842904779249));
#180099=CARTESIAN_POINT('Ctrl Pts',(19.2284499925962,-21.0104953583301,
18.882942014316));
#180100=CARTESIAN_POINT('Ctrl Pts',(19.2420150201229,-21.0071896895702,
18.8820942229203));
#180101=CARTESIAN_POINT('Ctrl Pts',(19.3520931255273,-20.9792083062091,
18.8751620709404));
#180102=CARTESIAN_POINT('Ctrl Pts',(19.4467735742749,-20.947886147957,18.8688614291534));
#180103=CARTESIAN_POINT('Ctrl Pts',(19.6655329465785,-20.8579603443488,
18.853521703438));
#180104=CARTESIAN_POINT('Ctrl Pts',(19.7868273168242,-20.7937354822206,
18.8443642515389));
#180105=CARTESIAN_POINT('Ctrl Pts',(19.9429078570594,-20.6906048252188,
18.8321474387152));
#180106=CARTESIAN_POINT('Ctrl Pts',(19.9837636513484,-20.6614725593594,
18.8289077999918));
#180107=CARTESIAN_POINT('Ctrl Pts',(20.0447099289925,-20.6146606637014,
18.8240527637777));
#180108=CARTESIAN_POINT('Ctrl Pts',(20.0655634722463,-20.5980072519908,
18.8223873935712));
#180109=CARTESIAN_POINT('Ctrl Pts',(20.091327007782,-20.5766225963108,18.8203304754329));
#180110=CARTESIAN_POINT('Ctrl Pts',(20.0965355111079,-20.572256822348,18.8199146679904));
#180111=CARTESIAN_POINT('Ctrl Pts',(20.104784895633,-20.5652742674967,18.8192562751029));
#180112=CARTESIAN_POINT('Ctrl Pts',(20.1078394666861,-20.5626738380742,
18.8190125248797));
#180113=CARTESIAN_POINT('Ctrl Pts',(20.1136142998931,-20.5577292045004,
18.8185518062909));
#180114=CARTESIAN_POINT('Ctrl Pts',(20.1163359548494,-20.5553867913711,
18.8183347197709));
#180115=CARTESIAN_POINT('Ctrl Pts',(20.1225810586224,-20.5499841746153,
18.8178366811033));
#180116=CARTESIAN_POINT('Ctrl Pts',(20.1261003557378,-20.5469192390823,
18.8175560837868));
#180117=CARTESIAN_POINT('Ctrl Pts',(20.1354925323464,-20.538684875531,18.816807311222));
#180118=CARTESIAN_POINT('Ctrl Pts',(20.1413470019452,-20.5334944302318,
18.8163406550191));
#180119=CARTESIAN_POINT('Ctrl Pts',(20.1844649596188,-20.4948379444219,
18.8129031626051));
#180120=CARTESIAN_POINT('Ctrl Pts',(20.2205622916639,-20.4600885033655,
18.8100220140627));
#180121=CARTESIAN_POINT('Ctrl Pts',(20.2561637673475,-20.4232945610323,
18.8071347119682));
#180122=CARTESIAN_POINT('Ctrl Pts',(20.2569311871159,-20.422500193563,18.8070724512626));
#180123=CARTESIAN_POINT('Ctrl Pts',(20.2676427367322,-20.4113951322806,
18.8062031037568));
#180124=CARTESIAN_POINT('Ctrl Pts',(20.2774827530772,-20.4009841961231,
18.8054006282567));
#180125=CARTESIAN_POINT('Ctrl Pts',(20.3957970167284,-20.2732323812727,
18.7956930308644));
#180126=CARTESIAN_POINT('Ctrl Pts',(20.4907566013449,-20.144071890234,18.7872529699876));
#180127=CARTESIAN_POINT('Ctrl Pts',(20.6095576002548,-19.9369884888591,
18.7740042318909));
#180128=CARTESIAN_POINT('Ctrl Pts',(20.644970273443,-19.8663901298712,18.769538109495));
#180129=CARTESIAN_POINT('Ctrl Pts',(20.6840439820399,-19.7762517870427,
18.7638050068164));
#180130=CARTESIAN_POINT('Ctrl Pts',(20.691487501346,-19.7584150208188,18.7626692709587));
#180131=CARTESIAN_POINT('Ctrl Pts',(20.7019069469471,-19.7324524680005,
18.7610133048494));
#180132=CARTESIAN_POINT('Ctrl Pts',(20.7050790507993,-19.7244060970536,
18.7604996968709));
#180133=CARTESIAN_POINT('Ctrl Pts',(20.7105356330737,-19.7103123879451,
18.7595993130592));
#180134=CARTESIAN_POINT('Ctrl Pts',(20.7128419002785,-19.7042735664588,
18.7592132750103));
#180135=CARTESIAN_POINT('Ctrl Pts',(20.717253308123,-19.6925619001657,18.7584640825683));
#180136=CARTESIAN_POINT('Ctrl Pts',(20.7193618587849,-19.6868904004394,
18.7581010469064));
#180137=CARTESIAN_POINT('Ctrl Pts',(20.7243240304092,-19.6733661089447,
18.7572347651345));
#180138=CARTESIAN_POINT('Ctrl Pts',(20.7271555172221,-19.6655053540056,
18.7567307863553));
#180139=CARTESIAN_POINT('Ctrl Pts',(20.7370939714386,-19.6373934334635,
18.7549266507367));
#180140=CARTESIAN_POINT('Ctrl Pts',(20.7439392410429,-19.6170517356877,
18.7536178675147));
#180141=CARTESIAN_POINT('Ctrl Pts',(20.8087912100549,-19.4141813327006,
18.7405283510565));
#180142=CARTESIAN_POINT('Ctrl Pts',(20.84207179726,-19.2247143729517,18.7278883131169));
#180143=CARTESIAN_POINT('Ctrl Pts',(20.8523695349017,-18.957134575205,18.7102207957596));
#180144=CARTESIAN_POINT('Ctrl Pts',(20.8511775341112,-18.8807488283608,
18.7052146034663));
#180145=CARTESIAN_POINT('Ctrl Pts',(20.8434255922919,-18.7696911120313,
18.6981244729446));
#180146=CARTESIAN_POINT('Ctrl Pts',(20.8401247623566,-18.7348556347325,
18.6959281023601));
#180147=CARTESIAN_POINT('Ctrl Pts',(20.8350811045628,-18.6927665563776,
18.6933205148));
#180148=CARTESIAN_POINT('Ctrl Pts',(20.8341618770439,-18.6854219060445,
18.6928671951307));
#180149=CARTESIAN_POINT('Ctrl Pts',(20.8326677828748,-18.6739717280811,
18.692163308659));
#180150=CARTESIAN_POINT('Ctrl Pts',(20.8321193573371,-18.6698628951892,
18.6919112923699));
#180151=CARTESIAN_POINT('Ctrl Pts',(20.8310765119621,-18.6622210688013,
18.691443672769));
#180152=CARTESIAN_POINT('Ctrl Pts',(20.8305852355322,-18.6586877493163,
18.6912279008464));
#180153=CARTESIAN_POINT('Ctrl Pts',(20.8294498587385,-18.6506705984575,
18.6907392946298));
#180154=CARTESIAN_POINT('Ctrl Pts',(20.8288002986951,-18.6461875931485,
18.690466772157));
#180155=CARTESIAN_POINT('Ctrl Pts',(20.8270811542106,-18.634585272112,18.6897631854897));
#180156=CARTESIAN_POINT('Ctrl Pts',(20.8259896246901,-18.6274691984896,
18.6893333318601));
#180157=CARTESIAN_POINT('Ctrl Pts',(20.8189514966166,-18.5830966976193,
18.6866626748909));
#180158=CARTESIAN_POINT('Ctrl Pts',(20.8120457445476,-18.5459967153876,
18.6844724648767));
#180159=CARTESIAN_POINT('Ctrl Pts',(20.7686152836847,-18.3429997244225,
18.6726271440897));
#180160=CARTESIAN_POINT('Ctrl Pts',(20.7132153880081,-18.1817670269906,
18.6636884066837));
#180161=CARTESIAN_POINT('Ctrl Pts',(20.5977361780559,-17.9434419168421,
18.6491175835415));
#180162=CARTESIAN_POINT('Ctrl Pts',(20.5506434548851,-17.8608971327872,
18.6437932139985));
#180163=CARTESIAN_POINT('Ctrl Pts',(20.4863803687323,-17.7640154423997,
18.6370231707435));
#180164=CARTESIAN_POINT('Ctrl Pts',(20.4743182342881,-17.7464143911656,
18.6357711300839));
#180165=CARTESIAN_POINT('Ctrl Pts',(20.4567927594812,-17.7216524400462,
18.6339766030276));
#180166=CARTESIAN_POINT('Ctrl Pts',(20.4515463460132,-17.7143390787895,
18.6334424111073));
#180167=CARTESIAN_POINT('Ctrl Pts',(20.4424165214023,-17.7017821943033,
18.6325178606856));
#180168=CARTESIAN_POINT('Ctrl Pts',(20.4385551833193,-17.6965227211013,
18.6321283602091));
#180169=CARTESIAN_POINT('Ctrl Pts',(20.4311162969374,-17.6864878993819,
18.6313808487706));
#180170=CARTESIAN_POINT('Ctrl Pts',(20.427542747514,-17.6817096539171,18.6310229963873));
#180171=CARTESIAN_POINT('Ctrl Pts',(20.4181998355861,-17.6693266073927,
18.6300905803239));
#180172=CARTESIAN_POINT('Ctrl Pts',(20.4123992004189,-17.6617456693907,
18.6295147893487));
#180173=CARTESIAN_POINT('Ctrl Pts',(20.3924552839219,-17.636042741397,18.6275454130094));
#180174=CARTESIAN_POINT('Ctrl Pts',(20.3780685804972,-17.6181124963164,
18.6261421830574));
#180175=CARTESIAN_POINT('Ctrl Pts',(20.2512922901167,-17.4652776528622,
18.6139197872578));
#180176=CARTESIAN_POINT('Ctrl Pts',(20.122833607584,-17.3446304201945,18.602396066731));
#180177=CARTESIAN_POINT('Ctrl Pts',(19.9107367932032,-17.1900298770749,
18.5850549848006));
#180178=CARTESIAN_POINT('Ctrl Pts',(19.8373844545476,-17.1431902102999,
18.5793250580783));
#180179=CARTESIAN_POINT('Ctrl Pts',(19.728299771966,-17.0826455043845,18.571359781479));
#180180=CARTESIAN_POINT('Ctrl Pts',(19.6947562758084,-17.0651862691705,
18.5689817325433));
#180181=CARTESIAN_POINT('Ctrl Pts',(19.6539540959718,-17.0453194348311,
18.5661891346508));
#180182=CARTESIAN_POINT('Ctrl Pts',(19.6471294859879,-17.0420416595946,
18.5657253429366));
#180183=CARTESIAN_POINT('Ctrl Pts',(19.6365078851409,-17.0370101810516,
18.5650087938176));
#180184=CARTESIAN_POINT('Ctrl Pts',(19.6327231138948,-17.0352310377443,
18.564754502849));
#180185=CARTESIAN_POINT('Ctrl Pts',(19.6257034045994,-17.0319565790059,
18.5642848126053));
#180186=CARTESIAN_POINT('Ctrl Pts',(19.6224699909983,-17.0304582295274,
18.5640692312618));
#180187=CARTESIAN_POINT('Ctrl Pts',(19.6151630084797,-17.0270945932702,
18.5635837702082));
#180188=CARTESIAN_POINT('Ctrl Pts',(19.6110873043842,-17.0252340739708,
18.5633141856012));
#180189=CARTESIAN_POINT('Ctrl Pts',(19.5990740855356,-17.0197961735086,
18.5625230093283));
#180190=CARTESIAN_POINT('Ctrl Pts',(19.5911202624566,-17.0162547527759,
18.5620035739807));
#180191=CARTESIAN_POINT('Ctrl Pts',(19.5344972672616,-16.9914609291305,
18.5583352841853));
#180192=CARTESIAN_POINT('Ctrl Pts',(19.4850610859561,-16.9719955616644,
18.5552869015237));
#180193=CARTESIAN_POINT('Ctrl Pts',(19.4326900253195,-16.9536189205482,
18.552164966228));
#180194=CARTESIAN_POINT('Ctrl Pts',(19.4304378215955,-16.9528329107057,
18.5520309130727));
#180195=CARTESIAN_POINT('Ctrl Pts',(19.2889259380069,-16.9037140023828,
18.5436205846945));
#180196=CARTESIAN_POINT('Ctrl Pts',(19.144993167015,-16.870051761806,18.535804091456));
#180197=CARTESIAN_POINT('Ctrl Pts',(18.9017579375211,-16.8393954862422,
18.5223328984335));
#180198=CARTESIAN_POINT('Ctrl Pts',(18.804073857189,-16.8339048737711,18.5168602449389));
#180199=CARTESIAN_POINT('Ctrl Pts',(18.6847002714384,-16.8354631937374,
18.5099105147111));
#180200=CARTESIAN_POINT('Ctrl Pts',(18.6630400526057,-16.8360786521938,
18.5086393220794));
#180201=CARTESIAN_POINT('Ctrl Pts',(18.6323460040724,-16.8374226232391,
18.5068220849068));
#180202=CARTESIAN_POINT('Ctrl Pts',(18.6233010830058,-16.8378768335093,
18.5062846281345));
#180203=CARTESIAN_POINT('Ctrl Pts',(18.6077349798491,-16.8387586862463,
18.5053562071911));
#180204=CARTESIAN_POINT('Ctrl Pts',(18.6012123030525,-16.8391585171784,
18.5049661204298));
#180205=CARTESIAN_POINT('Ctrl Pts',(18.5887491576818,-16.8399804310905,
18.5042187190399));
#180206=CARTESIAN_POINT('Ctrl Pts',(18.5828084053839,-16.8403973936268,
18.5038615689527));
#180207=CARTESIAN_POINT('Ctrl Pts',(18.5674130771166,-16.8415432444234,
18.502933678824));
#180208=CARTESIAN_POINT('Ctrl Pts',(18.5579615745834,-16.8423105943681,
18.5023617350231));
#180209=CARTESIAN_POINT('Ctrl Pts',(18.5259970074067,-16.8451220329862,
18.5004195123274));
#180210=CARTESIAN_POINT('Ctrl Pts',(18.5035122386515,-16.8474631524947,
18.4990399459163));
#180211=CARTESIAN_POINT('Ctrl Pts',(18.3020366076918,-16.8717082602263,
18.4865540254973));
#180212=CARTESIAN_POINT('Ctrl Pts',(18.1265215968773,-16.9160356784934,
18.4746992235394));
#180213=CARTESIAN_POINT('Ctrl Pts',(17.8809234710159,-17.0126828452792,
18.4572661424599));
#180214=CARTESIAN_POINT('Ctrl Pts',(17.8049397264581,-17.0479150690734,
18.4517595148268));
#180215=CARTESIAN_POINT('Ctrl Pts',(17.6986814552425,-17.1050644421313,
18.4440621133919));
#180216=CARTESIAN_POINT('Ctrl Pts',(17.6665877604628,-17.1234248881538,
18.441738217114));
#180217=CARTESIAN_POINT('Ctrl Pts',(17.6285601949496,-17.146522661701,18.4390006060156));
#180218=CARTESIAN_POINT('Ctrl Pts',(17.6221518817284,-17.1504619494723,
18.4385398308868));
#180219=CARTESIAN_POINT('Ctrl Pts',(17.612222568142,-17.1566388122636,18.4378269274789));
#180220=CARTESIAN_POINT('Ctrl Pts',(17.6086870295047,-17.1588527332691,
18.437573290062));
#180221=CARTESIAN_POINT('Ctrl Pts',(17.6021424077684,-17.1629778934257,
18.4371042010841));
#180222=CARTESIAN_POINT('Ctrl Pts',(17.5991316352445,-17.1648862649878,
18.4368885713057));
#180223=CARTESIAN_POINT('Ctrl Pts',(17.5923359161326,-17.1692178157897,
18.4364022353642));
#180224=CARTESIAN_POINT('Ctrl Pts',(17.5885538671497,-17.1716454414009,
18.4361318289867));
#180225=CARTESIAN_POINT('Ctrl Pts',(17.5774136063864,-17.1788463573483,
18.435335998597));
#180226=CARTESIAN_POINT('Ctrl Pts',(17.5700771912056,-17.1836534198499,
18.4348127690381));
#180227=CARTESIAN_POINT('Ctrl Pts',(17.5172408467851,-17.2187448206347,
18.4310491594108));
#180228=CARTESIAN_POINT('Ctrl Pts',(17.4728948475057,-17.2507383396572,
18.4279152641341));
#180229=CARTESIAN_POINT('Ctrl Pts',(17.2972522732232,-17.3881030042149,
18.41538893972));
#180230=CARTESIAN_POINT('Ctrl Pts',(17.1775038974791,-17.5072352240484,
18.406530471036));
#180231=CARTESIAN_POINT('Ctrl Pts',(17.0365796077152,-17.6855378391791,
18.3939311523265));
#180232=CARTESIAN_POINT('Ctrl Pts',(17.0019842259434,-17.733278133765,18.3906172203878));
#180233=CARTESIAN_POINT('Ctrl Pts',(16.9495311335903,-17.81241379327,18.3851630515493));
#180234=CARTESIAN_POINT('Ctrl Pts',(16.9304053205674,-17.8429319841393,
18.3830687313743));
#180235=CARTESIAN_POINT('Ctrl Pts',(16.9064660573374,-17.8833888946915,
18.3802971110623));
#180236=CARTESIAN_POINT('Ctrl Pts',(16.9009381459161,-17.8928993257645,
18.3796459180194));
#180237=CARTESIAN_POINT('Ctrl Pts',(16.8920438930034,-17.9084795798079,
18.3785794903944));
#180238=CARTESIAN_POINT('Ctrl Pts',(16.8886327949576,-17.914523713885,18.378165876683));
#180239=CARTESIAN_POINT('Ctrl Pts',(16.8821134573732,-17.9262092227942,
18.3773663372498));
#180240=CARTESIAN_POINT('Ctrl Pts',(16.8790011178966,-17.9318482312244,
18.3769805644079));
#180241=CARTESIAN_POINT('Ctrl Pts',(16.8719106741465,-17.9448345960143,
18.3760922344689));
#180242=CARTESIAN_POINT('Ctrl Pts',(16.8679502554473,-17.9521914402386,
18.3755890537669));
#180243=CARTESIAN_POINT('Ctrl Pts',(16.8574949048652,-17.9718917552561,
18.3742416978715));
#180244=CARTESIAN_POINT('Ctrl Pts',(16.8510783203701,-17.9842761358493,
18.3733947706254));
#180245=CARTESIAN_POINT('Ctrl Pts',(16.807171029365,-18.0711099105015,18.367456078307));
#180246=CARTESIAN_POINT('Ctrl Pts',(16.7739942120167,-18.147632526116,18.362216055964));
#180247=CARTESIAN_POINT('Ctrl Pts',(16.7454193588142,-18.2258897924551,
18.356854558525));
#180248=CARTESIAN_POINT('',(16.6170000449379,-18.9515638040726,18.8870727812038));
#180249=CARTESIAN_POINT('Ctrl Pts',(16.7454193851305,-18.225889720383,18.1318062882837));
#180250=CARTESIAN_POINT('Ctrl Pts',(16.7665449585877,-18.1680336246436,
18.1356559043328));
#180251=CARTESIAN_POINT('Ctrl Pts',(16.7901879235971,-18.11111997658,18.1395843126614));
#180252=CARTESIAN_POINT('Ctrl Pts',(16.8711047733789,-17.938065988932,18.1519520858756));
#180253=CARTESIAN_POINT('Ctrl Pts',(16.9365617134726,-17.8260991331353,
18.1605860013658));
#180254=CARTESIAN_POINT('Ctrl Pts',(17.027571406272,-17.6987946938612,18.1708505942142));
#180255=CARTESIAN_POINT('Ctrl Pts',(17.0437391931054,-17.6770723296644,
18.1726183489123));
#180256=CARTESIAN_POINT('Ctrl Pts',(17.0954975693988,-17.6102477688841,
18.1780951904285));
#180257=CARTESIAN_POINT('Ctrl Pts',(17.1325132009441,-17.566276161235,18.1817560508463));
#180258=CARTESIAN_POINT('Ctrl Pts',(17.1772632991259,-17.5173088715787,
18.1858493168984));
#180259=CARTESIAN_POINT('Ctrl Pts',(17.1832926097607,-17.5107941208812,
18.1863942385789));
#180260=CARTESIAN_POINT('Ctrl Pts',(17.1924515195223,-17.5010218186135,
18.1872118886485));
#180261=CARTESIAN_POINT('Ctrl Pts',(17.1955507732445,-17.4977361387655,
18.187486845595));
#180262=CARTESIAN_POINT('Ctrl Pts',(17.2011159192302,-17.4918739392213,
18.1879774508873));
#180263=CARTESIAN_POINT('Ctrl Pts',(17.203577819605,-17.4892937175194,18.1881933989095));
#180264=CARTESIAN_POINT('Ctrl Pts',(17.2089219344602,-17.4837210226793,
18.1886598143095));
#180265=CARTESIAN_POINT('Ctrl Pts',(17.21180643224,-17.4807308185842,18.188910099766));
#180266=CARTESIAN_POINT('Ctrl Pts',(17.219884348895,-17.4724060613665,18.1896070073417));
#180267=CARTESIAN_POINT('Ctrl Pts',(17.2250971918987,-17.4670903234193,
18.1900521420559));
#180268=CARTESIAN_POINT('Ctrl Pts',(17.2554545728113,-17.4364586612858,
18.1926187445845));
#180269=CARTESIAN_POINT('Ctrl Pts',(17.2812094973664,-17.4117525444168,
18.1946949947162));
#180270=CARTESIAN_POINT('Ctrl Pts',(17.3658491794521,-17.3345726732887,
18.2012494691061));
#180271=CARTESIAN_POINT('Ctrl Pts',(17.4270482459534,-17.2847307130793,
18.205590639856));
#180272=CARTESIAN_POINT('Ctrl Pts',(17.5646209109373,-17.184929349456,18.2148598574735));
#180273=CARTESIAN_POINT('Ctrl Pts',(17.6417259456608,-17.1362567900831,
18.2197668998467));
#180274=CARTESIAN_POINT('Ctrl Pts',(17.8150507045617,-17.0418920553965,
18.2306130202343));
#180275=CARTESIAN_POINT('Ctrl Pts',(17.9120567877858,-16.9981869926977,
18.2365759856562));
#180276=CARTESIAN_POINT('Ctrl Pts',(18.0251851384886,-16.9571392406406,
18.2436279186341));
#180277=CARTESIAN_POINT('Ctrl Pts',(18.0384920110797,-16.952460908076,18.2444586991437));
#180278=CARTESIAN_POINT('Ctrl Pts',(18.0597973654308,-16.9452089333397,
18.2457913137286));
#180279=CARTESIAN_POINT('Ctrl Pts',(18.0677662793405,-16.9425492780265,
18.2462903024008));
#180280=CARTESIAN_POINT('Ctrl Pts',(18.0818792474372,-16.9379322000762,
18.2471750621814));
#180281=CARTESIAN_POINT('Ctrl Pts',(18.0880168436865,-16.9359552735735,
18.2475601848501));
#180282=CARTESIAN_POINT('Ctrl Pts',(18.1007601237863,-16.9319148157044,
18.2483605652292));
#180283=CARTESIAN_POINT('Ctrl Pts',(18.1073670781434,-16.9298555758517,
18.2487759586172));
#180284=CARTESIAN_POINT('Ctrl Pts',(18.1244158085745,-16.9246334452194,
18.2498489949708));
#180285=CARTESIAN_POINT('Ctrl Pts',(18.1348720557028,-16.9215188419338,
18.2505082093358));
#180286=CARTESIAN_POINT('Ctrl Pts',(18.1791643074843,-16.9086974173438,
18.2533055816813));
#180287=CARTESIAN_POINT('Ctrl Pts',(18.2132139978124,-16.8997549375528,
18.2554683985051));
#180288=CARTESIAN_POINT('Ctrl Pts',(18.3030415105969,-16.8785429190307,
18.2612097537341));
#180289=CARTESIAN_POINT('Ctrl Pts',(18.3591176582475,-16.867674735274,18.2648299754842));
#180290=CARTESIAN_POINT('Ctrl Pts',(18.565926584198,-16.8362085130913,18.2782974231191));
#180291=CARTESIAN_POINT('Ctrl Pts',(18.7183156812933,-16.8296028862274,
18.2884830967201));
#180292=CARTESIAN_POINT('Ctrl Pts',(18.8925923659588,-16.8408281484325,
18.2998897592546));
#180293=CARTESIAN_POINT('Ctrl Pts',(18.9150854607903,-16.8426384302645,
18.3013563651973));
#180294=CARTESIAN_POINT('Ctrl Pts',(18.9886367327381,-16.8497431724784,
18.3061256908033));
#180295=CARTESIAN_POINT('Ctrl Pts',(19.0395359702751,-16.8565352923416,
18.3093846572935));
#180296=CARTESIAN_POINT('Ctrl Pts',(19.0979044103317,-16.8664965623328,
18.313036717202));
#180297=CARTESIAN_POINT('Ctrl Pts',(19.1056594076537,-16.8678646163246,
18.3135201862963));
#180298=CARTESIAN_POINT('Ctrl Pts',(19.1180124860542,-16.8701149581386,
18.3142873174329));
#180299=CARTESIAN_POINT('Ctrl Pts',(19.1226154997471,-16.8709692670943,
18.3145725017371));
#180300=CARTESIAN_POINT('Ctrl Pts',(19.1307460827797,-16.8725062022651,
18.315075018466));
#180301=CARTESIAN_POINT('Ctrl Pts',(19.1342747962258,-16.8731825483529,
18.3152927044161));
#180302=CARTESIAN_POINT('Ctrl Pts',(19.1417318290641,-16.8746315243847,
18.3157518485651));
#180303=CARTESIAN_POINT('Ctrl Pts',(19.1456596764027,-16.8754063133708,
18.315993182057));
#180304=CARTESIAN_POINT('Ctrl Pts',(19.1562137929178,-16.8775192913628,
18.3166403252247));
#180305=CARTESIAN_POINT('Ctrl Pts',(19.1628359541204,-16.8788780969971,
18.3170449741432));
#180306=CARTESIAN_POINT('Ctrl Pts',(19.1951516894006,-16.8856704536718,
18.3190132925926));
#180307=CARTESIAN_POINT('Ctrl Pts',(19.2207503853085,-16.8915503209158,
18.320552870753));
#180308=CARTESIAN_POINT('Ctrl Pts',(19.2937734347693,-16.9097602473839,
18.3249054532179));
#180309=CARTESIAN_POINT('Ctrl Pts',(19.340889889245,-16.9232627574063,18.3276661414446));
#180310=CARTESIAN_POINT('Ctrl Pts',(19.4793748859793,-16.9682067386742,
18.3357497549167));
#180311=CARTESIAN_POINT('Ctrl Pts',(19.5691064443162,-17.004278741696,18.340951245465));
#180312=CARTESIAN_POINT('Ctrl Pts',(19.7830127616348,-17.1077791966131,
18.3538818185892));
#180313=CARTESIAN_POINT('Ctrl Pts',(19.9034880253291,-17.1817264693793,
18.3616606999173));
#180314=CARTESIAN_POINT('Ctrl Pts',(20.0270784958069,-17.2757419618227,
18.3707579136162));
#180315=CARTESIAN_POINT('Ctrl Pts',(20.0383582927647,-17.2845041421101,
18.3715990264613));
#180316=CARTESIAN_POINT('Ctrl Pts',(20.0561708817946,-17.2986323433455,
18.3729450921797));
#180317=CARTESIAN_POINT('Ctrl Pts',(20.0627618103235,-17.3039246082167,
18.3734471074083));
#180318=CARTESIAN_POINT('Ctrl Pts',(20.0743308976924,-17.3133286567577,
18.3743353854216));
#180319=CARTESIAN_POINT('Ctrl Pts',(20.0793222992395,-17.317424031678,18.3747209828259));
#180320=CARTESIAN_POINT('Ctrl Pts',(20.0896082613464,-17.3259425478382,
18.3755205301221));
#180321=CARTESIAN_POINT('Ctrl Pts',(20.0949000849509,-17.3303688603787,
18.3759346067145));
#180322=CARTESIAN_POINT('Ctrl Pts',(20.1084298887783,-17.3417986482614,
18.3770003927451));
#180323=CARTESIAN_POINT('Ctrl Pts',(20.1166359453447,-17.348839450287,18.3776536332136));
#180324=CARTESIAN_POINT('Ctrl Pts',(20.1506772188183,-17.3785026589924,
18.3803924522826));
#180325=CARTESIAN_POINT('Ctrl Pts',(20.1760128201895,-17.4016880849536,
18.3825014210998));
#180326=CARTESIAN_POINT('Ctrl Pts',(20.2405625543297,-17.4637112869645,
18.388065843649));
#180327=CARTESIAN_POINT('Ctrl Pts',(20.2788398281181,-17.5034824458097,
18.391559854416));
#180328=CARTESIAN_POINT('Ctrl Pts',(20.3882817034996,-17.626472804715,18.4021426913351));
#180329=CARTESIAN_POINT('Ctrl Pts',(20.4545893180642,-17.7137596217042,
18.4093798637376));
#180330=CARTESIAN_POINT('Ctrl Pts',(20.5426716995883,-17.8505327819045,
18.4201260338893));
#180331=CARTESIAN_POINT('Ctrl Pts',(20.5697993579742,-17.8963654025274,
18.4236350106244));
#180332=CARTESIAN_POINT('Ctrl Pts',(20.6009705582955,-17.9538727284765,
18.4278922748696));
#180333=CARTESIAN_POINT('Ctrl Pts',(20.6066778448426,-17.9646222539345,
18.4286819727962));
#180334=CARTESIAN_POINT('Ctrl Pts',(20.6371280927676,-18.023188367161,18.4329494639269));
#180335=CARTESIAN_POINT('Ctrl Pts',(20.6601351117941,-18.0718908135102,
18.4363729718975));
#180336=CARTESIAN_POINT('Ctrl Pts',(20.6846901874173,-18.1294593325879,
18.4402339214409));
#180337=CARTESIAN_POINT('Ctrl Pts',(20.6880687963992,-18.1375182618265,
18.4407702610931));
#180338=CARTESIAN_POINT('Ctrl Pts',(20.693106683554,-18.149746837719,18.4415775823957));
#180339=CARTESIAN_POINT('Ctrl Pts',(20.6948027156616,-18.1539011057223,
18.441850711488));
#180340=CARTESIAN_POINT('Ctrl Pts',(20.6978222163122,-18.1613648085102,
18.4423393539879));
#180341=CARTESIAN_POINT('Ctrl Pts',(20.6991505413169,-18.1646722068587,
18.442555156883));
#180342=CARTESIAN_POINT('Ctrl Pts',(20.7020173757888,-18.1718627979906,
18.4430227446317));
#180343=CARTESIAN_POINT('Ctrl Pts',(20.7035527430864,-18.1757471814812,
18.4432743395604));
#180344=CARTESIAN_POINT('Ctrl Pts',(20.7078298736014,-18.1866624407219,
18.4439786014567));
#180345=CARTESIAN_POINT('Ctrl Pts',(20.7105455848225,-18.193703550998,18.4444297297222));
#180346=CARTESIAN_POINT('Ctrl Pts',(20.7264897761969,-18.2357102130028,
18.4471031370647));
#180347=CARTESIAN_POINT('Ctrl Pts',(20.7388287216077,-18.2710089936091,
18.4492756847059));
#180348=CARTESIAN_POINT('Ctrl Pts',(20.7762282916268,-18.3878484388335,
18.4562831207746));
#180349=CARTESIAN_POINT('Ctrl Pts',(20.7972989726569,-18.4705822758739,
18.4609582264682));
#180350=CARTESIAN_POINT('Ctrl Pts',(20.8467445313053,-18.729145644127,18.47528765741));
#180351=CARTESIAN_POINT('Ctrl Pts',(20.8579961072368,-18.907418831783,18.4848422731155));
#180352=CARTESIAN_POINT('Ctrl Pts',(20.8453858381803,-19.1077524797247,
18.4965085929344));
#180353=CARTESIAN_POINT('Ctrl Pts',(20.843585710898,-19.1304854658528,18.4978447068983));
#180354=CARTESIAN_POINT('Ctrl Pts',(20.8405145062713,-19.1626565346894,
18.499754658173));
#180355=CARTESIAN_POINT('Ctrl Pts',(20.8395464017098,-19.1721224352315,
18.500318984759));
#180356=CARTESIAN_POINT('Ctrl Pts',(20.8378680474266,-19.1875074856109,
18.5012401334012));
#180357=CARTESIAN_POINT('Ctrl Pts',(20.8371965449799,-19.1934307951084,
18.5015957311858));
#180358=CARTESIAN_POINT('Ctrl Pts',(20.8357371187209,-19.2058360087118,
18.5023424896483));
#180359=CARTESIAN_POINT('Ctrl Pts',(20.8349442072579,-19.2123172526645,
18.5027338041273));
#180360=CARTESIAN_POINT('Ctrl Pts',(20.8329836830202,-19.2277498652794,
18.5036683860005));
#180361=CARTESIAN_POINT('Ctrl Pts',(20.8317887815874,-19.2366975828618,
18.5042125102485));
#180362=CARTESIAN_POINT('Ctrl Pts',(20.8275553119192,-19.2669240739115,
18.5060584263487));
#180363=CARTESIAN_POINT('Ctrl Pts',(20.8242499870448,-19.2881635830734,
18.5073686159888));
#180364=CARTESIAN_POINT('Ctrl Pts',(20.7903285634653,-19.4862368617905,
18.5197137797789));
#180365=CARTESIAN_POINT('Ctrl Pts',(20.7376707225816,-19.6585228129816,
18.5314928065808));
#180366=CARTESIAN_POINT('Ctrl Pts',(20.6144200890412,-19.9319123596205,
18.5513053303523));
#180367=CARTESIAN_POINT('Ctrl Pts',(20.5556040619444,-20.0373447850727,
18.5592365127184));
#180368=CARTESIAN_POINT('Ctrl Pts',(20.4828132041204,-20.1450765017447,
18.5672667690492));
#180369=CARTESIAN_POINT('Ctrl Pts',(20.4774442085239,-20.1529085982732,
18.5678500457554));
#180370=CARTESIAN_POINT('Ctrl Pts',(20.4694073228555,-20.1644650118824,
18.5687095838543));
#180371=CARTESIAN_POINT('Ctrl Pts',(20.4667798352359,-20.168217096069,18.5689884815663));
#180372=CARTESIAN_POINT('Ctrl Pts',(20.4620818638478,-20.1748797280888,
18.5694833719108));
#180373=CARTESIAN_POINT('Ctrl Pts',(20.4600161760259,-20.1777935871438,
18.5696996861153));
#180374=CARTESIAN_POINT('Ctrl Pts',(20.4555575211057,-20.1840493477613,
18.570163817757));
#180375=CARTESIAN_POINT('Ctrl Pts',(20.4531622003528,-20.1873895026806,
18.5704114696076));
#180376=CARTESIAN_POINT('Ctrl Pts',(20.4465195932349,-20.1965955528215,
18.5710936534573));
#180377=CARTESIAN_POINT('Ctrl Pts',(20.4422518654122,-20.2024467262059,
18.5715267983814));
#180378=CARTESIAN_POINT('Ctrl Pts',(20.418642073164,-20.2344699468653,18.5738956669682));
#180379=CARTESIAN_POINT('Ctrl Pts',(20.3987273804613,-20.2602167596331,
18.5757939322477));
#180380=CARTESIAN_POINT('Ctrl Pts',(20.2757569702404,-20.4118416322731,
18.587002813859));
#180381=CARTESIAN_POINT('Ctrl Pts',(20.1590564167636,-20.525968930747,18.5956012035725));
#180382=CARTESIAN_POINT('Ctrl Pts',(19.9380286479564,-20.6971828982146,
18.610907039946));
#180383=CARTESIAN_POINT('Ctrl Pts',(19.8398780886808,-20.7609711771762,
18.6174315818076));
#180384=CARTESIAN_POINT('Ctrl Pts',(19.7244080862297,-20.8230917722246,
18.6251132076641));
#180385=CARTESIAN_POINT('Ctrl Pts',(19.7117745495097,-20.8297245572347,
18.6259534874781));
#180386=CARTESIAN_POINT('Ctrl Pts',(19.691555525141,-20.8400804523968,18.6272984691493));
#180387=CARTESIAN_POINT('Ctrl Pts',(19.6840129931034,-20.8438868063997,
18.6278002408497));
#180388=CARTESIAN_POINT('Ctrl Pts',(19.6706671524227,-20.85052187853,18.6286882352782));
#180389=CARTESIAN_POINT('Ctrl Pts',(19.6648732775618,-20.8533694058181,
18.6290737939911));
#180390=CARTESIAN_POINT('Ctrl Pts',(19.6528595246483,-20.8592057553701,
18.6298734058691));
#180391=CARTESIAN_POINT('Ctrl Pts',(19.6466378831849,-20.8621907527196,
18.630287586449));
#180392=CARTESIAN_POINT('Ctrl Pts',(19.6306234291891,-20.8697780125836,
18.6313539454941));
#180393=CARTESIAN_POINT('Ctrl Pts',(19.6208098143493,-20.874335669358,18.6320076581667));
#180394=CARTESIAN_POINT('Ctrl Pts',(19.5796456580451,-20.8930709090781,
18.6347510614082));
#180395=CARTESIAN_POINT('Ctrl Pts',(19.5479882159574,-20.9065577042136,
18.6368642402159));
#180396=CARTESIAN_POINT('Ctrl Pts',(19.4646003260422,-20.9397056260535,
18.6424424270416));
#180397=CARTESIAN_POINT('Ctrl Pts',(19.4124053896095,-20.9581195849772,
18.6459462303035));
#180398=CARTESIAN_POINT('Ctrl Pts',(19.2548630933418,-21.0068476894645,
18.6565478666252));
#180399=CARTESIAN_POINT('Ctrl Pts',(19.1478245025441,-21.0310486308391,
18.6637939813457));
#180400=CARTESIAN_POINT('Ctrl Pts',(18.9796595985377,-21.0555649677902,
18.6750194532467));
#180401=CARTESIAN_POINT('Ctrl Pts',(18.9195680272076,-21.0617154450963,
18.6789972395196));
#180402=CARTESIAN_POINT('Ctrl Pts',(18.8011480408859,-21.0687363924581,
18.6866874927192));
#180403=CARTESIAN_POINT('Ctrl Pts',(18.7428788892897,-21.0697828704326,
18.6904010721149));
#180404=CARTESIAN_POINT('Ctrl Pts',(18.6757329433062,-21.068216730707,18.694545712184));
#180405=CARTESIAN_POINT('Ctrl Pts',(18.6668314596741,-21.0679529046746,
18.6950924210869));
#180406=CARTESIAN_POINT('Ctrl Pts',(18.6534118171392,-21.0674703970495,
18.6959122202519));
#180407=CARTESIAN_POINT('Ctrl Pts',(18.6488923895553,-21.0672933960876,
18.6961875561341));
#180408=CARTESIAN_POINT('Ctrl Pts',(18.6408099464247,-21.0669509062252,
18.6966785703841));
#180409=CARTESIAN_POINT('Ctrl Pts',(18.6372467617224,-21.0667908958869,
18.6968945505375));
#180410=CARTESIAN_POINT('Ctrl Pts',(18.6295383728568,-21.0664252156676,
18.6973607322357));
#180411=CARTESIAN_POINT('Ctrl Pts',(18.6253933770102,-21.0662163622294,
18.697610753483));
#180412=CARTESIAN_POINT('Ctrl Pts',(18.6138349381355,-21.0655998869962,
18.6983061800108));
#180413=CARTESIAN_POINT('Ctrl Pts',(18.6064229018036,-21.065165448356,18.698750108121));
#180414=CARTESIAN_POINT('Ctrl Pts',(18.5637356133649,-21.0624380175422,
18.7012958839528));
#180415=CARTESIAN_POINT('Ctrl Pts',(18.5285176721152,-21.0593006265802,
18.7033533677342));
#180416=CARTESIAN_POINT('Ctrl Pts',(18.4162446755172,-21.04645702772,18.7098219918581));
#180417=CARTESIAN_POINT('Ctrl Pts',(18.3396344792758,-21.0333928980314,
18.7141001833032));
#180418=CARTESIAN_POINT('Ctrl Pts',(18.0791980983001,-20.9740810181825,
18.7286736677836));
#180419=CARTESIAN_POINT('Ctrl Pts',(17.900988834018,-20.9074191197759,18.7387863176717));
#180420=CARTESIAN_POINT('Ctrl Pts',(17.7149090153111,-20.8076974426352,
18.7510701684566));
#180421=CARTESIAN_POINT('Ctrl Pts',(17.695950837639,-20.7971594291215,18.7523419856698));
#180422=CARTESIAN_POINT('Ctrl Pts',(17.6698873657972,-20.7821430870851,
18.7541202974416));
#180423=CARTESIAN_POINT('Ctrl Pts',(17.6626413651777,-20.7779107563037,
18.7546179383417));
#180424=CARTESIAN_POINT('Ctrl Pts',(17.6502060398234,-20.7705478764707,
18.7554776666709));
#180425=CARTESIAN_POINT('Ctrl Pts',(17.645004606854,-20.7674378974956,18.7558390035255));
#180426=CARTESIAN_POINT('Ctrl Pts',(17.6343982077823,-20.7610342616876,
18.7565793983152));
#180427=CARTESIAN_POINT('Ctrl Pts',(17.6289945197368,-20.7577386158154,
18.7569585265789));
#180428=CARTESIAN_POINT('Ctrl Pts',(17.6164855843831,-20.7500323879735,
18.7578406668203));
#180429=CARTESIAN_POINT('Ctrl Pts',(17.609391566976,-20.7456038599841,18.7583443370504));
#180430=CARTESIAN_POINT('Ctrl Pts',(17.5945073694618,-20.7361891971656,
18.7594083542173));
#180431=CARTESIAN_POINT('Ctrl Pts',(17.5867232704195,-20.7311938196375,
18.7599690379269));
#180432=CARTESIAN_POINT('Ctrl Pts',(17.5312962851622,-20.6951090519398,
18.7639920475868));
#180433=CARTESIAN_POINT('Ctrl Pts',(17.4848948086058,-20.6621639231155,
18.7675237217266));
#180434=CARTESIAN_POINT('Ctrl Pts',(17.3461891787905,-20.5550237821855,
18.7786068267213));
#180435=CARTESIAN_POINT('Ctrl Pts',(17.25874479068,-20.4749314439539,18.7863698760382));
#180436=CARTESIAN_POINT('Ctrl Pts',(17.091001679314,-20.2932198850077,18.802708512097));
#180437=CARTESIAN_POINT('Ctrl Pts',(17.0123728631016,-20.1906768202147,
18.8112605488916));
#180438=CARTESIAN_POINT('Ctrl Pts',(16.9351302367768,-20.0682464606865,
18.8202923621346));
#180439=CARTESIAN_POINT('Ctrl Pts',(16.9268499817913,-20.0547907469947,
18.8212699336696));
#180440=CARTESIAN_POINT('Ctrl Pts',(16.915733185637,-20.0362640405035,18.8225941057163));
#180441=CARTESIAN_POINT('Ctrl Pts',(16.9127659692592,-20.0312725906094,
18.8229487229113));
#180442=CARTESIAN_POINT('Ctrl Pts',(16.9080867052436,-20.0233268863816,
18.8235097557657));
#180443=CARTESIAN_POINT('Ctrl Pts',(16.9063612281725,-20.0203806332709,
18.823717032333));
#180444=CARTESIAN_POINT('Ctrl Pts',(16.9028150096578,-20.0142917312017,
18.8241438287768));
#180445=CARTESIAN_POINT('Ctrl Pts',(16.9009952269551,-20.0111485699262,
18.8243632811183));
#180446=CARTESIAN_POINT('Ctrl Pts',(16.8966826662816,-20.0036554336294,
18.8248844213262));
#180447=CARTESIAN_POINT('Ctrl Pts',(16.8941972158079,-19.9993012232976,
18.8251856366385));
#180448=CARTESIAN_POINT('Ctrl Pts',(16.8858866529192,-19.9846212316007,
18.8261958838662));
#180449=CARTESIAN_POINT('Ctrl Pts',(16.8801326941077,-19.9742551434205,
18.8269004931045));
#180450=CARTESIAN_POINT('Ctrl Pts',(16.8159013534574,-19.8562125225849,
18.8348315484422));
#180451=CARTESIAN_POINT('Ctrl Pts',(16.7667827704242,-19.7436865297984,
18.841530865915));
#180452=CARTESIAN_POINT('Ctrl Pts',(16.6748842569598,-19.470747069851,18.857190033624));
#180453=CARTESIAN_POINT('Ctrl Pts',(16.6406595988271,-19.3083368764714,
18.8661051454986));
#180454=CARTESIAN_POINT('Ctrl Pts',(16.6232302279499,-19.1165532282056,
18.8772499173543));
#180455=CARTESIAN_POINT('Ctrl Pts',(16.6212927645111,-19.08945847855,18.8788369280021));
#180456=CARTESIAN_POINT('Ctrl Pts',(16.6193445967408,-19.0521296862209,
18.8810434740439));
#180457=CARTESIAN_POINT('Ctrl Pts',(16.6188859028437,-19.041920960038,18.8816489824037));
#180458=CARTESIAN_POINT('Ctrl Pts',(16.6182717243159,-19.0256205837814,
18.8826192351296));
#180459=CARTESIAN_POINT('Ctrl Pts',(16.6180685938325,-19.0195308084167,
18.8829824827062));
#180460=CARTESIAN_POINT('Ctrl Pts',(16.6177137006813,-19.0073076836854,
18.8837131443583));
#180461=CARTESIAN_POINT('Ctrl Pts',(16.6175623044064,-19.0011743835767,
18.884080566321));
#180462=CARTESIAN_POINT('Ctrl Pts',(16.6172825438711,-18.9874168809957,
18.8849065358592));
#180463=CARTESIAN_POINT('Ctrl Pts',(16.6171687078937,-18.9797924976334,
18.8853655343681));
#180464=CARTESIAN_POINT('Ctrl Pts',(16.6170306367622,-18.965299883049,18.8862404332388));
#180465=CARTESIAN_POINT('Ctrl Pts',(16.6169986298212,-18.9584318228613,
18.8866560826862));
#180466=CARTESIAN_POINT('Ctrl Pts',(16.6170000449379,-18.9515638040726,
18.8870727812038));
#180467=CARTESIAN_POINT('Ctrl Pts',(16.6170000447709,-18.9515646150098,
18.8870727320024));
#180468=CARTESIAN_POINT('Ctrl Pts',(16.6170019870511,-18.9421205433658,
18.8876457254658));
#180469=CARTESIAN_POINT('Ctrl Pts',(16.6170671251749,-18.9326766817956,
18.8882206949119));
#180470=CARTESIAN_POINT('Ctrl Pts',(16.6174515758742,-18.9043864311521,
18.8899491569953));
#180471=CARTESIAN_POINT('Ctrl Pts',(16.6179593948816,-18.885543960166,18.891108465017));
#180472=CARTESIAN_POINT('Ctrl Pts',(16.6223792669253,-18.7759249068819,
18.8979010800054));
#180473=CARTESIAN_POINT('Ctrl Pts',(16.631880159825,-18.6854794754026,18.9037040531802));
#180474=CARTESIAN_POINT('Ctrl Pts',(16.6686806511801,-18.4697987853706,
18.9179617591797));
#180475=CARTESIAN_POINT('Ctrl Pts',(16.7015809841445,-18.3459488760637,
18.9265076073661));
#180476=CARTESIAN_POINT('Ctrl Pts',(16.7454194046824,-18.2258896668368,
18.9348454761515));
#180477=CARTESIAN_POINT('Origin',(18.734,-18.952,0.));
#180478=CARTESIAN_POINT('',(16.7454193686617,-18.225889765486,19.9537492327042));
#180479=CARTESIAN_POINT('',(16.7454194015149,-18.2258896755116,19.7345260518445));
#180480=CARTESIAN_POINT('',(16.7454193692319,-18.2258897639242,0.));
#180481=CARTESIAN_POINT('',(16.6200858807113,-18.9511715411787,19.9109956519321));
#180482=CARTESIAN_POINT('Ctrl Pts',(16.7454193686617,-18.225889765486,19.9537492327042));
#180483=CARTESIAN_POINT('Ctrl Pts',(16.7274346678508,-18.2751440329415,
19.9507625194471));
#180484=CARTESIAN_POINT('Ctrl Pts',(16.7112837739167,-18.3250558959446,
19.9478475512712));
#180485=CARTESIAN_POINT('Ctrl Pts',(16.6439835682757,-18.5628628691546,
19.9342646472639));
#180486=CARTESIAN_POINT('Ctrl Pts',(16.6170670032748,-18.7565969919825,
19.9239833310379));
#180487=CARTESIAN_POINT('Ctrl Pts',(16.6170001249218,-18.951272731851,19.9127739724915));
#180488=CARTESIAN_POINT('Ctrl Pts',(16.7477768045735,-18.2267292102227,
19.1554367670381));
#180489=CARTESIAN_POINT('Ctrl Pts',(16.8351529008212,-17.9823751202301,
19.1710019290282));
#180490=CARTESIAN_POINT('Ctrl Pts',(17.3199689890727,-17.1326716746796,
19.2289590265787));
#180491=CARTESIAN_POINT('Ctrl Pts',(19.0938031787897,-16.4747288712945,
19.3293080596899));
#180492=CARTESIAN_POINT('Ctrl Pts',(21.0117476238401,-17.913637640173,19.4564838663712));
#180493=CARTESIAN_POINT('Ctrl Pts',(20.8399999988753,-20.3051794704029,
19.5836596730529));
#180494=CARTESIAN_POINT('Ctrl Pts',(18.7361280843894,-21.4552630390637,
19.7108354797341));
#180495=CARTESIAN_POINT('Ctrl Pts',(16.9296977662697,-20.4717617465338,
19.8199301623759));
#180496=CARTESIAN_POINT('Ctrl Pts',(16.6216055049255,-19.3568003466498,
19.8866329094569));
#180497=CARTESIAN_POINT('Ctrl Pts',(16.6201759917111,-18.9511685861838,
19.9109437209775));
#180498=CARTESIAN_POINT('Ctrl Pts',(16.7454194046824,-18.2258896668368,
18.9348454761515));
#180499=CARTESIAN_POINT('Ctrl Pts',(16.7570884628114,-18.1939319029804,
18.9370648780901));
#180500=CARTESIAN_POINT('Ctrl Pts',(16.7695325581869,-18.1622426395963,
18.9392681509443));
#180501=CARTESIAN_POINT('Ctrl Pts',(16.7978320888527,-18.094995909626,18.9439304994503));
#180502=CARTESIAN_POINT('Ctrl Pts',(16.8139071802867,-18.059561655898,18.946379141603));
#180503=CARTESIAN_POINT('Ctrl Pts',(16.8342943057911,-18.0177272746171,
18.9492432259045));
#180504=CARTESIAN_POINT('Ctrl Pts',(16.8376749300514,-18.0108844474981,
18.949710824525));
#180505=CARTESIAN_POINT('Ctrl Pts',(16.8429711197998,-18.0003086765001,
18.9504319722154));
#180506=CARTESIAN_POINT('Ctrl Pts',(16.8448608599526,-17.9965629737017,
18.950687085914));
#180507=CARTESIAN_POINT('Ctrl Pts',(16.848375936133,-17.9896468514508,18.9511575399267));
#180508=CARTESIAN_POINT('Ctrl Pts',(16.8499981269829,-17.9864749430819,
18.951373067141));
#180509=CARTESIAN_POINT('Ctrl Pts',(16.8536706109008,-17.9793385437404,
18.9518574579925));
#180510=CARTESIAN_POINT('Ctrl Pts',(16.8557254323329,-17.9753764444285,
18.9521260322908));
#180511=CARTESIAN_POINT('Ctrl Pts',(16.8610264414634,-17.9652336718004,
18.9528127264605));
#180512=CARTESIAN_POINT('Ctrl Pts',(16.8642907288321,-17.9590624481791,
18.953229730566));
#180513=CARTESIAN_POINT('Ctrl Pts',(16.8837668644529,-17.9226788929136,
18.9556841506719));
#180514=CARTESIAN_POINT('Ctrl Pts',(16.9006812294319,-17.8928460053321,
18.9576798978954));
#180515=CARTESIAN_POINT('Ctrl Pts',(16.9273135936181,-17.8484241948838,
18.960646065502));
#180516=CARTESIAN_POINT('Ctrl Pts',(16.9364993136674,-17.8335248586289,
18.9616399630232));
#180517=CARTESIAN_POINT('Ctrl Pts',(16.9793498503821,-17.7659124593839,
18.9661536890462));
#180518=CARTESIAN_POINT('Ctrl Pts',(17.0151572734018,-17.7145908870264,
18.9695902490886));
#180519=CARTESIAN_POINT('Ctrl Pts',(17.1378438074485,-17.5543720561936,
18.9805947905333));
#180520=CARTESIAN_POINT('Ctrl Pts',(17.2331970839525,-17.4524442963095,
18.9880574999124));
#180521=CARTESIAN_POINT('Ctrl Pts',(17.3845634027533,-17.3196492618426,
18.9993996751176));
#180522=CARTESIAN_POINT('Ctrl Pts',(17.4330378580147,-17.2807595921025,
19.0029643204398));
#180523=CARTESIAN_POINT('Ctrl Pts',(17.4907758960535,-17.2384737522687,
19.0071712870023));
#180524=CARTESIAN_POINT('Ctrl Pts',(17.4984402103519,-17.2329391005084,
19.0077289452487));
#180525=CARTESIAN_POINT('Ctrl Pts',(17.5128019793564,-17.222713658795,19.0087725980823));
#180526=CARTESIAN_POINT('Ctrl Pts',(17.5194900581518,-17.218009961449,19.0092580879349));
#180527=CARTESIAN_POINT('Ctrl Pts',(17.5314545473805,-17.2096985655876,
19.0101257429806));
#180528=CARTESIAN_POINT('Ctrl Pts',(17.5367203901491,-17.2060757781551,
19.0105073267565));
#180529=CARTESIAN_POINT('Ctrl Pts',(17.5469361783478,-17.1991154847975,
19.0112470798994));
#180530=CARTESIAN_POINT('Ctrl Pts',(17.5518839993482,-17.1957749574213,
19.0116051298251));
#180531=CARTESIAN_POINT('Ctrl Pts',(17.5647943129503,-17.187137819406,19.0125388137285));
#180532=CARTESIAN_POINT('Ctrl Pts',(17.5727786175947,-17.1818741989703,
19.0131156816155));
#180533=CARTESIAN_POINT('Ctrl Pts',(17.6001202371883,-17.1641139434264,
19.015089383579));
#180534=CARTESIAN_POINT('Ctrl Pts',(17.6196452446085,-17.1518796481589,
19.0164959082361));
#180535=CARTESIAN_POINT('Ctrl Pts',(17.788848981634,-17.0496650427208,19.0286642816667));
#180536=CARTESIAN_POINT('Ctrl Pts',(17.9489055021189,-16.9782238591999,
19.0401221716249));
#180537=CARTESIAN_POINT('Ctrl Pts',(18.1996624686206,-16.901671424279,19.0574454787337));
#180538=CARTESIAN_POINT('Ctrl Pts',(18.2849636857144,-16.8813160099883,
19.0632207210498));
#180539=CARTESIAN_POINT('Ctrl Pts',(18.4086969013825,-16.8597980877337,
19.0712401370994));
#180540=CARTESIAN_POINT('Ctrl Pts',(18.4462794366656,-16.8542992969227,
19.0736289775107));
#180541=CARTESIAN_POINT('Ctrl Pts',(18.4915193594574,-16.8489190220765,
19.0764325174345));
#180542=CARTESIAN_POINT('Ctrl Pts',(18.4990514862175,-16.8480642451338,
19.0768969000997));
#180543=CARTESIAN_POINT('Ctrl Pts',(18.5107480644012,-16.8468004655189,
19.0776141632025));
#180544=CARTESIAN_POINT('Ctrl Pts',(18.5149093224702,-16.8463633308553,
19.0778685820089));
#180545=CARTESIAN_POINT('Ctrl Pts',(18.5226170493732,-16.8455767407218,
19.0783383903923));
#180546=CARTESIAN_POINT('Ctrl Pts',(18.5261630740572,-16.8452239056892,
19.0785539627899));
#180547=CARTESIAN_POINT('Ctrl Pts',(18.5341667015867,-16.8444479362959,
19.0790392551567));
#180548=CARTESIAN_POINT('Ctrl Pts',(18.5386247531142,-16.8440299902206,
19.0793086809283));
#180549=CARTESIAN_POINT('Ctrl Pts',(18.5517426478401,-16.8428421486321,
19.0800989592126));
#180550=CARTESIAN_POINT('Ctrl Pts',(18.5604060672873,-16.8421114397183,
19.0806176627257));
#180551=CARTESIAN_POINT('Ctrl Pts',(18.621734271462,-16.8373190658068,19.0842683445178));
#180552=CARTESIAN_POINT('Ctrl Pts',(18.6745350045372,-16.8351759746401,
19.087300940387));
#180553=CARTESIAN_POINT('Ctrl Pts',(18.7465911725506,-16.8349501398834,
19.0913550533332));
#180554=CARTESIAN_POINT('Ctrl Pts',(18.7658176456134,-16.8351517965832,
19.0924285875697));
#180555=CARTESIAN_POINT('Ctrl Pts',(18.9163107073358,-16.8387811128402,
19.1007848648068));
#180556=CARTESIAN_POINT('Ctrl Pts',(19.0470061788596,-16.8541532531974,
19.1077814410658));
#180557=CARTESIAN_POINT('Ctrl Pts',(19.2706276321882,-16.9018310986907,
19.1203476264407));
#180558=CARTESIAN_POINT('Ctrl Pts',(19.3642927990027,-16.9286637675744,
19.1257988761686));
#180559=CARTESIAN_POINT('Ctrl Pts',(19.4760991229478,-16.9692127324013,
19.13272265801));
#180560=CARTESIAN_POINT('Ctrl Pts',(19.4963097525252,-16.9768948769489,
19.133991102269));
#180561=CARTESIAN_POINT('Ctrl Pts',(19.5248063821402,-16.9882291022287,
19.1358050821958));
#180562=CARTESIAN_POINT('Ctrl Pts',(19.5331924922735,-16.9916270177871,
19.1363420724951));
#180563=CARTESIAN_POINT('Ctrl Pts',(19.5475959053332,-16.9975708278052,
19.1372699398318));
#180564=CARTESIAN_POINT('Ctrl Pts',(19.5536237242554,-17.0000910278747,
19.1376599422343));
#180565=CARTESIAN_POINT('Ctrl Pts',(19.5651249942043,-17.0049623194101,
19.1384073568916));
#180566=CARTESIAN_POINT('Ctrl Pts',(19.570600385019,-17.0073086928032,19.1387646054515));
#180567=CARTESIAN_POINT('Ctrl Pts',(19.5847740770105,-17.0134534934314,
19.1396931323328));
#180568=CARTESIAN_POINT('Ctrl Pts',(19.5934567955743,-17.0172873339447,
19.1402656177185));
#180569=CARTESIAN_POINT('Ctrl Pts',(19.6227796478703,-17.0304711371218,
19.1422116434207));
#180570=CARTESIAN_POINT('Ctrl Pts',(19.6432947914618,-17.0400937907563,
19.1435945208269));
#180571=CARTESIAN_POINT('Ctrl Pts',(19.8251074307862,-17.1289613839584,
19.1560466407167));
#180572=CARTESIAN_POINT('Ctrl Pts',(19.9758290028525,-17.2281030094809,
19.1678585491742));
#180573=CARTESIAN_POINT('Ctrl Pts',(20.1760214330389,-17.3997968032999,
19.1852794517686));
#180574=CARTESIAN_POINT('Ctrl Pts',(20.2365392085328,-17.4583004514745,
19.1908145653132));
#180575=CARTESIAN_POINT('Ctrl Pts',(20.3184928357187,-17.5475620548898,
19.1985462418226));
#180576=CARTESIAN_POINT('Ctrl Pts',(20.3428465080606,-17.5755274105513,
19.2008771376845));
#180577=CARTESIAN_POINT('Ctrl Pts',(20.3712479842207,-17.6099252197752,
19.2036218635466));
#180578=CARTESIAN_POINT('Ctrl Pts',(20.3760103807324,-17.6157561633335,
19.2040830333732));
#180579=CARTESIAN_POINT('Ctrl Pts',(20.3833639932923,-17.6248583985714,
19.2047964138572));
#180580=CARTESIAN_POINT('Ctrl Pts',(20.3859767582418,-17.628112088002,19.2050501368392));
#180581=CARTESIAN_POINT('Ctrl Pts',(20.3908035467717,-17.6341594506911,
19.2055193042174));
#180582=CARTESIAN_POINT('Ctrl Pts',(20.3930201151048,-17.636950965186,19.2057349273356));
#180583=CARTESIAN_POINT('Ctrl Pts',(20.3980142547639,-17.6432732369954,
19.2062211473178));
#180584=CARTESIAN_POINT('Ctrl Pts',(20.4007876371128,-17.6468072349708,
19.206491445015));
#180585=CARTESIAN_POINT('Ctrl Pts',(20.4079005676947,-17.6559305725278,
19.2071854994357));
#180586=CARTESIAN_POINT('Ctrl Pts',(20.4122234191288,-17.6615329411301,
19.2076080995231));
#180587=CARTESIAN_POINT('Ctrl Pts',(20.4382099911459,-17.6955626851827,
19.2101540703532));
#180588=CARTESIAN_POINT('Ctrl Pts',(20.4591804384396,-17.7245150862502,
19.2122321053226));
#180589=CARTESIAN_POINT('Ctrl Pts',(20.4908383183962,-17.7706380626517,
19.2154308753774));
#180590=CARTESIAN_POINT('Ctrl Pts',(20.5020290720741,-17.7874528134322,
19.2165746493271));
#180591=CARTESIAN_POINT('Ctrl Pts',(20.5195033725233,-17.8145415947981,
19.2183861563385));
#180592=CARTESIAN_POINT('Ctrl Pts',(20.525942642236,-17.8247132167781,19.219059498116));
#180593=CARTESIAN_POINT('Ctrl Pts',(20.6129380321566,-17.9647623394819,
19.2282445481));
#180594=CARTESIAN_POINT('Ctrl Pts',(20.6792881132402,-18.1029389149436,
19.236334340286));
#180595=CARTESIAN_POINT('Ctrl Pts',(20.7506393516376,-18.3049850530612,
19.2481914398177));
#180596=CARTESIAN_POINT('Ctrl Pts',(20.7685626158003,-18.3637681306169,
19.2516394576249));
#180597=CARTESIAN_POINT('Ctrl Pts',(20.7931692537302,-18.4591642522932,
19.2572939947741));
#180598=CARTESIAN_POINT('Ctrl Pts',(20.801488339313,-18.4953197946267,19.2594500538526));
#180599=CARTESIAN_POINT('Ctrl Pts',(20.8110603208846,-18.5425698803645,
19.2622919772058));
#180600=CARTESIAN_POINT('Ctrl Pts',(20.8131817854244,-18.5534831302344,
19.2629500240045));
#180601=CARTESIAN_POINT('Ctrl Pts',(20.8164925494308,-18.5712608387683,
19.2640248641374));
#180602=CARTESIAN_POINT('Ctrl Pts',(20.817734114491,-18.5781154380642,19.2644399870978));
#180603=CARTESIAN_POINT('Ctrl Pts',(20.8200569496059,-18.5913106944204,
19.2652404915197));
#180604=CARTESIAN_POINT('Ctrl Pts',(20.8211431995176,-18.5976504050376,
19.265625709593));
#180605=CARTESIAN_POINT('Ctrl Pts',(20.8235645518027,-18.6121797016758,
19.2665099935391));
#180606=CARTESIAN_POINT('Ctrl Pts',(20.8248804239037,-18.6203723455762,
19.2670096643233));
#180607=CARTESIAN_POINT('Ctrl Pts',(20.8282490302082,-18.6421627671133,
19.2683415437393));
#180608=CARTESIAN_POINT('Ctrl Pts',(20.8302174652415,-18.6557729995072,
19.2691764057548));
#180609=CARTESIAN_POINT('Ctrl Pts',(20.8442539650008,-18.7599819410745,
19.2755923397658));
#180610=CARTESIAN_POINT('Ctrl Pts',(20.8505744557554,-18.8512456133866,
19.2813542853221));
#180611=CARTESIAN_POINT('Ctrl Pts',(20.8516030981444,-19.0834590446548,
19.2963554179827));
#180612=CARTESIAN_POINT('Ctrl Pts',(20.8381706346522,-19.2240026311207,
19.3057703904286));
#180613=CARTESIAN_POINT('Ctrl Pts',(20.8005242380613,-19.4146312952238,
19.3184843007429));
#180614=CARTESIAN_POINT('Ctrl Pts',(20.7881750889048,-19.4666995468883,
19.3219468570176));
#180615=CARTESIAN_POINT('Ctrl Pts',(20.7664135033988,-19.5450941272576,
19.3270930822964));
#180616=CARTESIAN_POINT('Ctrl Pts',(20.7584313696157,-19.571792784749,19.328833542518));
#180617=CARTESIAN_POINT('Ctrl Pts',(20.7478193396684,-19.604892174682,19.3309693567385));
#180618=CARTESIAN_POINT('Ctrl Pts',(20.745682549206,-19.6114466231811,19.3313912148695));
#180619=CARTESIAN_POINT('Ctrl Pts',(20.742244921945,-19.6218190804271,19.3320569578469));
#180620=CARTESIAN_POINT('Ctrl Pts',(20.7409651477704,-19.6256439439981,
19.332302051663));
#180621=CARTESIAN_POINT('Ctrl Pts',(20.7385269507804,-19.6328623659053,
19.3327638133681));
#180622=CARTESIAN_POINT('Ctrl Pts',(20.7373708515019,-19.6362565960473,
19.3329806078123));
#180623=CARTESIAN_POINT('Ctrl Pts',(20.734702778814,-19.6440251518377,19.3334760528216));
#180624=CARTESIAN_POINT('Ctrl Pts',(20.7331850824364,-19.6483974633965,
19.3337543612437));
#180625=CARTESIAN_POINT('Ctrl Pts',(20.7291068209342,-19.6600232633561,
19.3344930240172));
#180626=CARTESIAN_POINT('Ctrl Pts',(20.7265210136035,-19.6672679098113,
19.3349519231628));
#180627=CARTESIAN_POINT('Ctrl Pts',(20.7078196339748,-19.7187750054841,
19.3382056304466));
#180628=CARTESIAN_POINT('Ctrl Pts',(20.6902688878991,-19.7625063981389,
19.3409211871729));
#180629=CARTESIAN_POINT('Ctrl Pts',(20.669489497135,-19.8096648249915,19.3438351235066));
#180630=CARTESIAN_POINT('Ctrl Pts',(20.6676941633895,-19.8137049544192,
19.3440846459375));
#180631=CARTESIAN_POINT('Ctrl Pts',(20.6408105238953,-19.8736954415322,
19.3477883652465));
#180632=CARTESIAN_POINT('Ctrl Pts',(20.6133142530743,-19.9285385677627,
19.3511573717879));
#180633=CARTESIAN_POINT('Ctrl Pts',(20.5796910269915,-19.9889060188677,
19.3549257229204));
#180634=CARTESIAN_POINT('Ctrl Pts',(20.5758701114349,-19.9956780884566,
19.3553493252538));
#180635=CARTESIAN_POINT('Ctrl Pts',(20.5178668649513,-20.0971705871352,
19.3617128901422));
#180636=CARTESIAN_POINT('Ctrl Pts',(20.4564780317384,-20.1875829336354,
19.367589847347));
#180637=CARTESIAN_POINT('Ctrl Pts',(20.341388233038,-20.3317349235385,19.3778487607524));
#180638=CARTESIAN_POINT('Ctrl Pts',(20.2912750959758,-20.3880563862115,
19.3821205113765));
#180639=CARTESIAN_POINT('Ctrl Pts',(20.2250080929037,-20.4549767563713,
19.3876192914436));
#180640=CARTESIAN_POINT('Ctrl Pts',(20.2115678395912,-20.4681917783405,
19.3887272856715));
#180641=CARTESIAN_POINT('Ctrl Pts',(20.1917685395629,-20.4871459834144,
19.3903500300447));
#180642=CARTESIAN_POINT('Ctrl Pts',(20.1855480526442,-20.4930290564791,
19.3908585292913));
#180643=CARTESIAN_POINT('Ctrl Pts',(20.1745788286112,-20.503277939913,19.3917529902637));
#180644=CARTESIAN_POINT('Ctrl Pts',(20.1698454771274,-20.5076601083446,
19.3921382435731));
#180645=CARTESIAN_POINT('Ctrl Pts',(20.1606151615669,-20.5161275819359,
19.392888161763));
#180646=CARTESIAN_POINT('Ctrl Pts',(20.1561204887208,-20.5202152996795,
19.3932527185138));
#180647=CARTESIAN_POINT('Ctrl Pts',(20.145332999645,-20.5299415567236,19.3941262517233));
#180648=CARTESIAN_POINT('Ctrl Pts',(20.1390239366184,-20.5355618480545,
19.3946359892651));
#180649=CARTESIAN_POINT('Ctrl Pts',(20.1161323168404,-20.5557098530103,
19.3964815111889));
#180650=CARTESIAN_POINT('Ctrl Pts',(20.0993571637733,-20.5700156957051,
19.3978264467296));
#180651=CARTESIAN_POINT('Ctrl Pts',(19.9387773062635,-20.7026825455715,
19.4106353225211));
#180652=CARTESIAN_POINT('Ctrl Pts',(19.7801908653824,-20.8018201292752,
19.4229050703923));
#180653=CARTESIAN_POINT('Ctrl Pts',(19.5381705459434,-20.9119372376495,
19.4404587862508));
#180654=CARTESIAN_POINT('Ctrl Pts',(19.4637964908475,-20.9408295622266,
19.4456955606116));
#180655=CARTESIAN_POINT('Ctrl Pts',(19.3538078145852,-20.9765535584202,
19.453066728074));
#180656=CARTESIAN_POINT('Ctrl Pts',(19.3193708288086,-20.9867776747693,
19.4553229482392));
#180657=CARTESIAN_POINT('Ctrl Pts',(19.277485639458,-20.9980615827153,19.4579916528729));
#180658=CARTESIAN_POINT('Ctrl Pts',(19.2702728392629,-20.9999638879231,
19.4584485348146));
#180659=CARTESIAN_POINT('Ctrl Pts',(19.2590241650428,-21.0028671125153,
19.4591567307659));
#180660=CARTESIAN_POINT('Ctrl Pts',(19.2549952249584,-21.0038943109558,
19.4594095226368));
#180661=CARTESIAN_POINT('Ctrl Pts',(19.24750520083,-21.0057804471485,19.4598778411388));
#180662=CARTESIAN_POINT('Ctrl Pts',(19.2440450057794,-21.0066425014399,
19.4600935409866));
#180663=CARTESIAN_POINT('Ctrl Pts',(19.2362012187612,-21.0085756241998,
19.4605810425862));
#180664=CARTESIAN_POINT('Ctrl Pts',(19.2318163818485,-21.0096414199291,
19.4608525383525));
#180665=CARTESIAN_POINT('Ctrl Pts',(19.2204825495345,-21.0123579158214,
19.4615517217026));
#180666=CARTESIAN_POINT('Ctrl Pts',(19.2135284834494,-21.0139874997492,
19.4619782237731));
#180667=CARTESIAN_POINT('Ctrl Pts',(19.170699692491,-21.023795416176,19.464590392434));
#180668=CARTESIAN_POINT('Ctrl Pts',(19.1346226855039,-21.0310730384115,
19.4667279698121));
#180669=CARTESIAN_POINT('Ctrl Pts',(18.9307620373476,-21.066692512723,19.4785481229896));
#180670=CARTESIAN_POINT('Ctrl Pts',(18.7602181738375,-21.0756676543417,
19.4875020264752));
#180671=CARTESIAN_POINT('Ctrl Pts',(18.4950675593476,-21.0576437212988,
19.5021198005965));
#180672=CARTESIAN_POINT('Ctrl Pts',(18.4002682668898,-21.0447121721664,
19.5074782474928));
#180673=CARTESIAN_POINT('Ctrl Pts',(18.2857006089707,-21.0211000927665,
19.5142895682617));
#180674=CARTESIAN_POINT('Ctrl Pts',(18.2647952826919,-21.0164598377371,
19.5155460334569));
#180675=CARTESIAN_POINT('Ctrl Pts',(18.2351957815223,-21.0094169715902,
19.5173458095867));
#180676=CARTESIAN_POINT('Ctrl Pts',(18.2264405937413,-21.0072746017626,
19.517880758738));
#180677=CARTESIAN_POINT('Ctrl Pts',(18.2113694488999,-21.003484562464,19.5188062060002));
#180678=CARTESIAN_POINT('Ctrl Pts',(18.2050468930286,-21.001863461825,19.5191958415977));
#180679=CARTESIAN_POINT('Ctrl Pts',(18.1929617050235,-20.9987051896961,
19.5199433239361));
#180680=CARTESIAN_POINT('Ctrl Pts',(18.1871978655578,-20.9971728520587,
19.5203010107074));
#180681=CARTESIAN_POINT('Ctrl Pts',(18.1722402084362,-20.9931285536587,
19.5212323625708));
#180682=CARTESIAN_POINT('Ctrl Pts',(18.1630568175055,-20.9905788465731,
19.5218072494148));
#180683=CARTESIAN_POINT('Ctrl Pts',(18.1318698663868,-20.981692736647,19.5237702287538));
#180684=CARTESIAN_POINT('Ctrl Pts',(18.109952621851,-20.9750615680731,19.5251678811103));
#180685=CARTESIAN_POINT('Ctrl Pts',(17.9198017559213,-20.9141465473261,
19.5374567768308));
#180686=CARTESIAN_POINT('Ctrl Pts',(17.7589034331837,-20.8393528023252,
19.5490634132886));
#180687=CARTESIAN_POINT('Ctrl Pts',(17.5362480538972,-20.6997114176145,
19.5664271812964));
#180688=CARTESIAN_POINT('Ctrl Pts',(17.4661480575475,-20.649544776782,19.5721005136665));
#180689=CARTESIAN_POINT('Ctrl Pts',(17.3701134078433,-20.5715418365208,
19.5799980714077));
#180690=CARTESIAN_POINT('Ctrl Pts',(17.3415659457476,-20.5470643260711,
19.5823625497969));
#180691=CARTESIAN_POINT('Ctrl Pts',(17.3080786349526,-20.5167665622721,
19.5851413803673));
#180692=CARTESIAN_POINT('Ctrl Pts',(17.3025006794945,-20.5116652952008,
19.5856044240878));
#180693=CARTESIAN_POINT('Ctrl Pts',(17.2938810851329,-20.503697128483,19.5863200693361));
#180694=CARTESIAN_POINT('Ctrl Pts',(17.2908204773602,-20.5008509720533,
19.5865741983557));
#180695=CARTESIAN_POINT('Ctrl Pts',(17.285165605735,-20.4955610126774,19.5870437391401));
#180696=CARTESIAN_POINT('Ctrl Pts',(17.2825691070287,-20.4931197439159,
19.58725933202));
#180697=CARTESIAN_POINT('Ctrl Pts',(17.2767199481496,-20.4875923786542,
19.5877450077469));
#180698=CARTESIAN_POINT('Ctrl Pts',(17.2734709288942,-20.4845025077327,
19.5880147943394));
#180699=CARTESIAN_POINT('Ctrl Pts',(17.2639304891813,-20.475371494255,19.5888071133393));
#180700=CARTESIAN_POINT('Ctrl Pts',(17.2576664704176,-20.4693016811104,
19.5893274800962));
#180701=CARTESIAN_POINT('Ctrl Pts',(17.2133360562671,-20.4258112145312,
19.5930127545472));
#180702=CARTESIAN_POINT('Ctrl Pts',(17.1766560709689,-20.3869979909057,
19.5960761544868));
#180703=CARTESIAN_POINT('Ctrl Pts',(17.1324659651828,-20.3365450123097,
19.5998478774551));
#180704=CARTESIAN_POINT('Ctrl Pts',(17.1235520738394,-20.3261665271839,
19.6006131076102));
#180705=CARTESIAN_POINT('Ctrl Pts',(17.0811100918862,-20.275770895466,19.6042820088651));
#180706=CARTESIAN_POINT('Ctrl Pts',(17.0489682591895,-20.2346078308291,
19.6071384935807));
#180707=CARTESIAN_POINT('Ctrl Pts',(16.9542697434346,-20.1036177398395,
19.6159390347208));
#180708=CARTESIAN_POINT('Ctrl Pts',(16.8971322474374,-20.0101016915657,
19.6218308906142));
#180709=CARTESIAN_POINT('Ctrl Pts',(16.8130787470599,-19.8450279892142,
19.6321302016449));
#180710=CARTESIAN_POINT('Ctrl Pts',(16.7823335280967,-19.7756708576587,
19.6364278337816));
#180711=CARTESIAN_POINT('Ctrl Pts',(16.7486505846779,-19.6871424284868,
19.6419578080245));
#180712=CARTESIAN_POINT('Ctrl Pts',(16.7421624440022,-19.6693770328492,
19.6430695285059));
#180713=CARTESIAN_POINT('Ctrl Pts',(16.7330803286727,-19.6434354462674,
19.6446967392415));
#180714=CARTESIAN_POINT('Ctrl Pts',(16.7302965253059,-19.6353263419915,
19.6452059293288));
#180715=CARTESIAN_POINT('Ctrl Pts',(16.7255041824423,-19.6210853329903,
19.646101189266));
#180716=CARTESIAN_POINT('Ctrl Pts',(16.7234742631018,-19.6149607015629,
19.6464865467384));
#180717=CARTESIAN_POINT('Ctrl Pts',(16.7195884541053,-19.6030545244012,
19.6472363587356));
#180718=CARTESIAN_POINT('Ctrl Pts',(16.7177293756182,-19.5972740797814,
19.6476007036782));
#180719=CARTESIAN_POINT('Ctrl Pts',(16.7133468281112,-19.5834435293021,
19.6484732305761));
#180720=CARTESIAN_POINT('Ctrl Pts',(16.7108465750517,-19.5753862267157,
19.6489821696574));
#180721=CARTESIAN_POINT('Ctrl Pts',(16.7020108021448,-19.5462989944584,
19.6508218507045));
#180722=CARTESIAN_POINT('Ctrl Pts',(16.6959546563939,-19.5251862833178,
19.652161668566));
#180723=CARTESIAN_POINT('Ctrl Pts',(16.641457713617,-19.3234062371902,19.6650134940398));
#180724=CARTESIAN_POINT('Ctrl Pts',(16.6168436525179,-19.1371933084926,
19.6773392583007));
#180725=CARTESIAN_POINT('Ctrl Pts',(16.6170536900537,-18.8872094297229,
19.6938412674434));
#180726=CARTESIAN_POINT('Ctrl Pts',(16.6199199093975,-18.8242283085218,
19.6979837633764));
#180727=CARTESIAN_POINT('Ctrl Pts',(16.6300811408892,-18.711786107144,19.7052635121147));
#180728=CARTESIAN_POINT('Ctrl Pts',(16.636325596411,-18.6622755733997,19.7084278670485));
#180729=CARTESIAN_POINT('Ctrl Pts',(16.6455655237967,-18.6053135180284,
19.7119866163342));
#180730=CARTESIAN_POINT('Ctrl Pts',(16.6468596259147,-18.5976059518692,
19.712466400274));
#180731=CARTESIAN_POINT('Ctrl Pts',(16.6489941842261,-18.5853100717682,
19.7132288067553));
#180732=CARTESIAN_POINT('Ctrl Pts',(16.6498071586553,-18.5807171478172,
19.7135129229699));
#180733=CARTESIAN_POINT('Ctrl Pts',(16.6512728103078,-18.5725934303284,
19.7140142235687));
#180734=CARTESIAN_POINT('Ctrl Pts',(16.6519192986505,-18.5690615642145,
19.7142317557005));
#180735=CARTESIAN_POINT('Ctrl Pts',(16.6533073565544,-18.5615858265706,
19.7146913063151));
#180736=CARTESIAN_POINT('Ctrl Pts',(16.6540511534419,-18.5576424216259,
19.7149331963715));
#180737=CARTESIAN_POINT('Ctrl Pts',(16.6560859627734,-18.5470203405586,
19.7155834147478));
#180738=CARTESIAN_POINT('Ctrl Pts',(16.6573979718081,-18.5403456667975,
19.7159905631367));
#180739=CARTESIAN_POINT('Ctrl Pts',(16.6640292673832,-18.5074484580789,
19.7179906947645));
#180740=CARTESIAN_POINT('Ctrl Pts',(16.66981344442,-18.4813207867021,19.7195586388828));
#180741=CARTESIAN_POINT('Ctrl Pts',(16.6879077563223,-18.4063518552391,
19.7240162613594));
#180742=CARTESIAN_POINT('Ctrl Pts',(16.7014678343997,-18.3578291157312,
19.7268505474143));
#180743=CARTESIAN_POINT('Ctrl Pts',(16.7257202842388,-18.2816443291298,
19.7312843014982));
#180744=CARTESIAN_POINT('Ctrl Pts',(16.7352803842117,-18.2536571543875,
19.7329094646234));
#180745=CARTESIAN_POINT('Ctrl Pts',(16.7454194015149,-18.2258896755116,
19.7345260518445));
#180746=CARTESIAN_POINT('Origin',(18.734,-18.952,0.));
#180747=CARTESIAN_POINT('',(16.7454193641621,-18.2258897778089,20.7554136941352));
#180748=CARTESIAN_POINT('',(16.7454193692319,-18.2258897639242,20.5336910470276));
#180749=CARTESIAN_POINT('',(16.7454193692319,-18.2258897639242,0.));
#180750=CARTESIAN_POINT('Ctrl Pts',(16.7454193641621,-18.2258897778089,
20.7554136941352));
#180751=CARTESIAN_POINT('Ctrl Pts',(16.7360405261122,-18.2515753764448,
20.7536067807895));
#180752=CARTESIAN_POINT('Ctrl Pts',(16.7271552302181,-18.2774539415413,
20.7517981597966));
#180753=CARTESIAN_POINT('Ctrl Pts',(16.6954799886096,-18.3758873131554,
20.7449760055346));
#180754=CARTESIAN_POINT('Ctrl Pts',(16.6761041931915,-18.4494703059319,
20.7399903665825));
#180755=CARTESIAN_POINT('Ctrl Pts',(16.6536719553266,-18.5581190720105,
20.7329253955474));
#180756=CARTESIAN_POINT('Ctrl Pts',(16.647461042645,-18.5924691027361,20.7307344389072));
#180757=CARTESIAN_POINT('Ctrl Pts',(16.6409663520166,-18.6342676419938,
20.7281324118738));
#180758=CARTESIAN_POINT('Ctrl Pts',(16.6398690487731,-18.6415821111108,
20.7276794391764));
#180759=CARTESIAN_POINT('Ctrl Pts',(16.6382167997033,-18.6530034304887,
20.7269759827501));
#180760=CARTESIAN_POINT('Ctrl Pts',(16.6376355527073,-18.6571063309721,
20.7267240521062));
#180761=CARTESIAN_POINT('Ctrl Pts',(16.6365763773783,-18.6647442403221,
20.7262565330955));
#180762=CARTESIAN_POINT('Ctrl Pts',(16.636095341283,-18.6682787152918,20.7260407764863));
#180763=CARTESIAN_POINT('Ctrl Pts',(16.6350235902585,-18.6763053163347,
20.7255521289721));
#180764=CARTESIAN_POINT('Ctrl Pts',(16.6344383625037,-18.6807981222718,
20.7252795503376));
#180765=CARTESIAN_POINT('Ctrl Pts',(16.6327408114509,-18.6941651491507,
20.7244712651555));
#180766=CARTESIAN_POINT('Ctrl Pts',(16.6316702790213,-18.7030447059475,
20.723937857342));
#180767=CARTESIAN_POINT('Ctrl Pts',(16.6239226589407,-18.7709248029828,
20.7198853023156));
#180768=CARTESIAN_POINT('Ctrl Pts',(16.6196735652526,-18.8301816903796,
20.7164920546517));
#180769=CARTESIAN_POINT('Ctrl Pts',(16.6173229632376,-18.9098229033458,
20.7120327871221));
#180770=CARTESIAN_POINT('Ctrl Pts',(16.6170159593102,-18.9301096100837,
20.710905713788));
#180771=CARTESIAN_POINT('Ctrl Pts',(16.6168948154608,-19.0901947037228,
20.7020607995078));
#180772=CARTESIAN_POINT('Ctrl Pts',(16.6306360858099,-19.229658600869,20.694625739485));
#180773=CARTESIAN_POINT('Ctrl Pts',(16.6757501965833,-19.4554694899002,
20.6818794970703));
#180774=CARTESIAN_POINT('Ctrl Pts',(16.6991411812998,-19.5429488037882,
20.6767638054007));
#180775=CARTESIAN_POINT('Ctrl Pts',(16.7324404003773,-19.6416641112144,
20.6706560419502));
#180776=CARTESIAN_POINT('Ctrl Pts',(16.7369541278898,-19.6546273468824,
20.6698472702452));
#180777=CARTESIAN_POINT('Ctrl Pts',(16.744395444465,-19.6753473798551,20.668543378264));
#180778=CARTESIAN_POINT('Ctrl Pts',(16.7472431360756,-19.6831326008422,
20.6680509120219));
#180779=CARTESIAN_POINT('Ctrl Pts',(16.7523808194746,-19.6969266888519,
20.6671737261315));
#180780=CARTESIAN_POINT('Ctrl Pts',(16.7546526140128,-19.7029422564798,
20.6667896188495));
#180781=CARTESIAN_POINT('Ctrl Pts',(16.7594433811066,-19.7154551187021,
20.6659873301412));
#180782=CARTESIAN_POINT('Ctrl Pts',(16.7619670948556,-19.7219505040645,
20.6655689931112));
#180783=CARTESIAN_POINT('Ctrl Pts',(16.7686050596548,-19.7387881655782,
20.664479630898));
#180784=CARTESIAN_POINT('Ctrl Pts',(16.7727688488811,-19.7491105654152,
20.6638069414727));
#180785=CARTESIAN_POINT('Ctrl Pts',(16.791211431219,-19.7938119548698,20.6608723687528));
#180786=CARTESIAN_POINT('Ctrl Pts',(16.8063135223803,-19.8278420853112,
20.6585827070948));
#180787=CARTESIAN_POINT('Ctrl Pts',(16.848825701507,-19.9172037082198,20.6524167066109));
#180788=CARTESIAN_POINT('Ctrl Pts',(16.877770968577,-19.9717612418196,20.648490595315));
#180789=CARTESIAN_POINT('Ctrl Pts',(16.9832805763926,-20.151215140557,20.6350415616405));
#180790=CARTESIAN_POINT('Ctrl Pts',(17.0704030639735,-20.26941241792,20.6252363404938));
#180791=CARTESIAN_POINT('Ctrl Pts',(17.1821608935758,-20.3920922095799,
20.6144037584348));
#180792=CARTESIAN_POINT('Ctrl Pts',(17.1955082976187,-20.4063429784161,
20.6131348438654));
#180793=CARTESIAN_POINT('Ctrl Pts',(17.2456829975289,-20.4584496691791,
20.6084613702613));
#180794=CARTESIAN_POINT('Ctrl Pts',(17.2837289770879,-20.4951114915215,
20.6051052078539));
#180795=CARTESIAN_POINT('Ctrl Pts',(17.3295906236418,-20.5361082253448,
20.6013107228966));
#180796=CARTESIAN_POINT('Ctrl Pts',(17.3361072840997,-20.5418617948689,
20.6007772011702));
#180797=CARTESIAN_POINT('Ctrl Pts',(17.346033606484,-20.5505175425291,20.5999732956802));
#180798=CARTESIAN_POINT('Ctrl Pts',(17.3494172471693,-20.5534492326387,
20.599700790427));
#180799=CARTESIAN_POINT('Ctrl Pts',(17.355510653302,-20.558694998497,20.5992128261721));
#180800=CARTESIAN_POINT('Ctrl Pts',(17.3582169706351,-20.5610129750384,
20.5989970811374));
#180801=CARTESIAN_POINT('Ctrl Pts',(17.3641139142323,-20.5660379857098,
20.5985291096706));
#180802=CARTESIAN_POINT('Ctrl Pts',(17.3673067068545,-20.5687423884035,
20.5982770759103));
#180803=CARTESIAN_POINT('Ctrl Pts',(17.3763062268267,-20.5763195743023,
20.5975703608943));
#180804=CARTESIAN_POINT('Ctrl Pts',(17.382131205714,-20.5811707179265,20.5971172355403));
#180805=CARTESIAN_POINT('Ctrl Pts',(17.4172900636395,-20.6101332159044,
20.5944070748481));
#180806=CARTESIAN_POINT('Ctrl Pts',(17.447244237378,-20.633484709794,20.5922013749046));
#180807=CARTESIAN_POINT('Ctrl Pts',(17.5483208820626,-20.7079974955783,
20.5850329550837));
#180808=CARTESIAN_POINT('Ctrl Pts',(17.6219933520663,-20.7555536645223,
20.5802385223341));
#180809=CARTESIAN_POINT('Ctrl Pts',(17.8507216074712,-20.8838401976737,
20.5659712699388));
#180810=CARTESIAN_POINT('Ctrl Pts',(18.0130032845019,-20.9500851497846,
20.5565783776766));
#180811=CARTESIAN_POINT('Ctrl Pts',(18.2038289333754,-21.0016680788527,
20.545092520438));
#180812=CARTESIAN_POINT('Ctrl Pts',(18.2261825268263,-21.0073203998097,
20.5437418100362));
#180813=CARTESIAN_POINT('Ctrl Pts',(18.2579259868271,-21.0147975844692,
20.5418145682959));
#180814=CARTESIAN_POINT('Ctrl Pts',(18.2672432333167,-21.01692577511,20.5412477863095));
#180815=CARTESIAN_POINT('Ctrl Pts',(18.282402575048,-21.0202805409891,20.5403237114761));
#180816=CARTESIAN_POINT('Ctrl Pts',(18.2882360759247,-21.0215456393437,
20.539967658485));
#180817=CARTESIAN_POINT('Ctrl Pts',(18.3004558097034,-21.0241416433151,
20.5392208255046));
#180818=CARTESIAN_POINT('Ctrl Pts',(18.3068429912705,-21.0254677338496,
20.5388298955966));
#180819=CARTESIAN_POINT('Ctrl Pts',(18.3220483189512,-21.0285513864757,
20.5378978604684));
#180820=CARTESIAN_POINT('Ctrl Pts',(18.3308716806875,-21.0302823202017,
20.5373559108675));
#180821=CARTESIAN_POINT('Ctrl Pts',(18.3606151200208,-21.0359207390981,
20.535525135629));
#180822=CARTESIAN_POINT('Ctrl Pts',(18.3815824968738,-21.03956886522,20.5342280990653));
#180823=CARTESIAN_POINT('Ctrl Pts',(18.5599655130168,-21.0678418563937,
20.523135304694));
#180824=CARTESIAN_POINT('Ctrl Pts',(18.7196138749804,-21.074934203009,20.5127665038184));
#180825=CARTESIAN_POINT('Ctrl Pts',(19.009873038063,-21.0550736888552,20.4935483241033));
#180826=CARTESIAN_POINT('Ctrl Pts',(19.140118218806,-21.0338498936931,20.4848060784439));
#180827=CARTESIAN_POINT('Ctrl Pts',(19.2827905059857,-20.9966921067133,
20.4756083477493));
#180828=CARTESIAN_POINT('Ctrl Pts',(19.2979807394426,-20.9925544809781,
20.4746342744521));
#180829=CARTESIAN_POINT('Ctrl Pts',(19.3187012775334,-20.9866614065457,
20.4733140432787));
#180830=CARTESIAN_POINT('Ctrl Pts',(19.3242721829649,-20.98505223127,20.4729599299371));
#180831=CARTESIAN_POINT('Ctrl Pts',(19.3331114259021,-20.9824595901719,
20.4723994844782));
#180832=CARTESIAN_POINT('Ctrl Pts',(19.3363840699121,-20.9814910890827,
20.4721922947902));
#180833=CARTESIAN_POINT('Ctrl Pts',(19.3431356594666,-20.9794752644625,
20.4717655155514));
#180834=CARTESIAN_POINT('Ctrl Pts',(19.3466142525746,-20.9784268990843,
20.4715459942465));
#180835=CARTESIAN_POINT('Ctrl Pts',(19.3548927264501,-20.975908698818,20.4710244104032));
#180836=CARTESIAN_POINT('Ctrl Pts',(19.3596901480769,-20.9744307253132,
20.4707228225368));
#180837=CARTESIAN_POINT('Ctrl Pts',(19.3758345375252,-20.9693940721196,
20.4697100400223));
#180838=CARTESIAN_POINT('Ctrl Pts',(19.3871570025942,-20.9657567778582,
20.4690032981843));
#180839=CARTESIAN_POINT('Ctrl Pts',(19.5222461879926,-20.9211006942457,
20.4606069815779));
#180840=CARTESIAN_POINT('Ctrl Pts',(19.642017463001,-20.8688212656968,20.4535141585838));
#180841=CARTESIAN_POINT('Ctrl Pts',(19.8982505056643,-20.7275316417389,
20.4376180886874));
#180842=CARTESIAN_POINT('Ctrl Pts',(20.0307851172993,-20.6331701950501,
20.4288393245252));
#180843=CARTESIAN_POINT('Ctrl Pts',(20.1688712790456,-20.5087261798457,
20.4180455884596));
#180844=CARTESIAN_POINT('Ctrl Pts',(20.1862282510867,-20.4925469893425,
20.4166561898094));
#180845=CARTESIAN_POINT('Ctrl Pts',(20.2102696111499,-20.4693696030709,
20.414683107493));
#180846=CARTESIAN_POINT('Ctrl Pts',(20.217183956616,-20.4626117380895,20.4141098213108));
#180847=CARTESIAN_POINT('Ctrl Pts',(20.2283060812245,-20.4515913462797,
20.4131780403851));
#180848=CARTESIAN_POINT('Ctrl Pts',(20.2325425380601,-20.447357860417,20.4128208276019));
#180849=CARTESIAN_POINT('Ctrl Pts',(20.2413435741349,-20.4384880356557,
20.4120738948695));
#180850=CARTESIAN_POINT('Ctrl Pts',(20.2459048526978,-20.4338485231478,
20.4116840353014));
#180851=CARTESIAN_POINT('Ctrl Pts',(20.2566527554761,-20.4228149929531,
20.4107588105762));
#180852=CARTESIAN_POINT('Ctrl Pts',(20.2628205650714,-20.4164028930907,
20.4102226334635));
#180853=CARTESIAN_POINT('Ctrl Pts',(20.2832249136015,-20.3949209760093,
20.4084311950318));
#180854=CARTESIAN_POINT('Ctrl Pts',(20.2972801473271,-20.3796813050984,
20.4071681947257));
#180855=CARTESIAN_POINT('Ctrl Pts',(20.3711099713543,-20.2972322654157,
20.4003745800996));
#180856=CARTESIAN_POINT('Ctrl Pts',(20.4267721943403,-20.2264793467002,
20.3946760389935));
#180857=CARTESIAN_POINT('Ctrl Pts',(20.5545470055131,-20.0408686312935,
20.3800726963549));
#180858=CARTESIAN_POINT('Ctrl Pts',(20.6204508675071,-19.9222194295745,
20.3710222226614));
#180859=CARTESIAN_POINT('Ctrl Pts',(20.7047525840411,-19.7288703172134,
20.3572289567084));
#180860=CARTESIAN_POINT('Ctrl Pts',(20.7312152301385,-19.6580645001745,
20.3523667988651));
#180861=CARTESIAN_POINT('Ctrl Pts',(20.7566813026887,-19.576931562992,20.3471147804785));
#180862=CARTESIAN_POINT('Ctrl Pts',(20.7594632297126,-19.5678553592093,
20.3465316711897));
#180863=CARTESIAN_POINT('Ctrl Pts',(20.7634967477482,-19.5543727474595,
20.3456723340755));
#180864=CARTESIAN_POINT('Ctrl Pts',(20.7647951964889,-19.5499806408494,
20.3453934715943));
#180865=CARTESIAN_POINT('Ctrl Pts',(20.7670808512854,-19.5421559191414,
20.3448986229934));
#180866=CARTESIAN_POINT('Ctrl Pts',(20.7680736320409,-19.5387249925239,
20.3446823154755));
#180867=CARTESIAN_POINT('Ctrl Pts',(20.7701902917305,-19.5313401347524,
20.3442181754018));
#180868=CARTESIAN_POINT('Ctrl Pts',(20.7713113362327,-19.5273854497558,
20.3439705085504));
#180869=CARTESIAN_POINT('Ctrl Pts',(20.7743760289068,-19.5164529453746,
20.3432882291214));
#180870=CARTESIAN_POINT('Ctrl Pts',(20.7762954152734,-19.5094683014143,
20.3428550043192));
#180871=CARTESIAN_POINT('Ctrl Pts',(20.7866465547068,-19.471029450789,20.3404848093727));
#180872=CARTESIAN_POINT('Ctrl Pts',(20.7943880307124,-19.4393919109625,
20.3385853481042));
#180873=CARTESIAN_POINT('Ctrl Pts',(20.8364006996118,-19.2487434345245,
20.3273767205319));
#180874=CARTESIAN_POINT('Ctrl Pts',(20.8529854693216,-19.0863792388588,
20.3187794064944));
#180875=CARTESIAN_POINT('Ctrl Pts',(20.8492492329854,-18.8068802901938,
20.3034769057816));
#180876=CARTESIAN_POINT('Ctrl Pts',(20.8380201086876,-18.690402658304,20.2969546328247));
#180877=CARTESIAN_POINT('Ctrl Pts',(20.8147015410847,-18.5613924012989,
20.2892743167573));
#180878=CARTESIAN_POINT('Ctrl Pts',(20.8120175788886,-18.547356791536,20.2884328134288));
#180879=CARTESIAN_POINT('Ctrl Pts',(20.8075198216203,-18.5250620303588,
20.2870862436861));
#180880=CARTESIAN_POINT('Ctrl Pts',(20.8057982531811,-18.5167845642371,
20.2865841185034));
#180881=CARTESIAN_POINT('Ctrl Pts',(20.8026745699976,-18.5022042542989,
20.2856957174239));
#180882=CARTESIAN_POINT('Ctrl Pts',(20.8012931087123,-18.4958970613438,
20.2853101075588));
#180883=CARTESIAN_POINT('Ctrl Pts',(20.7983761272525,-18.4828648506809,
20.2845106046769));
#180884=CARTESIAN_POINT('Ctrl Pts',(20.7968365495482,-18.4761408284032,
20.284096585308));
#180885=CARTESIAN_POINT('Ctrl Pts',(20.7928002841325,-18.4589003978175,
20.2830310946563));
#180886=CARTESIAN_POINT('Ctrl Pts',(20.790255891726,-18.4483954641057,20.2823780939087));
#180887=CARTESIAN_POINT('Ctrl Pts',(20.7793002217544,-18.4046308838208,
20.2796415419497));
#180888=CARTESIAN_POINT('Ctrl Pts',(20.7701619251216,-18.3715602143114,
20.2775346483525));
#180889=CARTESIAN_POINT('Ctrl Pts',(20.7442601975305,-18.2859820621578,
20.2719769907113));
#180890=CARTESIAN_POINT('Ctrl Pts',(20.7262435650024,-18.2338839147211,
20.2684877854883));
#180891=CARTESIAN_POINT('Ctrl Pts',(20.6664543640362,-18.0806349347482,
20.2579141905084));
#180892=CARTESIAN_POINT('Ctrl Pts',(20.6188548690702,-17.9819610303114,
20.2506814214578));
#180893=CARTESIAN_POINT('Ctrl Pts',(20.5395005856195,-17.8455638043169,
20.2402574808709));
#180894=CARTESIAN_POINT('Ctrl Pts',(20.5137225298926,-17.8045587714529,
20.2370653629312));
#180895=CARTESIAN_POINT('Ctrl Pts',(20.4766378279767,-17.7498289203209,
20.2327524276101));
#180896=CARTESIAN_POINT('Ctrl Pts',(20.4665318091789,-17.7353096289295,
20.2316030570057));
#180897=CARTESIAN_POINT('Ctrl Pts',(20.4252240664983,-17.6775213820953,
20.227012174627));
#180898=CARTESIAN_POINT('Ctrl Pts',(20.3925711674896,-17.6353081949318,
20.223621104637));
#180899=CARTESIAN_POINT('Ctrl Pts',(20.3527634222104,-17.5876796496449,
20.21979193505));
#180900=CARTESIAN_POINT('Ctrl Pts',(20.3471300078977,-17.5810234797385,
20.2192567388969));
#180901=CARTESIAN_POINT('Ctrl Pts',(20.3385382349731,-17.5709981352117,
20.2184507974542));
#180902=CARTESIAN_POINT('Ctrl Pts',(20.3356101161446,-17.5676033318597,
20.2181779153833));
#180903=CARTESIAN_POINT('Ctrl Pts',(20.3303349298428,-17.5615265219983,
20.2176895381327));
#180904=CARTESIAN_POINT('Ctrl Pts',(20.3279918646178,-17.5588411298857,
20.2174737548424));
#180905=CARTESIAN_POINT('Ctrl Pts',(20.3228860372971,-17.5530190740532,
20.2170060061097));
#180906=CARTESIAN_POINT('Ctrl Pts',(20.3201207727011,-17.5498846817113,
20.2167542316922));
#180907=CARTESIAN_POINT('Ctrl Pts',(20.312327717259,-17.5411039101721,20.2160489631704));
#180908=CARTESIAN_POINT('Ctrl Pts',(20.30727887805,-17.5354761791097,20.2155970148345));
#180909=CARTESIAN_POINT('Ctrl Pts',(20.2769252619159,-17.5020047503762,
20.2129085675889));
#180910=CARTESIAN_POINT('Ctrl Pts',(20.2509103215909,-17.4748107576996,
20.2107224536262));
#180911=CARTESIAN_POINT('Ctrl Pts',(20.1629358979216,-17.3876258498124,
20.2036494572595));
#180912=CARTESIAN_POINT('Ctrl Pts',(20.0980329414591,-17.3307224890346,
20.1989257950945));
#180913=CARTESIAN_POINT('Ctrl Pts',(19.8901911631465,-17.1698395991743,
20.1846222364707));
#180914=CARTESIAN_POINT('Ctrl Pts',(19.7375891400057,-17.0796549754226,
20.1751337271928));
#180915=CARTESIAN_POINT('Ctrl Pts',(19.5545458331111,-17.0003549538476,
20.1635411326293));
#180916=CARTESIAN_POINT('Ctrl Pts',(19.533378390977,-16.9915898444035,20.1621988867852));
#180917=CARTESIAN_POINT('Ctrl Pts',(19.5032078544977,-16.9796665720263,
20.1602816776846));
#180918=CARTESIAN_POINT('Ctrl Pts',(19.4943187978461,-16.976222888166,20.1597163252292));
#180919=CARTESIAN_POINT('Ctrl Pts',(19.4798307673967,-16.9707223714449,
20.1587939585398));
#180920=CARTESIAN_POINT('Ctrl Pts',(19.4742457626429,-16.9686289341688,
20.1584381751179));
#180921=CARTESIAN_POINT('Ctrl Pts',(19.4625307855116,-16.9642941630305,
20.1576913997106));
#180922=CARTESIAN_POINT('Ctrl Pts',(19.4563991538341,-16.9620575232385,
20.1573002555702));
#180923=CARTESIAN_POINT('Ctrl Pts',(19.4417768995244,-16.9568002418517,
20.1563667710111));
#180924=CARTESIAN_POINT('Ctrl Pts',(19.4332771908663,-16.95380540967,20.155823579052));
#180925=CARTESIAN_POINT('Ctrl Pts',(19.4045264538029,-16.9438811306457,
20.1539841327016));
#180926=CARTESIAN_POINT('Ctrl Pts',(19.3841900478059,-16.9372047330692,
20.1526795603885));
#180927=CARTESIAN_POINT('Ctrl Pts',(19.2725816986725,-16.9024296476072,
20.145498802058));
#180928=CARTESIAN_POINT('Ctrl Pts',(19.1796014448044,-16.8802268548258,
20.1394325029876));
#180929=CARTESIAN_POINT('Ctrl Pts',(18.9174370425839,-16.8360915784474,
20.1221548578037));
#180930=CARTESIAN_POINT('Ctrl Pts',(18.7466341502385,-16.8281932984175,
20.1106595013735));
#180931=CARTESIAN_POINT('Ctrl Pts',(18.540141983836,-16.8435753205552,20.0974447705595));
#180932=CARTESIAN_POINT('Ctrl Pts',(18.5036223171641,-16.8472524956502,
20.0951366546194));
#180933=CARTESIAN_POINT('Ctrl Pts',(18.4601350065862,-16.8527768363765,
20.092437206709));
#180934=CARTESIAN_POINT('Ctrl Pts',(18.4530601786526,-16.8537119488968,
20.0919996008124));
#180935=CARTESIAN_POINT('Ctrl Pts',(18.4415214171114,-16.855296486326,20.0912885799688));
#180936=CARTESIAN_POINT('Ctrl Pts',(18.4370546583934,-16.8559244262979,
20.0910139979897));
#180937=CARTESIAN_POINT('Ctrl Pts',(18.4290603574544,-16.857074337887,20.0905237950216));
#180938=CARTESIAN_POINT('Ctrl Pts',(18.4255321088041,-16.8575909482428,
20.0903078764517));
#180939=CARTESIAN_POINT('Ctrl Pts',(18.4178913415178,-16.8587294453988,
20.0898412216783));
#180940=CARTESIAN_POINT('Ctrl Pts',(18.4137793581951,-16.8593545355285,
20.0895906690237));
#180941=CARTESIAN_POINT('Ctrl Pts',(18.4022916800185,-16.8611355073814,
20.0888922643463));
#180942=CARTESIAN_POINT('Ctrl Pts',(18.394920134009,-16.8623183055104,20.0884459100984));
#180943=CARTESIAN_POINT('Ctrl Pts',(18.352020930785,-16.8694346594201,20.0858580448895));
#180944=CARTESIAN_POINT('Ctrl Pts',(18.3166407948072,-16.8762355506018,
20.0837626319533));
#180945=CARTESIAN_POINT('Ctrl Pts',(18.2031928520395,-16.9010611719684,
20.0771197047338));
#180946=CARTESIAN_POINT('Ctrl Pts',(18.125965213378,-16.922615362146,20.0727135403215));
#180947=CARTESIAN_POINT('Ctrl Pts',(17.8744490857913,-17.0084658944423,
20.0582255013741));
#180948=CARTESIAN_POINT('Ctrl Pts',(17.7074292920161,-17.0912745602107,
20.0482965085914));
#180949=CARTESIAN_POINT('Ctrl Pts',(17.5350077516949,-17.2071232330054,
20.0362150186401));
#180950=CARTESIAN_POINT('Ctrl Pts',(17.516859682758,-17.2197336413192,20.034919587627));
#180951=CARTESIAN_POINT('Ctrl Pts',(17.4920437698835,-17.2375597841495,
20.0331134233622));
#180952=CARTESIAN_POINT('Ctrl Pts',(17.4852044146602,-17.242535138082,20.0326119152336));
#180953=CARTESIAN_POINT('Ctrl Pts',(17.473501847422,-17.2511559902638,20.0317472901836));
#180954=CARTESIAN_POINT('Ctrl Pts',(17.4686241491818,-17.25478171908,20.0313849438357));
#180955=CARTESIAN_POINT('Ctrl Pts',(17.4587685996162,-17.2621737252347,
20.0306487794923));
#180956=CARTESIAN_POINT('Ctrl Pts',(17.4537916604268,-17.2659411133045,
20.0302749201504));
#180957=CARTESIAN_POINT('Ctrl Pts',(17.4422641877347,-17.2747475169028,
20.029404048733));
#180958=CARTESIAN_POINT('Ctrl Pts',(17.4357263880047,-17.2798029643262,
20.0289063901853));
#180959=CARTESIAN_POINT('Ctrl Pts',(17.422045515538,-17.2905104880988,20.0278570206401));
#180960=CARTESIAN_POINT('Ctrl Pts',(17.4149089987358,-17.2961706326518,
20.0273049933974));
#180961=CARTESIAN_POINT('Ctrl Pts',(17.3960082076488,-17.3113610437656,
20.0258304731548));
#180962=CARTESIAN_POINT('Ctrl Pts',(17.3843094296213,-17.3209716229731,
20.0249047679479));
#180963=CARTESIAN_POINT('Ctrl Pts',(17.3489493617208,-17.3506609641303,
20.0220662692862));
#180964=CARTESIAN_POINT('Ctrl Pts',(17.3256264036911,-17.3711345299148,
20.0201376565915));
#180965=CARTESIAN_POINT('Ctrl Pts',(17.1786303110739,-17.5060072572271,
20.0076107591758));
#180966=CARTESIAN_POINT('Ctrl Pts',(17.0685518872788,-17.6342991144025,
19.9964225465834));
#180967=CARTESIAN_POINT('Ctrl Pts',(16.9197631082974,-17.8565364236068,
19.9788044483057));
#180968=CARTESIAN_POINT('Ctrl Pts',(16.8705046912916,-17.942601249661,19.9723517461347));
#180969=CARTESIAN_POINT('Ctrl Pts',(16.8232353258586,-18.0405388944351,
19.9656327814036));
#180970=CARTESIAN_POINT('Ctrl Pts',(16.8190812886968,-18.0492988732645,
19.9650371083211));
#180971=CARTESIAN_POINT('Ctrl Pts',(16.8130369085061,-18.0622746826635,
19.96416290171));
#180972=CARTESIAN_POINT('Ctrl Pts',(16.8111000205147,-18.0664685160761,
19.9638816023127));
#180973=CARTESIAN_POINT('Ctrl Pts',(16.8076882729552,-18.0739197556727,
19.9633840685189));
#180974=CARTESIAN_POINT('Ctrl Pts',(16.8062079245954,-18.0771745888948,
19.9631674992382));
#180975=CARTESIAN_POINT('Ctrl Pts',(16.8030539889756,-18.0841560105213,
19.962704612285));
#180976=CARTESIAN_POINT('Ctrl Pts',(16.8013829440263,-18.087883686548,19.962458450798));
#180977=CARTESIAN_POINT('Ctrl Pts',(16.7968258157529,-18.0981288236308,
19.9617845621694));
#180978=CARTESIAN_POINT('Ctrl Pts',(16.7939618112104,-18.104656129263,19.9613581669635));
#180979=CARTESIAN_POINT('Ctrl Pts',(16.7788510580554,-18.1395730454917,
19.959092281467));
#180980=CARTESIAN_POINT('Ctrl Pts',(16.7671936907237,-18.1682155204825,
19.9572865138634));
#180981=CARTESIAN_POINT('Ctrl Pts',(16.7525148760944,-18.206674153451,19.9549187101212));
#180982=CARTESIAN_POINT('Ctrl Pts',(16.7489321427425,-18.216269415617,19.9543325979226));
#180983=CARTESIAN_POINT('Ctrl Pts',(16.7454193686617,-18.225889765486,19.9537492327042));
#180984=CARTESIAN_POINT('',(16.6170003908425,-18.9532864008441,20.489056279057));
#180985=CARTESIAN_POINT('Ctrl Pts',(16.7454194015149,-18.2258896755116,
19.7345260518445));
#180986=CARTESIAN_POINT('Ctrl Pts',(16.7805470671853,-18.1296863961113,
19.7401268841278));
#180987=CARTESIAN_POINT('Ctrl Pts',(16.8226235259406,-18.0361205379653,
19.7456314811537));
#180988=CARTESIAN_POINT('Ctrl Pts',(16.920754698698,-17.854436923613,19.7569906966531));
#180989=CARTESIAN_POINT('Ctrl Pts',(16.9768430308415,-17.7667158280565,
19.7628328170713));
#180990=CARTESIAN_POINT('Ctrl Pts',(17.0475681359745,-17.672221026253,19.7697495704607));
#180991=CARTESIAN_POINT('Ctrl Pts',(17.0561041186407,-17.6610499425794,
19.7705776622703));
#180992=CARTESIAN_POINT('Ctrl Pts',(17.0699092552613,-17.6433513288339,
19.7719067746021));
#180993=CARTESIAN_POINT('Ctrl Pts',(17.0751071271484,-17.6367685433421,
19.7724049734974));
#180994=CARTESIAN_POINT('Ctrl Pts',(17.0843685900936,-17.6251817146288,
19.7732888173723));
#180995=CARTESIAN_POINT('Ctrl Pts',(17.0884161969959,-17.6201649888904,
19.7736738183237));
#180996=CARTESIAN_POINT('Ctrl Pts',(17.0968603404038,-17.6097963242568,
19.7744744269932));
#180997=CARTESIAN_POINT('Ctrl Pts',(17.1012603511473,-17.6044473258933,
19.7748901727685));
#180998=CARTESIAN_POINT('Ctrl Pts',(17.1126754381001,-17.590708235081,19.7759651477101));
#180999=CARTESIAN_POINT('Ctrl Pts',(17.1197293573079,-17.5823508152199,
19.7766259591332));
#181000=CARTESIAN_POINT('Ctrl Pts',(17.1499117127893,-17.5471480912477,
19.7794391942736));
#181001=CARTESIAN_POINT('Ctrl Pts',(17.1736463807451,-17.5208323187453,
19.781616626741));
#181002=CARTESIAN_POINT('Ctrl Pts',(17.2376864166998,-17.4533154235877,
19.78740633834));
#181003=CARTESIAN_POINT('Ctrl Pts',(17.2790311894566,-17.4131450266149,
19.7910611796364));
#181004=CARTESIAN_POINT('Ctrl Pts',(17.4217679760684,-17.2853622516311,
19.8033999111042));
#181005=CARTESIAN_POINT('Ctrl Pts',(17.5298269232643,-17.2056906492849,
19.8123263219024));
#181006=CARTESIAN_POINT('Ctrl Pts',(17.7216270372015,-17.0905908270338,
19.8270271227065));
#181007=CARTESIAN_POINT('Ctrl Pts',(17.8014472459869,-17.0493459978098,
19.8328476519824));
#181008=CARTESIAN_POINT('Ctrl Pts',(17.8924920046086,-17.0094124344906,
19.8389896548687));
#181009=CARTESIAN_POINT('Ctrl Pts',(17.9013574933049,-17.0055959771613,
19.8395826563883));
#181010=CARTESIAN_POINT('Ctrl Pts',(17.9144966605783,-17.0000459690647,
19.8404537047473));
#181011=CARTESIAN_POINT('Ctrl Pts',(17.9187502547813,-16.9982655973604,
19.8407344892869));
#181012=CARTESIAN_POINT('Ctrl Pts',(17.92631175527,-16.995129672559,19.8412314547815));
#181013=CARTESIAN_POINT('Ctrl Pts',(17.9296173078232,-16.9937685876548,
19.8414479677669));
#181014=CARTESIAN_POINT('Ctrl Pts',(17.9367125496775,-16.9908680685971,
19.8419111136574));
#181015=CARTESIAN_POINT('Ctrl Pts',(17.9405032468212,-16.989331246961,19.8421575883929));
#181016=CARTESIAN_POINT('Ctrl Pts',(17.9509339837396,-16.985137584304,19.8428332177713));
#181017=CARTESIAN_POINT('Ctrl Pts',(17.9575831404241,-16.9825033608588,
19.8432610289936));
#181018=CARTESIAN_POINT('Ctrl Pts',(17.9933579520465,-16.9685396382364,
19.8455480551594));
#181019=CARTESIAN_POINT('Ctrl Pts',(18.0227200873404,-16.9578217808749,
19.8473727975963));
#181020=CARTESIAN_POINT('Ctrl Pts',(18.2073708560607,-16.8950177611634,
19.8585872796774));
#181021=CARTESIAN_POINT('Ctrl Pts',(18.3680441283967,-16.8604448809359,
19.867242164921));
#181022=CARTESIAN_POINT('Ctrl Pts',(18.6477495083044,-16.8335146082774,
19.8826236740673));
#181023=CARTESIAN_POINT('Ctrl Pts',(18.7651027488652,-16.8319889558617,
19.8891640363662));
#181024=CARTESIAN_POINT('Ctrl Pts',(18.8962303217916,-16.8411767829979,
19.8968647178187));
#181025=CARTESIAN_POINT('Ctrl Pts',(18.9104790372967,-16.8423202932162,
19.8977064888719));
#181026=CARTESIAN_POINT('Ctrl Pts',(18.933136461051,-16.84436977291,19.8990534110273));
#181027=CARTESIAN_POINT('Ctrl Pts',(18.9415533623288,-16.8451819957849,
19.8995556185606));
#181028=CARTESIAN_POINT('Ctrl Pts',(18.9563884359381,-16.8467033280388,
19.9004441205013));
#181029=CARTESIAN_POINT('Ctrl Pts',(18.9628086892343,-16.8473914198324,
19.9008297484497));
#181030=CARTESIAN_POINT('Ctrl Pts',(18.9760805738049,-16.8488752834648,
19.9016292448346));
#181031=CARTESIAN_POINT('Ctrl Pts',(18.9829316571276,-16.8496751902137,
19.9020432394084));
#181032=CARTESIAN_POINT('Ctrl Pts',(19.0005059946725,-16.8518142140413,
19.9031085736971));
#181033=CARTESIAN_POINT('Ctrl Pts',(19.01122302866,-16.8532019710466,19.9037614419402));
#181034=CARTESIAN_POINT('Ctrl Pts',(19.0558970768893,-16.859334985966,19.9064966534943));
#181035=CARTESIAN_POINT('Ctrl Pts',(19.0897453569516,-16.8648225724381,
19.9086023100447));
#181036=CARTESIAN_POINT('Ctrl Pts',(19.1775688356774,-16.8812591182249,
19.9141559119266));
#181037=CARTESIAN_POINT('Ctrl Pts',(19.2312738298428,-16.8934959241307,
19.9176422276242));
#181038=CARTESIAN_POINT('Ctrl Pts',(19.3900378905899,-16.9362462203215,
19.9282102855123));
#181039=CARTESIAN_POINT('Ctrl Pts',(19.4932690692309,-16.9728193543973,
19.9354404234675));
#181040=CARTESIAN_POINT('Ctrl Pts',(19.6343907574575,-17.035488498096,19.945640463466));
#181041=CARTESIAN_POINT('Ctrl Pts',(19.6749836787234,-17.0550894193858,
19.9486119323262));
#181042=CARTESIAN_POINT('Ctrl Pts',(19.736474907382,-17.0872413962037,19.953145621297));
#181043=CARTESIAN_POINT('Ctrl Pts',(19.757833739142,-17.0988823220274,19.9547265584958));
#181044=CARTESIAN_POINT('Ctrl Pts',(19.7915882865671,-17.1180409113933,
19.9572300303378));
#181045=CARTESIAN_POINT('Ctrl Pts',(19.8041153284032,-17.1253221071828,
19.9581602467062));
#181046=CARTESIAN_POINT('Ctrl Pts',(19.8484743481873,-17.1517182139479,
19.9614557631727));
#181047=CARTESIAN_POINT('Ctrl Pts',(19.8798790953437,-17.1715424555092,
19.9637918498234));
#181048=CARTESIAN_POINT('Ctrl Pts',(19.9167024942233,-17.1961654074032,
19.9665198187964));
#181049=CARTESIAN_POINT('Ctrl Pts',(19.9226366668805,-17.2001771825051,
19.9669590791207));
#181050=CARTESIAN_POINT('Ctrl Pts',(19.9322810788318,-17.2067688190714,
19.9676722425014));
#181051=CARTESIAN_POINT('Ctrl Pts',(19.9360035651826,-17.209330539392,19.9679473241312));
#181052=CARTESIAN_POINT('Ctrl Pts',(19.9426493510208,-17.2139354252945,
19.9684380640906));
#181053=CARTESIAN_POINT('Ctrl Pts',(19.9455757058702,-17.2159740701458,
19.968654022789));
#181054=CARTESIAN_POINT('Ctrl Pts',(19.9518987425389,-17.2204027887527,
19.9691203616557));
#181055=CARTESIAN_POINT('Ctrl Pts',(19.9552935364261,-17.2227954581248,
19.9693705604363));
#181056=CARTESIAN_POINT('Ctrl Pts',(19.9647485856289,-17.2295011619625,
19.9700669807399));
#181057=CARTESIAN_POINT('Ctrl Pts',(19.9707932521212,-17.233836217556,19.970511718235));
#181058=CARTESIAN_POINT('Ctrl Pts',(20.005611422008,-17.2590857356219,19.9730714313171));
#181059=CARTESIAN_POINT('Ctrl Pts',(20.0338788372301,-17.2806922305908,
19.9751414727124));
#181060=CARTESIAN_POINT('Ctrl Pts',(20.1227035916488,-17.3522040719066,
19.9816674583579));
#181061=CARTESIAN_POINT('Ctrl Pts',(20.1810396157034,-17.4047692662367,
19.9859877187922));
#181062=CARTESIAN_POINT('Ctrl Pts',(20.3688979775496,-17.5939856051794,
20.0005313012805));
#181063=CARTESIAN_POINT('Ctrl Pts',(20.4830620021931,-17.7445767773613,
20.0105821242138));
#181064=CARTESIAN_POINT('Ctrl Pts',(20.5865921456588,-17.9272715407187,
20.0227985062851));
#181065=CARTESIAN_POINT('Ctrl Pts',(20.5970657291424,-17.9464394051464,
20.0240791289184));
#181066=CARTESIAN_POINT('Ctrl Pts',(20.6111617514148,-17.9732131976032,
20.0258678733392));
#181067=CARTESIAN_POINT('Ctrl Pts',(20.6150384242497,-17.9806842486053,
20.0263670041261));
#181068=CARTESIAN_POINT('Ctrl Pts',(20.6216325552855,-17.993579870596,20.0272286183272));
#181069=CARTESIAN_POINT('Ctrl Pts',(20.6243714561481,-17.9989934077762,
20.0275903434822));
#181070=CARTESIAN_POINT('Ctrl Pts',(20.6299763470006,-18.0101909114067,
20.0283386268809));
#181071=CARTESIAN_POINT('Ctrl Pts',(20.632839225805,-18.0159763566793,20.0287252891717));
#181072=CARTESIAN_POINT('Ctrl Pts',(20.6394506640489,-18.0294922343711,
20.0296287515117));
#181073=CARTESIAN_POINT('Ctrl Pts',(20.6431786939973,-18.0372325313185,
20.0301462597869));
#181074=CARTESIAN_POINT('Ctrl Pts',(20.6550037767144,-18.0621714531796,
20.0318141325822));
#181075=CARTESIAN_POINT('Ctrl Pts',(20.6629161564608,-18.0794561459516,
20.0329708459852));
#181076=CARTESIAN_POINT('Ctrl Pts',(20.7015120020373,-18.1668607320337,
20.0388253434902));
#181077=CARTESIAN_POINT('Ctrl Pts',(20.728606331535,-18.2384942470877,20.043643404423));
#181078=CARTESIAN_POINT('Ctrl Pts',(20.7850259438845,-18.4162132051225,
20.0556347989979));
#181079=CARTESIAN_POINT('Ctrl Pts',(20.8100759289639,-18.5234207200323,
20.0629064440229));
#181080=CARTESIAN_POINT('Ctrl Pts',(20.8373686026678,-18.7019490180111,
20.0748350385553));
#181081=CARTESIAN_POINT('Ctrl Pts',(20.8445447065821,-18.7723141522826,
20.0794882829132));
#181082=CARTESIAN_POINT('Ctrl Pts',(20.8506425760097,-18.8904915403675,
20.0871064238349));
#181083=CARTESIAN_POINT('Ctrl Pts',(20.8514909562973,-18.9381471566793,
20.090124697644));
#181084=CARTESIAN_POINT('Ctrl Pts',(20.8506069586826,-18.9935165982999,
20.0935390885672));
#181085=CARTESIAN_POINT('Ctrl Pts',(20.8504414148626,-19.0012380655234,
20.094013142129));
#181086=CARTESIAN_POINT('Ctrl Pts',(20.8501088494901,-19.0135941658069,
20.0947681954648));
#181087=CARTESIAN_POINT('Ctrl Pts',(20.8499688502697,-19.0182293725133,
20.0950506449308));
#181088=CARTESIAN_POINT('Ctrl Pts',(20.8496935528338,-19.0264490182648,
20.0955500550927));
#181089=CARTESIAN_POINT('Ctrl Pts',(20.8495643741406,-19.0300336172403,
20.095767354518));
#181090=CARTESIAN_POINT('Ctrl Pts',(20.8492707881097,-19.0376429674077,
20.0962275733651));
#181091=CARTESIAN_POINT('Ctrl Pts',(20.8491040049387,-19.0416675739152,
20.0964703584332));
#181092=CARTESIAN_POINT('Ctrl Pts',(20.8486216767113,-19.0525552852036,
20.0971255264038));
#181093=CARTESIAN_POINT('Ctrl Pts',(20.8482842046051,-19.0594174385846,
20.0975366982362));
#181094=CARTESIAN_POINT('Ctrl Pts',(20.8464248682664,-19.0938114437129,
20.0995892687076));
#181095=CARTESIAN_POINT('Ctrl Pts',(20.8443985385574,-19.1213147432433,
20.1012040233315));
#181096=CARTESIAN_POINT('Ctrl Pts',(20.8369402554542,-19.2012083688462,
20.1058374163366));
#181097=CARTESIAN_POINT('Ctrl Pts',(20.8300898620696,-19.2534474654108,
20.1087953003085));
#181098=CARTESIAN_POINT('Ctrl Pts',(20.7978729314948,-19.4437421511963,
20.1194779234525));
#181099=CARTESIAN_POINT('Ctrl Pts',(20.7607489010224,-19.5794336791868,
20.1269381944543));
#181100=CARTESIAN_POINT('Ctrl Pts',(20.6771589183375,-19.7972615199283,
20.1398370889753));
#181101=CARTESIAN_POINT('Ctrl Pts',(20.6381698851839,-19.8817674888697,
20.1450882757069));
#181102=CARTESIAN_POINT('Ctrl Pts',(20.5871670337418,-19.9755483317184,
20.1513463222675));
#181103=CARTESIAN_POINT('Ctrl Pts',(20.5804591410119,-19.9876002459716,
20.1521589521558));
#181104=CARTESIAN_POINT('Ctrl Pts',(20.5695220576024,-20.006806535564,20.153467908742));
#181105=CARTESIAN_POINT('Ctrl Pts',(20.5653676055214,-20.0140031741268,
20.1539615487339));
#181106=CARTESIAN_POINT('Ctrl Pts',(20.557921528808,-20.0267281759423,20.154840124743));
#181107=CARTESIAN_POINT('Ctrl Pts',(20.5546468518162,-20.0322663722316,
20.1552244421332));
#181108=CARTESIAN_POINT('Ctrl Pts',(20.5477769766532,-20.0437648689254,
20.156026462982));
#181109=CARTESIAN_POINT('Ctrl Pts',(20.5441775314504,-20.0497225300086,
20.1564443185528));
#181110=CARTESIAN_POINT('Ctrl Pts',(20.5347659407548,-20.0651280560199,
20.1575308860973));
#181111=CARTESIAN_POINT('Ctrl Pts',(20.5289088590093,-20.0745480938452,
20.1582012458132));
#181112=CARTESIAN_POINT('Ctrl Pts',(20.5032689013427,-20.1150715061749,
20.1611112162393));
#181113=CARTESIAN_POINT('Ctrl Pts',(20.4827505349386,-20.1456997412839,
20.1633780270702));
#181114=CARTESIAN_POINT('Ctrl Pts',(20.4262468486197,-20.2254586287154,
20.1694666057189));
#181115=CARTESIAN_POINT('Ctrl Pts',(20.388925480486,-20.2735963247478,20.1733366023569));
#181116=CARTESIAN_POINT('Ctrl Pts',(20.2457494232857,-20.4426778973935,
20.1876414227859));
#181117=CARTESIAN_POINT('Ctrl Pts',(20.1283032675158,-20.5530680687911,
20.1984390453116));
#181118=CARTESIAN_POINT('Ctrl Pts',(19.9521815025712,-20.6843995608512,
20.2126879119689));
#181119=CARTESIAN_POINT('Ctrl Pts',(19.9033933730999,-20.7176995507841,
20.2164535629882));
#181120=CARTESIAN_POINT('Ctrl Pts',(19.8456903419437,-20.7536418558616,
20.2206488561441));
#181121=CARTESIAN_POINT('Ctrl Pts',(19.838078254587,-20.7583166963077,20.2211972789703));
#181122=CARTESIAN_POINT('Ctrl Pts',(19.8265626690247,-20.7652888141176,
20.2220191380875));
#181123=CARTESIAN_POINT('Ctrl Pts',(19.8226811269092,-20.7676219083122,
20.2222948364231));
#181124=CARTESIAN_POINT('Ctrl Pts',(19.8157287864319,-20.7717704684062,
20.2227862419451));
#181125=CARTESIAN_POINT('Ctrl Pts',(19.8126608682162,-20.7735906392703,
20.2230022529377));
#181126=CARTESIAN_POINT('Ctrl Pts',(19.8060173208294,-20.7775095323721,
20.2234682121569));
#181127=CARTESIAN_POINT('Ctrl Pts',(19.8024401340686,-20.7796055016136,
20.2237179816327));
#181128=CARTESIAN_POINT('Ctrl Pts',(19.7924566053026,-20.7854157878599,
20.2244119999043));
#181129=CARTESIAN_POINT('Ctrl Pts',(19.7860368255959,-20.7891070621364,
20.2248547812215));
#181130=CARTESIAN_POINT('Ctrl Pts',(19.7491314869355,-20.8100701643897,
20.2273809787281));
#181131=CARTESIAN_POINT('Ctrl Pts',(19.7182383083398,-20.8266178134458,
20.2294208254995));
#181132=CARTESIAN_POINT('Ctrl Pts',(19.6186103344541,-20.8768402762856,
20.2358094510425));
#181133=CARTESIAN_POINT('Ctrl Pts',(19.5484508390511,-20.9075605787205,
20.2400290466047));
#181134=CARTESIAN_POINT('Ctrl Pts',(19.2977415968042,-21.00149700293,20.2546427344995));
#181135=CARTESIAN_POINT('Ctrl Pts',(19.1104657182348,-21.0440111564456,
20.2648395706612));
#181136=CARTESIAN_POINT('Ctrl Pts',(18.8986139739447,-21.0626997512307,
20.2772165061168));
#181137=CARTESIAN_POINT('Ctrl Pts',(18.8771713707648,-21.0642625567977,
20.2784773115034));
#181138=CARTESIAN_POINT('Ctrl Pts',(18.8473618295938,-21.0659791877052,
20.2802426699385));
#181139=CARTESIAN_POINT('Ctrl Pts',(18.8390117297827,-21.0664104246855,
20.2807385402028));
#181140=CARTESIAN_POINT('Ctrl Pts',(18.8246133213678,-21.0670685230588,
20.2815960291988));
#181141=CARTESIAN_POINT('Ctrl Pts',(18.8185661500767,-21.0673189348971,
20.2819569064628));
#181142=CARTESIAN_POINT('Ctrl Pts',(18.8060591709852,-21.0677831293116,
20.2827048536851));
#181143=CARTESIAN_POINT('Ctrl Pts',(18.7995992984212,-21.0679932667691,
20.2830920339934));
#181144=CARTESIAN_POINT('Ctrl Pts',(18.7844986935655,-21.0684152684608,
20.28399917092));
#181145=CARTESIAN_POINT('Ctrl Pts',(18.7758574716495,-21.0686038021395,
20.2845198532456));
#181146=CARTESIAN_POINT('Ctrl Pts',(18.7479225577069,-21.069042151022,20.2862083194631));
#181147=CARTESIAN_POINT('Ctrl Pts',(18.7286269651951,-21.0690811034595,
20.2873826739654));
#181148=CARTESIAN_POINT('Ctrl Pts',(18.6306517019469,-21.06793947872,20.2933882035967));
#181149=CARTESIAN_POINT('Ctrl Pts',(18.5520906242898,-21.0626366974371,
20.2983467403219));
#181150=CARTESIAN_POINT('Ctrl Pts',(18.3720042015798,-21.040351840264,20.3100318878856));
#181151=CARTESIAN_POINT('Ctrl Pts',(18.271055601448,-21.0203167156928,20.3168231199227));
#181152=CARTESIAN_POINT('Ctrl Pts',(18.0548301710431,-20.9607755953748,
20.3316409160328));
#181153=CARTESIAN_POINT('Ctrl Pts',(17.9406711823433,-20.9184910992178,
20.3396418470578));
#181154=CARTESIAN_POINT('Ctrl Pts',(17.8221907809327,-20.8625974806489,
20.3477326435652));
#181155=CARTESIAN_POINT('Ctrl Pts',(17.8136480826569,-20.8584970865319,
20.3483146849025));
#181156=CARTESIAN_POINT('Ctrl Pts',(17.801020453579,-20.8523313162533,20.3491727597964));
#181157=CARTESIAN_POINT('Ctrl Pts',(17.7969143617505,-20.8503098938446,
20.349451416912));
#181158=CARTESIAN_POINT('Ctrl Pts',(17.789615757918,-20.8466873510864,20.3499460449661));
#181159=CARTESIAN_POINT('Ctrl Pts',(17.7864207174449,-20.8450914555257,
20.3501623361305));
#181160=CARTESIAN_POINT('Ctrl Pts',(17.7796287575105,-20.841677425954,20.350621609908));
#181161=CARTESIAN_POINT('Ctrl Pts',(17.7760329990429,-20.8398571101519,
20.3508644529268));
#181162=CARTESIAN_POINT('Ctrl Pts',(17.7662297297349,-20.8348590850703,
20.3515257573096));
#181163=CARTESIAN_POINT('Ctrl Pts',(17.7600326231549,-20.8316609221254,
20.3519429545262));
#181164=CARTESIAN_POINT('Ctrl Pts',(17.7462223590738,-20.8244471723838,
20.3528710401299));
#181165=CARTESIAN_POINT('Ctrl Pts',(17.7386176166978,-20.8204156383723,
20.3533809781286));
#181166=CARTESIAN_POINT('Ctrl Pts',(17.7152720038246,-20.8078563404309,
20.3549436150115));
#181167=CARTESIAN_POINT('Ctrl Pts',(17.6996141548693,-20.799174992557,20.3559877143731));
#181168=CARTESIAN_POINT('Ctrl Pts',(17.6398791393012,-20.7650576773131,
20.3599629557947));
#181169=CARTESIAN_POINT('Ctrl Pts',(17.5966117920201,-20.738232727672,20.3628255060107));
#181170=CARTESIAN_POINT('Ctrl Pts',(17.4424243266523,-20.6347626986873,
20.3731182866498));
#181171=CARTESIAN_POINT('Ctrl Pts',(17.3379252307763,-20.5491335902069,
20.3802936736151));
#181172=CARTESIAN_POINT('Ctrl Pts',(17.1708493965805,-20.3832169122454,
20.3932651296098));
#181173=CARTESIAN_POINT('Ctrl Pts',(17.1045822428723,-20.3072917346343,
20.3989293074954));
#181174=CARTESIAN_POINT('Ctrl Pts',(17.035548290577,-20.215782571959,20.4056473067735));
#181175=CARTESIAN_POINT('Ctrl Pts',(17.0272365379278,-20.2045346577935,
20.406471141151));
#181176=CARTESIAN_POINT('Ctrl Pts',(17.014131840751,-20.1864280086187,20.4077947087111));
#181177=CARTESIAN_POINT('Ctrl Pts',(17.0092669658064,-20.1796216645841,
20.4082916577737));
#181178=CARTESIAN_POINT('Ctrl Pts',(17.0007273822617,-20.167523155208,20.4091740573063));
#181179=CARTESIAN_POINT('Ctrl Pts',(16.9970362280716,-20.1622426871665,
20.4095588707449));
#181180=CARTESIAN_POINT('Ctrl Pts',(16.9894217324656,-20.1512429987109,
20.4103598600947));
#181181=CARTESIAN_POINT('Ctrl Pts',(16.9855022822326,-20.1455211898797,
20.4107761778783));
#181182=CARTESIAN_POINT('Ctrl Pts',(16.975451360508,-20.1306925852483,20.4118542857492));
#181183=CARTESIAN_POINT('Ctrl Pts',(16.9693625437384,-20.1215572533339,
20.4125176756502));
#181184=CARTESIAN_POINT('Ctrl Pts',(16.9437147949679,-20.0824205030374,
20.4153566730717));
#181185=CARTESIAN_POINT('Ctrl Pts',(16.9248487405476,-20.0519741376835,
20.4175578628909));
#181186=CARTESIAN_POINT('Ctrl Pts',(16.8772303561213,-19.9705852968379,
20.4234264701927));
#181187=CARTESIAN_POINT('Ctrl Pts',(16.8498027401428,-19.9189070450648,
20.4271379056861));
#181188=CARTESIAN_POINT('Ctrl Pts',(16.7582330083887,-19.7276417390236,
20.4408045120723));
#181189=CARTESIAN_POINT('Ctrl Pts',(16.7071876152669,-19.5823176408604,
20.4510983065187));
#181190=CARTESIAN_POINT('Ctrl Pts',(16.6660226855411,-19.4057911702342,
20.4629186754329));
#181191=CARTESIAN_POINT('Ctrl Pts',(16.6602607812044,-19.3786876543303,
20.4647138057823));
#181192=CARTESIAN_POINT('Ctrl Pts',(16.6468711367126,-19.3090051237982,
20.4692668120853));
#181193=CARTESIAN_POINT('Ctrl Pts',(16.6400127084185,-19.2662886606018,
20.4719989723584));
#181194=CARTESIAN_POINT('Ctrl Pts',(16.6335056830334,-19.215948681038,20.4751271739653));
#181195=CARTESIAN_POINT('Ctrl Pts',(16.6325834880109,-19.208503272498,20.4755875014242));
#181196=CARTESIAN_POINT('Ctrl Pts',(16.6311572014448,-19.1964637424467,
20.4763279164765));
#181197=CARTESIAN_POINT('Ctrl Pts',(16.6306285495896,-19.1918726731822,
20.4766093334647));
#181198=CARTESIAN_POINT('Ctrl Pts',(16.6297175168666,-19.1837261699198,
20.4771069971511));
#181199=CARTESIAN_POINT('Ctrl Pts',(16.6293291064758,-19.180171464651,20.4773235793922));
#181200=CARTESIAN_POINT('Ctrl Pts',(16.6285936556603,-19.1732789772606,
20.4777424096378));
#181201=CARTESIAN_POINT('Ctrl Pts',(16.6282455464994,-19.1699413739676,
20.4779447190852));
#181202=CARTESIAN_POINT('Ctrl Pts',(16.627496289301,-19.162588228519,20.4783893491729));
#181203=CARTESIAN_POINT('Ctrl Pts',(16.6270986830808,-19.1585723276542,
20.4786314723414));
#181204=CARTESIAN_POINT('Ctrl Pts',(16.6261439843523,-19.1486401023826,
20.4792285954265));
#181205=CARTESIAN_POINT('Ctrl Pts',(16.625600310828,-19.142722481973,20.4795828693057));
#181206=CARTESIAN_POINT('Ctrl Pts',(16.6234160992151,-19.1177968324816,
20.481069122359));
#181207=CARTESIAN_POINT('Ctrl Pts',(16.6220075783014,-19.0987687221853,
20.4821890723319));
#181208=CARTESIAN_POINT('Ctrl Pts',(16.6183136910291,-19.0376545455932,
20.4857465427669));
#181209=CARTESIAN_POINT('Ctrl Pts',(16.6170276587043,-18.9955169040541,
20.4881393462053));
#181210=CARTESIAN_POINT('Ctrl Pts',(16.6170004413562,-18.953367004782,20.4904971916622));
#181211=CARTESIAN_POINT('Ctrl Pts',(16.7454193692319,-18.2258897639242,
20.5336910470276));
#181212=CARTESIAN_POINT('Ctrl Pts',(16.7207024917391,-18.2935812815386,
20.529371954925));
#181213=CARTESIAN_POINT('Ctrl Pts',(16.6994546610031,-18.3625126961517,
20.5250528628225));
#181214=CARTESIAN_POINT('Ctrl Pts',(16.6817841805163,-18.4322892821379,
20.5207337707199));
#181215=CARTESIAN_POINT('Ctrl Pts',(16.6641059734603,-18.5020963785351,
20.5164127900573));
#181216=CARTESIAN_POINT('Ctrl Pts',(16.6500083270565,-18.572748895104,20.5120918093947));
#181217=CARTESIAN_POINT('Ctrl Pts',(16.6395483122343,-18.643842365638,20.5077708287321));
#181218=CARTESIAN_POINT('Ctrl Pts',(16.629072807401,-18.7150411169649,20.503443449222));
#181219=CARTESIAN_POINT('Ctrl Pts',(16.6222457295304,-18.7866816316723,
20.499116069712));
#181220=CARTESIAN_POINT('Ctrl Pts',(16.6190721599129,-18.8583558265323,
20.4947886902019));
#181221=CARTESIAN_POINT('Ctrl Pts',(16.6176708340988,-18.8900043836992,
20.492877886487));
#181222=CARTESIAN_POINT('Ctrl Pts',(16.6169811726838,-18.9216595290166,
20.490967082772));
#181223=CARTESIAN_POINT('Ctrl Pts',(16.6170003908425,-18.9532864008441,
20.489056279057));
#181224=CARTESIAN_POINT('Origin',(18.734,-18.952,0.));
#181225=CARTESIAN_POINT('',(16.7454193692319,-18.2258897639242,21.5555703664997));
#181226=CARTESIAN_POINT('',(16.7454193692319,-18.2258897639242,21.3335535355786));
#181227=CARTESIAN_POINT('',(16.7454193692319,-18.2258897639242,0.));
#181228=CARTESIAN_POINT('',(16.6170006158577,-18.953614788214,21.5109437210328));
#181229=CARTESIAN_POINT('Ctrl Pts',(16.6170006158577,-18.953614788214,21.5109437210328));
#181230=CARTESIAN_POINT('Ctrl Pts',(16.6169459675925,-18.8819705053332,
21.515267181378));
#181231=CARTESIAN_POINT('Ctrl Pts',(16.6205324541972,-18.8101917050093,
21.5195906417233));
#181232=CARTESIAN_POINT('Ctrl Pts',(16.6277745368492,-18.7386849785526,
21.5239141020685));
#181233=CARTESIAN_POINT('Ctrl Pts',(16.6350090210574,-18.6672532774524,
21.5282330262089));
#181234=CARTESIAN_POINT('Ctrl Pts',(16.6458914496557,-18.5960935752594,
21.5325519503494));
#181235=CARTESIAN_POINT('Ctrl Pts',(16.6603842616694,-18.5256119493375,
21.5368708744898));
#181236=CARTESIAN_POINT('Ctrl Pts',(16.6748666465897,-18.4551810325882,
21.5411866913088));
#181237=CARTESIAN_POINT('Ctrl Pts',(16.6929541629953,-18.3854277094975,
21.5455025081278));
#181238=CARTESIAN_POINT('Ctrl Pts',(16.7145577235254,-18.3167505277555,
21.5498183249468));
#181239=CARTESIAN_POINT('Ctrl Pts',(16.7241553333615,-18.2862399647356,
21.5517356721311));
#181240=CARTESIAN_POINT('Ctrl Pts',(16.7344462197403,-18.2559416643843,
21.5536530193154));
#181241=CARTESIAN_POINT('Ctrl Pts',(16.7454193692319,-18.2258897639242,
21.5555703664997));
#181242=CARTESIAN_POINT('Ctrl Pts',(16.6170005689161,-18.9535520277953,
21.5099894676285));
#181243=CARTESIAN_POINT('Ctrl Pts',(16.6170514757345,-19.0229900275103,
21.5054225881129));
#181244=CARTESIAN_POINT('Ctrl Pts',(16.620518744223,-19.0923904496927,21.5009009048524));
#181245=CARTESIAN_POINT('Ctrl Pts',(16.6297026110579,-19.1847375792016,
21.4950376377229));
#181246=CARTESIAN_POINT('Ctrl Pts',(16.6323978968568,-19.2079355069445,
21.4935779411454));
#181247=CARTESIAN_POINT('Ctrl Pts',(16.6362853529812,-19.2371664355986,
21.4917592136074));
#181248=CARTESIAN_POINT('Ctrl Pts',(16.6371205542672,-19.2432442762527,
21.491382182899));
#181249=CARTESIAN_POINT('Ctrl Pts',(16.6385604120732,-19.2533948985387,
21.4907544855754));
#181250=CARTESIAN_POINT('Ctrl Pts',(16.6391505446227,-19.2574696572047,
21.4905030441404));
#181251=CARTESIAN_POINT('Ctrl Pts',(16.6402462872948,-19.2648830325642,
21.4900465921496));
#181252=CARTESIAN_POINT('Ctrl Pts',(16.6407480030291,-19.2682221989029,
21.4898413667541));
#181253=CARTESIAN_POINT('Ctrl Pts',(16.6417946456342,-19.2750764736125,
21.4894208862801));
#181254=CARTESIAN_POINT('Ctrl Pts',(16.64234044042,-19.2785913960278,21.489205687508));
#181255=CARTESIAN_POINT('Ctrl Pts',(16.6435933949801,-19.286528444324,21.4887207108561));
#181256=CARTESIAN_POINT('Ctrl Pts',(16.6443057263194,-19.2909496979963,
21.4884512303207));
#181257=CARTESIAN_POINT('Ctrl Pts',(16.6465011846869,-19.3043063085817,
21.4876390674743));
#181258=CARTESIAN_POINT('Ctrl Pts',(16.6480276539481,-19.3132345736134,
21.4870987991144));
#181259=CARTESIAN_POINT('Ctrl Pts',(16.6601842244475,-19.3816901054389,
21.4829746672044));
#181260=CARTESIAN_POINT('Ctrl Pts',(16.6733041426196,-19.4407529849975,
21.4795222754193));
#181261=CARTESIAN_POINT('Ctrl Pts',(16.6938224022332,-19.5174393922494,
21.4750845544611));
#181262=CARTESIAN_POINT('Ctrl Pts',(16.6989527891217,-19.5356344855662,
21.4740350315778));
#181263=CARTESIAN_POINT('Ctrl Pts',(16.7159624561297,-19.5930064378668,
21.4707298068458));
#181264=CARTESIAN_POINT('Ctrl Pts',(16.7287348634327,-19.6319093108685,
21.4684945478098));
#181265=CARTESIAN_POINT('Ctrl Pts',(16.7545785188735,-19.7035449482025,
21.4643518492426));
#181266=CARTESIAN_POINT('Ctrl Pts',(16.7673542878302,-19.7363684517502,
21.4624429450972));
#181267=CARTESIAN_POINT('Ctrl Pts',(16.8090252811438,-19.8360012189636,
21.4565793344634));
#181268=CARTESIAN_POINT('Ctrl Pts',(16.8405504665062,-19.9016494246912,
21.452616563004));
#181269=CARTESIAN_POINT('Ctrl Pts',(16.9018314006153,-20.0140248950145,
21.445503598111));
#181270=CARTESIAN_POINT('Ctrl Pts',(16.9301557787408,-20.0614521294023,
21.4423912249842));
#181271=CARTESIAN_POINT('Ctrl Pts',(16.9790291445708,-20.1364590544566,
21.437242443796));
#181272=CARTESIAN_POINT('Ctrl Pts',(16.9984530235103,-20.1647417077771,
21.4352459079915));
#181273=CARTESIAN_POINT('Ctrl Pts',(17.0248611085902,-20.2012594082697,
21.4325885617402));
#181274=CARTESIAN_POINT('Ctrl Pts',(17.0312338007241,-20.2099316688001,
21.4319514451171));
#181275=CARTESIAN_POINT('Ctrl Pts',(17.0417740979783,-20.2240485456339,
21.4309042020825));
#181276=CARTESIAN_POINT('Ctrl Pts',(17.0459025703592,-20.2295222394353,
21.4304956168755));
#181277=CARTESIAN_POINT('Ctrl Pts',(17.0539413835458,-20.2400734125033,
21.4297030690238));
#181278=CARTESIAN_POINT('Ctrl Pts',(17.0578483390271,-20.2451533856151,
21.4293192434305));
#181279=CARTESIAN_POINT('Ctrl Pts',(17.0669162730086,-20.2568337239774,
21.4284314759975));
#181280=CARTESIAN_POINT('Ctrl Pts',(17.0720934640131,-20.26342131388,21.427926888305));
#181281=CARTESIAN_POINT('Ctrl Pts',(17.0861067224784,-20.2810358966646,
21.4265670572115));
#181282=CARTESIAN_POINT('Ctrl Pts',(17.095014197555,-20.2920052958124,21.425708937557));
#181283=CARTESIAN_POINT('Ctrl Pts',(17.1997104957267,-20.4183312382032,
21.4156928955381));
#181284=CARTESIAN_POINT('Ctrl Pts',(17.30736564342,-20.5232638048164,21.4060185095525));
#181285=CARTESIAN_POINT('Ctrl Pts',(17.4998886808629,-20.6746996138827,
21.3898623194387));
#181286=CARTESIAN_POINT('Ctrl Pts',(17.5784756438701,-20.728369537953,21.3835372013986));
#181287=CARTESIAN_POINT('Ctrl Pts',(17.6991998501707,-20.7994046229204,
21.3744154243431));
#181288=CARTESIAN_POINT('Ctrl Pts',(17.7387161832013,-20.8209905935789,
21.3715175782669));
#181289=CARTESIAN_POINT('Ctrl Pts',(17.8009151235537,-20.8524342986676,
21.367122344912));
#181290=CARTESIAN_POINT('Ctrl Pts',(17.8231312489496,-20.8631818732465,
21.3655841969589));
#181291=CARTESIAN_POINT('Ctrl Pts',(17.8514873236358,-20.876292969929,21.3636654975228));
#181292=CARTESIAN_POINT('Ctrl Pts',(17.8574561994436,-20.8790192075851,
21.3632640852257));
#181293=CARTESIAN_POINT('Ctrl Pts',(17.8664998554624,-20.8830991129605,
21.3626597245716));
#181294=CARTESIAN_POINT('Ctrl Pts',(17.8695652741808,-20.8844732572568,
21.3624555348102));
#181295=CARTESIAN_POINT('Ctrl Pts',(17.8758768732228,-20.8872845532612,
21.362036496942));
#181296=CARTESIAN_POINT('Ctrl Pts',(17.8791233500479,-20.8887208152752,
21.3618217113365));
#181297=CARTESIAN_POINT('Ctrl Pts',(17.8864142923672,-20.8919244698704,
21.3613410118763));
#181298=CARTESIAN_POINT('Ctrl Pts',(17.8904606766289,-20.8936873824908,
21.3610753741924));
#181299=CARTESIAN_POINT('Ctrl Pts',(17.9007719012331,-20.8981414195365,
21.3604012976051));
#181300=CARTESIAN_POINT('Ctrl Pts',(17.9070443375919,-20.9008149795909,
21.3599939052019));
#181301=CARTESIAN_POINT('Ctrl Pts',(17.9427393211832,-20.9158262225968,
21.3576899849652));
#181302=CARTESIAN_POINT('Ctrl Pts',(17.9724265960238,-20.9275285599298,
21.3558294339172));
#181303=CARTESIAN_POINT('Ctrl Pts',(18.1885432690977,-21.0071224391009,
21.3426052568029));
#181304=CARTESIAN_POINT('Ctrl Pts',(18.3834490244943,-21.0491849386751,
21.3322947224257));
#181305=CARTESIAN_POINT('Ctrl Pts',(18.6371247253503,-21.0675206933882,
21.3181606462519));
#181306=CARTESIAN_POINT('Ctrl Pts',(18.6930029352775,-21.0693405949616,
21.3150107969211));
#181307=CARTESIAN_POINT('Ctrl Pts',(18.7835680454164,-21.0687038019494,
21.309801662039));
#181308=CARTESIAN_POINT('Ctrl Pts',(18.8182383208852,-21.0676076382361,
21.307782974275));
#181309=CARTESIAN_POINT('Ctrl Pts',(18.8637161113335,-21.0650501312871,
21.3050967260059));
#181310=CARTESIAN_POINT('Ctrl Pts',(18.8745625673642,-21.0643563347299,
21.3044532004413));
#181311=CARTESIAN_POINT('Ctrl Pts',(18.8923078656794,-21.063083973047,21.303395506849));
#181312=CARTESIAN_POINT('Ctrl Pts',(18.8992101478068,-21.0625550281638,
21.3029828981763));
#181313=CARTESIAN_POINT('Ctrl Pts',(18.9125583738092,-21.0614662286663,
21.3021825812569));
#181314=CARTESIAN_POINT('Ctrl Pts',(18.9190045968349,-21.0609106572951,
21.3017950117789));
#181315=CARTESIAN_POINT('Ctrl Pts',(18.9338721230383,-21.0595606001864,
21.300898600921));
#181316=CARTESIAN_POINT('Ctrl Pts',(18.942291371816,-21.058745179232,21.3003891073578));
#181317=CARTESIAN_POINT('Ctrl Pts',(18.9648977846113,-21.0564188673869,
21.2990159480839));
#181318=CARTESIAN_POINT('Ctrl Pts',(18.9790747481408,-21.0548149962795,
21.2981493777601));
#181319=CARTESIAN_POINT('Ctrl Pts',(19.1068139128671,-21.0390542716253,
21.2902909847284));
#181320=CARTESIAN_POINT('Ctrl Pts',(19.2190520317045,-21.0158563304589,
21.2830111545704));
#181321=CARTESIAN_POINT('Ctrl Pts',(19.4859266474189,-20.9377197327291,
21.2648703778687));
#181322=CARTESIAN_POINT('Ctrl Pts',(19.637133800448,-20.8736725972321,21.2538528597599));
#181323=CARTESIAN_POINT('Ctrl Pts',(19.8079481029028,-20.7766639129949,
21.2413707544212));
#181324=CARTESIAN_POINT('Ctrl Pts',(19.8360663236225,-20.7598199618748,
21.2393167900982));
#181325=CARTESIAN_POINT('Ctrl Pts',(19.8699385060303,-20.7384449825376,
21.2368539161157));
#181326=CARTESIAN_POINT('Ctrl Pts',(19.8760732407335,-20.7345292932913,
21.2364083234476));
#181327=CARTESIAN_POINT('Ctrl Pts',(19.8856564238649,-20.7283427392234,
21.2357131445788));
#181328=CARTESIAN_POINT('Ctrl Pts',(19.8891185620725,-20.726093332958,21.2354621790488));
#181329=CARTESIAN_POINT('Ctrl Pts',(19.8955710570241,-20.7218741484199,
21.2349948231166));
#181330=CARTESIAN_POINT('Ctrl Pts',(19.8985629708215,-20.7199069288454,
21.2347782737317));
#181331=CARTESIAN_POINT('Ctrl Pts',(19.9053761830702,-20.7154023583099,
21.2342854893252));
#181332=CARTESIAN_POINT('Ctrl Pts',(19.9091942256614,-20.7128601796951,
21.2340095821272));
#181333=CARTESIAN_POINT('Ctrl Pts',(19.9209015364339,-20.7050100275109,
21.233164215217));
#181334=CARTESIAN_POINT('Ctrl Pts',(19.9287634550979,-20.6996612107963,
21.2325974300523));
#181335=CARTESIAN_POINT('Ctrl Pts',(19.9989616830963,-20.6512071007596,
21.2275423215691));
#181336=CARTESIAN_POINT('Ctrl Pts',(20.0589845694252,-20.6048313017748,
21.2232594657571));
#181337=CARTESIAN_POINT('Ctrl Pts',(20.2235750656522,-20.4629209023133,
21.2112292821058));
#181338=CARTESIAN_POINT('Ctrl Pts',(20.3212188237948,-20.35999665412,21.2037067473853));
#181339=CARTESIAN_POINT('Ctrl Pts',(20.4457144141763,-20.1992148075485,
21.1924562677934));
#181340=CARTESIAN_POINT('Ctrl Pts',(20.4814022607839,-20.1487019229487,
21.1889868977398));
#181341=CARTESIAN_POINT('Ctrl Pts',(20.5349766171185,-20.0653556732191,
21.1833006273557));
#181342=CARTESIAN_POINT('Ctrl Pts',(20.5542939889263,-20.0334837838675,
21.1811348733856));
#181343=CARTESIAN_POINT('Ctrl Pts',(20.578279529162,-19.9914450901906,21.1782817260774));
#181344=CARTESIAN_POINT('Ctrl Pts',(20.5837231445138,-19.9817268369287,
21.1776224012635));
#181345=CARTESIAN_POINT('Ctrl Pts',(20.5924494090229,-19.965855719353,21.1765458481843));
#181346=CARTESIAN_POINT('Ctrl Pts',(20.5957788408715,-19.959728719179,21.1761302977831));
#181347=CARTESIAN_POINT('Ctrl Pts',(20.6021220740288,-19.9479168221561,
21.1753292269764));
#181348=CARTESIAN_POINT('Ctrl Pts',(20.6051403520067,-19.9422344075029,
21.174943871447));
#181349=CARTESIAN_POINT('Ctrl Pts',(20.6119900834686,-19.92919549933,21.1740596351986));
#181350=CARTESIAN_POINT('Ctrl Pts',(20.615804283385,-19.9218301054796,21.1735601516561));
#181351=CARTESIAN_POINT('Ctrl Pts',(20.6258185648125,-19.9022105666896,
21.1722295668705));
#181352=CARTESIAN_POINT('Ctrl Pts',(20.6319427775811,-19.8899183345578,
21.1713958232673));
#181353=CARTESIAN_POINT('Ctrl Pts',(20.6774820204886,-19.7962414414736,
21.1650403524921));
#181354=CARTESIAN_POINT('Ctrl Pts',(20.7117607596288,-19.7124765686798,
21.1593417739695));
#181355=CARTESIAN_POINT('Ctrl Pts',(20.7851821673454,-19.4941470710627,
21.144468198504));
#181356=CARTESIAN_POINT('Ctrl Pts',(20.8165236172352,-19.3574160158983,
21.135116863114));
#181357=CARTESIAN_POINT('Ctrl Pts',(20.8410813995823,-19.1639686555513,
21.1223459890741));
#181358=CARTESIAN_POINT('Ctrl Pts',(20.8458833598798,-19.1090740002333,
21.1187766099113));
#181359=CARTESIAN_POINT('Ctrl Pts',(20.8499084970286,-19.0256716074268,
21.1134918171265));
#181360=CARTESIAN_POINT('Ctrl Pts',(20.8507067513395,-18.997265727816,21.1117161926146));
#181361=CARTESIAN_POINT('Ctrl Pts',(20.8509881550703,-18.9619136032291,
21.1095435934988));
#181362=CARTESIAN_POINT('Ctrl Pts',(20.851009275974,-18.9549760302146,21.1091190226181));
#181363=CARTESIAN_POINT('Ctrl Pts',(20.8509887281256,-18.943995775956,21.108450002406));
#181364=CARTESIAN_POINT('Ctrl Pts',(20.8509695834442,-18.9399531739421,
21.1082043236695));
#181365=CARTESIAN_POINT('Ctrl Pts',(20.8509116405711,-18.9323294206652,
21.1077422381066));
#181366=CARTESIAN_POINT('Ctrl Pts',(20.8508753357138,-18.9287483567602,
21.107525700363));
#181367=CARTESIAN_POINT('Ctrl Pts',(20.8507715502681,-18.9205607228903,
21.1070317729593));
#181368=CARTESIAN_POINT('Ctrl Pts',(20.8506981199238,-18.9159542762498,
21.1067547192566));
#181369=CARTESIAN_POINT('Ctrl Pts',(20.8504631957205,-18.9037225650517,
21.1060211765708));
#181370=CARTESIAN_POINT('Ctrl Pts',(20.8502755294535,-18.8960977910171,
21.1055661137898));
#181371=CARTESIAN_POINT('Ctrl Pts',(20.8486704700771,-18.8426333170003,
21.102389630185));
#181372=CARTESIAN_POINT('Ctrl Pts',(20.8458049307357,-18.7968456285292,
21.0997433818247));
#181373=CARTESIAN_POINT('Ctrl Pts',(20.8378764030201,-18.7136402040259,
21.0950120349543));
#181374=CARTESIAN_POINT('Ctrl Pts',(20.8332961902683,-18.6761974474987,
21.0929116943981));
#181375=CARTESIAN_POINT('Ctrl Pts',(20.8083599867846,-18.5094499292422,
21.0836114693363));
#181376=CARTESIAN_POINT('Ctrl Pts',(20.7770394305811,-18.3820778286941,
21.0766340367471));
#181377=CARTESIAN_POINT('Ctrl Pts',(20.7052143912656,-18.1749503400491,
21.0645333126297));
#181378=CARTESIAN_POINT('Ctrl Pts',(20.6710804829987,-18.093391249084,21.0595612181679));
#181379=CARTESIAN_POINT('Ctrl Pts',(20.6228634134068,-17.9958068894792,
21.0532176350172));
#181380=CARTESIAN_POINT('Ctrl Pts',(20.6135045225415,-17.9775396544109,
21.0520126166617));
#181381=CARTESIAN_POINT('Ctrl Pts',(20.5997293308401,-17.9515893352124,
21.0502742671261));
#181382=CARTESIAN_POINT('Ctrl Pts',(20.5955279170785,-17.9437930547351,
21.0497485408595));
#181383=CARTESIAN_POINT('Ctrl Pts',(20.5881610424839,-17.930325881316,21.0488342716432));
#181384=CARTESIAN_POINT('Ctrl Pts',(20.5850181554353,-17.924642728623,21.0484465390221));
#181385=CARTESIAN_POINT('Ctrl Pts',(20.5789258966257,-17.9137450576527,
21.047699324946));
#181386=CARTESIAN_POINT('Ctrl Pts',(20.5759804390021,-17.9085284141219,
21.0473399870205));
#181387=CARTESIAN_POINT('Ctrl Pts',(20.5682085162118,-17.8948991601638,
21.0463967903315));
#181388=CARTESIAN_POINT('Ctrl Pts',(20.5633463524841,-17.8865071636666,
21.0458116441741));
#181389=CARTESIAN_POINT('Ctrl Pts',(20.5462830393813,-17.8575173275916,
21.0437748159947));
#181390=CARTESIAN_POINT('Ctrl Pts',(20.5337906375998,-17.8370938506119,
21.0423125608835));
#181391=CARTESIAN_POINT('Ctrl Pts',(20.437688250306,-17.6858043523982,21.0312702200361));
#181392=CARTESIAN_POINT('Ctrl Pts',(20.3402658860461,-17.5643046430061,
21.0211539584876));
#181393=CARTESIAN_POINT('Ctrl Pts',(20.1778803722248,-17.4020245537588,
21.0059870829959));
#181394=CARTESIAN_POINT('Ctrl Pts',(20.1225696484507,-17.3522846203843,
21.0010639598907));
#181395=CARTESIAN_POINT('Ctrl Pts',(20.028998481291,-17.276654713559,20.9932278202406));
#181396=CARTESIAN_POINT('Ctrl Pts',(19.9923064786629,-17.2489238869821,
20.9902670047035));
#181397=CARTESIAN_POINT('Ctrl Pts',(19.9410818214538,-17.2127697453463,
20.9863123316715));
#181398=CARTESIAN_POINT('Ctrl Pts',(19.9273112377688,-17.2032928406762,
20.9852661631811));
#181399=CARTESIAN_POINT('Ctrl Pts',(19.9035327472823,-17.1873402083815,
20.9834904469739));
#181400=CARTESIAN_POINT('Ctrl Pts',(19.8935799343699,-17.1807841978066,
20.9827562531052));
#181401=CARTESIAN_POINT('Ctrl Pts',(19.8793557607081,-17.1715858930414,
20.9817203767252));
#181402=CARTESIAN_POINT('Ctrl Pts',(19.875129755275,-17.1688743472027,20.9814142824737));
#181403=CARTESIAN_POINT('Ctrl Pts',(19.8678311048005,-17.1642278640575,
20.9808885509462));
#181404=CARTESIAN_POINT('Ctrl Pts',(19.8647630701667,-17.1622857590666,
20.9806684405972));
#181405=CARTESIAN_POINT('Ctrl Pts',(19.8588031819148,-17.1585345174327,
20.9802425906173));
#181406=CARTESIAN_POINT('Ctrl Pts',(19.8559119557867,-17.1567244782347,
20.9800367880116));
#181407=CARTESIAN_POINT('Ctrl Pts',(19.8481023035486,-17.1518615142039,
20.9794829568551));
#181408=CARTESIAN_POINT('Ctrl Pts',(19.8431756674405,-17.1488217361098,
20.9791357894279));
#181409=CARTESIAN_POINT('Ctrl Pts',(19.824860016079,-17.1376242850711,20.9778530720615));
#181410=CARTESIAN_POINT('Ctrl Pts',(19.811392596281,-17.1295949858659,20.9769255598791));
#181411=CARTESIAN_POINT('Ctrl Pts',(19.6817599742594,-17.0542471521348,
20.9681342241796));
#181412=CARTESIAN_POINT('Ctrl Pts',(19.5595112920428,-16.9979642118648,
20.9608716898857));
#181413=CARTESIAN_POINT('Ctrl Pts',(19.2810467922208,-16.9005973156725,
20.9448519428443));
#181414=CARTESIAN_POINT('Ctrl Pts',(19.1238293827648,-16.865007414114,20.9361045840124));
#181415=CARTESIAN_POINT('Ctrl Pts',(18.9455575971384,-16.8455146318888,
20.9256316173492));
#181416=CARTESIAN_POINT('Ctrl Pts',(18.9269818773604,-16.8437317094385,
20.9245344936359));
#181417=CARTESIAN_POINT('Ctrl Pts',(18.8998851475894,-16.8414920359134,
20.9229246681688));
#181418=CARTESIAN_POINT('Ctrl Pts',(18.8913807799546,-16.8408408313162,
20.9224180718565));
#181419=CARTESIAN_POINT('Ctrl Pts',(18.8764412597701,-16.8397876390288,
20.9215256834124));
#181420=CARTESIAN_POINT('Ctrl Pts',(18.8700077344895,-16.8393636221384,
20.9211405879492));
#181421=CARTESIAN_POINT('Ctrl Pts',(18.8574951701933,-16.8385963436045,
20.9203900242757));
#181422=CARTESIAN_POINT('Ctrl Pts',(18.8514163839996,-16.838249905147,20.9200246597673));
#181423=CARTESIAN_POINT('Ctrl Pts',(18.836854598859,-16.8374830175194,20.9191476427967));
#181424=CARTESIAN_POINT('Ctrl Pts',(18.8283704481463,-16.8370873888186,
20.9186352166053));
#181425=CARTESIAN_POINT('Ctrl Pts',(18.797586088843,-16.8358374739629,20.9167705181264));
#181426=CARTESIAN_POINT('Ctrl Pts',(18.7752757174883,-16.8352847894329,
20.9154088510575));
#181427=CARTESIAN_POINT('Ctrl Pts',(18.5696370358765,-16.8334428625074,
20.902759415006));
#181428=CARTESIAN_POINT('Ctrl Pts',(18.3869084940813,-16.855622073206,20.8906947770097));
#181429=CARTESIAN_POINT('Ctrl Pts',(18.1303751017278,-16.9212430484505,
20.873210704081));
#181430=CARTESIAN_POINT('Ctrl Pts',(18.0526121623917,-16.9459967132677,
20.8678505798224));
#181431=CARTESIAN_POINT('Ctrl Pts',(17.9424738267629,-16.9882025260496,
20.8603296450368));
#181432=CARTESIAN_POINT('Ctrl Pts',(17.9088201517948,-17.0021044161105,
20.8580420077422));
#181433=CARTESIAN_POINT('Ctrl Pts',(17.8686912632749,-17.0199063379301,
20.8553410607037));
#181434=CARTESIAN_POINT('Ctrl Pts',(17.8618590201806,-17.0229807559185,
20.8548821606062));
#181435=CARTESIAN_POINT('Ctrl Pts',(17.8512527308878,-17.0278213132715,
20.8541714267529));
#181436=CARTESIAN_POINT('Ctrl Pts',(17.8474674131566,-17.0295623982193,
20.8539181004372));
#181437=CARTESIAN_POINT('Ctrl Pts',(17.8404512827614,-17.0328146490806,
20.8534492048727));
#181438=CARTESIAN_POINT('Ctrl Pts',(17.8372191776505,-17.0343227909208,
20.8532334596927));
#181439=CARTESIAN_POINT('Ctrl Pts',(17.8299130309321,-17.0377544438658,
20.8527463458966));
#181440=CARTESIAN_POINT('Ctrl Pts',(17.8258413198539,-17.0396827906032,
20.8524752803585));
#181441=CARTESIAN_POINT('Ctrl Pts',(17.8135516627866,-17.045551229067,20.8516582496771));
#181442=CARTESIAN_POINT('Ctrl Pts',(17.8053528508338,-17.0495314623478,
20.8511147112901));
#181443=CARTESIAN_POINT('Ctrl Pts',(17.742406216224,-17.0805937132484,20.8469515463504));
#181444=CARTESIAN_POINT('Ctrl Pts',(17.6888224654806,-17.1099834118851,
20.8434650927345));
#181445=CARTESIAN_POINT('Ctrl Pts',(17.4971413360328,-17.2261791556759,
20.8309358352664));
#181446=CARTESIAN_POINT('Ctrl Pts',(17.3679310295523,-17.3265344579058,
20.822334812292));
#181447=CARTESIAN_POINT('Ctrl Pts',(17.1948920697157,-17.4962777335003,
20.8088862716257));
#181448=CARTESIAN_POINT('Ctrl Pts',(17.1414401068225,-17.5549561348151,
20.8043989609515));
#181449=CARTESIAN_POINT('Ctrl Pts',(17.0791842933686,-17.6315267840372,
20.7986403172648));
#181450=CARTESIAN_POINT('Ctrl Pts',(17.0671665414322,-17.6467296366283,
20.7975015884369));
#181451=CARTESIAN_POINT('Ctrl Pts',(17.0500837422399,-17.668960636741,20.7958420316206));
#181452=CARTESIAN_POINT('Ctrl Pts',(17.044850238435,-17.6758585304013,20.7953278661296));
#181453=CARTESIAN_POINT('Ctrl Pts',(17.0357827044756,-17.6879632815061,
20.7944268228756));
#181454=CARTESIAN_POINT('Ctrl Pts',(17.0319299155863,-17.6931559926538,
20.7940406860234));
#181455=CARTESIAN_POINT('Ctrl Pts',(17.024519245587,-17.7032401613848,20.7932915348351));
#181456=CARTESIAN_POINT('Ctrl Pts',(17.0209584160246,-17.708129381874,20.7929286403344));
#181457=CARTESIAN_POINT('Ctrl Pts',(17.0125342438771,-17.719801029225,20.792063066597));
#181458=CARTESIAN_POINT('Ctrl Pts',(17.007689987609,-17.7265970495051,20.7915596575451));
#181459=CARTESIAN_POINT('Ctrl Pts',(16.9905654135399,-17.7509242367281,
20.7897596025362));
#181460=CARTESIAN_POINT('Ctrl Pts',(16.9785112585108,-17.768612332288,20.7884543812602));
#181461=CARTESIAN_POINT('Ctrl Pts',(16.8760651530056,-17.923950817612,20.7770190472491));
#181462=CARTESIAN_POINT('Ctrl Pts',(16.8018176257906,-18.0714332124806,
20.7662793014811));
#181463=CARTESIAN_POINT('Ctrl Pts',(16.7454193641621,-18.2258897778089,
20.7554136941352));
#181464=CARTESIAN_POINT('',(16.6170002905217,-18.953109084689,21.2890562789773));
#181465=CARTESIAN_POINT('Ctrl Pts',(16.6170002905217,-18.953109084689,21.2890562789773));
#181466=CARTESIAN_POINT('Ctrl Pts',(16.6170426459378,-19.0339562954196,
21.2842160179952));
#181467=CARTESIAN_POINT('Ctrl Pts',(16.6217204202766,-19.1146414522941,
21.2793757570132));
#181468=CARTESIAN_POINT('Ctrl Pts',(16.6309534061133,-19.1946603056566,
21.2745354960311));
#181469=CARTESIAN_POINT('Ctrl Pts',(16.6402204413664,-19.2749742526441,
21.2696773851287));
#181470=CARTESIAN_POINT('Ctrl Pts',(16.6540762119897,-19.354616695186,21.2648192742263));
#181471=CARTESIAN_POINT('Ctrl Pts',(16.6723897124588,-19.4330946084755,
21.2599611633239));
#181472=CARTESIAN_POINT('Ctrl Pts',(16.6907932575821,-19.5119583855476,
21.2550791658403));
#181473=CARTESIAN_POINT('Ctrl Pts',(16.7136983366374,-19.5896458842218,
21.2501971683567));
#181474=CARTESIAN_POINT('Ctrl Pts',(16.7409237561882,-19.6656778589483,
21.2453151708731));
#181475=CARTESIAN_POINT('Ctrl Pts',(16.7538532441133,-19.7017858240547,
21.2429966858486));
#181476=CARTESIAN_POINT('Ctrl Pts',(16.7677564318017,-19.7375207423804,
21.240678200824));
#181477=CARTESIAN_POINT('Ctrl Pts',(16.7826102745739,-19.7728331983426,
21.2383597157995));
#181478=CARTESIAN_POINT('Ctrl Pts',(16.810725579552,-19.8396724993995,21.2339712949342));
#181479=CARTESIAN_POINT('Ctrl Pts',(16.842333782473,-19.9051959888482,21.2295828740689));
#181480=CARTESIAN_POINT('Ctrl Pts',(16.8772900904223,-19.9690139191162,
21.2251944532036));
#181481=CARTESIAN_POINT('Ctrl Pts',(16.9121945323206,-20.0327371602073,
21.2208125436112));
#181482=CARTESIAN_POINT('Ctrl Pts',(16.9504369878248,-20.0947594462028,
21.2164306340188));
#181483=CARTESIAN_POINT('Ctrl Pts',(16.9918247589115,-20.1547112826186,
21.2120487244264));
#181484=CARTESIAN_POINT('Ctrl Pts',(17.0331639104988,-20.2145926917514,
21.2076719623992));
#181485=CARTESIAN_POINT('Ctrl Pts',(17.0776407650442,-20.2724080879841,
21.203295200372));
#181486=CARTESIAN_POINT('Ctrl Pts',(17.1250177576845,-20.3278143566315,
21.1989184383448));
#181487=CARTESIAN_POINT('Ctrl Pts',(17.1723647132798,-20.3831854976676,
21.1945444511876));
#181488=CARTESIAN_POINT('Ctrl Pts',(17.2226078460713,-20.4361501759871,
21.1901704640305));
#181489=CARTESIAN_POINT('Ctrl Pts',(17.2754683635278,-20.4863971016037,
21.1857964768734));
#181490=CARTESIAN_POINT('Ctrl Pts',(17.3283128004351,-20.5366287417445,
21.1814238203145));
#181491=CARTESIAN_POINT('Ctrl Pts',(17.3837726918675,-20.5841439384587,
21.1770511637557));
#181492=CARTESIAN_POINT('Ctrl Pts',(17.4415325036287,-20.6286683544529,
21.1726785071969));
#181493=CARTESIAN_POINT('Ctrl Pts',(17.4992937927453,-20.6731939092732,
21.1683057387962));
#181494=CARTESIAN_POINT('Ctrl Pts',(17.5593547357629,-20.7147282386116,
21.1639329703954));
#181495=CARTESIAN_POINT('Ctrl Pts',(17.6213681906132,-20.7530384384407,
21.1595602019947));
#181496=CARTESIAN_POINT('Ctrl Pts',(17.6834459816507,-20.7913883833894,
21.1551828970422));
#181497=CARTESIAN_POINT('Ctrl Pts',(17.7474799176421,-20.8265072664897,
21.1508055920898));
#181498=CARTESIAN_POINT('Ctrl Pts',(17.8130961649932,-20.858206999953,21.1464282871373));
#181499=CARTESIAN_POINT('Ctrl Pts',(17.8787482388868,-20.8899240415053,
21.1420485921716));
#181500=CARTESIAN_POINT('Ctrl Pts',(17.945983899379,-20.9182180292927,21.1376688972058));
#181501=CARTESIAN_POINT('Ctrl Pts',(18.0144096452291,-20.9429492010899,
21.1332892022401));
#181502=CARTESIAN_POINT('Ctrl Pts',(18.0829566199304,-20.9677241887274,
21.1289017478355));
#181503=CARTESIAN_POINT('Ctrl Pts',(18.1526974286133,-20.9889236147803,
21.124514293431));
#181504=CARTESIAN_POINT('Ctrl Pts',(18.2232243125218,-21.0064578839882,
21.1201268390264));
#181505=CARTESIAN_POINT('Ctrl Pts',(18.2711425297296,-21.018371226446,21.1171458623903));
#181506=CARTESIAN_POINT('Ctrl Pts',(18.3194233717923,-21.0285936957892,
21.1141648857542));
#181507=CARTESIAN_POINT('Ctrl Pts',(18.3679374554048,-21.0371108396065,
21.1111839091181));
#181508=CARTESIAN_POINT('Ctrl Pts',(18.4393551978057,-21.0496489550946,
21.1067956035861));
#181509=CARTESIAN_POINT('Ctrl Pts',(18.5115571842922,-21.0585380615907,
21.102407298054));
#181510=CARTESIAN_POINT('Ctrl Pts',(18.5841373443173,-21.0636889412107,
21.098018992522));
#181511=CARTESIAN_POINT('Ctrl Pts',(18.6566098258321,-21.0688321790862,
21.0936371973945));
#181512=CARTESIAN_POINT('Ctrl Pts',(18.7294588899518,-21.07024816573,21.089255402267));
#181513=CARTESIAN_POINT('Ctrl Pts',(18.8022695648095,-21.067898926348,21.0848736071394));
#181514=CARTESIAN_POINT('Ctrl Pts',(18.8749947356317,-21.0655524457572,
21.080496957702));
#181515=CARTESIAN_POINT('Ctrl Pts',(18.9476811270357,-21.0594495382254,
21.0761203082645));
#181516=CARTESIAN_POINT('Ctrl Pts',(19.0199116621127,-21.0496042337553,
21.0717436588271));
#181517=CARTESIAN_POINT('Ctrl Pts',(19.0920964218622,-21.0397651686413,
21.0673697830443));
#181518=CARTESIAN_POINT('Ctrl Pts',(19.1638254217295,-21.0261884773497,
21.0629959072615));
#181519=CARTESIAN_POINT('Ctrl Pts',(19.2346860285047,-21.0089400819811,
21.0586220314788));
#181520=CARTESIAN_POINT('Ctrl Pts',(19.3055251008402,-20.9916969283757,
21.0542494849107));
#181521=CARTESIAN_POINT('Ctrl Pts',(19.3754958356271,-20.9707843999674,
21.0498769383427));
#181522=CARTESIAN_POINT('Ctrl Pts',(19.4441967837545,-20.9463193145394,
21.0455043917747));
#181523=CARTESIAN_POINT('Ctrl Pts',(19.512899513531,-20.9218535946485,21.0411317318117));
#181524=CARTESIAN_POINT('Ctrl Pts',(19.5803319375393,-20.8938352985226,
21.0367590718487));
#181525=CARTESIAN_POINT('Ctrl Pts',(19.6461103373975,-20.8624302479841,
21.0323864118857));
#181526=CARTESIAN_POINT('Ctrl Pts',(19.7119570287599,-20.8309925925458,
21.0280092122026));
#181527=CARTESIAN_POINT('Ctrl Pts',(19.7761458312172,-20.7961613707408,
21.0236320125194));
#181528=CARTESIAN_POINT('Ctrl Pts',(19.8383162627571,-20.7581491056417,
21.0192548128363));
#181529=CARTESIAN_POINT('Ctrl Pts',(19.9005206631089,-20.7201160713208,
21.0148752215295));
#181530=CARTESIAN_POINT('Ctrl Pts',(19.9607040986315,-20.6788988059761,
21.0104956302228));
#181531=CARTESIAN_POINT('Ctrl Pts',(20.0185360770276,-20.6347525269078,
21.006116038916));
#181532=CARTESIAN_POINT('Ctrl Pts',(20.0764705677122,-20.5905279946616,
21.0017286843969));
#181533=CARTESIAN_POINT('Ctrl Pts',(20.1320449095234,-20.5433643929912,
20.9973413298778));
#181534=CARTESIAN_POINT('Ctrl Pts',(20.1849630763877,-20.4935560810297,
20.9929539753587));
#181535=CARTESIAN_POINT('Ctrl Pts',(20.2209300198673,-20.4597028157469,
20.989972017718));
#181536=CARTESIAN_POINT('Ctrl Pts',(20.2556706968499,-20.4246286057098,
20.9869900600773));
#181537=CARTESIAN_POINT('Ctrl Pts',(20.2891028444412,-20.3884345245123,
20.9840081024366));
#181538=CARTESIAN_POINT('Ctrl Pts',(20.338299896607,-20.3351731509824,20.9796200048666));
#181539=CARTESIAN_POINT('Ctrl Pts',(20.3848536071561,-20.2792773791151,
20.9752319072966));
#181540=CARTESIAN_POINT('Ctrl Pts',(20.428469154839,-20.2210403001084,20.9708438097266));
#181541=CARTESIAN_POINT('Ctrl Pts',(20.472019950475,-20.1628896804098,20.9664622267669));
#181542=CARTESIAN_POINT('Ctrl Pts',(20.5126409556541,-20.1024050366756,
20.9620806438073));
#181543=CARTESIAN_POINT('Ctrl Pts',(20.5500756139241,-20.0399146862278,
20.9576990608477));
#181544=CARTESIAN_POINT('Ctrl Pts',(20.5874662643004,-19.9774977989509,
20.953322628843));
#181545=CARTESIAN_POINT('Ctrl Pts',(20.621677762229,-19.9130803007029,20.9489461968383));
#181546=CARTESIAN_POINT('Ctrl Pts',(20.6524961365199,-19.8470204322574,
20.9445697648336));
#181547=CARTESIAN_POINT('Ctrl Pts',(20.6832949569897,-19.7810024778609,
20.9401961096128));
#181548=CARTESIAN_POINT('Ctrl Pts',(20.7107047219756,-19.7133446569422,
20.9358224543921));
#181549=CARTESIAN_POINT('Ctrl Pts',(20.7345574961774,-19.6444295664459,
20.9314487991714));
#181550=CARTESIAN_POINT('Ctrl Pts',(20.7584030058596,-19.5755354644946,
20.9270764759762));
#181551=CARTESIAN_POINT('Ctrl Pts',(20.7786935177564,-19.5053853087556,
20.922704152781));
#181552=CARTESIAN_POINT('Ctrl Pts',(20.7953099439741,-19.4343798450118,
20.9183318295858));
#181553=CARTESIAN_POINT('Ctrl Pts',(20.8119267916513,-19.3633725802829,
20.9139593954909));
#181554=CARTESIAN_POINT('Ctrl Pts',(20.8248692606565,-19.2915104346493,
20.9095869613959));
#181555=CARTESIAN_POINT('Ctrl Pts',(20.8340690642333,-19.2192057736098,
20.905214527301));
#181556=CARTESIAN_POINT('Ctrl Pts',(20.8432784147593,-19.1468260795634,
20.9008375557824));
#181557=CARTESIAN_POINT('Ctrl Pts',(20.8487372843852,-19.0740034328328,
20.8964605842638));
#181558=CARTESIAN_POINT('Ctrl Pts',(20.8504292318327,-19.0011559421033,
20.8920836127452));
#181559=CARTESIAN_POINT('Ctrl Pts',(20.8521221031445,-18.9282686740168,
20.8877042512424));
#181560=CARTESIAN_POINT('Ctrl Pts',(20.8500439708189,-18.8553570174668,
20.8833248897395));
#181561=CARTESIAN_POINT('Ctrl Pts',(20.8442305256586,-18.7828369763254,
20.8789455282366));
#181562=CARTESIAN_POINT('Ctrl Pts',(20.8384067752504,-18.7101883819803,
20.8745584036252));
#181563=CARTESIAN_POINT('Ctrl Pts',(20.8288345526933,-18.6379332679819,
20.8701712790138));
#181564=CARTESIAN_POINT('Ctrl Pts',(20.8156011171495,-18.5664798460756,
20.8657841544023));
#181565=CARTESIAN_POINT('Ctrl Pts',(20.8066002449081,-18.5178799855435,
20.86280020152));
#181566=CARTESIAN_POINT('Ctrl Pts',(20.7959066970833,-18.4696507896963,
20.8598162486376));
#181567=CARTESIAN_POINT('Ctrl Pts',(20.7835610193721,-18.4219163953954,
20.8568322957552));
#181568=CARTESIAN_POINT('Ctrl Pts',(20.7654052821341,-18.3517174852658,
20.8524440502713));
#181569=CARTESIAN_POINT('Ctrl Pts',(20.7436033945615,-18.2823154158224,
20.8480558047873));
#181570=CARTESIAN_POINT('Ctrl Pts',(20.7182422504866,-18.2141167494895,
20.8436675593033));
#181571=CARTESIAN_POINT('Ctrl Pts',(20.6929187442307,-18.1460192950363,
20.8392858263012));
#181572=CARTESIAN_POINT('Ctrl Pts',(20.6640466341085,-18.0791221467405,
20.834904093299));
#181573=CARTESIAN_POINT('Ctrl Pts',(20.6317631446628,-18.0138187559115,
20.8305223602969));
#181574=CARTESIAN_POINT('Ctrl Pts',(20.599517588069,-17.9485920960646,20.8261457757973));
#181575=CARTESIAN_POINT('Ctrl Pts',(20.563868827466,-17.8849559039143,20.8217691912977));
#181576=CARTESIAN_POINT('Ctrl Pts',(20.525002297749,-17.823284017364,20.8173926067981));
#181577=CARTESIAN_POINT('Ctrl Pts',(20.4861604147302,-17.7616512392287,
20.813018797652));
#181578=CARTESIAN_POINT('Ctrl Pts',(20.4441050677791,-17.7019807022678,
20.8086449885059));
#181579=CARTESIAN_POINT('Ctrl Pts',(20.3990670884687,-17.6446207165102,
20.8042711793597));
#181580=CARTESIAN_POINT('Ctrl Pts',(20.3540428128668,-17.5872781836785,
20.7998987010328));
#181581=CARTESIAN_POINT('Ctrl Pts',(20.3060380043386,-17.5322451854803,
20.7955262227058));
#181582=CARTESIAN_POINT('Ctrl Pts',(20.2553251935424,-17.47983878074,20.7911537443788));
#181583=CARTESIAN_POINT('Ctrl Pts',(20.2046110851032,-17.4274310350208,
20.7867811541686));
#181584=CARTESIAN_POINT('Ctrl Pts',(20.1511891736979,-17.3776503614482,
20.7824085639583));
#181585=CARTESIAN_POINT('Ctrl Pts',(20.0953692567414,-17.3307773913496,
20.778035973748));
#181586=CARTESIAN_POINT('Ctrl Pts',(20.0394914100484,-17.2838557766281,
20.7736588456772));
#181587=CARTESIAN_POINT('Ctrl Pts',(19.9812109592545,-17.2398482010919,
20.7692817176064));
#181588=CARTESIAN_POINT('Ctrl Pts',(19.9208705927643,-17.1989948100387,
20.7649045895356));
#181589=CARTESIAN_POINT('Ctrl Pts',(19.8604972727169,-17.1581191078091,
20.7605250709931));
#181590=CARTESIAN_POINT('Ctrl Pts',(19.7980622103152,-17.120401269318,20.7561455524505));
#181591=CARTESIAN_POINT('Ctrl Pts',(19.7339345415247,-17.086036465344,20.751766033908));
#181592=CARTESIAN_POINT('Ctrl Pts',(19.6696932144357,-17.0516107540391,
20.7473787532148));
#181593=CARTESIAN_POINT('Ctrl Pts',(19.6037537269743,-17.0205501505905,
20.7429914725216));
#181594=CARTESIAN_POINT('Ctrl Pts',(19.5365065755261,-16.9930022470055,
20.7386041918285));
#181595=CARTESIAN_POINT('Ctrl Pts',(19.4907905185625,-16.9742745908536,
20.7356216242436));
#181596=CARTESIAN_POINT('Ctrl Pts',(19.4444705161313,-16.9571693364,20.7326390566587));
#181597=CARTESIAN_POINT('Ctrl Pts',(19.3976727117744,-16.9417195390578,
20.7296564890738));
#181598=CARTESIAN_POINT('Ctrl Pts',(19.3288196246044,-16.9189884246865,
20.7252682706791));
#181599=CARTESIAN_POINT('Ctrl Pts',(19.2586629666827,-16.8997544121691,
20.7208800522844));
#181600=CARTESIAN_POINT('Ctrl Pts',(19.1875916213734,-16.884164503395,20.7164918338897));
#181601=CARTESIAN_POINT('Ctrl Pts',(19.1166257528894,-16.8685977315697,
20.7121101280401));
#181602=CARTESIAN_POINT('Ctrl Pts',(19.0447483590908,-16.8566644299584,
20.7077284221905));
#181603=CARTESIAN_POINT('Ctrl Pts',(18.9723645424295,-16.8484621836267,
20.7033467163409));
#181604=CARTESIAN_POINT('Ctrl Pts',(18.9000657760626,-16.8402695748564,
20.6989701589539));
#181605=CARTESIAN_POINT('Ctrl Pts',(18.827262245817,-16.8357993666553,20.6945936015669));
#181606=CARTESIAN_POINT('Ctrl Pts',(18.7543686580674,-16.8350979905134,
20.69021704418));
#181607=CARTESIAN_POINT('Ctrl Pts',(18.6815212944638,-16.8343970591364,
20.6858432621074));
#181608=CARTESIAN_POINT('Ctrl Pts',(18.6085844678331,-16.8374602225037,
20.6814694800349));
#181609=CARTESIAN_POINT('Ctrl Pts',(18.5359759922545,-16.8442819229422,
20.6770956979624));
#181610=CARTESIAN_POINT('Ctrl Pts',(18.4633896080828,-16.8511015478521,
20.6727232466298));
#181611=CARTESIAN_POINT('Ctrl Pts',(18.3911318565986,-16.8616773944406,
20.6683507952972));
#181612=CARTESIAN_POINT('Ctrl Pts',(18.3196168456417,-16.8759519270055,
20.6639783439647));
#181613=CARTESIAN_POINT('Ctrl Pts',(18.2481000027887,-16.8902268252204,
20.6596057806294));
#181614=CARTESIAN_POINT('Ctrl Pts',(18.1773264108895,-16.9082005011352,
20.6552332172941));
#181615=CARTESIAN_POINT('Ctrl Pts',(18.1076997198728,-16.9297643660759,
20.6508606539588));
#181616=CARTESIAN_POINT('Ctrl Pts',(18.0380007641074,-16.951350611906,20.6464835523899));
#181617=CARTESIAN_POINT('Ctrl Pts',(17.9694515476174,-16.9765343433904,
20.642106450821));
#181618=CARTESIAN_POINT('Ctrl Pts',(17.9024394812806,-17.0051574014042,
20.6377293492521));
#181619=CARTESIAN_POINT('Ctrl Pts',(17.8353908149959,-17.0337960924599,
20.6333498570437));
#181620=CARTESIAN_POINT('Ctrl Pts',(17.7698814039051,-17.0658776377278,
20.6289703648353));
#181621=CARTESIAN_POINT('Ctrl Pts',(17.7062751578752,-17.1011972960687,
20.624590872627));
#181622=CARTESIAN_POINT('Ctrl Pts',(17.6425561688023,-17.1365795590437,
20.6202036177018));
#181623=CARTESIAN_POINT('Ctrl Pts',(17.5807474907214,-17.1752111409601,
20.6158163627765));
#181624=CARTESIAN_POINT('Ctrl Pts',(17.5211845891613,-17.2168435865225,
20.6114291078513));
#181625=CARTESIAN_POINT('Ctrl Pts',(17.480688941821,-17.2451486688682,20.608446299365));
#181626=CARTESIAN_POINT('Ctrl Pts',(17.4412307372722,-17.2748399742566,
20.6054634908787));
#181627=CARTESIAN_POINT('Ctrl Pts',(17.4029060721978,-17.305829305519,20.6024806823923));
#181628=CARTESIAN_POINT('Ctrl Pts',(17.3472665725173,-17.3508194152439,
20.5981502604174));
#181629=CARTESIAN_POINT('Ctrl Pts',(17.2937883055875,-17.3987327323833,
20.5938198384424));
#181630=CARTESIAN_POINT('Ctrl Pts',(17.2428007358767,-17.4493311227425,
20.5894894164674));
#181631=CARTESIAN_POINT('Ctrl Pts',(17.1918849324912,-17.4998582945566,
20.5851650896735));
#181632=CARTESIAN_POINT('Ctrl Pts',(17.1434532240763,-17.553062699864,20.5808407628797));
#181633=CARTESIAN_POINT('Ctrl Pts',(17.0978028464621,-17.608665389877,20.5765164360858));
#181634=CARTESIAN_POINT('Ctrl Pts',(17.0522038396047,-17.6642055097116,
20.5721969754935));
#181635=CARTESIAN_POINT('Ctrl Pts',(17.0093802643348,-17.7221381759371,
20.5678775149012));
#181636=CARTESIAN_POINT('Ctrl Pts',(16.9695918504464,-17.7821483505209,
20.563558054309));
#181637=CARTESIAN_POINT('Ctrl Pts',(16.9298290257308,-17.8421199306856,
20.5592413716968));
#181638=CARTESIAN_POINT('Ctrl Pts',(16.8930977626958,-17.9041659555432,
20.5549246890847));
#181639=CARTESIAN_POINT('Ctrl Pts',(16.8596158552961,-17.9679405109026,
20.5506080064725));
#181640=CARTESIAN_POINT('Ctrl Pts',(16.8261394677777,-18.031704552286,20.5462920355157));
#181641=CARTESIAN_POINT('Ctrl Pts',(16.7959116072599,-18.0971961216295,
20.5419760645588));
#181642=CARTESIAN_POINT('Ctrl Pts',(16.7691044222789,-18.164044183566,20.5376600936019));
#181643=CARTESIAN_POINT('Ctrl Pts',(16.7608869615361,-18.184535754206,20.5363370780771));
#181644=CARTESIAN_POINT('Ctrl Pts',(16.7529905929685,-18.2051546356672,
20.5350140625523));
#181645=CARTESIAN_POINT('Ctrl Pts',(16.7454193692319,-18.2258897639242,
20.5336910470276));
#181646=CARTESIAN_POINT('Ctrl Pts',(16.7454193692319,-18.2258897639242,
21.3335535355786));
#181647=CARTESIAN_POINT('Ctrl Pts',(16.7201109656642,-18.2952012797656,
21.3291191852467));
#181648=CARTESIAN_POINT('Ctrl Pts',(16.6984027965461,-18.3659130286271,
21.3246848349147));
#181649=CARTESIAN_POINT('Ctrl Pts',(16.6804408864183,-18.4376227386191,
21.3202504845828));
#181650=CARTESIAN_POINT('Ctrl Pts',(16.6624933610866,-18.509275019889,21.3158196855004));
#181651=CARTESIAN_POINT('Ctrl Pts',(16.6482862472522,-18.581923225276,21.311388886418));
#181652=CARTESIAN_POINT('Ctrl Pts',(16.637915803284,-18.6551498016211,21.3069580873356));
#181653=CARTESIAN_POINT('Ctrl Pts',(16.6275504569996,-18.7283403827929,
21.3025294662518));
#181654=CARTESIAN_POINT('Ctrl Pts',(16.6210180978407,-18.8021083105054,
21.298100845168));
#181655=CARTESIAN_POINT('Ctrl Pts',(16.618363660142,-18.8760271267351,21.2936722240842));
#181656=CARTESIAN_POINT('Ctrl Pts',(16.6174414213416,-18.9017089502108,
21.2921335757303));
#181657=CARTESIAN_POINT('Ctrl Pts',(16.6169868263616,-18.9274089350833,
21.2905949273764));
#181658=CARTESIAN_POINT('Ctrl Pts',(16.6170002905213,-18.9531090839331,
21.2890562790225));
#181659=CARTESIAN_POINT('Origin',(18.734,19.211,0.));
#181660=CARTESIAN_POINT('',(16.7454193623258,19.9371102171621,0.755484062589681));
#181661=CARTESIAN_POINT('',(16.7454193623539,19.9371102172391,0.534177402122747));
#181662=CARTESIAN_POINT('',(16.7454193623258,19.9371102171621,0.));
#181663=CARTESIAN_POINT('',(16.6170002905282,19.2121090969791,0.710943721022754));
#181664=CARTESIAN_POINT('Ctrl Pts',(16.6170002905282,19.2121090969791,0.710943721022754));
#181665=CARTESIAN_POINT('Ctrl Pts',(16.6170426220575,19.2929098178344,0.715781198916212));
#181666=CARTESIAN_POINT('Ctrl Pts',(16.6217150381803,19.3735486726215,0.72061867680967));
#181667=CARTESIAN_POINT('Ctrl Pts',(16.6309374842428,19.4535222769504,0.725456154703128));
#181668=CARTESIAN_POINT('Ctrl Pts',(16.6404786393294,19.5362596067819,0.730460806017553));
#181669=CARTESIAN_POINT('Ctrl Pts',(16.6548898616796,19.6182845120318,0.735465457331979));
#181670=CARTESIAN_POINT('Ctrl Pts',(16.6740271613156,19.6990582996761,0.740470108646404));
#181671=CARTESIAN_POINT('Ctrl Pts',(16.6931644609517,19.7798320873204,0.74547475996083));
#181672=CARTESIAN_POINT('Ctrl Pts',(16.717027633524,19.8593544704023,0.750479411275255));
#181673=CARTESIAN_POINT('Ctrl Pts',(16.7454193623258,19.9371102171621,0.755484062589681));
#181674=CARTESIAN_POINT('',(17.1140596925741,20.5738948603531,2.19263333745477E-7));
#181675=CARTESIAN_POINT('Ctrl Pts',(17.1140596925741,20.5738948603531,2.19263333745477E-7));
#181676=CARTESIAN_POINT('Ctrl Pts',(17.1607064305025,20.6293392920392,0.00438522669745755));
#181677=CARTESIAN_POINT('Ctrl Pts',(17.2102945911146,20.6824950671961,0.00877023413158137));
#181678=CARTESIAN_POINT('Ctrl Pts',(17.2625707969829,20.7330332126824,0.0131552415657052));
#181679=CARTESIAN_POINT('Ctrl Pts',(17.3147693813982,20.7834963174457,0.017533737994626));
#181680=CARTESIAN_POINT('Ctrl Pts',(17.3696477435684,20.8313491749509,0.0219122344235468));
#181681=CARTESIAN_POINT('Ctrl Pts',(17.4269127458044,20.876296342973,0.0262907308524677));
#181682=CARTESIAN_POINT('Ctrl Pts',(17.4841103523032,20.9211906122366,0.0306640741864277));
#181683=CARTESIAN_POINT('Ctrl Pts',(17.5436886409258,20.9631856884277,0.0350374175203878));
#181684=CARTESIAN_POINT('Ctrl Pts',(17.605319441071,21.0020246218005,0.0394107608543478));
#181685=CARTESIAN_POINT('Ctrl Pts',(17.6669112432928,21.0408389791862,0.0437813368819024));
#181686=CARTESIAN_POINT('Ctrl Pts',(17.7305525723991,21.0765008992432,0.0481519129094571));
#181687=CARTESIAN_POINT('Ctrl Pts',(17.7958853222654,21.10879605106,0.0525224889370117));
#181688=CARTESIAN_POINT('Ctrl Pts',(17.8611983685245,21.1410814630298,0.0568917468490216));
#181689=CARTESIAN_POINT('Ctrl Pts',(17.9282013899053,21.1700019086929,0.0612610047610315));
#181690=CARTESIAN_POINT('Ctrl Pts',(17.9965121600447,21.1953892475817,0.0656302626730415));
#181691=CARTESIAN_POINT('Ctrl Pts',(18.0648249509204,21.2207773374667,0.069999649834336));
#181692=CARTESIAN_POINT('Ctrl Pts',(18.134445113711,21.242631946831,0.0743690369956306));
#181693=CARTESIAN_POINT('Ctrl Pts',(18.2049725448517,21.260833883928,0.0787384241569251));
#181694=CARTESIAN_POINT('Ctrl Pts',(18.275571771191,21.2790543501514,0.0831122592474014));
#181695=CARTESIAN_POINT('Ctrl Pts',(18.3470796408086,21.2936146004556,0.0874860943378777));
#181696=CARTESIAN_POINT('Ctrl Pts',(18.4190839151667,21.3044461682865,0.091859929428354));
#181697=CARTESIAN_POINT('Ctrl Pts',(18.4911280120912,21.3152837266066,0.0962361835049216));
#181698=CARTESIAN_POINT('Ctrl Pts',(18.5636685792402,21.322388450086,0.100612437581489));
#181699=CARTESIAN_POINT('Ctrl Pts',(18.6362889712808,21.3257438508875,0.104988691658057));
#181700=CARTESIAN_POINT('Ctrl Pts',(18.7090335036841,21.3291049875528,0.109372426688014));
#181701=CARTESIAN_POINT('Ctrl Pts',(18.7818576501797,21.3287040083353,0.113756161717971));
#181702=CARTESIAN_POINT('Ctrl Pts',(18.854346170805,21.3245765420662,0.118139896747928));
#181703=CARTESIAN_POINT('Ctrl Pts',(18.8963545400865,21.3221846029601,0.120680348096384));
#181704=CARTESIAN_POINT('Ctrl Pts',(18.9382502971219,21.318542128427,0.123220799444841));
#181705=CARTESIAN_POINT('Ctrl Pts',(18.9799541345816,21.3136639207639,0.125761250793297));
#181706=CARTESIAN_POINT('Ctrl Pts',(19.0521147654861,21.3052231017867,0.130157023059194));
#181707=CARTESIAN_POINT('Ctrl Pts',(19.1239757191856,21.2930474831033,0.134552795325092));
#181708=CARTESIAN_POINT('Ctrl Pts',(19.1951211491521,21.2771694717047,0.138948567590989));
#181709=CARTESIAN_POINT('Ctrl Pts',(19.2661637519632,21.2613144089446,0.143337986606115));
#181710=CARTESIAN_POINT('Ctrl Pts',(19.336492418998,21.2417676813877,0.14772740562124));
#181711=CARTESIAN_POINT('Ctrl Pts',(19.4056976665711,21.2186133205184,0.152116824636366));
#181712=CARTESIAN_POINT('Ctrl Pts',(19.4748248958988,21.1954850626206,0.156501295258381));
#181713=CARTESIAN_POINT('Ctrl Pts',(19.5428307683091,21.1687574028734,0.160885765880397));
#181714=CARTESIAN_POINT('Ctrl Pts',(19.60931884804,21.1385647626645,0.165270236502412));
#181715=CARTESIAN_POINT('Ctrl Pts',(19.6757666435217,21.1083904157775,0.169652050631602));
#181716=CARTESIAN_POINT('Ctrl Pts',(19.7406980347466,21.0747554526422,0.174033864760792));
#181717=CARTESIAN_POINT('Ctrl Pts',(19.8037358627713,21.0378426817602,0.178415678889982));
#181718=CARTESIAN_POINT('Ctrl Pts',(19.8667560838771,21.0009402208807,0.182796269146952));
#181719=CARTESIAN_POINT('Ctrl Pts',(19.9278833775877,20.9607620127547,0.187176859403921));
#181720=CARTESIAN_POINT('Ctrl Pts',(19.9867660017252,20.9175363590974,0.19155744966089));
#181721=CARTESIAN_POINT('Ctrl Pts',(20.0456514086938,20.8743086625676,0.195938246947401));
#181722=CARTESIAN_POINT('Ctrl Pts',(20.10229154935,20.828033520426,0.200319044233912));
#181723=CARTESIAN_POINT('Ctrl Pts',(20.1563657971913,20.7789810391011,0.204699841520423));
#181724=CARTESIAN_POINT('Ctrl Pts',(20.2104971638002,20.7298767435135,0.209085266254418));
#181725=CARTESIAN_POINT('Ctrl Pts',(20.2620568697779,20.6779895750515,0.213470690988413));
#181726=CARTESIAN_POINT('Ctrl Pts',(20.3107599897288,20.6236276702622,0.217856115722409));
#181727=CARTESIAN_POINT('Ctrl Pts',(20.3594903544992,20.569235355095,0.222243993689488));
#181728=CARTESIAN_POINT('Ctrl Pts',(20.405360649667,20.5123659213335,0.226631871656568));
#181729=CARTESIAN_POINT('Ctrl Pts',(20.4481269507233,20.4533597694727,0.231019749623648));
#181730=CARTESIAN_POINT('Ctrl Pts',(20.490968988079,20.3942491216074,0.2354153982333));
#181731=CARTESIAN_POINT('Ctrl Pts',(20.5306957923998,20.3329946025316,0.239811046842951));
#181732=CARTESIAN_POINT('Ctrl Pts',(20.5671076961723,20.2699641987498,0.244206695452603));
#181733=CARTESIAN_POINT('Ctrl Pts',(20.5912140439174,20.2282351850302,0.247116816126646));
#181734=CARTESIAN_POINT('Ctrl Pts',(20.613868403521,20.1857283140019,0.250026936800689));
#181735=CARTESIAN_POINT('Ctrl Pts',(20.6350244604073,20.1425551518472,0.252937057474731));
#181736=CARTESIAN_POINT('Ctrl Pts',(20.6668851126084,20.0775371236191,0.257319648387442));
#181737=CARTESIAN_POINT('Ctrl Pts',(20.6954700480251,20.010752620059,0.261702239300152));
#181738=CARTESIAN_POINT('Ctrl Pts',(20.720580205096,19.9425655054202,0.266084830212863));
#181739=CARTESIAN_POINT('Ctrl Pts',(20.745652583015,19.8744809807952,0.270460827356878));
#181740=CARTESIAN_POINT('Ctrl Pts',(20.7672603940222,19.8049984839899,0.274836824500893));
#181741=CARTESIAN_POINT('Ctrl Pts',(20.7852512551748,19.7345048119586,0.279212821644908));
#181742=CARTESIAN_POINT('Ctrl Pts',(20.8032205628375,19.6640955930636,0.283583576237746));
#181743=CARTESIAN_POINT('Ctrl Pts',(20.8175814089924,19.5926780716229,0.287954330830584));
#181744=CARTESIAN_POINT('Ctrl Pts',(20.8282307375361,19.5206556441581,0.292325085423422));
#181745=CARTESIAN_POINT('Ctrl Pts',(20.8388731698584,19.4486798564987,0.296693009632014));
#181746=CARTESIAN_POINT('Ctrl Pts',(20.845808782324,19.3761004173277,0.301060933840606));
#181747=CARTESIAN_POINT('Ctrl Pts',(20.8489855761766,19.3033309946067,0.305428858049198));
#181748=CARTESIAN_POINT('Ctrl Pts',(20.8521613682029,19.2305845202816,0.309795404799371));
#181749=CARTESIAN_POINT('Ctrl Pts',(20.8515806736046,19.1576486643711,0.314161951549544));
#181750=CARTESIAN_POINT('Ctrl Pts',(20.8472434850165,19.0849405971963,0.318528498299718));
#181751=CARTESIAN_POINT('Ctrl Pts',(20.842906223341,19.0122313047933,0.322895118632042));
#181752=CARTESIAN_POINT('Ctrl Pts',(20.8348123728149,18.9397502915731,0.327261738964367));
#181753=CARTESIAN_POINT('Ctrl Pts',(20.823013932432,18.8679113961305,0.331628359296692));
#181754=CARTESIAN_POINT('Ctrl Pts',(20.8112032798744,18.7959981426281,0.335999499372999));
#181755=CARTESIAN_POINT('Ctrl Pts',(20.7956804601328,18.7247288123435,0.340370639449306));
#181756=CARTESIAN_POINT('Ctrl Pts',(20.7765488036571,18.6545079653052,0.344741779525613));
#181757=CARTESIAN_POINT('Ctrl Pts',(20.7574067702789,18.5842490308755,0.349115290483644));
#181758=CARTESIAN_POINT('Ctrl Pts',(20.7346521545123,18.5150401717767,0.353488801441674));
#181759=CARTESIAN_POINT('Ctrl Pts',(20.7084376488589,18.4472690455608,0.357862312399705));
#181760=CARTESIAN_POINT('Ctrl Pts',(20.6821764073163,18.3793770952528,0.362243620564604));
#181761=CARTESIAN_POINT('Ctrl Pts',(20.6524431558452,18.3129284384101,0.366624928729503));
#181762=CARTESIAN_POINT('Ctrl Pts',(20.6194377827199,18.2482885336239,0.371006236894402));
#181763=CARTESIAN_POINT('Ctrl Pts',(20.5965703635706,18.2035034681465,0.37404177931499));
#181764=CARTESIAN_POINT('Ctrl Pts',(20.572133215651,18.1595861430692,0.377077321735578));
#181765=CARTESIAN_POINT('Ctrl Pts',(20.54620485702,18.1166497104705,0.380112864156166));
#181766=CARTESIAN_POINT('Ctrl Pts',(20.5087129403854,18.0545644402657,0.384502201136291));
#181767=CARTESIAN_POINT('Ctrl Pts',(20.4679538797132,17.9942872987423,0.388891538116417));
#181768=CARTESIAN_POINT('Ctrl Pts',(20.4241274618398,17.9361830865827,0.393280875096542));
#181769=CARTESIAN_POINT('Ctrl Pts',(20.3803660305828,17.8781650324147,0.397663703487275));
#181770=CARTESIAN_POINT('Ctrl Pts',(20.3335465592593,17.8223138929919,0.402046531878009));
#181771=CARTESIAN_POINT('Ctrl Pts',(20.2839133009207,17.7689674900928,0.406429360268742));
#181772=CARTESIAN_POINT('Ctrl Pts',(20.2343383423802,17.7156837484944,0.410807040538659));
#181773=CARTESIAN_POINT('Ctrl Pts',(20.1819564893205,17.6648992500389,0.415184720808577));
#181774=CARTESIAN_POINT('Ctrl Pts',(20.127052568789,17.6169192176711,0.419562401078494));
#181775=CARTESIAN_POINT('Ctrl Pts',(20.0721834605649,17.5689696074593,0.423937305642237));
#181776=CARTESIAN_POINT('Ctrl Pts',(20.0147958199512,17.5238212515477,0.42831221020598));
#181777=CARTESIAN_POINT('Ctrl Pts',(19.9552106611292,17.4817419159812,0.432687114769722));
#181778=CARTESIAN_POINT('Ctrl Pts',(19.8956436547537,17.4396753997627,0.437060686531428));
#181779=CARTESIAN_POINT('Ctrl Pts',(19.8338808528526,17.4006763255857,0.441434258293133));
#181780=CARTESIAN_POINT('Ctrl Pts',(19.7702742782372,17.3649705797946,0.445807830054838));
#181781=CARTESIAN_POINT('Ctrl Pts',(19.7066661290221,17.3292639500971,0.450181510085618));
#181782=CARTESIAN_POINT('Ctrl Pts',(19.6412145378354,17.2968510448943,0.454555190116397));
#181783=CARTESIAN_POINT('Ctrl Pts',(19.5742968108293,17.2679121816783,0.458928870147177));
#181784=CARTESIAN_POINT('Ctrl Pts',(19.5073098565464,17.2389433808242,0.463307074807999));
#181785=CARTESIAN_POINT('Ctrl Pts',(19.438854181596,17.2134559893026,0.46768527946882));
#181786=CARTESIAN_POINT('Ctrl Pts',(19.3693270226857,17.191582119955,0.472063484129642));
#181787=CARTESIAN_POINT('Ctrl Pts',(19.2997619936055,17.1696963363115,0.476444073518355));
#181788=CARTESIAN_POINT('Ctrl Pts',(19.2291247856184,17.1514281144628,0.480824662907068));
#181789=CARTESIAN_POINT('Ctrl Pts',(19.1578251136209,17.1368589071463,0.485205252295781));
#181790=CARTESIAN_POINT('Ctrl Pts',(19.0863994489355,17.1222639547802,0.489593582564874));
#181791=CARTESIAN_POINT('Ctrl Pts',(19.0143094596386,17.1113811421464,0.493981912833966));
#181792=CARTESIAN_POINT('Ctrl Pts',(18.9419717193456,17.1042402215838,0.498370243103058));
#181793=CARTESIAN_POINT('Ctrl Pts',(18.8929675902332,17.0994027108761,0.501343052347906));
#181794=CARTESIAN_POINT('Ctrl Pts',(18.8438498553954,17.0962813345305,0.504315861592753));
#181795=CARTESIAN_POINT('Ctrl Pts',(18.7947475345845,17.0948717578932,0.5072886708376));
#181796=CARTESIAN_POINT('Ctrl Pts',(18.7222522737112,17.0927906418817,0.511677762395247));
#181797=CARTESIAN_POINT('Ctrl Pts',(18.6495091103978,17.0944351532161,0.516066853952895));
#181798=CARTESIAN_POINT('Ctrl Pts',(18.5769329023863,17.0998346993077,0.520455945510542));
#181799=CARTESIAN_POINT('Ctrl Pts',(18.5044640605617,17.1052262575382,0.524838544030911));
#181800=CARTESIAN_POINT('Ctrl Pts',(18.4321621606072,17.1143617873598,0.52922114255128));
#181801=CARTESIAN_POINT('Ctrl Pts',(18.3604434342997,17.1272187033611,0.533603741071649));
#181802=CARTESIAN_POINT('Ctrl Pts',(18.2888085527942,17.1400605886216,0.537981215991468));
#181803=CARTESIAN_POINT('Ctrl Pts',(18.2177559628243,17.1566151328627,0.542358690911286));
#181804=CARTESIAN_POINT('Ctrl Pts',(18.1476964397083,17.1768079895965,0.546736165831104));
#181805=CARTESIAN_POINT('Ctrl Pts',(18.0776810968814,17.1969881124977,0.551110880268136));
#181806=CARTESIAN_POINT('Ctrl Pts',(18.0086580405141,17.2208018623067,0.555485594705167));
#181807=CARTESIAN_POINT('Ctrl Pts',(17.9410261268035,17.2481241923067,0.559860309142198));
#181808=CARTESIAN_POINT('Ctrl Pts',(17.8734145775146,17.2754382953703,0.564233706323447));
#181809=CARTESIAN_POINT('Ctrl Pts',(17.8071937860416,17.3062587006989,0.568607103504695));
#181810=CARTESIAN_POINT('Ctrl Pts',(17.742744167297,17.340411623544,0.572980500685944));
#181811=CARTESIAN_POINT('Ctrl Pts',(17.6782927189291,17.3745655159369,0.577354022021053));
#181812=CARTESIAN_POINT('Ctrl Pts',(17.6156129682129,17.4120518861517,0.581727543356163));
#181813=CARTESIAN_POINT('Ctrl Pts',(17.5550606878344,17.4526510305885,0.586101064691273));
#181814=CARTESIAN_POINT('Ctrl Pts',(17.4944454063011,17.4932924160932,0.590479136423054));
#181815=CARTESIAN_POINT('Ctrl Pts',(17.435962415829,17.5370527729163,0.594857208154836));
#181816=CARTESIAN_POINT('Ctrl Pts',(17.3799377355334,17.5836695529341,0.599235279886618));
#181817=CARTESIAN_POINT('Ctrl Pts',(17.3238823567117,17.6303118764522,0.603615750567371));
#181818=CARTESIAN_POINT('Ctrl Pts',(17.2702883244171,17.6798134120468,0.607996221248125));
#181819=CARTESIAN_POINT('Ctrl Pts',(17.2194458037231,17.7318737083873,0.612376691928879));
#181820=CARTESIAN_POINT('Ctrl Pts',(17.1685131538602,17.7840262926627,0.616764927924508));
#181821=CARTESIAN_POINT('Ctrl Pts',(17.1203420749117,17.8387463335722,0.621153163920138));
#181822=CARTESIAN_POINT('Ctrl Pts',(17.0751829640465,17.895699638398,0.625541399915768));
#181823=CARTESIAN_POINT('Ctrl Pts',(17.0445739865328,17.9343027550967,0.628515759116856));
#181824=CARTESIAN_POINT('Ctrl Pts',(17.0153478916349,17.9739312043245,0.631490118317945));
#181825=CARTESIAN_POINT('Ctrl Pts',(16.9875709408017,18.0144739696991,0.634464477519034));
#181826=CARTESIAN_POINT('Ctrl Pts',(16.9460128011877,18.0751315240105,0.638914528054931));
#181827=CARTESIAN_POINT('Ctrl Pts',(16.907540976001,18.1380696073307,0.643364578590828));
#181828=CARTESIAN_POINT('Ctrl Pts',(16.8724100479184,18.2029465042425,0.647814629126725));
#181829=CARTESIAN_POINT('Ctrl Pts',(16.8373354125813,18.2677194443605,0.652257549035117));
#181830=CARTESIAN_POINT('Ctrl Pts',(16.8055912619724,18.3344246233501,0.656700468943509));
#181831=CARTESIAN_POINT('Ctrl Pts',(16.7773892640252,18.4026910071835,0.6611433888519));
#181832=CARTESIAN_POINT('Ctrl Pts',(16.7492305714797,18.4708525649974,0.665579486462369));
#181833=CARTESIAN_POINT('Ctrl Pts',(16.7246033918711,18.5405701336241,0.670015584072838));
#181834=CARTESIAN_POINT('Ctrl Pts',(16.7036729534574,18.6114492648012,0.674451681683307));
#181835=CARTESIAN_POINT('Ctrl Pts',(16.6827615040683,18.6822640912779,0.67888375466872));
#181836=CARTESIAN_POINT('Ctrl Pts',(16.6655402658946,18.7542379435046,0.683315827654133));
#181837=CARTESIAN_POINT('Ctrl Pts',(16.6521255559742,18.8269585968775,0.687747900639545));
#181838=CARTESIAN_POINT('Ctrl Pts',(16.6387183882743,18.8996383641481,0.69217748175805));
#181839=CARTESIAN_POINT('Ctrl Pts',(16.6291135834743,18.9730636427319,0.696607062876554));
#181840=CARTESIAN_POINT('Ctrl Pts',(16.6233766644396,19.0468106721261,0.701036643995058));
#181841=CARTESIAN_POINT('Ctrl Pts',(16.6190996536644,19.1017908518083,0.704339002989208));
#181842=CARTESIAN_POINT('Ctrl Pts',(16.6169713924502,19.1569495703029,0.707641361983357));
#181843=CARTESIAN_POINT('Ctrl Pts',(16.6170002905278,19.2121090962233,0.710943720977507));
#181844=CARTESIAN_POINT('',(20.3539256943887,20.5739122292573,0.));
#181845=CARTESIAN_POINT('Origin',(18.734,19.211,0.));
#181846=CARTESIAN_POINT('',(16.617000615792,19.2126147021618,0.489056278967189));
#181847=CARTESIAN_POINT('Ctrl Pts',(16.617000615792,19.2126147021618,0.489056278967189));
#181848=CARTESIAN_POINT('Ctrl Pts',(16.6169439872409,19.1383702930775,0.484575909845402));
#181849=CARTESIAN_POINT('Ctrl Pts',(16.620797922571,19.0639813997485,0.480095540723615));
#181850=CARTESIAN_POINT('Ctrl Pts',(16.6285774658501,18.9899005818784,0.475615171601828));
#181851=CARTESIAN_POINT('Ctrl Pts',(16.6360763305565,18.9184925299366,0.471296449965575));
#181852=CARTESIAN_POINT('Ctrl Pts',(16.6472223423582,18.847371251054,0.466977728329323));
#181853=CARTESIAN_POINT('Ctrl Pts',(16.6619760571586,18.7769426532218,0.46265900669307));
#181854=CARTESIAN_POINT('Ctrl Pts',(16.6767199431811,18.7065609742206,0.458343162146202));
#181855=CARTESIAN_POINT('Ctrl Pts',(16.6950666659526,18.6368715461706,0.454027317599334));
#181856=CARTESIAN_POINT('Ctrl Pts',(16.7169252821381,18.568272544104,0.449711473052466));
#181857=CARTESIAN_POINT('Ctrl Pts',(16.7387770072278,18.4996951683974,0.445396989108594));
#181858=CARTESIAN_POINT('Ctrl Pts',(16.7641382782578,18.4322080094981,0.441082505164722));
#181859=CARTESIAN_POINT('Ctrl Pts',(16.7928681313892,18.3661946563476,0.43676802122085));
#181860=CARTESIAN_POINT('Ctrl Pts',(16.8215990088179,18.300178949642,0.432453383453916));
#181861=CARTESIAN_POINT('Ctrl Pts',(16.8536985054739,18.235637607015,0.428138745686983));
#181862=CARTESIAN_POINT('Ctrl Pts',(16.8889780484646,18.1729330472689,0.423824107920049));
#181863=CARTESIAN_POINT('Ctrl Pts',(16.9242924797719,18.1101664783144,0.419505203361778));
#181864=CARTESIAN_POINT('Ctrl Pts',(16.9627929858512,18.0492407485845,0.415186298803507));
#181865=CARTESIAN_POINT('Ctrl Pts',(17.0042462481892,17.9904915165816,0.410867394245236));
#181866=CARTESIAN_POINT('Ctrl Pts',(17.0457241655954,17.9317073424234,0.406545920941331));
#181867=CARTESIAN_POINT('Ctrl Pts',(17.0901580238556,17.8751026293948,0.402224447637425));
#181868=CARTESIAN_POINT('Ctrl Pts',(17.1372743354942,17.8209798014746,0.39790297433352));
#181869=CARTESIAN_POINT('Ctrl Pts',(17.1844652352621,17.7667712936627,0.393574659861494));
#181870=CARTESIAN_POINT('Ctrl Pts',(17.2343467107437,17.7150528602031,0.389246345389468));
#181871=CARTESIAN_POINT('Ctrl Pts',(17.2866094106097,17.6660891670571,0.384918030917442));
#181872=CARTESIAN_POINT('Ctrl Pts',(17.3002561761556,17.6533038336867,0.383787827293062));
#181873=CARTESIAN_POINT('Ctrl Pts',(17.314065135147,17.64070610536,0.382657623668683));
#181874=CARTESIAN_POINT('Ctrl Pts',(17.3280304443276,17.6283002152896,0.381527420044303));
#181875=CARTESIAN_POINT('Ctrl Pts',(17.3823195172276,17.5800732650869,0.377133839768919));
#181876=CARTESIAN_POINT('Ctrl Pts',(17.4391958858,17.5345513015008,0.372740259493535));
#181877=CARTESIAN_POINT('Ctrl Pts',(17.4983592346194,17.4920232988985,0.368346679218151));
#181878=CARTESIAN_POINT('Ctrl Pts',(17.5574362854365,17.4495573293242,0.363959507592861));
#181879=CARTESIAN_POINT('Ctrl Pts',(17.6187933062775,17.4100769290324,0.359572335967571));
#181880=CARTESIAN_POINT('Ctrl Pts',(17.6820956267705,17.3738320192261,0.35518516434228));
#181881=CARTESIAN_POINT('Ctrl Pts',(17.7453254808101,17.3376286014228,0.350803015009472));
#181882=CARTESIAN_POINT('Ctrl Pts',(17.8104957951169,17.304653553715,0.346420865676663));
#181883=CARTESIAN_POINT('Ctrl Pts',(17.877242918952,17.2751135611627,0.342038716343855));
#181884=CARTESIAN_POINT('Ctrl Pts',(17.9439489018954,17.245591776161,0.337659268034266));
#181885=CARTESIAN_POINT('Ctrl Pts',(18.0122293270667,17.2195010391259,0.333279819724678));
#181886=CARTESIAN_POINT('Ctrl Pts',(18.0816971982504,17.1970014759614,0.328900371415089));
#181887=CARTESIAN_POINT('Ctrl Pts',(18.151144994395,17.1745084147899,0.324522188691947));
#181888=CARTESIAN_POINT('Ctrl Pts',(18.2217790979678,17.155604615017,0.320144005968805));
#181889=CARTESIAN_POINT('Ctrl Pts',(18.2931954157568,17.1404009759226,0.315765823245664));
#181890=CARTESIAN_POINT('Ctrl Pts',(18.3646144753839,17.1251967531253,0.311387472433939));
#181891=CARTESIAN_POINT('Ctrl Pts',(18.4368153380914,17.113693071257,0.307009121622214));
#181892=CARTESIAN_POINT('Ctrl Pts',(18.5093833633923,17.1059497947652,0.302630770810489));
#181893=CARTESIAN_POINT('Ctrl Pts',(18.5820273386456,17.0981984141328,0.298247837601298));
#181894=CARTESIAN_POINT('Ctrl Pts',(18.6550387645183,17.09421534768,0.293864904392108));
#181895=CARTESIAN_POINT('Ctrl Pts',(18.7279983301932,17.0940085073483,0.289481971182917));
#181896=CARTESIAN_POINT('Ctrl Pts',(18.8009982495664,17.093801552614,0.285096613787635));
#181897=CARTESIAN_POINT('Ctrl Pts',(18.8739457709895,17.0973749591399,0.280711256392353));
#181898=CARTESIAN_POINT('Ctrl Pts',(18.9464247464519,17.1046845613501,0.276325898997071));
#181899=CARTESIAN_POINT('Ctrl Pts',(19.0190318084557,17.1120070812604,0.271932791695594));
#181900=CARTESIAN_POINT('Ctrl Pts',(19.0911681952095,17.1230789093043,0.267539684394118));
#181901=CARTESIAN_POINT('Ctrl Pts',(19.1624265854904,17.1378044807966,0.263146577092641));
#181902=CARTESIAN_POINT('Ctrl Pts',(19.209979484077,17.1476313040667,0.26021492251605));
#181903=CARTESIAN_POINT('Ctrl Pts',(19.2571416240955,17.1590841897826,0.25728326793946));
#181904=CARTESIAN_POINT('Ctrl Pts',(19.3037962299318,17.1721225499419,0.254351613362869));
#181905=CARTESIAN_POINT('Ctrl Pts',(19.3728933426701,17.1914328200792,0.250009729787665));
#181906=CARTESIAN_POINT('Ctrl Pts',(19.441158849408,17.2143020129624,0.245667846212462));
#181907=CARTESIAN_POINT('Ctrl Pts',(19.5081940657064,17.2406415177372,0.241325962637258));
#181908=CARTESIAN_POINT('Ctrl Pts',(19.575128336692,17.2669413590381,0.236990617308954));
#181909=CARTESIAN_POINT('Ctrl Pts',(19.6408355376982,17.2967009666761,0.232655271980649));
#181910=CARTESIAN_POINT('Ctrl Pts',(19.7049304637962,17.3297815027296,0.228319926652345));
#181911=CARTESIAN_POINT('Ctrl Pts',(19.7689517228447,17.3628240179031,0.223989564122503));
#181912=CARTESIAN_POINT('Ctrl Pts',(19.8313639491299,17.3991796603212,0.219659201592662));
#181913=CARTESIAN_POINT('Ctrl Pts',(19.8918020078126,17.4386615699294,0.21532883906282));
#181914=CARTESIAN_POINT('Ctrl Pts',(19.9522029223966,17.4781192146956,0.211001137892668));
#181915=CARTESIAN_POINT('Ctrl Pts',(20.0106316627094,17.5206990484192,0.206673436722516));
#181916=CARTESIAN_POINT('Ctrl Pts',(20.0667492121328,17.5661691462161,0.202345735552364));
#181917=CARTESIAN_POINT('Ctrl Pts',(20.1228517146943,17.6116270520643,0.198019194773624));
#181918=CARTESIAN_POINT('Ctrl Pts',(20.1766438725233,17.6599733741804,0.193692653994883));
#181919=CARTESIAN_POINT('Ctrl Pts',(20.2278185824314,17.710934987148,0.189366113216143));
#181920=CARTESIAN_POINT('Ctrl Pts',(20.2789973003963,17.7619005914824,0.185039233578198));
#181921=CARTESIAN_POINT('Ctrl Pts',(20.3275578154845,17.8154815434691,0.180712353940253));
#181922=CARTESIAN_POINT('Ctrl Pts',(20.3732301490776,17.8713681407361,0.176385474302308));
#181923=CARTESIAN_POINT('Ctrl Pts',(20.4189572946786,17.9273218082918,0.172053401915454));
#181924=CARTESIAN_POINT('Ctrl Pts',(20.4617890269818,17.9855862615223,0.167721329528601));
#181925=CARTESIAN_POINT('Ctrl Pts',(20.5014965046459,18.0458197109183,0.163389257141747));
#181926=CARTESIAN_POINT('Ctrl Pts',(20.5412284893311,18.1060903357408,0.159054511047183));
#181927=CARTESIAN_POINT('Ctrl Pts',(20.5778321351825,18.1683319477764,0.154719764952619));
#181928=CARTESIAN_POINT('Ctrl Pts',(20.6111242325247,18.2321774340216,0.150385018858055));
#181929=CARTESIAN_POINT('Ctrl Pts',(20.6444833803135,18.2961515053878,0.146041542563685));
#181930=CARTESIAN_POINT('Ctrl Pts',(20.6745174591996,18.3617354510943,0.141698066269316));
#181931=CARTESIAN_POINT('Ctrl Pts',(20.7010913635959,18.4285419709235,0.137354589974947));
#181932=CARTESIAN_POINT('Ctrl Pts',(20.7218496990689,18.480728210842,0.133961662210443));
#181933=CARTESIAN_POINT('Ctrl Pts',(20.7404975995388,18.5336600360754,0.130568734445939));
#181934=CARTESIAN_POINT('Ctrl Pts',(20.7569922795081,18.5871480648016,0.127175806681435));
#181935=CARTESIAN_POINT('Ctrl Pts',(20.7789195363731,18.6582525510522,0.12266540704014));
#181936=CARTESIAN_POINT('Ctrl Pts',(20.7971288498248,18.7306277670711,0.118155007398845));
#181937=CARTESIAN_POINT('Ctrl Pts',(20.8114809457081,18.8038613010046,0.113644607757551));
#181938=CARTESIAN_POINT('Ctrl Pts',(20.8265483310552,18.8807446973446,0.108909415767653));
#181939=CARTESIAN_POINT('Ctrl Pts',(20.8373637791173,18.9585737514705,0.104174223777755));
#181940=CARTESIAN_POINT('Ctrl Pts',(20.8438249692462,19.0368517897157,0.0994390317878569));
#181941=CARTESIAN_POINT('Ctrl Pts',(20.8499589678183,19.1111658657987,0.0949436276401115));
#181942=CARTESIAN_POINT('Ctrl Pts',(20.8521688918293,19.1858840436361,0.0904482234923663));
#181943=CARTESIAN_POINT('Ctrl Pts',(20.8504195410052,19.2605714277716,0.0859528193446209));
#181944=CARTESIAN_POINT('Ctrl Pts',(20.8486718350827,19.3351885839162,0.0814616421919066));
#181945=CARTESIAN_POINT('Ctrl Pts',(20.8429722647592,19.4097745558195,0.0769704650391922));
#181946=CARTESIAN_POINT('Ctrl Pts',(20.8333376405566,19.4838927828696,0.0724792878864778));
#181947=CARTESIAN_POINT('Ctrl Pts',(20.8237095586262,19.5579606808563,0.0679911604119481));
#181948=CARTESIAN_POINT('Ctrl Pts',(20.8101517936905,19.6315610202815,0.0635030329374184));
#181949=CARTESIAN_POINT('Ctrl Pts',(20.7927330149949,19.7042619719479,0.0590149054628886));
#181950=CARTESIAN_POINT('Ctrl Pts',(20.7753215178591,19.7769325324869,0.0545286541571083));
#181951=CARTESIAN_POINT('Ctrl Pts',(20.7540523227982,19.8487040161605,0.0500424028513279));
#181952=CARTESIAN_POINT('Ctrl Pts',(20.7290450048267,19.919155652887,0.0455561515455476));
#181953=CARTESIAN_POINT('Ctrl Pts',(20.704034580516,19.9896160409194,0.0410693429701386));
#181954=CARTESIAN_POINT('Ctrl Pts',(20.6752852491506,20.0587558278079,0.0365825343947297));
#181955=CARTESIAN_POINT('Ctrl Pts',(20.642965902348,20.1261711226173,0.0320957258193207));
#181956=CARTESIAN_POINT('Ctrl Pts',(20.6106450021441,20.1935896576844,0.0276087015893536));
#181957=CARTESIAN_POINT('Ctrl Pts',(20.5747539463686,20.2592831330904,0.0231216773593865));
#181958=CARTESIAN_POINT('Ctrl Pts',(20.5355083127276,20.3228708554384,0.0186346531294194));
#181959=CARTESIAN_POINT('Ctrl Pts',(20.4962355967949,20.3865024578589,0.0141445325320924));
#181960=CARTESIAN_POINT('Ctrl Pts',(20.4536039241545,20.448025026832,0.00965441193476544));
#181961=CARTESIAN_POINT('Ctrl Pts',(20.4078726283013,20.5070861947508,0.00516429133743847));
#181962=CARTESIAN_POINT('Ctrl Pts',(20.390340082504,20.5297291706837,0.00344286089162564));
#181963=CARTESIAN_POINT('Ctrl Pts',(20.3723523809939,20.5520106992443,0.00172143044581282));
#181964=CARTESIAN_POINT('Ctrl Pts',(20.3539256943887,20.5739122292573,0.));
#181965=CARTESIAN_POINT('Ctrl Pts',(16.617000568856,19.2125519458626,0.490010468414518));
#181966=CARTESIAN_POINT('Ctrl Pts',(16.6170514727118,19.2819895701466,0.494577329568179));
#181967=CARTESIAN_POINT('Ctrl Pts',(16.620518701297,19.351389617805,0.499098993300903));
#181968=CARTESIAN_POINT('Ctrl Pts',(16.6297024930679,19.4437365273411,0.504962251941776));
#181969=CARTESIAN_POINT('Ctrl Pts',(16.6323977852857,19.4669346043809,0.506421959053868));
#181970=CARTESIAN_POINT('Ctrl Pts',(16.6362852638933,19.4961657824342,0.50824070320294));
#181971=CARTESIAN_POINT('Ctrl Pts',(16.6371204772031,19.5022437235427,0.508617740340019));
#181972=CARTESIAN_POINT('Ctrl Pts',(16.6385603510653,19.5123944747752,0.509245445913265));
#181973=CARTESIAN_POINT('Ctrl Pts',(16.6391504869417,19.5164692620273,0.509496889213504));
#181974=CARTESIAN_POINT('Ctrl Pts',(16.6402462304663,19.5238826521267,0.509953342278766));
#181975=CARTESIAN_POINT('Ctrl Pts',(16.6407479434933,19.5272218046519,0.510158566898216));
#181976=CARTESIAN_POINT('Ctrl Pts',(16.6417945776025,19.5340760326796,0.510579044653468));
#181977=CARTESIAN_POINT('Ctrl Pts',(16.642340366501,19.5375909222486,0.51079424148904));
#181978=CARTESIAN_POINT('Ctrl Pts',(16.6435932942979,19.5455278134933,0.51127920871026));
#181979=CARTESIAN_POINT('Ctrl Pts',(16.6443056041383,19.5499489430603,0.511548681784669));
#181980=CARTESIAN_POINT('Ctrl Pts',(16.6465009500227,19.5633049044377,0.512360805496415));
#181981=CARTESIAN_POINT('Ctrl Pts',(16.6480273223423,19.5722326453654,0.512901042489817));
#181982=CARTESIAN_POINT('Ctrl Pts',(16.6601811269454,19.6406730694997,0.517024267613215));
#181983=CARTESIAN_POINT('Ctrl Pts',(16.6732971358806,19.6997216069459,0.52047584790657));
#181984=CARTESIAN_POINT('Ctrl Pts',(16.6938141846331,19.7764103007183,0.52491372259378));
#181985=CARTESIAN_POINT('Ctrl Pts',(16.6989489234585,19.7946215484647,0.525964177555541));
#181986=CARTESIAN_POINT('Ctrl Pts',(16.7159637149531,19.8520104643281,0.52927037703059));
#181987=CARTESIAN_POINT('Ctrl Pts',(16.7287365187921,19.8909142528046,0.531505687114406));
#181988=CARTESIAN_POINT('Ctrl Pts',(16.7435546041396,19.9319879022533,0.533880981460195));
#181989=CARTESIAN_POINT('Ctrl Pts',(16.7444845157121,19.9345499751618,0.534029210069973));
#181990=CARTESIAN_POINT('Ctrl Pts',(16.7454193623539,19.9371102172391,0.534177402122746));
#181991=CARTESIAN_POINT('Origin',(18.734,19.211,0.));
#181992=CARTESIAN_POINT('',(16.7454191763733,19.9371097078984,1.5557606494604));
#181993=CARTESIAN_POINT('',(16.7454193623274,19.9371102171666,1.33163196712539));
#181994=CARTESIAN_POINT('',(16.7454193623258,19.9371102171621,0.));
#181995=CARTESIAN_POINT('',(16.6170003908423,19.2122864004549,1.51094372094299));
#181996=CARTESIAN_POINT('Ctrl Pts',(16.7454191763733,19.9371097078984,1.5557606494604));
#181997=CARTESIAN_POINT('Ctrl Pts',(16.716143910019,19.8569341743039,1.55013146713003));
#181998=CARTESIAN_POINT('Ctrl Pts',(16.691724399299,19.7750071540623,1.54446139084034));
#181999=CARTESIAN_POINT('Ctrl Pts',(16.6660226724897,19.6647911110356,1.53708122705044));
#182000=CARTESIAN_POINT('Ctrl Pts',(16.6602607680098,19.6376875904994,1.53528609642957));
#182001=CARTESIAN_POINT('Ctrl Pts',(16.6468711285243,19.5680050736347,1.53073309112472));
#182002=CARTESIAN_POINT('Ctrl Pts',(16.6400127040676,19.5252886290076,1.52800093208224));
#182003=CARTESIAN_POINT('Ctrl Pts',(16.6335056814302,19.4749486682767,1.52487273165061));
#182004=CARTESIAN_POINT('Ctrl Pts',(16.6325834864648,19.4675032598284,1.52441240419798));
#182005=CARTESIAN_POINT('Ctrl Pts',(16.631157199937,19.4554637294837,1.52367198912816));
#182006=CARTESIAN_POINT('Ctrl Pts',(16.6306285480662,19.4508726598322,1.52339057211655));
#182007=CARTESIAN_POINT('Ctrl Pts',(16.6297175152803,19.4427261555249,1.52289290836678));
#182008=CARTESIAN_POINT('Ctrl Pts',(16.6293291048428,19.4391714495985,1.5226763260859));
#182009=CARTESIAN_POINT('Ctrl Pts',(16.6285936539188,19.4322789607038,1.52225749574951));
#182010=CARTESIAN_POINT('Ctrl Pts',(16.6282455446969,19.4289413565642,1.52205518625118));
#182011=CARTESIAN_POINT('Ctrl Pts',(16.6274962873484,19.4215882090119,1.52161055603733));
#182012=CARTESIAN_POINT('Ctrl Pts',(16.6270986810427,19.4175723068912,1.52136843279376));
#182013=CARTESIAN_POINT('Ctrl Pts',(16.6261439820916,19.4076400782142,1.52077130950579));
#182014=CARTESIAN_POINT('Ctrl Pts',(16.6256003084409,19.4017224556519,1.52041703549923));
#182015=CARTESIAN_POINT('Ctrl Pts',(16.6234160970895,19.3767968052736,1.51893078240055));
#182016=CARTESIAN_POINT('Ctrl Pts',(16.622007576511,19.3577686962519,1.51781083250504));
#182017=CARTESIAN_POINT('Ctrl Pts',(16.618313690624,19.2966545307416,1.51425336271375));
#182018=CARTESIAN_POINT('Ctrl Pts',(16.6170276587975,19.2545168990468,1.51186055981017));
#182019=CARTESIAN_POINT('Ctrl Pts',(16.6170004413594,19.2123670096225,1.50950271487047));
#182020=CARTESIAN_POINT('Ctrl Pts',(16.7454193623258,19.9371102171621,0.755484062589681));
#182021=CARTESIAN_POINT('Ctrl Pts',(16.7570609175801,19.9689926653415,0.757536136459943));
#182022=CARTESIAN_POINT('Ctrl Pts',(16.7694632428329,20.0005783913288,0.759588210330205));
#182023=CARTESIAN_POINT('Ctrl Pts',(16.7826102683356,20.0318331835122,0.761640284200467));
#182024=CARTESIAN_POINT('Ctrl Pts',(16.8107255683611,20.0986724742163,0.766028704419563));
#182025=CARTESIAN_POINT('Ctrl Pts',(16.8423337653793,20.1641959540946,0.770417124638659));
#182026=CARTESIAN_POINT('Ctrl Pts',(16.8772900666095,20.2280138756423,0.774805544857755));
#182027=CARTESIAN_POINT('Ctrl Pts',(16.9121945017389,20.291737107917,0.779187453797423));
#182028=CARTESIAN_POINT('Ctrl Pts',(16.950436949649,20.3537593859495,0.78356936273709));
#182029=CARTESIAN_POINT('Ctrl Pts',(16.9918247124447,20.4137112153097,0.787951271676757));
#182030=CARTESIAN_POINT('Ctrl Pts',(17.0331638556813,20.4735926172943,0.792328033044615));
#182031=CARTESIAN_POINT('Ctrl Pts',(17.0776407011702,20.5314080072912,0.796704794412473));
#182032=CARTESIAN_POINT('Ctrl Pts',(17.1250176841708,20.5868142706589,0.801081555780331));
#182033=CARTESIAN_POINT('Ctrl Pts',(17.1723646300877,20.6421854063664,0.805455542274424));
#182034=CARTESIAN_POINT('Ctrl Pts',(17.2226077526131,20.6951500803167,0.809829528768517));
#182035=CARTESIAN_POINT('Ctrl Pts',(17.2754682593319,20.7453970025596,0.81420351526261));
#182036=CARTESIAN_POINT('Ctrl Pts',(17.3283126854692,20.7956286392937,0.818576171155629));
#182037=CARTESIAN_POINT('Ctrl Pts',(17.3837725656567,20.8431438335996,0.822948827048648));
#182038=CARTESIAN_POINT('Ctrl Pts',(17.4415323658093,20.8876682482141,0.827321482941666));
#182039=CARTESIAN_POINT('Ctrl Pts',(17.4992936432934,20.9321938016366,0.831694250674801));
#182040=CARTESIAN_POINT('Ctrl Pts',(17.5593545743128,20.9737281306084,0.836067018407934));
#182041=CARTESIAN_POINT('Ctrl Pts',(17.6213680169052,21.0120383311286,0.840439786141068));
#182042=CARTESIAN_POINT('Ctrl Pts',(17.6834457957083,21.0503882767916,0.844817090427792));
#182043=CARTESIAN_POINT('Ctrl Pts',(17.7474797192073,21.0855071616625,0.849194394714516));
#182044=CARTESIAN_POINT('Ctrl Pts',(17.8130959539107,21.1172068979773,0.853571699001239));
#182045=CARTESIAN_POINT('Ctrl Pts',(17.8787480151553,21.1489239423855,0.857951393301242));
#182046=CARTESIAN_POINT('Ctrl Pts',(17.945983662843,21.1772179341103,0.862331087601244));
#182047=CARTESIAN_POINT('Ctrl Pts',(18.0144093958347,21.2019491109511,0.866710781901247));
#182048=CARTESIAN_POINT('Ctrl Pts',(18.0829563577891,21.2267241036896,0.87109823564749));
#182049=CARTESIAN_POINT('Ctrl Pts',(18.1526971536752,21.2479235359394,0.875485689393733));
#182050=CARTESIAN_POINT('Ctrl Pts',(18.2232240248379,21.2654578124647,0.879873143139976));
#182051=CARTESIAN_POINT('Ctrl Pts',(18.2711423361325,21.2773711854389,0.882854125720618));
#182052=CARTESIAN_POINT('Ctrl Pts',(18.3194232738606,21.2875936785606,0.885835108301261));
#182053=CARTESIAN_POINT('Ctrl Pts',(18.3679374539171,21.2961108393453,0.888816090881903));
#182054=CARTESIAN_POINT('Ctrl Pts',(18.4393551938946,21.3086489544605,0.893204396292285));
#182055=CARTESIAN_POINT('Ctrl Pts',(18.5115571780253,21.3175380608514,0.897592701702668));
#182056=CARTESIAN_POINT('Ctrl Pts',(18.5841373357919,21.3226889406057,0.90198100711305));
#182057=CARTESIAN_POINT('Ctrl Pts',(18.6566098149829,21.3278321786104,0.906362802114936));
#182058=CARTESIAN_POINT('Ctrl Pts',(18.7294588768749,21.3292481656289,0.910744597116822));
#182059=CARTESIAN_POINT('Ctrl Pts',(18.8022695496257,21.3268989268379,0.915126392118709));
#182060=CARTESIAN_POINT('Ctrl Pts',(18.8749947182522,21.3245524468404,0.919503041425181));
#182061=CARTESIAN_POINT('Ctrl Pts',(18.9476811075809,21.3184495401269,0.923879690731654));
#182062=CARTESIAN_POINT('Ctrl Pts',(19.0199116407238,21.3086042366706,0.928256340038127));
#182063=CARTESIAN_POINT('Ctrl Pts',(19.0920963984856,21.2987651725774,0.932630215686693));
#182064=CARTESIAN_POINT('Ctrl Pts',(19.163825396507,21.2851884825072,0.937004091335259));
#182065=CARTESIAN_POINT('Ctrl Pts',(19.2346860015942,21.2679400885314,0.941377966983825));
#182066=CARTESIAN_POINT('Ctrl Pts',(19.3055250721922,21.2506969363307,0.945750513414592));
#182067=CARTESIAN_POINT('Ctrl Pts',(19.3754958054007,21.2297844095034,0.950123059845359));
#182068=CARTESIAN_POINT('Ctrl Pts',(19.4441967521215,21.2053193258042,0.954495606276126));
#182069=CARTESIAN_POINT('Ctrl Pts',(19.5128994804463,21.1808536076582,0.95886826609902));
#182070=CARTESIAN_POINT('Ctrl Pts',(19.5803319031763,21.1528353134295,0.963240925921913));
#182071=CARTESIAN_POINT('Ctrl Pts',(19.6461103019391,21.1214302649133,0.967613585744807));
#182072=CARTESIAN_POINT('Ctrl Pts',(19.7119569921549,21.0899926115231,0.971990785284362));
#182073=CARTESIAN_POINT('Ctrl Pts',(19.7761457936512,21.0551613918966,0.976367984823917));
#182074=CARTESIAN_POINT('Ctrl Pts',(19.838316224423,21.0171491290799,0.980745184363471));
#182075=CARTESIAN_POINT('Ctrl Pts',(19.9005206239767,20.9791160970608,0.985124775524485));
#182076=CARTESIAN_POINT('Ctrl Pts',(19.960704058896,20.937898834125,0.989504366685498));
#182077=CARTESIAN_POINT('Ctrl Pts',(20.0185360368887,20.893752557548,0.993883957846511));
#182078=CARTESIAN_POINT('Ctrl Pts',(20.0764705271474,20.8495280278141,0.998271312217941));
#182079=CARTESIAN_POINT('Ctrl Pts',(20.1320448687351,20.8023644287408,1.00265866658937));
#182080=CARTESIAN_POINT('Ctrl Pts',(20.1849630355814,20.7525561194379,1.0070460209608));
#182081=CARTESIAN_POINT('Ctrl Pts',(20.2209299950565,20.7187028408952,1.01002797982831));
#182082=CARTESIAN_POINT('Ctrl Pts',(20.2556706870372,20.6836286165394,1.01300993869582));
#182083=CARTESIAN_POINT('Ctrl Pts',(20.2891028485224,20.6474345200939,1.01599189756334));
#182084=CARTESIAN_POINT('Ctrl Pts',(20.338299904051,20.59417314262,1.02037999541497));
#182085=CARTESIAN_POINT('Ctrl Pts',(20.3848536174481,20.5382773665806,1.02476809326661));
#182086=CARTESIAN_POINT('Ctrl Pts',(20.4284691674673,20.4800402832467,1.02915619111824));
#182087=CARTESIAN_POINT('Ctrl Pts',(20.4720199654849,20.421889659162,1.03353777436399));
#182088=CARTESIAN_POINT('Ctrl Pts',(20.5126409725289,20.3614050108817,1.03791935760974));
#182089=CARTESIAN_POINT('Ctrl Pts',(20.5500756321549,20.2989146557949,1.04230094085549));
#182090=CARTESIAN_POINT('Ctrl Pts',(20.5874662839342,20.2364977638033,1.04667737315167));
#182091=CARTESIAN_POINT('Ctrl Pts',(20.62167778275,20.1720802607426,1.05105380544786));
#182092=CARTESIAN_POINT('Ctrl Pts',(20.6524961574242,20.1060203874485,1.05543023774404));
#182093=CARTESIAN_POINT('Ctrl Pts',(20.6832949783004,20.0400024281564,1.05980389325936));
#182094=CARTESIAN_POINT('Ctrl Pts',(20.7107047431844,19.9723446023035,1.06417754877469));
#182095=CARTESIAN_POINT('Ctrl Pts',(20.7345575167902,19.9034295068915,1.06855120429001));
#182096=CARTESIAN_POINT('Ctrl Pts',(20.758403025892,19.8345353999817,1.07292352778254));
#182097=CARTESIAN_POINT('Ctrl Pts',(20.7786935367104,19.7643852393011,1.07729585127507));
#182098=CARTESIAN_POINT('Ctrl Pts',(20.7953099613678,19.6933797706848,1.0816681747676));
#182099=CARTESIAN_POINT('Ctrl Pts',(20.8119268074934,19.6223725010462,1.08604060916218));
#182100=CARTESIAN_POINT('Ctrl Pts',(20.8248692744613,19.550510350571,1.09041304355677));
#182101=CARTESIAN_POINT('Ctrl Pts',(20.8340690755323,19.4782056848069,1.09478547795135));
#182102=CARTESIAN_POINT('Ctrl Pts',(20.8432784235523,19.4058259860114,1.09916244977106));
#182103=CARTESIAN_POINT('Ctrl Pts',(20.8487372902008,19.3330033346485,1.10353942159077));
#182104=CARTESIAN_POINT('Ctrl Pts',(20.8504292342169,19.2601558394492,1.10791639341048));
#182105=CARTESIAN_POINT('Ctrl Pts',(20.8521221020959,19.1872685668714,1.1122957552158));
#182106=CARTESIAN_POINT('Ctrl Pts',(20.8500439658808,19.1143569059928,1.11667511702111));
#182107=CARTESIAN_POINT('Ctrl Pts',(20.844230516392,19.041836860729,1.12105447882643));
#182108=CARTESIAN_POINT('Ctrl Pts',(20.8384067616499,18.9691882622835,1.12544160373905));
#182109=CARTESIAN_POINT('Ctrl Pts',(20.8288345343212,18.8969331443913,1.12982872865168));
#182110=CARTESIAN_POINT('Ctrl Pts',(20.815601093585,18.8254797188399,1.1342158535643));
#182111=CARTESIAN_POINT('Ctrl Pts',(20.8066002264401,18.7768799024162,1.13719980379112));
#182112=CARTESIAN_POINT('Ctrl Pts',(20.7959066867639,18.728650750081,1.14018375401795));
#182113=CARTESIAN_POINT('Ctrl Pts',(20.7835610201373,18.6809163983542,1.14316770424477));
#182114=CARTESIAN_POINT('Ctrl Pts',(20.7654052835722,18.6107174904079,1.14755594960082));
#182115=CARTESIAN_POINT('Ctrl Pts',(20.7436033968818,18.5413154230199,1.15194419495686));
#182116=CARTESIAN_POINT('Ctrl Pts',(20.7182422538736,18.4731167585976,1.15633244031291));
#182117=CARTESIAN_POINT('Ctrl Pts',(20.692918748692,18.4050193060766,1.16071417318576));
#182118=CARTESIAN_POINT('Ctrl Pts',(20.6640466398308,18.3381221595675,1.16509590605861));
#182119=CARTESIAN_POINT('Ctrl Pts',(20.6317631518085,18.2728187703658,1.16947763893146));
#182120=CARTESIAN_POINT('Ctrl Pts',(20.5995175966481,18.207592112168,1.17385422330028));
#182121=CARTESIAN_POINT('Ctrl Pts',(20.5638688376431,18.1439559215066,1.1782308076691));
#182122=CARTESIAN_POINT('Ctrl Pts',(20.5250023096655,18.0822840362727,1.18260739203792));
#182123=CARTESIAN_POINT('Ctrl Pts',(20.486160428393,18.0206512594659,1.18698120105247));
#182124=CARTESIAN_POINT('Ctrl Pts',(20.4441050833308,17.9609807236605,1.19135501006701));
#182125=CARTESIAN_POINT('Ctrl Pts',(20.3990671060294,17.9036207388754,1.19572881908156));
#182126=CARTESIAN_POINT('Ctrl Pts',(20.3540428324429,17.8462782070248,1.20010129727632));
#182127=CARTESIAN_POINT('Ctrl Pts',(20.3060380260511,17.7912452096239,1.20447377547108));
#182128=CARTESIAN_POINT('Ctrl Pts',(20.2553252174912,17.7388388054886,1.20884625366584));
#182129=CARTESIAN_POINT('Ctrl Pts',(20.2046111112934,17.6864310603796,1.21321884374345));
#182130=CARTESIAN_POINT('Ctrl Pts',(20.15118920223,17.6366503872243,1.21759143382106));
#182131=CARTESIAN_POINT('Ctrl Pts',(20.0953692876952,17.589777417342,1.22196402389866));
#182132=CARTESIAN_POINT('Ctrl Pts',(20.0394914434218,17.5428558028332,1.22634115183705));
#182133=CARTESIAN_POINT('Ctrl Pts',(19.9812109951272,17.4988482273088,1.23071827977543));
#182134=CARTESIAN_POINT('Ctrl Pts',(19.9208706311964,17.4579948360591,1.23509540771381));
#182135=CARTESIAN_POINT('Ctrl Pts',(19.8604973137098,17.4171191336329,1.23947492612385));
#182136=CARTESIAN_POINT('Ctrl Pts',(19.798062253929,17.3794012947369,1.2438544445339));
#182137=CARTESIAN_POINT('Ctrl Pts',(19.7339345878002,17.3450364901422,1.24823396294394));
#182138=CARTESIAN_POINT('Ctrl Pts',(19.6696932633544,17.310610778203,1.25262124350598));
#182139=CARTESIAN_POINT('Ctrl Pts',(19.6037537785759,17.2795501739061,1.25700852406801));
#182140=CARTESIAN_POINT('Ctrl Pts',(19.5365066298311,17.2520022692517,1.26139580463005));
#182141=CARTESIAN_POINT('Ctrl Pts',(19.4907905552443,17.2332746044005,1.26437837339544));
#182142=CARTESIAN_POINT('Ctrl Pts',(19.4444705346851,17.2161693425274,1.26736094216082));
#182143=CARTESIAN_POINT('Ctrl Pts',(19.3976727118507,17.200719539083,1.27034351092621));
#182144=CARTESIAN_POINT('Ctrl Pts',(19.3288196249543,17.1779884247991,1.27473172930774));
#182145=CARTESIAN_POINT('Ctrl Pts',(19.2586629673008,17.1587544123363,1.27911994768926));
#182146=CARTESIAN_POINT('Ctrl Pts',(19.1875916222504,17.1431645035873,1.28350816607079));
#182147=CARTESIAN_POINT('Ctrl Pts',(19.116625754035,17.1275977317894,1.28788987190657));
#182148=CARTESIAN_POINT('Ctrl Pts',(19.0447483604959,17.1156644301751,1.29227157774234));
#182149=CARTESIAN_POINT('Ctrl Pts',(18.9723645440813,17.1074621838139,1.29665328357812));
#182150=CARTESIAN_POINT('Ctrl Pts',(18.9000657779753,17.0992695750156,1.30102984095045));
#182151=CARTESIAN_POINT('Ctrl Pts',(18.8272622479781,17.0947993667585,1.30540639832278));
#182152=CARTESIAN_POINT('Ctrl Pts',(18.7543686604617,17.0940979905364,1.3097829556951));
#182153=CARTESIAN_POINT('Ctrl Pts',(18.6815212970999,17.0933970590794,1.31415673775246));
#182154=CARTESIAN_POINT('Ctrl Pts',(18.6085844706957,17.0964602223415,1.31853051980982));
#182155=CARTESIAN_POINT('Ctrl Pts',(18.535975995326,17.1032819226536,1.32290430186718));
#182156=CARTESIAN_POINT('Ctrl Pts',(18.4633896113716,17.1101015474364,1.32727675318408));
#182157=CARTESIAN_POINT('Ctrl Pts',(18.3911318600869,17.1206773938757,1.33164920450098));
#182158=CARTESIAN_POINT('Ctrl Pts',(18.3196168493103,17.1349519262733,1.33602165581788));
#182159=CARTESIAN_POINT('Ctrl Pts',(18.2481000066454,17.1492268243192,1.34039421913703));
#182160=CARTESIAN_POINT('Ctrl Pts',(18.1773264149147,17.1672005000461,1.34476678245618));
#182161=CARTESIAN_POINT('Ctrl Pts',(18.1076997240457,17.1887643647835,1.34913934577533));
#182162=CARTESIAN_POINT('Ctrl Pts',(18.0380007684381,17.2103506104072,1.35351644732747));
#182163=CARTESIAN_POINT('Ctrl Pts',(17.9694515520846,17.2355343416688,1.35789354887962));
#182164=CARTESIAN_POINT('Ctrl Pts',(17.9024394858624,17.2641573994472,1.36227065043177));
#182165=CARTESIAN_POINT('Ctrl Pts',(17.8353908196981,17.2927960902648,1.36665014262299));
#182166=CARTESIAN_POINT('Ctrl Pts',(17.7698814087054,17.3248776352815,1.37102963481421));
#182167=CARTESIAN_POINT('Ctrl Pts',(17.706275162751,17.3601972933612,1.37540912700542));
#182168=CARTESIAN_POINT('Ctrl Pts',(17.6425561737593,17.3955795560715,1.37979638191308));
#182169=CARTESIAN_POINT('Ctrl Pts',(17.5807474957366,17.4342111377127,1.38418363682075));
#182170=CARTESIAN_POINT('Ctrl Pts',(17.5211845942116,17.4758435829925,1.38857089172841));
#182171=CARTESIAN_POINT('Ctrl Pts',(17.4806889448312,17.5041486665888,1.39155370035482));
#182172=CARTESIAN_POINT('Ctrl Pts',(17.4412307383374,17.5338399733657,1.39453650898123));
#182173=CARTESIAN_POINT('Ctrl Pts',(17.4029060714275,17.5648293061418,1.39751931760764));
#182174=CARTESIAN_POINT('Ctrl Pts',(17.3472596997714,17.6098249725906,1.40185027442443));
#182175=CARTESIAN_POINT('Ctrl Pts',(17.2937750953766,17.6577445694628,1.40618123124122));
#182176=CARTESIAN_POINT('Ctrl Pts',(17.2427818430318,17.7083498716173,1.41051218805802));
#182177=CARTESIAN_POINT('Ctrl Pts',(17.1918753392824,17.7588690851488,1.41483577714667));
#182178=CARTESIAN_POINT('Ctrl Pts',(17.143452120906,17.8120645856498,1.41915936623532));
#182179=CARTESIAN_POINT('Ctrl Pts',(17.0978092703806,17.8676575655078,1.42348295532397));
#182180=CARTESIAN_POINT('Ctrl Pts',(17.0522098689332,17.9231976244002,1.427802428632));
#182181=CARTESIAN_POINT('Ctrl Pts',(17.0093859023338,17.9811302577511,1.43212190194003));
#182182=CARTESIAN_POINT('Ctrl Pts',(16.9695971044423,18.0411404263128,1.43644137524806));
#182183=CARTESIAN_POINT('Ctrl Pts',(16.929832242303,18.1011144945499,1.44075825008999));
#182184=CARTESIAN_POINT('Ctrl Pts',(16.8930992016319,18.1631632070369,1.44507512493191));
#182185=CARTESIAN_POINT('Ctrl Pts',(16.8596158064165,18.2269406040058,1.44939199977384));
#182186=CARTESIAN_POINT('Ctrl Pts',(16.826140825032,18.2907019747554,1.45370778985555));
#182187=CARTESIAN_POINT('Ctrl Pts',(16.795914098134,18.3561907283349,1.45802357993727));
#182188=CARTESIAN_POINT('Ctrl Pts',(16.7691077535852,18.4230358764645,1.46233937001898));
#182189=CARTESIAN_POINT('Ctrl Pts',(16.742282805863,18.4899274140556,1.46665815518985));
#182190=CARTESIAN_POINT('Ctrl Pts',(16.7188831698401,18.5581767662136,1.47097694036071));
#182191=CARTESIAN_POINT('Ctrl Pts',(16.6990325458087,18.6273935740738,1.47529572553157));
#182192=CARTESIAN_POINT('Ctrl Pts',(16.6791751531992,18.6966339831755,1.47961598330273));
#182193=CARTESIAN_POINT('Ctrl Pts',(16.6628692969198,18.7668420214691,1.48393624107389));
#182194=CARTESIAN_POINT('Ctrl Pts',(16.6501878706664,18.8376154667879,1.48825649884505));
#182195=CARTESIAN_POINT('Ctrl Pts',(16.6374866781147,18.9084992253316,1.49258349051994));
#182196=CARTESIAN_POINT('Ctrl Pts',(16.6284212609924,18.9799496580401,1.49691048219483));
#182197=CARTESIAN_POINT('Ctrl Pts',(16.6230126894231,19.051558554374,1.50123747386971));
#182198=CARTESIAN_POINT('Ctrl Pts',(16.6189685454458,19.1051025785432,1.5044728895608));
#182199=CARTESIAN_POINT('Ctrl Pts',(16.6169678502349,19.1587350720429,1.50770830525189));
#182200=CARTESIAN_POINT('Ctrl Pts',(16.6170003908423,19.2122864004549,1.51094372094299));
#182201=CARTESIAN_POINT('Ctrl Pts',(16.7454193623539,19.9371102172391,0.534177402122746));
#182202=CARTESIAN_POINT('Ctrl Pts',(16.756562724423,19.9676282756865,0.535943849822347));
#182203=CARTESIAN_POINT('Ctrl Pts',(16.7684072898019,19.9978861948824,0.537705174453422));
#182204=CARTESIAN_POINT('Ctrl Pts',(16.8090263026562,20.0950034808735,0.543420741127037));
#182205=CARTESIAN_POINT('Ctrl Pts',(16.8405517695276,20.1606520575966,0.547383534943635));
#182206=CARTESIAN_POINT('Ctrl Pts',(16.9018328518271,20.2730273714616,0.554496494854256));
#182207=CARTESIAN_POINT('Ctrl Pts',(16.9301570205818,20.3204541225289,0.557608838259091));
#182208=CARTESIAN_POINT('Ctrl Pts',(16.9790300138036,20.3954603342754,0.562757572606629));
#182209=CARTESIAN_POINT('Ctrl Pts',(16.9984537533276,20.423742744312,0.564754091846472));
#182210=CARTESIAN_POINT('Ctrl Pts',(17.0248616471255,20.460260144395,0.56741141665792));
#182211=CARTESIAN_POINT('Ctrl Pts',(17.0312342977272,20.4689323409034,0.568048528655164));
#182212=CARTESIAN_POINT('Ctrl Pts',(17.0417745265414,20.4830491155063,0.56909576419284));
#182213=CARTESIAN_POINT('Ctrl Pts',(17.0459029725942,20.4885227706915,0.569504346541613));
#182214=CARTESIAN_POINT('Ctrl Pts',(17.0539417347487,20.4990738703718,0.570296888908976));
#182215=CARTESIAN_POINT('Ctrl Pts',(17.0578486655817,20.5041538086753,0.57068071187744));
#182216=CARTESIAN_POINT('Ctrl Pts',(17.0669165426598,20.5158340681388,0.571568473305868));
#182217=CARTESIAN_POINT('Ctrl Pts',(17.0720937011993,20.5224216141067,0.572073057614116));
#182218=CARTESIAN_POINT('Ctrl Pts',(17.0861068718921,20.5400360809601,0.573432879666399));
#182219=CARTESIAN_POINT('Ctrl Pts',(17.0950142907443,20.551005408837,0.57429099364533));
#182220=CARTESIAN_POINT('Ctrl Pts',(17.1997115698296,20.6773325280239,0.584307127282494));
#182221=CARTESIAN_POINT('Ctrl Pts',(17.3073680119756,20.7822661100089,0.593981625988371));
#182222=CARTESIAN_POINT('Ctrl Pts',(17.4998930276581,20.9337027526133,0.610137964852008));
#182223=CARTESIAN_POINT('Ctrl Pts',(17.5784805043172,20.9873727236999,0.616463116035545));
#182224=CARTESIAN_POINT('Ctrl Pts',(17.6992044460439,21.0584071728718,0.62558485400973));
#182225=CARTESIAN_POINT('Ctrl Pts',(17.7387199493818,21.0799925750724,0.62848263433545));
#182226=CARTESIAN_POINT('Ctrl Pts',(17.8009176767065,21.1114355468572,0.632877777298203));
#182227=CARTESIAN_POINT('Ctrl Pts',(17.8231334431907,21.1221829136802,0.634415899125118));
#182228=CARTESIAN_POINT('Ctrl Pts',(17.8514890955971,21.1352937823555,0.63633456896334));
#182229=CARTESIAN_POINT('Ctrl Pts',(17.8574579143101,21.138019987403,0.636735977221417));
#182230=CARTESIAN_POINT('Ctrl Pts',(17.8665014919926,21.1420998480894,0.637340332364613));
#182231=CARTESIAN_POINT('Ctrl Pts',(17.8695668896895,21.1434739798638,0.63754452063482));
#182232=CARTESIAN_POINT('Ctrl Pts',(17.8758784656048,21.1462852593308,0.637963556785993));
#182233=CARTESIAN_POINT('Ctrl Pts',(17.8791249403604,21.1477215172385,0.638178342160096));
#182234=CARTESIAN_POINT('Ctrl Pts',(17.8864158931906,21.1509251693241,0.638659042109321));
#182235=CARTESIAN_POINT('Ctrl Pts',(17.8904622900809,21.1526880834597,0.638924680508405));
#182236=CARTESIAN_POINT('Ctrl Pts',(17.9007735587099,21.1571421292849,0.639598759682447));
#182237=CARTESIAN_POINT('Ctrl Pts',(17.9070460265367,21.159815696384,0.640006153946092));
#182238=CARTESIAN_POINT('Ctrl Pts',(17.9427413969337,21.1748270650212,0.642310098073665));
#182239=CARTESIAN_POINT('Ctrl Pts',(17.9724290328811,21.1865295053802,0.644170670350717));
#182240=CARTESIAN_POINT('Ctrl Pts',(18.1885440303228,21.2661224211325,0.657394732742192));
#182241=CARTESIAN_POINT('Ctrl Pts',(18.3834475168518,21.3081844708969,0.667705160540902));
#182242=CARTESIAN_POINT('Ctrl Pts',(18.637122459161,21.326520630638,0.681839180760794));
#182243=CARTESIAN_POINT('Ctrl Pts',(18.6930022215356,21.3283406221212,0.6849891144651));
#182244=CARTESIAN_POINT('Ctrl Pts',(18.7835696213148,21.3277037771267,0.690198378493945));
#182245=CARTESIAN_POINT('Ctrl Pts',(18.8182406329936,21.3266075582574,0.692217108574196));
#182246=CARTESIAN_POINT('Ctrl Pts',(18.8637192659375,21.324049938197,0.694903406692536));
#182247=CARTESIAN_POINT('Ctrl Pts',(18.8745658310064,21.3233561181223,0.695546938774921));
#182248=CARTESIAN_POINT('Ctrl Pts',(18.8923112791503,21.3220837172094,0.696604641425374));
#182249=CARTESIAN_POINT('Ctrl Pts',(18.8992136022352,21.3215547578925,0.697017252603233));
#182250=CARTESIAN_POINT('Ctrl Pts',(18.9125618877222,21.3204659312838,0.697817573212983));
#182251=CARTESIAN_POINT('Ctrl Pts',(18.9190081293011,21.3199103474658,0.698205143869197));
#182252=CARTESIAN_POINT('Ctrl Pts',(18.9338756702912,21.3185602637672,0.699101555770323));
#182253=CARTESIAN_POINT('Ctrl Pts',(18.9422949152877,21.3177448288805,0.699611049189496));
#182254=CARTESIAN_POINT('Ctrl Pts',(18.9649012567384,21.3154184859775,0.700984204353337));
#182255=CARTESIAN_POINT('Ctrl Pts',(18.9790781526884,21.3138145990467,0.701850770658813));
#182256=CARTESIAN_POINT('Ctrl Pts',(19.106811711782,21.2980543600734,0.709708819570844));
#182257=CARTESIAN_POINT('Ctrl Pts',(19.2190444174331,21.2748578120664,0.716988278950171));
#182258=CARTESIAN_POINT('Ctrl Pts',(19.4859092918018,21.1967258837588,0.735128312832324));
#182259=CARTESIAN_POINT('Ctrl Pts',(19.6371123258896,21.132682254234,0.746145465618919));
#182260=CARTESIAN_POINT('Ctrl Pts',(19.8079305733085,21.0356743765984,0.758627853763173));
#182261=CARTESIAN_POINT('Ctrl Pts',(19.8360559134626,21.0188264556625,0.760682339621224));
#182262=CARTESIAN_POINT('Ctrl Pts',(19.8699355201268,20.9974468835483,0.763145753105675));
#182263=CARTESIAN_POINT('Ctrl Pts',(19.8760707536261,20.993530889175,0.763591381934539));
#182264=CARTESIAN_POINT('Ctrl Pts',(19.8856545564423,20.9873439502646,0.764286605607547));
#182265=CARTESIAN_POINT('Ctrl Pts',(19.8891168183034,20.985094468668,0.764537580047137));
#182266=CARTESIAN_POINT('Ctrl Pts',(19.8955694360586,20.9808752122556,0.765004944770918));
#182267=CARTESIAN_POINT('Ctrl Pts',(19.8985613494921,20.9789079968479,0.76522149408671));
#182268=CARTESIAN_POINT('Ctrl Pts',(19.9053744241816,20.9744035262513,0.765714268441916));
#182269=CARTESIAN_POINT('Ctrl Pts',(19.9091923301671,20.9718614443066,0.765990165718856));
#182270=CARTESIAN_POINT('Ctrl Pts',(19.9208987848998,20.9640118857327,0.766835470681614));
#182271=CARTESIAN_POINT('Ctrl Pts',(19.9287599901286,20.9586635748104,0.76740220439784));
#182272=CARTESIAN_POINT('Ctrl Pts',(19.998928625162,20.9102301392836,0.772455181903175));
#182273=CARTESIAN_POINT('Ctrl Pts',(20.0589248387729,20.8638775671038,0.776736150494002));
#182274=CARTESIAN_POINT('Ctrl Pts',(20.2235252286147,20.7219736403893,0.788766768780923));
#182275=CARTESIAN_POINT('Ctrl Pts',(20.3211982725721,20.6190236933256,0.796291251981862));
#182276=CARTESIAN_POINT('Ctrl Pts',(20.4457161798494,20.4582123097537,0.80754379327122));
#182277=CARTESIAN_POINT('Ctrl Pts',(20.4814031027039,20.4077006159384,0.811013082959222));
#182278=CARTESIAN_POINT('Ctrl Pts',(20.5349762899166,20.3243561805785,0.816699232903889));
#182279=CARTESIAN_POINT('Ctrl Pts',(20.5542933360489,20.2924848601878,0.818864949667193));
#182280=CARTESIAN_POINT('Ctrl Pts',(20.5782785544778,20.2504468188019,0.821718054571487));
#182281=CARTESIAN_POINT('Ctrl Pts',(20.5837221443767,20.2407286327283,0.822377375253046));
#182282=CARTESIAN_POINT('Ctrl Pts',(20.5924483826058,20.2248576007117,0.823453923213482));
#182283=CARTESIAN_POINT('Ctrl Pts',(20.5957778127629,20.2187306184926,0.823869472658562));
#182284=CARTESIAN_POINT('Ctrl Pts',(20.6021210519353,20.2069187394009,0.824670542748269));
#182285=CARTESIAN_POINT('Ctrl Pts',(20.6051393374452,20.2012363246328,0.825055898523084));
#182286=CARTESIAN_POINT('Ctrl Pts',(20.6119890984084,20.1881973926964,0.825940136923312));
#182287=CARTESIAN_POINT('Ctrl Pts',(20.6158033200074,20.1808319750276,0.82643962238248));
#182288=CARTESIAN_POINT('Ctrl Pts',(20.6258176840739,20.1612123217581,0.827770215726289));
#182289=CARTESIAN_POINT('Ctrl Pts',(20.6319419562772,20.1489199981086,0.828603966026123));
#182290=CARTESIAN_POINT('Ctrl Pts',(20.6774831391373,20.0552393110141,0.834959697891674));
#182291=CARTESIAN_POINT('Ctrl Pts',(20.711763278092,19.9714705122986,0.8406585477474));
#182292=CARTESIAN_POINT('Ctrl Pts',(20.7851878759223,19.753127877923,0.855533026036699));
#182293=CARTESIAN_POINT('Ctrl Pts',(20.8165298322493,19.6163873061826,0.864885018278535));
#182294=CARTESIAN_POINT('Ctrl Pts',(20.8410840997466,19.4229394133724,0.877655839379692));
#182295=CARTESIAN_POINT('Ctrl Pts',(20.8458846130369,19.3680539115681,0.881224599450029));
#182296=CARTESIAN_POINT('Ctrl Pts',(20.8499087233967,19.2846638846011,0.886508591014392));
#182297=CARTESIAN_POINT('Ctrl Pts',(20.8507068063223,19.2562611687222,0.888284013697192));
#182298=CARTESIAN_POINT('Ctrl Pts',(20.8509881595326,19.2209124692084,0.890456401206748));
#182299=CARTESIAN_POINT('Ctrl Pts',(20.8510092763564,19.2139751549177,0.890880956092271));
#182300=CARTESIAN_POINT('Ctrl Pts',(20.8509887259096,19.2029952209623,0.891549956632903));
#182301=CARTESIAN_POINT('Ctrl Pts',(20.8509695805187,19.1989526805118,0.891795631578339));
#182302=CARTESIAN_POINT('Ctrl Pts',(20.8509116365182,19.1913289835508,0.892257713649244));
#182303=CARTESIAN_POINT('Ctrl Pts',(20.8508753308638,19.1877479144022,0.892474251670799));
#182304=CARTESIAN_POINT('Ctrl Pts',(20.8507715425597,19.1795601916312,0.89296818434669));
#182305=CARTESIAN_POINT('Ctrl Pts',(20.8506981096344,19.1749536613371,0.893245243014076));
#182306=CARTESIAN_POINT('Ctrl Pts',(20.8504631740722,19.1627215689918,0.893978808342041));
#182307=CARTESIAN_POINT('Ctrl Pts',(20.8502754963577,19.1550964975247,0.894433888654916));
#182308=CARTESIAN_POINT('Ctrl Pts',(20.8486701978515,19.1016253983308,0.897610763825298));
#182309=CARTESIAN_POINT('Ctrl Pts',(20.8458040228594,19.0558313995566,0.900257365127691));
#182310=CARTESIAN_POINT('Ctrl Pts',(20.8378739168719,18.9726179803269,0.904989142841095));
#182311=CARTESIAN_POINT('Ctrl Pts',(20.8332930773317,18.9351735114383,0.907089570446307));
#182312=CARTESIAN_POINT('Ctrl Pts',(20.8083555701369,18.7684312259721,0.916389477500067));
#182313=CARTESIAN_POINT('Ctrl Pts',(20.777035687811,18.641065964461,0.923366564881029));
#182314=CARTESIAN_POINT('Ctrl Pts',(20.705212815092,18.4339465175242,0.935466838489206));
#182315=CARTESIAN_POINT('Ctrl Pts',(20.6710793765109,18.352388911897,0.940438849597747));
#182316=CARTESIAN_POINT('Ctrl Pts',(20.6228630349491,18.2548061462674,0.946782331582785));
#182317=CARTESIAN_POINT('Ctrl Pts',(20.6135042311001,18.2365390965994,0.947987338026081));
#182318=CARTESIAN_POINT('Ctrl Pts',(20.5997291506858,18.2105889996192,0.949725672894016));
#182319=CARTESIAN_POINT('Ctrl Pts',(20.5955277563891,18.202792758427,0.950251396563604));
#182320=CARTESIAN_POINT('Ctrl Pts',(20.588160908399,18.1893256380738,0.951165662242911));
#182321=CARTESIAN_POINT('Ctrl Pts',(20.5850180281311,18.1836424993534,0.951553393935635));
#182322=CARTESIAN_POINT('Ctrl Pts',(20.5789257769324,18.1727448449794,0.952300606915968));
#182323=CARTESIAN_POINT('Ctrl Pts',(20.5759803200329,18.1675282041279,0.952659944677853));
#182324=CARTESIAN_POINT('Ctrl Pts',(20.5682083863953,18.153898934718,0.953603142492548));
#182325=CARTESIAN_POINT('Ctrl Pts',(20.563346210824,18.1455069202548,0.954188289950987));
#182326=CARTESIAN_POINT('Ctrl Pts',(20.5462827913925,18.1165169130269,0.956225130370639));
#182327=CARTESIAN_POINT('Ctrl Pts',(20.5337902901707,18.0960932858948,0.957687396616656));
#182328=CARTESIAN_POINT('Ctrl Pts',(20.4376925009152,17.9448111592422,0.968729204112628));
#182329=CARTESIAN_POINT('Ctrl Pts',(20.34027644589,17.8233178575756,0.97884485449836));
#182330=CARTESIAN_POINT('Ctrl Pts',(20.1778921519579,17.6610350514906,0.994011792193418));
#182331=CARTESIAN_POINT('Ctrl Pts',(20.1225742907394,17.6112881889482,0.998935581684665));
#182332=CARTESIAN_POINT('Ctrl Pts',(20.0289959185024,17.5356527557143,1.00677230860608));
#182333=CARTESIAN_POINT('Ctrl Pts',(19.9923045519036,17.5079224861622,1.00973306822747));
#182334=CARTESIAN_POINT('Ctrl Pts',(19.9410807314654,17.4717689909137,1.01368767338731));
#182335=CARTESIAN_POINT('Ctrl Pts',(19.9273103184001,17.462292215346,1.014733828231));
#182336=CARTESIAN_POINT('Ctrl Pts',(19.903532099743,17.4463397800455,1.01650952332766));
#182337=CARTESIAN_POINT('Ctrl Pts',(19.8935793863024,17.4397838398172,1.0172437096036));
#182338=CARTESIAN_POINT('Ctrl Pts',(19.8793553338677,17.4305856185229,1.01827957692009));
#182339=CARTESIAN_POINT('Ctrl Pts',(19.8751293491425,17.4278740873655,1.01858566960918));
#182340=CARTESIAN_POINT('Ctrl Pts',(19.8678307253824,17.4232276234403,1.01911139911738));
#182341=CARTESIAN_POINT('Ctrl Pts',(19.8647626966823,17.42128552311,1.01933150900175));
#182342=CARTESIAN_POINT('Ctrl Pts',(19.8588028095985,17.4175342839181,1.01975735882644));
#182343=CARTESIAN_POINT('Ctrl Pts',(19.855911578675,17.4157242425584,1.01996316173796));
#182344=CARTESIAN_POINT('Ctrl Pts',(19.8481018998813,17.410861264295,1.02051699468));
#182345=CARTESIAN_POINT('Ctrl Pts',(19.8431752419216,17.4078214742838,1.02086416357736));
#182346=CARTESIAN_POINT('Ctrl Pts',(19.8248594297354,17.3966239311569,1.02214689192026));
#182347=CARTESIAN_POINT('Ctrl Pts',(19.8113918692479,17.3885945546693,1.023074413435));
#182348=CARTESIAN_POINT('Ctrl Pts',(19.6817562469272,17.3132450594279,1.0318659480391));
#182349=CARTESIAN_POINT('Ctrl Pts',(19.5595044184214,17.2569610832956,1.03912864395588));
#182350=CARTESIAN_POINT('Ctrl Pts',(19.2810394942221,17.1595956316299,1.05514838674519));
#182351=CARTESIAN_POINT('Ctrl Pts',(19.1238252819166,17.1240069057325,1.06389558018213));
#182352=CARTESIAN_POINT('Ctrl Pts',(18.9455568359212,17.1045145556216,1.07436835072972));
#182353=CARTESIAN_POINT('Ctrl Pts',(18.9269811360656,17.1027316417664,1.07546547326997));
#182354=CARTESIAN_POINT('Ctrl Pts',(18.8998844264901,17.1004919792369,1.07707529753234));
#182355=CARTESIAN_POINT('Ctrl Pts',(18.8913800590163,17.099840777574,1.07758189383347));
#182356=CARTESIAN_POINT('Ctrl Pts',(18.8764405353975,17.0987875901689,1.07847428247974));
#182357=CARTESIAN_POINT('Ctrl Pts',(18.8700070065114,17.098363575262,1.07885937815791));
#182358=CARTESIAN_POINT('Ctrl Pts',(18.8574944324215,17.097596300476,1.07960994241787));
#182359=CARTESIAN_POINT('Ctrl Pts',(18.8514156400376,17.0972498638034,1.07997530729846));
#182360=CARTESIAN_POINT('Ctrl Pts',(18.8368538355291,17.0964829803371,1.08085232543758));
#182361=CARTESIAN_POINT('Ctrl Pts',(18.8283696716416,17.0960873541176,1.081364752428));
#182362=CARTESIAN_POINT('Ctrl Pts',(18.7975852360219,17.0948374476746,1.08322945554901));
#182363=CARTESIAN_POINT('Ctrl Pts',(18.77527480158,17.0942847709103,1.08459112651012));
#182364=CARTESIAN_POINT('Ctrl Pts',(18.5696370501641,17.092442947411,1.09724050598387));
#182365=CARTESIAN_POINT('Ctrl Pts',(18.3869095019468,17.114621993147,1.10930507321904));
#182366=CARTESIAN_POINT('Ctrl Pts',(18.1303765751045,17.1802425924788,1.12678910836463));
#182367=CARTESIAN_POINT('Ctrl Pts',(18.0526131915509,17.2049963454408,1.13214926255902));
#182368=CARTESIAN_POINT('Ctrl Pts',(17.942474308772,17.2472023294859,1.13967023409712));
#182369=CARTESIAN_POINT('Ctrl Pts',(17.9088205167623,17.2611042593566,1.14195787922325));
#182370=CARTESIAN_POINT('Ctrl Pts',(17.8686915012132,17.278906231316,1.14465883465502));
#182371=CARTESIAN_POINT('Ctrl Pts',(17.861859245781,17.2819806538699,1.1451177355558));
#182372=CARTESIAN_POINT('Ctrl Pts',(17.8512529387791,17.2868212178856,1.14582847055771));
#182373=CARTESIAN_POINT('Ctrl Pts',(17.8474676156361,17.2885623048334,1.14608179722232));
#182374=CARTESIAN_POINT('Ctrl Pts',(17.8404514779522,17.2918145581987,1.14655069325017));
#182375=CARTESIAN_POINT('Ctrl Pts',(17.837219370951,17.2933227005223,1.1467664385459));
#182376=CARTESIAN_POINT('Ctrl Pts',(17.8299132224204,17.2967543534277,1.14725355243876));
#182377=CARTESIAN_POINT('Ctrl Pts',(17.8258415114156,17.2986826996313,1.14752461795879));
#182378=CARTESIAN_POINT('Ctrl Pts',(17.8135518570699,17.3045511352816,1.14834164841966));
#182379=CARTESIAN_POINT('Ctrl Pts',(17.8053530477413,17.308531366248,1.14888518660741));
#182380=CARTESIAN_POINT('Ctrl Pts',(17.7424065273014,17.3395935525834,1.15304834380841));
#182381=CARTESIAN_POINT('Ctrl Pts',(17.6888228828542,17.3689831792963,1.15653479048717));
#182382=CARTESIAN_POINT('Ctrl Pts',(17.4971417733759,17.4851788360589,1.16906404592256));
#182383=CARTESIAN_POINT('Ctrl Pts',(17.3679313906238,17.5855341478838,1.17766507248722));
#182384=CARTESIAN_POINT('Ctrl Pts',(17.1948923580372,17.755277429185,1.19111361657844));
#182385=CARTESIAN_POINT('Ctrl Pts',(17.1414403898582,17.8139558127117,1.19560092677501));
#182386=CARTESIAN_POINT('Ctrl Pts',(17.0791845688009,17.8905264389171,1.20135956975125));
#182387=CARTESIAN_POINT('Ctrl Pts',(17.0671668158494,17.9057292862489,1.2024982983823));
#182388=CARTESIAN_POINT('Ctrl Pts',(17.0500840151202,17.9279602786127,1.20415785490096));
#182389=CARTESIAN_POINT('Ctrl Pts',(17.0448505108801,17.9348581697942,1.20467202029336));
#182390=CARTESIAN_POINT('Ctrl Pts',(17.0357829761627,17.9469629165049,1.20557306336989));
#182391=CARTESIAN_POINT('Ctrl Pts',(17.0319301869602,17.9521556257389,1.20595920014339));
#182392=CARTESIAN_POINT('Ctrl Pts',(17.0245195163643,17.9622397907126,1.20670835117519));
#182393=CARTESIAN_POINT('Ctrl Pts',(17.0209586865201,17.9671290093577,1.2070712455981));
#182394=CARTESIAN_POINT('Ctrl Pts',(17.0125345137373,17.9788006522251,1.20793681914304));
#182395=CARTESIAN_POINT('Ctrl Pts',(17.0076902571042,17.9855966698619,1.20844022807978));
#182396=CARTESIAN_POINT('Ctrl Pts',(16.9905656820661,18.0099238470477,1.21024028263255));
#182397=CARTESIAN_POINT('Ctrl Pts',(16.9785115262743,18.0276119351793,1.21154550356417));
#182398=CARTESIAN_POINT('Ctrl Pts',(16.8609883967056,18.2058115432035,1.22466377459197));
#182399=CARTESIAN_POINT('Ctrl Pts',(16.7775784210625,18.379759765152,1.23734170243807));
#182400=CARTESIAN_POINT('Ctrl Pts',(16.6954799621187,18.6348874106491,1.25502391933077));
#182401=CARTESIAN_POINT('Ctrl Pts',(16.6761041769799,18.708470376627,1.26000955659167));
#182402=CARTESIAN_POINT('Ctrl Pts',(16.6536719490474,18.8171191060143,1.26707452535752));
#182403=CARTESIAN_POINT('Ctrl Pts',(16.6474610385367,18.8514691274986,1.26926548143157));
#182404=CARTESIAN_POINT('Ctrl Pts',(16.6409663501366,18.8932676544488,1.27186750771622));
#182405=CARTESIAN_POINT('Ctrl Pts',(16.6398690473808,18.9005821205761,1.27232048023146));
#182406=CARTESIAN_POINT('Ctrl Pts',(16.6382167990534,18.9120034350701,1.2730239363616));
#182407=CARTESIAN_POINT('Ctrl Pts',(16.6376355523324,18.9161063336645,1.27327586689129));
#182408=CARTESIAN_POINT('Ctrl Pts',(16.6365763775096,18.9237442393853,1.27374338568317));
#182409=CARTESIAN_POINT('Ctrl Pts',(16.6360953416481,18.9272787126141,1.27395914218768));
#182410=CARTESIAN_POINT('Ctrl Pts',(16.6350235911771,18.9353053093827,1.27444778944548));
#182411=CARTESIAN_POINT('Ctrl Pts',(16.6344383637346,18.9397981127852,1.27472036792849));
#182412=CARTESIAN_POINT('Ctrl Pts',(16.6327408137149,18.9531651309163,1.27552865258896));
#182413=CARTESIAN_POINT('Ctrl Pts',(16.6316702819437,18.9620446814931,1.27606206003475));
#182414=CARTESIAN_POINT('Ctrl Pts',(16.6239226730706,19.029924671547,1.28011460872583));
#182415=CARTESIAN_POINT('Ctrl Pts',(16.6196735815236,19.0891814573785,1.28350785079841));
#182416=CARTESIAN_POINT('Ctrl Pts',(16.6173229666297,19.1688226796919,1.28796711911347));
#182417=CARTESIAN_POINT('Ctrl Pts',(16.6170159594102,19.1891094974751,1.28909419861729));
#182418=CARTESIAN_POINT('Ctrl Pts',(16.6168948152935,19.3491947907339,1.29793912363836));
#182419=CARTESIAN_POINT('Ctrl Pts',(16.6306361030147,19.4886587757916,1.30537418782863));
#182420=CARTESIAN_POINT('Ctrl Pts',(16.6757502469593,19.7144696845794,1.31812043168447));
#182421=CARTESIAN_POINT('Ctrl Pts',(16.6991412224403,19.801948935857,1.32323611985921));
#182422=CARTESIAN_POINT('Ctrl Pts',(16.7324404233321,19.9006641777299,1.32934387929102));
#182423=CARTESIAN_POINT('Ctrl Pts',(16.7369541495324,19.9136274082935,1.33015265068163));
#182424=CARTESIAN_POINT('Ctrl Pts',(16.7428594777534,19.9300705448463,1.33118740163996));
#182425=CARTESIAN_POINT('Ctrl Pts',(16.7441347553409,19.9335920948211,1.33140952983418));
#182426=CARTESIAN_POINT('Ctrl Pts',(16.7454193623274,19.9371102171666,1.33163196712539));
#182427=CARTESIAN_POINT('Origin',(18.734,19.211,0.));
#182428=CARTESIAN_POINT('',(16.7454193622815,19.9371102170409,2.35747630371139));
#182429=CARTESIAN_POINT('',(16.7452305776443,19.937179123763,2.13351566305583));
#182430=CARTESIAN_POINT('',(16.7454193623258,19.9371102171621,0.));
#182431=CARTESIAN_POINT('Ctrl Pts',(16.7454193622815,19.9371102170409,2.35747630371138));
#182432=CARTESIAN_POINT('Ctrl Pts',(16.7421916428779,19.9282705393179,2.35692304823925));
#182433=CARTESIAN_POINT('Ctrl Pts',(16.7390229031478,19.919409444425,2.35636787685067));
#182434=CARTESIAN_POINT('Ctrl Pts',(16.7330803316954,19.9024354550413,2.35530316719403));
#182435=CARTESIAN_POINT('Ctrl Pts',(16.7302965276,19.8943263487455,2.35479397698));
#182436=CARTESIAN_POINT('Ctrl Pts',(16.7255041835947,19.8800853364624,2.35389871683677));
#182437=CARTESIAN_POINT('Ctrl Pts',(16.7234742638274,19.8739607037764,2.35351335928524));
#182438=CARTESIAN_POINT('Ctrl Pts',(16.7195884540883,19.8620545243586,2.35276354714619));
#182439=CARTESIAN_POINT('Ctrl Pts',(16.7177293752827,19.8562740787429,2.35239920214096));
#182440=CARTESIAN_POINT('Ctrl Pts',(16.7133468271313,19.8424435261815,2.351526675112));
#182441=CARTESIAN_POINT('Ctrl Pts',(16.7108465737502,19.8343862225071,2.3510177359621));
#182442=CARTESIAN_POINT('Ctrl Pts',(16.7020108002507,19.8052989880253,2.34917805477513));
#182443=CARTESIAN_POINT('Ctrl Pts',(16.6959546542506,19.7841862757418,2.34783823684224));
#182444=CARTESIAN_POINT('Ctrl Pts',(16.6414577133137,19.5824062330039,2.33498641159933));
#182445=CARTESIAN_POINT('Ctrl Pts',(16.6168436530152,19.3961933092232,2.32266064775721));
#182446=CARTESIAN_POINT('Ctrl Pts',(16.6170536898772,19.1462094399707,2.3061586393481));
#182447=CARTESIAN_POINT('Ctrl Pts',(16.6199199086378,19.0832283233664,2.30201614374009));
#182448=CARTESIAN_POINT('Ctrl Pts',(16.6300811390682,18.9707861221989,2.2947363950253));
#182449=CARTESIAN_POINT('Ctrl Pts',(16.6363255948254,18.921275584138,2.29157203981558));
#182450=CARTESIAN_POINT('Ctrl Pts',(16.6455655229157,18.8643135233085,2.28801329018632));
#182451=CARTESIAN_POINT('Ctrl Pts',(16.6468596252141,18.8566059559694,2.28753350617277));
#182452=CARTESIAN_POINT('Ctrl Pts',(16.6489941838508,18.8443100738919,2.28677109956862));
#182453=CARTESIAN_POINT('Ctrl Pts',(16.6498071584168,18.8397171491461,2.28648698330481));
#182454=CARTESIAN_POINT('Ctrl Pts',(16.6512728103321,18.8315934301886,2.28598568261531));
#182455=CARTESIAN_POINT('Ctrl Pts',(16.6519192987997,18.8280615633969,2.28576815044178));
#182456=CARTESIAN_POINT('Ctrl Pts',(16.6533073569953,18.8205858242115,2.28530859973261));
#182457=CARTESIAN_POINT('Ctrl Pts',(16.6540511540512,18.8166424184035,2.28506670962336));
#182458=CARTESIAN_POINT('Ctrl Pts',(16.6560859638992,18.8060203347525,2.28441649108939));
#182459=CARTESIAN_POINT('Ctrl Pts',(16.6573979732943,18.7993456592714,2.28400934259613));
#182460=CARTESIAN_POINT('Ctrl Pts',(16.6640292714419,18.7664484385469,2.28200921024176));
#182461=CARTESIAN_POINT('Ctrl Pts',(16.6698134510644,18.7403207569644,2.28044126551913));
#182462=CARTESIAN_POINT('Ctrl Pts',(16.6879077730099,18.6653517902546,2.27598364097259));
#182463=CARTESIAN_POINT('Ctrl Pts',(16.7014678599552,18.6168290260983,2.27314935350431));
#182464=CARTESIAN_POINT('Ctrl Pts',(16.756810292162,18.4429805862964,2.26303183181702));
#182465=CARTESIAN_POINT('Ctrl Pts',(16.8085640147541,18.3211507605477,2.25599588680572));
#182466=CARTESIAN_POINT('Ctrl Pts',(16.9207548827088,18.1134366353935,2.24300919011769));
#182467=CARTESIAN_POINT('Ctrl Pts',(16.9768431354944,18.0257156875147,2.23716707856686));
#182468=CARTESIAN_POINT('Ctrl Pts',(17.0475681402362,17.9312210206559,2.23025033500863));
#182469=CARTESIAN_POINT('Ctrl Pts',(17.056104121899,17.920049938363,2.22942224329744));
#182470=CARTESIAN_POINT('Ctrl Pts',(17.0699092577066,17.9023513257223,2.22809313104478));
#182471=CARTESIAN_POINT('Ctrl Pts',(17.0751071298142,17.8957685399776,2.22759493212877));
#182472=CARTESIAN_POINT('Ctrl Pts',(17.0843685936553,17.8841817101953,2.22671108816971));
#182473=CARTESIAN_POINT('Ctrl Pts',(17.0884162012368,17.8791649836453,2.22632608715451));
#182474=CARTESIAN_POINT('Ctrl Pts',(17.0968603465692,17.8687963167266,2.22552547830482));
#182475=CARTESIAN_POINT('Ctrl Pts',(17.1012603585654,17.8634473168953,2.2251097324128));
#182476=CARTESIAN_POINT('Ctrl Pts',(17.1126754498701,17.8497082210246,2.22403475706673));
#182477=CARTESIAN_POINT('Ctrl Pts',(17.1197293722189,17.8413507976079,2.22337394535432));
#182478=CARTESIAN_POINT('Ctrl Pts',(17.1499117511812,17.8061480471852,2.22056070805275));
#182479=CARTESIAN_POINT('Ctrl Pts',(17.1736464405703,17.779832252762,2.21838327367008));
#182480=CARTESIAN_POINT('Ctrl Pts',(17.2376865467791,17.7123152911793,2.21259355592549));
#182481=CARTESIAN_POINT('Ctrl Pts',(17.2790313710179,17.6721448524831,2.20893871029385));
#182482=CARTESIAN_POINT('Ctrl Pts',(17.4217681706141,17.5443621044183,2.19659997877115));
#182483=CARTESIAN_POINT('Ctrl Pts',(17.5298270654757,17.4646905569085,2.1876735729432));
#182484=CARTESIAN_POINT('Ctrl Pts',(17.7216270922426,17.3495907987171,2.17297277944647));
#182485=CARTESIAN_POINT('Ctrl Pts',(17.801447271982,17.3083459866533,2.1671522524706));
#182486=CARTESIAN_POINT('Ctrl Pts',(17.8924920006888,17.2684124361835,2.16101025159265));
#182487=CARTESIAN_POINT('Ctrl Pts',(17.9013574903227,17.264595978432,2.1604172500096));
#182488=CARTESIAN_POINT('Ctrl Pts',(17.9144966592135,17.259045969636,2.15954620154277));
#182489=CARTESIAN_POINT('Ctrl Pts',(17.918750254094,17.2572655976455,2.15926541695837));
#182490=CARTESIAN_POINT('Ctrl Pts',(17.9263117559006,17.2541296722974,2.15876845137721));
#182491=CARTESIAN_POINT('Ctrl Pts',(17.9296173090924,17.2527685871322,2.15855193835014));
#182492=CARTESIAN_POINT('Ctrl Pts',(17.93671255248,17.2498680674558,2.15808879236009));
#182493=CARTESIAN_POINT('Ctrl Pts',(17.9405032505194,17.2483312454638,2.15784231756675));
#182494=CARTESIAN_POINT('Ctrl Pts',(17.9509339903075,17.2441375816814,2.15716668800416));
#182495=CARTESIAN_POINT('Ctrl Pts',(17.9575831489717,17.2415033574815,2.15673887665619));
#182496=CARTESIAN_POINT('Ctrl Pts',(17.9933579779158,17.2275396283182,2.15445184939543));
#182497=CARTESIAN_POINT('Ctrl Pts',(18.0227201288014,17.2168217658297,2.1526271060226));
#182498=CARTESIAN_POINT('Ctrl Pts',(18.2073709333748,17.1540177398109,2.14141262205081));
#182499=CARTESIAN_POINT('Ctrl Pts',(18.3680442264973,17.119444862239,2.13275773579844));
#182500=CARTESIAN_POINT('Ctrl Pts',(18.647749584182,17.0925146075893,2.11737622763435));
#182501=CARTESIAN_POINT('Ctrl Pts',(18.765102781162,17.0909889587338,2.11083586759811));
#182502=CARTESIAN_POINT('Ctrl Pts',(18.8962303121261,17.1001767822463,2.10313518861532));
#182503=CARTESIAN_POINT('Ctrl Pts',(18.9104790289181,17.1013202925066,2.10229341748671));
#182504=CARTESIAN_POINT('Ctrl Pts',(18.933136455166,17.1033697723491,2.10094649518382));
#182505=CARTESIAN_POINT('Ctrl Pts',(18.9415533576519,17.1041819953193,2.10044428757857));
#182506=CARTESIAN_POINT('Ctrl Pts',(18.9563884336583,17.1057033277943,2.09955578549437));
#182507=CARTESIAN_POINT('Ctrl Pts',(18.9628086881437,17.1063914197102,2.09917015747445));
#182508=CARTESIAN_POINT('Ctrl Pts',(18.9760805754408,17.107875283648,2.0983706609248));
#182509=CARTESIAN_POINT('Ctrl Pts',(18.982931660299,17.1086751905841,2.09795666625769));
#182510=CARTESIAN_POINT('Ctrl Pts',(19.0005060023557,17.1108142150008,2.09689133169374));
#182511=CARTESIAN_POINT('Ctrl Pts',(19.0112230393153,17.1122019724386,2.09623846326779));
#182512=CARTESIAN_POINT('Ctrl Pts',(19.0558971050588,17.1183349900579,2.09350325063088));
#182513=CARTESIAN_POINT('Ctrl Pts',(19.0897453995607,17.1238225794588,2.0913975931615));
#182514=CARTESIAN_POINT('Ctrl Pts',(19.1775689213188,17.140259135785,2.08584398846928));
#182515=CARTESIAN_POINT('Ctrl Pts',(19.2312739437073,17.1524959508476,2.08235767083882));
#182516=CARTESIAN_POINT('Ctrl Pts',(19.3900380553204,17.1952462725111,2.07178960915063));
#182517=CARTESIAN_POINT('Ctrl Pts',(19.4932692555904,17.2318194244407,2.06455946934908));
#182518=CARTESIAN_POINT('Ctrl Pts',(19.634393389881,17.2944896723399,2.05435925219723));
#182519=CARTESIAN_POINT('Ctrl Pts',(19.6749886672248,17.31409183085,2.0513876085094));
#182520=CARTESIAN_POINT('Ctrl Pts',(19.7364761528521,17.3462421536707,2.04685419159514));
#182521=CARTESIAN_POINT('Ctrl Pts',(19.7578290743788,17.3578798332692,2.0452736925429));
#182522=CARTESIAN_POINT('Ctrl Pts',(19.7915116571956,17.3769973235664,2.04277555976828));
#182523=CARTESIAN_POINT('Ctrl Pts',(19.8039733020188,17.3842395141737,2.04185020593773));
#182524=CARTESIAN_POINT('Ctrl Pts',(19.8483316372979,17.4106283925259,2.03855475772147));
#182525=CARTESIAN_POINT('Ctrl Pts',(19.8797984294329,17.4304890421585,2.036214036563));
#182526=CARTESIAN_POINT('Ctrl Pts',(19.9166855144527,17.4551539522948,2.0334813444334));
#182527=CARTESIAN_POINT('Ctrl Pts',(19.9226233604314,17.4591681359994,2.0330418114839));
#182528=CARTESIAN_POINT('Ctrl Pts',(19.9322725397851,17.4657629527011,2.03232829476937));
#182529=CARTESIAN_POINT('Ctrl Pts',(19.9359961402759,17.4683254146268,2.03205313052908));
#182530=CARTESIAN_POINT('Ctrl Pts',(19.9426431282497,17.4729310977855,2.03156230138629));
#182531=CARTESIAN_POINT('Ctrl Pts',(19.9455695757653,17.4749697917366,2.03134633565539));
#182532=CARTESIAN_POINT('Ctrl Pts',(19.9518919175143,17.4793979908006,2.03088004765549));
#182533=CARTESIAN_POINT('Ctrl Pts',(19.9552859274201,17.4817900864337,2.03062990642015));
#182534=CARTESIAN_POINT('Ctrl Pts',(19.9647365856681,17.4884926071104,2.02993380883579));
#182535=CARTESIAN_POINT('Ctrl Pts',(19.9707776691004,17.4928250197387,2.02948933428373));
#182536=CARTESIAN_POINT('Ctrl Pts',(20.0055339930903,17.5180290960197,2.02693416356667));
#182537=CARTESIAN_POINT('Ctrl Pts',(20.0337452836321,17.5395899038462,2.02486821527087));
#182538=CARTESIAN_POINT('Ctrl Pts',(20.1223163602661,17.6108809289267,2.01836096441317));
#182539=CARTESIAN_POINT('Ctrl Pts',(20.180471695445,17.6632516697405,2.01405444907915));
#182540=CARTESIAN_POINT('Ctrl Pts',(20.3685245510814,17.8524794553587,1.99950158846896));
#182541=CARTESIAN_POINT('Ctrl Pts',(20.4829689215705,18.0033781368208,1.98943100879019));
#182542=CARTESIAN_POINT('Ctrl Pts',(20.5866623369713,18.1863993984059,1.97719285653013));
#182543=CARTESIAN_POINT('Ctrl Pts',(20.5971134214388,18.2055287401437,1.9759148084833));
#182544=CARTESIAN_POINT('Ctrl Pts',(20.6111846233546,18.2322571252334,1.97412909782014));
#182545=CARTESIAN_POINT('Ctrl Pts',(20.6150578370876,18.2397219062003,1.97363038583349));
#182546=CARTESIAN_POINT('Ctrl Pts',(20.6216476391332,18.2526095910884,1.97276930173931));
#182547=CARTESIAN_POINT('Ctrl Pts',(20.6243856087345,18.2580214931434,1.97240768572763));
#182548=CARTESIAN_POINT('Ctrl Pts',(20.6299899663207,18.2692183221425,1.97165944714882));
#182549=CARTESIAN_POINT('Ctrl Pts',(20.6328532201495,18.2750047393109,1.97127271973035));
#182550=CARTESIAN_POINT('Ctrl Pts',(20.6394677986218,18.2885275655266,1.97036879242577));
#182551=CARTESIAN_POINT('Ctrl Pts',(20.6431985299606,18.2962738695449,1.96985088210365));
#182552=CARTESIAN_POINT('Ctrl Pts',(20.655041264629,18.321251617166,1.96818041075684));
#182553=CARTESIAN_POINT('Ctrl Pts',(20.6629677837243,18.3385695000105,1.96702147309343));
#182554=CARTESIAN_POINT('Ctrl Pts',(20.7016803305764,18.4262563710278,1.96114803843375));
#182555=CARTESIAN_POINT('Ctrl Pts',(20.7288509626346,18.4981495322422,1.9563123883028));
#182556=CARTESIAN_POINT('Ctrl Pts',(20.7863169013329,18.6794517145641,1.94407896681212));
#182557=CARTESIAN_POINT('Ctrl Pts',(20.8118368066024,18.7901214493379,1.93657050814318));
#182558=CARTESIAN_POINT('Ctrl Pts',(20.838684788936,18.9722663393065,1.92441465085685));
#182559=CARTESIAN_POINT('Ctrl Pts',(20.8454862070558,19.0427177893555,1.91976443922954));
#182560=CARTESIAN_POINT('Ctrl Pts',(20.8507833979373,19.1574721367558,1.91238827195877));
#182561=CARTESIAN_POINT('Ctrl Pts',(20.8514394498415,19.201619973507,1.90959840157073));
#182562=CARTESIAN_POINT('Ctrl Pts',(20.850590709431,19.2533051170209,1.90641237483187));
#182563=CARTESIAN_POINT('Ctrl Pts',(20.8504264467416,19.260850312004,1.90594927201401));
#182564=CARTESIAN_POINT('Ctrl Pts',(20.8500975219409,19.2729782457116,1.90520829232597));
#182565=CARTESIAN_POINT('Ctrl Pts',(20.8499583145524,19.2775615301487,1.90492904820232));
#182566=CARTESIAN_POINT('Ctrl Pts',(20.8496838918709,19.2857227468474,1.90443324652));
#182567=CARTESIAN_POINT('Ctrl Pts',(20.8495544901033,19.2893008258325,1.90421636759464));
#182568=CARTESIAN_POINT('Ctrl Pts',(20.8492590293721,19.296934347474,1.90375473807953));
#182569=CARTESIAN_POINT('Ctrl Pts',(20.8490903856668,19.3009896355848,1.90351013370199));
#182570=CARTESIAN_POINT('Ctrl Pts',(20.8485987210255,19.3120463909267,1.90284489049644));
#182571=CARTESIAN_POINT('Ctrl Pts',(20.8482525878264,19.3190468513378,1.90242552717083));
#182572=CARTESIAN_POINT('Ctrl Pts',(20.8462782661088,19.3553234555422,1.90026125721361));
#182573=CARTESIAN_POINT('Ctrl Pts',(20.8440766601191,19.3845667511332,1.89854659067145));
#182574=CARTESIAN_POINT('Ctrl Pts',(20.8357346925322,19.4712656403498,1.89352746604681));
#182575=CARTESIAN_POINT('Ctrl Pts',(20.8278489853177,19.5285284139365,1.89029647469377));
#182576=CARTESIAN_POINT('Ctrl Pts',(20.788742703519,19.7461643735881,1.87810454699388));
#182577=CARTESIAN_POINT('Ctrl Pts',(20.741348770102,19.903041153496,1.86945634464088));
#182578=CARTESIAN_POINT('Ctrl Pts',(20.6682810631338,20.0716168596661,1.85913538181585));
#182579=CARTESIAN_POINT('Ctrl Pts',(20.6599039307459,20.0902034043091,1.85798332696463));
#182580=CARTESIAN_POINT('Ctrl Pts',(20.6312618117153,20.1513780538946,1.85414006252209));
#182581=CARTESIAN_POINT('Ctrl Pts',(20.6098433056162,20.1934075884302,1.85141553414203));
#182582=CARTESIAN_POINT('Ctrl Pts',(20.5810086876706,20.2456030633377,1.84790785791638));
#182583=CARTESIAN_POINT('Ctrl Pts',(20.5748807369915,20.2564676911074,1.84717076020984));
#182584=CARTESIAN_POINT('Ctrl Pts',(20.56499553434,20.2736373846039,1.84599450959108));
#182585=CARTESIAN_POINT('Ctrl Pts',(20.5613008304095,20.2799782649969,1.84555761732416));
#182586=CARTESIAN_POINT('Ctrl Pts',(20.5543409904014,20.2917812792063,1.84473964862079));
#182587=CARTESIAN_POINT('Ctrl Pts',(20.5510840430924,20.2972481639976,1.84435887347424));
#182588=CARTESIAN_POINT('Ctrl Pts',(20.5437773004826,20.3093879325525,1.84350901728435));
#182589=CARTESIAN_POINT('Ctrl Pts',(20.5397151630692,20.3160532453395,1.84303948746125));
#182590=CARTESIAN_POINT('Ctrl Pts',(20.5277474085598,20.3354482094954,1.84166459699428));
#182591=CARTESIAN_POINT('Ctrl Pts',(20.5197435074365,20.348116374469,1.84075562142775));
#182592=CARTESIAN_POINT('Ctrl Pts',(20.4518211010642,20.4531346031113,1.83312694610929));
#182593=CARTESIAN_POINT('Ctrl Pts',(20.3849269097415,20.5407523968702,1.82614110006005));
#182594=CARTESIAN_POINT('Ctrl Pts',(20.2087744242698,20.737589066304,1.80894051006129));
#182595=CARTESIAN_POINT('Ctrl Pts',(20.093790390985,20.8408471399132,1.79858371413249));
#182596=CARTESIAN_POINT('Ctrl Pts',(19.9303629427929,20.9581756585949,1.78563722283704));
#182597=CARTESIAN_POINT('Ctrl Pts',(19.8911957173415,20.9843600557152,1.78265478097309));
#182598=CARTESIAN_POINT('Ctrl Pts',(19.8446510339292,21.0132770160377,1.77927640763443));
#182599=CARTESIAN_POINT('Ctrl Pts',(19.8380954080138,21.0173004998691,1.77880430422388));
#182600=CARTESIAN_POINT('Ctrl Pts',(19.8275603628862,21.0236875493102,1.77805175554134));
#182601=CARTESIAN_POINT('Ctrl Pts',(19.8235949394439,21.0260739069185,1.77776987540688));
#182602=CARTESIAN_POINT('Ctrl Pts',(19.8165433605853,21.0302860494207,1.77727110927092));
#182603=CARTESIAN_POINT('Ctrl Pts',(19.8134603555851,21.0321170194716,1.77705388761988));
#182604=CARTESIAN_POINT('Ctrl Pts',(19.8068995904272,21.0359908866476,1.77659343174892));
#182605=CARTESIAN_POINT('Ctrl Pts',(19.8034206477541,21.0380316763177,1.77635033394191));
#182606=CARTESIAN_POINT('Ctrl Pts',(19.7939794401185,21.043533796457,1.77569343488257));
#182607=CARTESIAN_POINT('Ctrl Pts',(19.7880060051588,21.0469760000352,1.77528085567321));
#182608=CARTESIAN_POINT('Ctrl Pts',(19.7578040861663,21.0641839354206,1.77320957268517));
#182609=CARTESIAN_POINT('Ctrl Pts',(19.7333210628913,21.077500224425,1.7715780985201));
#182610=CARTESIAN_POINT('Ctrl Pts',(19.6610868310265,21.1149593768655,1.76688117621785));
#182611=CARTESIAN_POINT('Ctrl Pts',(19.6126727537498,21.1377813258652,1.76387848682696));
#182612=CARTESIAN_POINT('Ctrl Pts',(19.4338614638177,21.2139276885613,1.75312847144989));
#182613=CARTESIAN_POINT('Ctrl Pts',(19.2990960428324,21.256041328324,1.74564122025373));
#182614=CARTESIAN_POINT('Ctrl Pts',(19.0716516178646,21.302896039203,1.73279280139117));
#182615=CARTESIAN_POINT('Ctrl Pts',(18.9810702371879,21.3155168090212,1.72762832630728));
#182616=CARTESIAN_POINT('Ctrl Pts',(18.8762502781846,21.3232601501756,1.72146648929322));
#182617=CARTESIAN_POINT('Ctrl Pts',(18.8625275804191,21.3241395437659,1.72065630407728));
#182618=CARTESIAN_POINT('Ctrl Pts',(18.8405123634133,21.3253351112831,1.71935053622582));
#182619=CARTESIAN_POINT('Ctrl Pts',(18.8322247188535,21.3257363306046,1.71885761924));
#182620=CARTESIAN_POINT('Ctrl Pts',(18.8175087545359,21.3263620634427,1.71797987500258));
#182621=CARTESIAN_POINT('Ctrl Pts',(18.8110813339525,21.3266060214707,1.7175956623554));
#182622=CARTESIAN_POINT('Ctrl Pts',(18.7976905510128,21.3270531758071,1.71679340046814));
#182623=CARTESIAN_POINT('Ctrl Pts',(18.7907271070015,21.3272512995053,1.71637519683166));
#182624=CARTESIAN_POINT('Ctrl Pts',(18.7726478169181,21.327676394513,1.71528672090801));
#182625=CARTESIAN_POINT('Ctrl Pts',(18.7615310417624,21.3278501711727,1.71461479001464));
#182626=CARTESIAN_POINT('Ctrl Pts',(18.7133131946029,21.3282240262187,1.71168858940707));
#182627=CARTESIAN_POINT('Ctrl Pts',(18.6762136545317,21.3275363181911,1.70940674227916));
#182628=CARTESIAN_POINT('Ctrl Pts',(18.5777708330888,21.3231213996842,1.70326734249333));
#182629=CARTESIAN_POINT('Ctrl Pts',(18.516542549804,21.3176977726179,1.69936055696257));
#182630=CARTESIAN_POINT('Ctrl Pts',(18.36174033495,21.2971649520164,1.68927415811314));
#182631=CARTESIAN_POINT('Ctrl Pts',(18.2687866912904,21.2784225407487,1.68301718166094));
#182632=CARTESIAN_POINT('Ctrl Pts',(18.0583073335769,21.2210662665182,1.66860237089002));
#182633=CARTESIAN_POINT('Ctrl Pts',(17.9422606745775,21.1782526002636,1.66046638293103));
#182634=CARTESIAN_POINT('Ctrl Pts',(17.8220625072784,21.1215360673019,1.65225851978827));
#182635=CARTESIAN_POINT('Ctrl Pts',(17.8135548442014,21.1174518818586,1.65167887829982));
#182636=CARTESIAN_POINT('Ctrl Pts',(17.8009689142666,21.1113059935614,1.65082364741596));
#182637=CARTESIAN_POINT('Ctrl Pts',(17.7968696879234,21.1092878220127,1.65054545915621));
#182638=CARTESIAN_POINT('Ctrl Pts',(17.7895785896349,21.10566882322,1.65005134398387));
#182639=CARTESIAN_POINT('Ctrl Pts',(17.7863842100186,21.104073180113,1.64983509944681));
#182640=CARTESIAN_POINT('Ctrl Pts',(17.7795884741099,21.1006570911798,1.64937557413273));
#182641=CARTESIAN_POINT('Ctrl Pts',(17.775988293417,21.0988344349209,1.64913243477582));
#182642=CARTESIAN_POINT('Ctrl Pts',(17.7661608853262,21.0938237806574,1.64846950909021));
#182643=CARTESIAN_POINT('Ctrl Pts',(17.7599441495859,21.0906151585597,1.64805099729787));
#182644=CARTESIAN_POINT('Ctrl Pts',(17.746084520927,21.0833746079779,1.6471196134722));
#182645=CARTESIAN_POINT('Ctrl Pts',(17.738450134856,21.0793265608257,1.64660770179372));
#182646=CARTESIAN_POINT('Ctrl Pts',(17.7149891599453,21.0667020056668,1.64503739217747));
#182647=CARTESIAN_POINT('Ctrl Pts',(17.6992466078717,21.0579700829618,1.64398769200332));
#182648=CARTESIAN_POINT('Ctrl Pts',(17.6390698668063,21.0235808963217,1.63998321147129));
#182649=CARTESIAN_POINT('Ctrl Pts',(17.595460012099,20.9965108250675,1.63709810804985));
#182650=CARTESIAN_POINT('Ctrl Pts',(17.4394665069196,20.8916386457181,1.62668254710155));
#182651=CARTESIAN_POINT('Ctrl Pts',(17.3337055116919,20.8045937384282,1.61941161073459));
#182652=CARTESIAN_POINT('Ctrl Pts',(17.1675665894962,20.6384580563916,1.60645461422335));
#182653=CARTESIAN_POINT('Ctrl Pts',(17.1029964524114,20.5642087881035,1.60091752310745));
#182654=CARTESIAN_POINT('Ctrl Pts',(17.0354275830518,20.4746198254017,1.59434067433861));
#182655=CARTESIAN_POINT('Ctrl Pts',(17.0271440165423,20.4634080631506,1.59351950248195));
#182656=CARTESIAN_POINT('Ctrl Pts',(17.0140749827288,20.4453486965718,1.59219940498084));
#182657=CARTESIAN_POINT('Ctrl Pts',(17.0092181867436,20.4385530389244,1.59170324014818));
#182658=CARTESIAN_POINT('Ctrl Pts',(17.000687933655,20.4264668905444,1.59082174746918));
#182659=CARTESIAN_POINT('Ctrl Pts',(16.9969981445197,20.4211880159669,1.59043705228111));
#182660=CARTESIAN_POINT('Ctrl Pts',(16.9893818306756,20.4101849841693,1.58963582355046));
#182661=CARTESIAN_POINT('Ctrl Pts',(16.9854592604967,20.4044581951228,1.58921914573037));
#182662=CARTESIAN_POINT('Ctrl Pts',(16.9753906772944,20.389602292374,1.58813905962648));
#182663=CARTESIAN_POINT('Ctrl Pts',(16.9692876168749,20.3804444455288,1.58747404038014));
#182664=CARTESIAN_POINT('Ctrl Pts',(16.9434955384188,20.3410808854293,1.58461862004461));
#182665=CARTESIAN_POINT('Ctrl Pts',(16.9245094793968,20.3104238670881,1.58240226714949));
#182666=CARTESIAN_POINT('Ctrl Pts',(16.8765249250203,20.22833015227,1.57648309716843));
#182667=CARTESIAN_POINT('Ctrl Pts',(16.8488808830936,20.1761420687189,1.57273531387891));
#182668=CARTESIAN_POINT('Ctrl Pts',(16.7944884861391,20.0621795251588,1.564593524878));
#182669=CARTESIAN_POINT('Ctrl Pts',(16.7684510840594,20.0001866912494,1.56018933018398));
#182670=CARTESIAN_POINT('Ctrl Pts',(16.7454191763733,19.9371097078984,1.5557606494604));
#182671=CARTESIAN_POINT('',(16.6200798910611,19.2101717422182,2.08900081352829));
#182672=CARTESIAN_POINT('Ctrl Pts',(16.7454193623274,19.9371102171666,1.33163196712539));
#182673=CARTESIAN_POINT('Ctrl Pts',(16.7469780041856,19.9413788322432,1.33190185517408));
#182674=CARTESIAN_POINT('Ctrl Pts',(16.7485503803193,19.9456424013342,1.33217219827261));
#182675=CARTESIAN_POINT('Ctrl Pts',(16.7523808360471,19.9559267329139,1.33282619370626));
#182676=CARTESIAN_POINT('Ctrl Pts',(16.7546526297506,19.9619422979385,1.33321030082241));
#182677=CARTESIAN_POINT('Ctrl Pts',(16.759443395003,19.9744551546147,1.33401258917509));
#182678=CARTESIAN_POINT('Ctrl Pts',(16.7619671077401,19.9809505370368,1.33443092601526));
#182679=CARTESIAN_POINT('Ctrl Pts',(16.7686050697039,19.9977881906055,1.33552028771208));
#182680=CARTESIAN_POINT('Ctrl Pts',(16.7727688570567,20.0081105854564,1.33619297680958));
#182681=CARTESIAN_POINT('Ctrl Pts',(16.7912114292745,20.0528119494043,1.33912754783629));
#182682=CARTESIAN_POINT('Ctrl Pts',(16.8063135111907,20.0868420597437,1.34141720810393));
#182683=CARTESIAN_POINT('Ctrl Pts',(16.8488256597736,20.1762036238896,1.34758320436534));
#182684=CARTESIAN_POINT('Ctrl Pts',(16.877770903168,20.2307611200909,1.35150931277073));
#182685=CARTESIAN_POINT('Ctrl Pts',(16.9832811391662,20.4102161226008,1.36495842821662));
#182686=CARTESIAN_POINT('Ctrl Pts',(17.0704045123377,20.5284143929022,1.37476374100119));
#182687=CARTESIAN_POINT('Ctrl Pts',(17.182161885078,20.6510932466381,1.38559625206135));
#182688=CARTESIAN_POINT('Ctrl Pts',(17.1955077083043,20.6653423239262,1.3868650160503));
#182689=CARTESIAN_POINT('Ctrl Pts',(17.2456814512456,20.7174481782719,1.39153841104537));
#182690=CARTESIAN_POINT('Ctrl Pts',(17.2837281587797,20.7541107583554,1.39489464216723));
#182691=CARTESIAN_POINT('Ctrl Pts',(17.3295906043271,20.7951082083525,1.3986891934953));
#182692=CARTESIAN_POINT('Ctrl Pts',(17.3361072826995,20.8008617937687,1.39922271671008));
#182693=CARTESIAN_POINT('Ctrl Pts',(17.34603362632,20.8095175597638,1.40002662392817));
#182694=CARTESIAN_POINT('Ctrl Pts',(17.3494172701489,20.8124492525178,1.40029912943583));
#182695=CARTESIAN_POINT('Ctrl Pts',(17.3555106790092,20.8176950205516,1.4007870939087));
#182696=CARTESIAN_POINT('Ctrl Pts',(17.3582169959057,20.8200129966446,1.40100283890852));
#182697=CARTESIAN_POINT('Ctrl Pts',(17.3641139352505,20.8250380035355,1.40147081003789));
#182698=CARTESIAN_POINT('Ctrl Pts',(17.3673067240393,20.8277424029174,1.40172284349725));
#182699=CARTESIAN_POINT('Ctrl Pts',(17.3763062231989,20.8353195711663,1.40242955688792));
#182700=CARTESIAN_POINT('Ctrl Pts',(17.3821311849721,20.8401707006116,1.40288268092881));
#182701=CARTESIAN_POINT('Ctrl Pts',(17.417289729973,20.8691329421873,1.40559281767779));
#182702=CARTESIAN_POINT('Ctrl Pts',(17.4472435951132,20.8924842096638,1.40779849604528));
#182703=CARTESIAN_POINT('Ctrl Pts',(17.5483186695137,20.9669959259958,1.41496681029301));
#182704=CARTESIAN_POINT('Ctrl Pts',(17.6219897840333,21.0145513909353,1.41976116469807));
#182705=CARTESIAN_POINT('Ctrl Pts',(17.8507182640593,21.1428388654111,1.43402845752519));
#182706=CARTESIAN_POINT('Ctrl Pts',(18.0130018975068,21.2090848392259,1.44342145627763));
#182707=CARTESIAN_POINT('Ctrl Pts',(18.203829514806,21.260668227523,1.45490743269495));
#182708=CARTESIAN_POINT('Ctrl Pts',(18.2261829610864,21.2663205053858,1.45625813426368));
#182709=CARTESIAN_POINT('Ctrl Pts',(18.2579262484205,21.2737976447255,1.4581853655483));
#182710=CARTESIAN_POINT('Ctrl Pts',(18.2672434705479,21.275925828617,1.4587521460584));
#182711=CARTESIAN_POINT('Ctrl Pts',(18.2824027834644,21.2792805864823,1.45967621913986));
#182712=CARTESIAN_POINT('Ctrl Pts',(18.2882362799591,21.2805456832778,1.46003227186507));
#182713=CARTESIAN_POINT('Ctrl Pts',(18.3004560133001,21.2831416859249,1.46077910482126));
#182714=CARTESIAN_POINT('Ctrl Pts',(18.306843198826,21.2844677766205,1.46117003497336));
#182715=CARTESIAN_POINT('Ctrl Pts',(18.322048551967,21.2875514327962,1.46210207166755));
#182716=CARTESIAN_POINT('Ctrl Pts',(18.3308719352508,21.2892823696739,1.46264402259786));
#182717=CARTESIAN_POINT('Ctrl Pts',(18.3606155230247,21.294920812619,1.46447480700334));
#182718=CARTESIAN_POINT('Ctrl Pts',(18.3815830273768,21.2985689560884,1.46577185151558));
#182719=CARTESIAN_POINT('Ctrl Pts',(18.56002645564,21.3268514647283,1.47686840352228));
#182720=CARTESIAN_POINT('Ctrl Pts',(18.719736661254,21.3339396080834,1.48724143341919));
#182721=CARTESIAN_POINT('Ctrl Pts',(19.009993183724,21.3140540498511,1.50645963799945));
#182722=CARTESIAN_POINT('Ctrl Pts',(19.140175957676,21.2928347141087,1.51519755611925));
#182723=CARTESIAN_POINT('Ctrl Pts',(19.2827889005186,21.2556925418244,1.52439146540134));
#182724=CARTESIAN_POINT('Ctrl Pts',(19.2979796641196,21.2515547823996,1.52536557302689));
#182725=CARTESIAN_POINT('Ctrl Pts',(19.3187008095772,21.2456615412594,1.52668584307872));
#182726=CARTESIAN_POINT('Ctrl Pts',(19.3242717952639,21.2440523440716,1.52703996155975));
#182727=CARTESIAN_POINT('Ctrl Pts',(19.3331111342403,21.2414596762579,1.52760041314962));
#182728=CARTESIAN_POINT('Ctrl Pts',(19.3363837941966,21.240491170947,1.52780760386142));
#182729=CARTESIAN_POINT('Ctrl Pts',(19.3431353897698,21.2384753454715,1.52823438350765));
#182730=CARTESIAN_POINT('Ctrl Pts',(19.3466139729846,21.237426983589,1.5284539042033));
#182731=CARTESIAN_POINT('Ctrl Pts',(19.3548923804098,21.2349088048287,1.5289754838968));
#182732=CARTESIAN_POINT('Ctrl Pts',(19.3596897455866,21.2334308496864,1.52927706824309));
#182733=CARTESIAN_POINT('Ctrl Pts',(19.3758337499603,21.2283943206485,1.53028982671829));
#182734=CARTESIAN_POINT('Ctrl Pts',(19.3871558880309,21.2247571373248,1.53099654832436));
#182735=CARTESIAN_POINT('Ctrl Pts',(19.5221745262441,21.1801244815896,1.53938848306166));
#182736=CARTESIAN_POINT('Ctrl Pts',(19.6418803129861,21.1278811940742,1.54647761906019));
#182737=CARTESIAN_POINT('Ctrl Pts',(19.8981324773847,20.9866162340896,1.56237404472561));
#182738=CARTESIAN_POINT('Ctrl Pts',(20.0307366459323,20.8922151917734,1.57115672268068));
#182739=CARTESIAN_POINT('Ctrl Pts',(20.1688783508615,20.7677196144716,1.58195489211107));
#182740=CARTESIAN_POINT('Ctrl Pts',(20.1862330008015,20.7515424643417,1.5833441127189));
#182741=CARTESIAN_POINT('Ctrl Pts',(20.2102717257774,20.7283675424148,1.5853169836262));
#182742=CARTESIAN_POINT('Ctrl Pts',(20.2171856918803,20.7216100310121,1.58589023946448));
#182743=CARTESIAN_POINT('Ctrl Pts',(20.2283073699279,20.710590061733,1.58682198427699));
#182744=CARTESIAN_POINT('Ctrl Pts',(20.2325437551732,20.7063566403256,1.58717919148745));
#182745=CARTESIAN_POINT('Ctrl Pts',(20.241344768238,20.6974868251186,1.58792612316353));
#182746=CARTESIAN_POINT('Ctrl Pts',(20.2459060943181,20.6928472566641,1.58831598729466));
#182747=CARTESIAN_POINT('Ctrl Pts',(20.2566543318127,20.6818133636003,1.58924124210576));
#182748=CARTESIAN_POINT('Ctrl Pts',(20.2628224252603,20.6754009536247,1.58977744488563));
#182749=CARTESIAN_POINT('Ctrl Pts',(20.2832287128909,20.6539169318808,1.59156905774313));
#182750=CARTESIAN_POINT('Ctrl Pts',(20.2972855530825,20.6386754213347,1.59283220887405));
#182751=CARTESIAN_POINT('Ctrl Pts',(20.3711298304456,20.5562094234078,1.59962720789639));
#182752=CARTESIAN_POINT('Ctrl Pts',(20.4268030090818,20.4854398164007,1.60532705925388));
#182753=CARTESIAN_POINT('Ctrl Pts',(20.5546053111571,20.2997760491549,1.61993439702845));
#182754=CARTESIAN_POINT('Ctrl Pts',(20.6205212450552,20.1810880882199,1.62898763181619));
#182755=CARTESIAN_POINT('Ctrl Pts',(20.7047974341816,19.9877506634228,1.64277917976509));
#182756=CARTESIAN_POINT('Ctrl Pts',(20.7312356335687,19.9170003225781,1.64763729017112));
#182757=CARTESIAN_POINT('Ctrl Pts',(20.7566829070162,19.8359263478053,1.65288547243642));
#182758=CARTESIAN_POINT('Ctrl Pts',(20.7594643792006,19.8268515558295,1.65346848951061));
#182759=CARTESIAN_POINT('Ctrl Pts',(20.7634973726325,19.8133706398942,1.65432771734407));
#182760=CARTESIAN_POINT('Ctrl Pts',(20.764795734358,19.8089788119596,1.65460656180705));
#182761=CARTESIAN_POINT('Ctrl Pts',(20.7670812933886,19.801154395927,1.65510139061855));
#182762=CARTESIAN_POINT('Ctrl Pts',(20.7680740637074,19.7977234958364,1.65531769626575));
#182763=CARTESIAN_POINT('Ctrl Pts',(20.77019076326,19.7903384788437,1.65578184593678));
#182764=CARTESIAN_POINT('Ctrl Pts',(20.7713118568443,19.7863836077578,1.65602952418444));
#182765=CARTESIAN_POINT('Ctrl Pts',(20.77437682753,19.7754500697815,1.65671186730624));
#182766=CARTESIAN_POINT('Ctrl Pts',(20.7762964352237,19.7684645762021,1.65714514397713));
#182767=CARTESIAN_POINT('Ctrl Pts',(20.7866510679994,19.730012410175,1.65951615387513));
#182768=CARTESIAN_POINT('Ctrl Pts',(20.7943952489512,19.6983622573656,1.6614163478016));
#182769=CARTESIAN_POINT('Ctrl Pts',(20.8364044400941,19.507710963868,1.6726249309217));
#182770=CARTESIAN_POINT('Ctrl Pts',(20.8529860108762,19.3453575011157,1.681221689799));
#182771=CARTESIAN_POINT('Ctrl Pts',(20.8492485378129,19.0658729950936,1.69652341869061));
#182772=CARTESIAN_POINT('Ctrl Pts',(20.8380194480306,18.9493989181104,1.70304550621825));
#182773=CARTESIAN_POINT('Ctrl Pts',(20.8147014991038,18.8203921794501,1.71072561347407));
#182774=CARTESIAN_POINT('Ctrl Pts',(20.8120175446922,18.8063566176377,1.71156711398024));
#182775=CARTESIAN_POINT('Ctrl Pts',(20.8075197986346,18.7840619190204,1.71291367999649));
#182776=CARTESIAN_POINT('Ctrl Pts',(20.805798232832,18.7757844676587,1.71341580429983));
#182777=CARTESIAN_POINT('Ctrl Pts',(20.8026745529542,18.7612041759646,1.71430420428939));
#182778=CARTESIAN_POINT('Ctrl Pts',(20.8012930921936,18.7548969865231,1.71468981394865));
#182779=CARTESIAN_POINT('Ctrl Pts',(20.7983761102137,18.7418647756467,1.71548931686087));
#182780=CARTESIAN_POINT('Ctrl Pts',(20.7968365313959,18.7351407496575,1.71590333646829));
#182781=CARTESIAN_POINT('Ctrl Pts',(20.7928002593891,18.7179002940254,1.71696882869623));
#182782=CARTESIAN_POINT('Ctrl Pts',(20.7902558612143,18.7073953390516,1.71762183079105));
#182783=CARTESIAN_POINT('Ctrl Pts',(20.779300133204,18.6636305401481,1.72035839656207));
#182784=CARTESIAN_POINT('Ctrl Pts',(20.7701617750408,18.6305596757707,1.72246530292395));
#182785=CARTESIAN_POINT('Ctrl Pts',(20.7442598257753,18.5449809024626,1.72802300247571));
#182786=CARTESIAN_POINT('Ctrl Pts',(20.7262430089568,18.4928823372306,1.73151223757575));
#182787=CARTESIAN_POINT('Ctrl Pts',(20.6664533522414,18.3396326436658,1.74208588985661));
#182788=CARTESIAN_POINT('Ctrl Pts',(20.6188535678228,18.240958459499,1.7493186861522));
#182789=CARTESIAN_POINT('Ctrl Pts',(20.5394824059182,18.1045327043741,1.75974481558208));
#182790=CARTESIAN_POINT('Ctrl Pts',(20.5136858765388,18.0635005392597,1.76293908883565));
#182791=CARTESIAN_POINT('Ctrl Pts',(20.4766030372342,18.0087790893354,1.76725143628182));
#182792=CARTESIAN_POINT('Ctrl Pts',(20.4665200398357,17.994293462095,1.76839814769748));
#182793=CARTESIAN_POINT('Ctrl Pts',(20.4252329219593,17.9365328701719,1.77298682028713));
#182794=CARTESIAN_POINT('Ctrl Pts',(20.3925763983772,17.8943145292206,1.77637830339518));
#182795=CARTESIAN_POINT('Ctrl Pts',(20.3527644106781,17.8466808199386,1.78020788810544));
#182796=CARTESIAN_POINT('Ctrl Pts',(20.3471307456209,17.8400243452549,1.78074310877312));
#182797=CARTESIAN_POINT('Ctrl Pts',(20.3385386644697,17.8299986339549,1.78154907971394));
#182798=CARTESIAN_POINT('Ctrl Pts',(20.3356104914802,17.8266037658125,1.78182196699794));
#182799=CARTESIAN_POINT('Ctrl Pts',(20.3303352479972,17.8205268872433,1.78231034977937));
#182800=CARTESIAN_POINT('Ctrl Pts',(20.3279921801335,17.8178414908725,1.78252613341665));
#182801=CARTESIAN_POINT('Ctrl Pts',(20.3228863945425,17.8120194799911,1.78299387854626));
#182802=CARTESIAN_POINT('Ctrl Pts',(20.3201211746278,17.8088851365821,1.78324564903745));
#182803=CARTESIAN_POINT('Ctrl Pts',(20.3123283672193,17.8001046388885,1.78395089557332));
#182804=CARTESIAN_POINT('Ctrl Pts',(20.3072797334942,17.7944771308379,1.78440282600401));
#182805=CARTESIAN_POINT('Ctrl Pts',(20.276929880101,17.7610098010537,1.787090943966));
#182806=CARTESIAN_POINT('Ctrl Pts',(20.2509187004627,17.7338194959622,1.78927676090886));
#182807=CARTESIAN_POINT('Ctrl Pts',(20.1629633807314,17.6466520905559,1.7963483171119));
#182808=CARTESIAN_POINT('Ctrl Pts',(20.0980772765486,17.5897608879431,1.80107091205644));
#182809=CARTESIAN_POINT('Ctrl Pts',(19.8902343793694,17.4288646978125,1.81537503209623));
#182810=CARTESIAN_POINT('Ctrl Pts',(19.7376080142937,17.3386622944883,1.82486499111222));
#182811=CARTESIAN_POINT('Ctrl Pts',(19.5545392181901,17.2593521993591,1.83645920381707));
#182812=CARTESIAN_POINT('Ctrl Pts',(19.5333738500598,17.2505880193407,1.83780131860654));
#182813=CARTESIAN_POINT('Ctrl Pts',(19.5032057589267,17.2386657565649,1.83971837261292));
#182814=CARTESIAN_POINT('Ctrl Pts',(19.494317047693,17.2352222164772,1.84028370317441));
#182815=CARTESIAN_POINT('Ctrl Pts',(19.4798294268298,17.2297218670089,1.84120604387949));
#182816=CARTESIAN_POINT('Ctrl Pts',(19.474244484625,17.227628457385,1.84156182335105));
#182817=CARTESIAN_POINT('Ctrl Pts',(19.4625295139323,17.2232936967814,1.84230859841604));
#182818=CARTESIAN_POINT('Ctrl Pts',(19.4563978257604,17.2210570409227,1.84269974619969));
#182819=CARTESIAN_POINT('Ctrl Pts',(19.4417752064424,17.215799639779,1.84363325416427));
#182820=CARTESIAN_POINT('Ctrl Pts',(19.4332751880835,17.2128047073207,1.84417646599856));
#182821=CARTESIAN_POINT('Ctrl Pts',(19.4045223054752,17.202879724896,1.84601604998599));
#182822=CARTESIAN_POINT('Ctrl Pts',(19.3841840465882,17.1962027759157,1.84732074175406));
#182823=CARTESIAN_POINT('Ctrl Pts',(19.2725582188344,17.1614227213189,1.85450262999146));
#182824=CARTESIAN_POINT('Ctrl Pts',(19.1795617834052,17.1392175769133,1.86057000651584));
#182825=CARTESIAN_POINT('Ctrl Pts',(18.9174228140019,17.0950938246616,1.87784603494144));
#182826=CARTESIAN_POINT('Ctrl Pts',(18.7466635818049,17.0871969393988,1.88933835478954));
#182827=CARTESIAN_POINT('Ctrl Pts',(18.5401924715562,17.1025703036216,1.90255195357782));
#182828=CARTESIAN_POINT('Ctrl Pts',(18.5036512627533,17.1062489512997,1.90486145989074));
#182829=CARTESIAN_POINT('Ctrl Pts',(18.4601412063994,17.1117760230161,1.90756232652012));
#182830=CARTESIAN_POINT('Ctrl Pts',(18.4530650517299,17.1127112919025,1.90800001532627));
#182831=CARTESIAN_POINT('Ctrl Pts',(18.441524560895,17.1142960469123,1.90871114363025));
#182832=CARTESIAN_POINT('Ctrl Pts',(18.4370573982327,17.1149240372782,1.90898575073626));
#182833=CARTESIAN_POINT('Ctrl Pts',(18.4290626635575,17.1160740021586,1.90947598072661));
#182834=CARTESIAN_POINT('Ctrl Pts',(18.4255343847336,17.1165906129906,1.90969190133198));
#182835=CARTESIAN_POINT('Ctrl Pts',(18.4178938842344,17.1177290620179,1.91015854020462));
#182836=CARTESIAN_POINT('Ctrl Pts',(18.4137821975803,17.1183541016403,1.91040907503212));
#182837=CARTESIAN_POINT('Ctrl Pts',(18.4022961757809,17.1201347990691,1.91110737980264));
#182838=CARTESIAN_POINT('Ctrl Pts',(18.3949259874871,17.1213173606338,1.91155365266393));
#182839=CARTESIAN_POINT('Ctrl Pts',(18.3520505285585,17.1284296236444,1.91414009184981));
#182840=CARTESIAN_POINT('Ctrl Pts',(18.3166925806269,17.1352255332595,1.91623421947737));
#182841=CARTESIAN_POINT('Ctrl Pts',(18.2033482143863,17.1600242560738,1.92287118862285));
#182842=CARTESIAN_POINT('Ctrl Pts',(18.1261998397853,17.1815484026885,1.9272729718461));
#182843=CARTESIAN_POINT('Ctrl Pts',(17.8746285671835,17.2673742539128,1.94176382115605));
#182844=CARTESIAN_POINT('Ctrl Pts',(17.707486886663,17.3502299638787,1.95169903594166));
#182845=CARTESIAN_POINT('Ctrl Pts',(17.5349726967251,17.4661474885047,1.96378739445251));
#182846=CARTESIAN_POINT('Ctrl Pts',(17.5168356724065,17.4787506800756,1.96508206419694));
#182847=CARTESIAN_POINT('Ctrl Pts',(17.4920322842555,17.4965681147022,1.96688733410905));
#182848=CARTESIAN_POINT('Ctrl Pts',(17.4851946321198,17.5015422946797,1.96738872126685));
#182849=CARTESIAN_POINT('Ctrl Pts',(17.4734942106061,17.5101616518994,1.9682531929688));
#182850=CARTESIAN_POINT('Ctrl Pts',(17.4686169667912,17.5137870759543,1.96861550756697));
#182851=CARTESIAN_POINT('Ctrl Pts',(17.45876165597,17.5211789642441,1.96935165781247));
#182852=CARTESIAN_POINT('Ctrl Pts',(17.4537845054486,17.5249465449805,1.96972553503268));
#182853=CARTESIAN_POINT('Ctrl Pts',(17.4422554560339,17.5337542330438,1.97059653048465));
#182854=CARTESIAN_POINT('Ctrl Pts',(17.4357163019506,17.5388107864266,1.97109429575));
#182855=CARTESIAN_POINT('Ctrl Pts',(17.4220322084014,17.5495209824846,1.97214392175216));
#182856=CARTESIAN_POINT('Ctrl Pts',(17.4148938318021,17.5551827018701,1.97269609907122));
#182857=CARTESIAN_POINT('Ctrl Pts',(17.3959866774258,17.5703785478384,1.9741711358098));
#182858=CARTESIAN_POINT('Ctrl Pts',(17.3842834573516,17.5799930605662,1.97509721038692));
#182859=CARTESIAN_POINT('Ctrl Pts',(17.3489064523796,17.6096977509895,1.97793713997375));
#182860=CARTESIAN_POINT('Ctrl Pts',(17.3255714093268,17.6301831934223,1.97986683265445));
#182861=CARTESIAN_POINT('Ctrl Pts',(17.1785843790634,17.7650591581541,1.99239369235755));
#182862=CARTESIAN_POINT('Ctrl Pts',(17.068523564442,17.8933376442339,2.00358053853695));
#182863=CARTESIAN_POINT('Ctrl Pts',(16.9197543474234,18.1155517291386,2.02119661537595));
#182864=CARTESIAN_POINT('Ctrl Pts',(16.8705008590982,18.2016091889806,2.02764871574891));
#182865=CARTESIAN_POINT('Ctrl Pts',(16.8232353237548,18.2995388988549,2.03436713610169));
#182866=CARTESIAN_POINT('Ctrl Pts',(16.8190812869895,18.3082988768957,2.03496280913001));
#182867=CARTESIAN_POINT('Ctrl Pts',(16.8130369074776,18.3212746848877,2.0358370156457));
#182868=CARTESIAN_POINT('Ctrl Pts',(16.8111000197744,18.3254685176871,2.03611831500184));
#182869=CARTESIAN_POINT('Ctrl Pts',(16.8076882727686,18.3329197560845,2.03661584871558));
#182870=CARTESIAN_POINT('Ctrl Pts',(16.8062079246754,18.3361745887213,2.03683241795747));
#182871=CARTESIAN_POINT('Ctrl Pts',(16.8030539896857,18.3431560089453,2.03729530481816));
#182872=CARTESIAN_POINT('Ctrl Pts',(16.8013829450984,18.3468836841543,2.03754146625164));
#182873=CARTESIAN_POINT('Ctrl Pts',(16.7968258179881,18.3571288185767,2.03821535470679));
#182874=CARTESIAN_POINT('Ctrl Pts',(16.7939618142309,18.3636561223642,2.03864174979378));
#182875=CARTESIAN_POINT('Ctrl Pts',(16.778851067992,18.3985730221803,2.04090763423713));
#182876=CARTESIAN_POINT('Ctrl Pts',(16.7671937061721,18.4272154823405,2.04271340093821));
#182877=CARTESIAN_POINT('Ctrl Pts',(16.7338151901355,18.5146675025509,2.04809760755346));
#182878=CARTESIAN_POINT('Ctrl Pts',(16.714073416347,18.5741986452579,2.05158934566686));
#182879=CARTESIAN_POINT('Ctrl Pts',(16.6439835858626,18.8218627412806,2.06573526308096));
#182880=CARTESIAN_POINT('Ctrl Pts',(16.6170670028706,19.0155969299278,2.07601658232645));
#182881=CARTESIAN_POINT('Ctrl Pts',(16.6170001249202,19.210272736479,2.08722594468162));
#182882=CARTESIAN_POINT('Ctrl Pts',(16.7452305776443,19.937179123763,2.13351566305583));
#182883=CARTESIAN_POINT('Ctrl Pts',(16.6631152304279,19.7049844831246,2.11869586837805));
#182884=CARTESIAN_POINT('Ctrl Pts',(16.6210475619504,19.4574404220335,2.10387607370028));
#182885=CARTESIAN_POINT('Ctrl Pts',(16.6201761352154,19.2101685860996,2.0890562790225));
#182886=CARTESIAN_POINT('Origin',(18.734,19.211,0.));
#182887=CARTESIAN_POINT('',(16.7454192904825,19.9371100204066,3.1547244898053));
#182888=CARTESIAN_POINT('',(16.7454193815904,19.9371102699217,2.93545674419276));
#182889=CARTESIAN_POINT('',(16.7454193623258,19.9371102171621,0.));
#182890=CARTESIAN_POINT('',(16.6170000449367,19.2105638097622,3.11292712502269));
#182891=CARTESIAN_POINT('Ctrl Pts',(16.7454192904822,19.9371100204058,3.15472448980525));
#182892=CARTESIAN_POINT('Ctrl Pts',(16.6825886116752,19.7650370943612,3.14472559793947));
#182893=CARTESIAN_POINT('Ctrl Pts',(16.6422996596358,19.5853832163324,3.13494345425051));
#182894=CARTESIAN_POINT('Ctrl Pts',(16.6232302297006,19.3755532516873,3.1227499899056));
#182895=CARTESIAN_POINT('Ctrl Pts',(16.6212927655662,19.3484584959526,3.1211629789051));
#182896=CARTESIAN_POINT('Ctrl Pts',(16.6193445971681,19.3111296954677,3.11895643238462));
#182897=CARTESIAN_POINT('Ctrl Pts',(16.6188859031343,19.3009209671181,3.11835092389697));
#182898=CARTESIAN_POINT('Ctrl Pts',(16.6182717244409,19.2846205874733,3.11738067097006));
#182899=CARTESIAN_POINT('Ctrl Pts',(16.6180685939078,19.2785308108873,3.11701742332083));
#182900=CARTESIAN_POINT('Ctrl Pts',(16.6177137006786,19.2663076837147,3.11628676152292));
#182901=CARTESIAN_POINT('Ctrl Pts',(16.6175623043752,19.2601743823862,3.11591933948709));
#182902=CARTESIAN_POINT('Ctrl Pts',(16.617282543914,19.2464168826775,3.11509337012116));
#182903=CARTESIAN_POINT('Ctrl Pts',(16.6171687079842,19.238792503409,3.11463437185928));
#182904=CARTESIAN_POINT('Ctrl Pts',(16.6170306368109,19.224299891525,3.11375947315431));
#182905=CARTESIAN_POINT('Ctrl Pts',(16.6169986298382,19.217431829944,3.11334382362381));
#182906=CARTESIAN_POINT('Ctrl Pts',(16.6170000449367,19.2105638097622,3.11292712502269));
#182907=CARTESIAN_POINT('Ctrl Pts',(16.6170000447698,19.2105646206611,3.11292717422179));
#182908=CARTESIAN_POINT('Ctrl Pts',(16.6170022358522,19.1999106439826,3.11228077304953));
#182909=CARTESIAN_POINT('Ctrl Pts',(16.6170848523641,19.189256952315,3.11163185797907));
#182910=CARTESIAN_POINT('Ctrl Pts',(16.617578463977,19.1570039612813,3.10965950800197));
#182911=CARTESIAN_POINT('Ctrl Pts',(16.6182396504169,19.135410453098,3.10832836959221));
#182912=CARTESIAN_POINT('Ctrl Pts',(16.6268211686643,18.9486429508904,3.0967206675243));
#182913=CARTESIAN_POINT('Ctrl Pts',(16.653738701196,18.7849385490117,3.08584003822765));
#182914=CARTESIAN_POINT('Ctrl Pts',(16.7229664099705,18.5441422443587,3.06928820566192));
#182915=CARTESIAN_POINT('Ctrl Pts',(16.7514475268371,18.4637096097316,3.06367451624404));
#182916=CARTESIAN_POINT('Ctrl Pts',(16.7992807838426,18.3507981705593,3.05584845144454));
#182917=CARTESIAN_POINT('Ctrl Pts',(16.8147682333084,18.3167766190301,3.05349838712842));
#182918=CARTESIAN_POINT('Ctrl Pts',(16.8344565103413,18.2763982294107,3.05073418849401));
#182919=CARTESIAN_POINT('Ctrl Pts',(16.8377998991885,18.269633376248,3.05027194497506));
#182920=CARTESIAN_POINT('Ctrl Pts',(16.8430499687137,18.2591521007839,3.04955726673714));
#182921=CARTESIAN_POINT('Ctrl Pts',(16.8449315586639,18.2554232795284,3.04930331101138));
#182922=CARTESIAN_POINT('Ctrl Pts',(16.8484392813086,18.2485227380709,3.04883392980308));
#182923=CARTESIAN_POINT('Ctrl Pts',(16.8500623741091,18.2453495841412,3.04861832422634));
#182924=CARTESIAN_POINT('Ctrl Pts',(16.8537470662463,18.2381906451431,3.04813241718085));
#182925=CARTESIAN_POINT('Ctrl Pts',(16.8558133232472,18.2342073178473,3.04786241320548));
#182926=CARTESIAN_POINT('Ctrl Pts',(16.8619409706261,18.2224857795106,3.04706886341686));
#182927=CARTESIAN_POINT('Ctrl Pts',(16.8660376864509,18.21476600405,3.04654749332886));
#182928=CARTESIAN_POINT('Ctrl Pts',(16.8957248933654,18.1596509685486,3.04283265561891));
#182929=CARTESIAN_POINT('Ctrl Pts',(16.9230704567465,18.113217968088,3.03974256746979));
#182930=CARTESIAN_POINT('Ctrl Pts',(17.0431963457532,17.9259724041349,3.02723686434036));
#182931=CARTESIAN_POINT('Ctrl Pts',(17.1508610506887,17.7954464955516,3.01836477575473));
#182932=CARTESIAN_POINT('Ctrl Pts',(17.3157914500564,17.6381394297858,3.0057328892593));
#182933=CARTESIAN_POINT('Ctrl Pts',(17.3604032780398,17.5990331474007,3.00239916825214));
#182934=CARTESIAN_POINT('Ctrl Pts',(17.4347742939646,17.5391716443286,2.99691537414576));
#182935=CARTESIAN_POINT('Ctrl Pts',(17.4635284852218,17.5172174322036,2.99481187324192));
#182936=CARTESIAN_POINT('Ctrl Pts',(17.49944302071,17.4912253906929,2.99219808287639));
#182937=CARTESIAN_POINT('Ctrl Pts',(17.5060838158974,17.4864776070072,2.99171533769635));
#182938=CARTESIAN_POINT('Ctrl Pts',(17.5189478807948,17.4773925222532,2.99078117999397));
#182939=CARTESIAN_POINT('Ctrl Pts',(17.5251673367488,17.473050021074,2.99032997530338));
#182940=CARTESIAN_POINT('Ctrl Pts',(17.5314512392659,17.4687125723419,2.98987449873408));
#182941=CARTESIAN_POINT('Ctrl Pts',(17.5314925441408,17.468684063919,2.98987150484728));
#182942=CARTESIAN_POINT('Ctrl Pts',(17.5315768734892,17.4686258646419,2.98986539246833));
#182943=CARTESIAN_POINT('Ctrl Pts',(17.5316198981255,17.4685961738595,2.98986227396587));
#182944=CARTESIAN_POINT('Ctrl Pts',(17.5317077841706,17.4685355295655,2.98985590386711));
#182945=CARTESIAN_POINT('Ctrl Pts',(17.5317526455997,17.4685045762447,2.989852652271));
#182946=CARTESIAN_POINT('Ctrl Pts',(17.5318443334227,17.4684413190506,2.9898460066985));
#182947=CARTESIAN_POINT('Ctrl Pts',(17.5318911599234,17.4684090153321,2.98984261271621));
#182948=CARTESIAN_POINT('Ctrl Pts',(17.5319869188542,17.4683429607958,2.98983567215982));
#182949=CARTESIAN_POINT('Ctrl Pts',(17.532035851442,17.4683092101251,2.98983212557636));
#182950=CARTESIAN_POINT('Ctrl Pts',(17.5321359783802,17.4682401549831,2.9898248685293));
#182951=CARTESIAN_POINT('Ctrl Pts',(17.5321871727421,17.4682048507912,2.98982115806717));
#182952=CARTESIAN_POINT('Ctrl Pts',(17.5322919949396,17.4681325710724,2.98981356082453));
#182953=CARTESIAN_POINT('Ctrl Pts',(17.5323456230126,17.4680955957052,2.98980967402941));
#182954=CARTESIAN_POINT('Ctrl Pts',(17.5324555034409,17.4680198430686,2.98980171029951));
#182955=CARTESIAN_POINT('Ctrl Pts',(17.5325117560146,17.4679810660143,2.98979763335183));
#182956=CARTESIAN_POINT('Ctrl Pts',(17.5326270977567,17.4679015647688,2.98978927393826));
#182957=CARTESIAN_POINT('Ctrl Pts',(17.5326861871207,17.4678608408577,2.98978499146153));
#182958=CARTESIAN_POINT('Ctrl Pts',(17.5328074395509,17.4677772837584,2.98977620381573));
#182959=CARTESIAN_POINT('Ctrl Pts',(17.5328696027798,17.4677344509305,2.98977169863868));
#182960=CARTESIAN_POINT('Ctrl Pts',(17.5329972684181,17.4676464945229,2.9897624463637));
#182961=CARTESIAN_POINT('Ctrl Pts',(17.5330627710907,17.4676013713019,2.98975769925103));
#182962=CARTESIAN_POINT('Ctrl Pts',(17.5331974145518,17.4675086298381,2.9897479414536));
#182963=CARTESIAN_POINT('Ctrl Pts',(17.5332665555702,17.4674610120575,2.98974293075714));
#182964=CARTESIAN_POINT('Ctrl Pts',(17.5334088131685,17.4673630509814,2.98973262135242));
#182965=CARTESIAN_POINT('Ctrl Pts',(17.5334819301287,17.4673127081403,2.98972732262231));
#182966=CARTESIAN_POINT('Ctrl Pts',(17.5336325228447,17.4672090352814,2.98971640939513));
#182967=CARTESIAN_POINT('Ctrl Pts',(17.5337099990025,17.4671557058178,2.98971079487556));
#182968=CARTESIAN_POINT('Ctrl Pts',(17.5338697470543,17.4670457615125,2.98969921842569));
#182969=CARTESIAN_POINT('Ctrl Pts',(17.533952019471,17.4669891472809,2.98969325646527));
#182970=CARTESIAN_POINT('Ctrl Pts',(17.5341218614312,17.4668722914069,2.98968094882359));
#182971=CARTESIAN_POINT('Ctrl Pts',(17.5342094314499,17.4668120505761,2.98967460311699));
#182972=CARTESIAN_POINT('Ctrl Pts',(17.5343904466872,17.4666875473522,2.98966148612111));
#182973=CARTESIAN_POINT('Ctrl Pts',(17.5344838925254,17.4666232858781,2.98965471479764));
#182974=CARTESIAN_POINT('Ctrl Pts',(17.5346773306777,17.4664902838982,2.98964069795859));
#182975=CARTESIAN_POINT('Ctrl Pts',(17.5347773236958,17.4664215445095,2.98963345240471));
#182976=CARTESIAN_POINT('Ctrl Pts',(17.5400137337795,17.4628224798223,2.98925402426785));
#182977=CARTESIAN_POINT('Ctrl Pts',(17.5451656672636,17.4593148758986,2.98888098255558));
#182978=CARTESIAN_POINT('Ctrl Pts',(17.5569193235446,17.4513883410315,2.98803048541268));
#182979=CARTESIAN_POINT('Ctrl Pts',(17.563530552666,17.4469837360625,2.98755249604682));
#182980=CARTESIAN_POINT('Ctrl Pts',(17.5825872750337,17.4344418554582,2.98617575830628));
#182981=CARTESIAN_POINT('Ctrl Pts',(17.5950937277645,17.426398478788,2.98527351997095));
#182982=CARTESIAN_POINT('Ctrl Pts',(17.6829756194647,17.3711783210871,2.97894129442115));
#182983=CARTESIAN_POINT('Ctrl Pts',(17.7611636702856,17.3286658187697,2.97334119730489));
#182984=CARTESIAN_POINT('Ctrl Pts',(17.9728007499609,17.2303088197515,2.95828433474882));
#182985=CARTESIAN_POINT('Ctrl Pts',(18.1097027478052,17.1829937628595,2.9486215907319));
#182986=CARTESIAN_POINT('Ctrl Pts',(18.3017272040593,17.137930883214,2.93572098062541));
#182987=CARTESIAN_POINT('Ctrl Pts',(18.3535535737208,17.127796552358,2.93230559192251));
#182988=CARTESIAN_POINT('Ctrl Pts',(18.4329899716001,17.1153271677221,2.92722072924385));
#182989=CARTESIAN_POINT('Ctrl Pts',(18.4603548788472,17.1115786096582,2.92549593550986));
#182990=CARTESIAN_POINT('Ctrl Pts',(18.4946139090447,17.1075669612551,2.92337655087486));
#182991=CARTESIAN_POINT('Ctrl Pts',(18.5014450166571,17.1068007623458,2.9229559318332));
#182992=CARTESIAN_POINT('Ctrl Pts',(18.5122856716193,17.105638276262,2.9222916937104));
#182993=CARTESIAN_POINT('Ctrl Pts',(18.5162927576658,17.1052201472015,2.92204687476352));
#182994=CARTESIAN_POINT('Ctrl Pts',(18.523869501796,17.1044513918134,2.92158532925242));
#182995=CARTESIAN_POINT('Ctrl Pts',(18.5274388125086,17.1040984026494,2.92136847784437));
#182996=CARTESIAN_POINT('Ctrl Pts',(18.5356236201462,17.1033099602906,2.92087251471041));
#182997=CARTESIAN_POINT('Ctrl Pts',(18.5402396578402,17.1028805958115,2.92059374766919));
#182998=CARTESIAN_POINT('Ctrl Pts',(18.552544682937,17.1017767917782,2.91985306293506));
#182999=CARTESIAN_POINT('Ctrl Pts',(18.5602360932612,17.1011292259914,2.91939261310972));
#183000=CARTESIAN_POINT('Ctrl Pts',(18.615361245259,17.0967915422639,2.91610950222449));
#183001=CARTESIAN_POINT('Ctrl Pts',(18.662907819489,17.0946590053868,2.91336769521128));
#183002=CARTESIAN_POINT('Ctrl Pts',(18.8710151684416,17.0923477195949,2.90160475788779));
#183003=CARTESIAN_POINT('Ctrl Pts',(19.031232575485,17.1088293059051,2.89313068402648));
#183004=CARTESIAN_POINT('Ctrl Pts',(19.27952085583,17.163351341788,2.87913576518118));
#183005=CARTESIAN_POINT('Ctrl Pts',(19.3695414749106,17.1894802447096,2.87388016513978));
#183006=CARTESIAN_POINT('Ctrl Pts',(19.4774371695767,17.2287187781517,2.86719339279597));
#183007=CARTESIAN_POINT('Ctrl Pts',(19.4972331111016,17.2362562602278,2.86595032402239));
#183008=CARTESIAN_POINT('Ctrl Pts',(19.5252501141197,17.2474081905364,2.8641664457785));
#183009=CARTESIAN_POINT('Ctrl Pts',(19.5335668337337,17.2507800093094,2.86363379513879));
#183010=CARTESIAN_POINT('Ctrl Pts',(19.5478883456293,17.2566926365101,2.86271106875666));
#183011=CARTESIAN_POINT('Ctrl Pts',(19.5539033453923,17.2592085119332,2.86232184191933));
#183012=CARTESIAN_POINT('Ctrl Pts',(19.5654056162361,17.2640820845475,2.86157426508889));
#183013=CARTESIAN_POINT('Ctrl Pts',(19.5708947281593,17.2664352977949,2.86121607082922));
#183014=CARTESIAN_POINT('Ctrl Pts',(19.585159085184,17.2726220923853,2.86028146247286));
#183015=CARTESIAN_POINT('Ctrl Pts',(19.5939183341471,17.276492012189,2.85970380963945));
#183016=CARTESIAN_POINT('Ctrl Pts',(19.623783128052,17.2899294746985,2.85772128238144));
#183017=CARTESIAN_POINT('Ctrl Pts',(19.6447571061295,17.2997837890974,2.85630658819478));
#183018=CARTESIAN_POINT('Ctrl Pts',(19.8208603977366,17.3860803973864,2.84423347168089));
#183019=CARTESIAN_POINT('Ctrl Pts',(19.9662183658207,17.480909681432,2.83289423849767));
#183020=CARTESIAN_POINT('Ctrl Pts',(20.1663040368651,17.649564341385,2.81560267873459));
#183021=CARTESIAN_POINT('Ctrl Pts',(20.2305439069275,17.7110218447689,2.80974511321255));
#183022=CARTESIAN_POINT('Ctrl Pts',(20.3166746267585,17.8044812659972,2.80162753133702));
#183023=CARTESIAN_POINT('Ctrl Pts',(20.3418465338895,17.8333266459226,2.79921925369641));
#183024=CARTESIAN_POINT('Ctrl Pts',(20.37106228502,17.8686983221541,2.79639601807684));
#183025=CARTESIAN_POINT('Ctrl Pts',(20.3758689733621,17.8745820273164,2.79593057915607));
#183026=CARTESIAN_POINT('Ctrl Pts',(20.3832759479575,17.8837489366469,2.79521203995973));
#183027=CARTESIAN_POINT('Ctrl Pts',(20.385898284876,17.8870141259032,2.79495739271188));
#183028=CARTESIAN_POINT('Ctrl Pts',(20.3907339269993,17.8930719321444,2.79448737262402));
#183029=CARTESIAN_POINT('Ctrl Pts',(20.3929498519756,17.8958623319795,2.79427181562138));
#183030=CARTESIAN_POINT('Ctrl Pts',(20.3979314831574,17.9021680683938,2.7937868221346));
#183031=CARTESIAN_POINT('Ctrl Pts',(20.400693092122,17.9056865727529,2.79351767824017));
#183032=CARTESIAN_POINT('Ctrl Pts',(20.4087760818118,17.916052403551,2.79272899282741));
#183033=CARTESIAN_POINT('Ctrl Pts',(20.4140666390407,17.9229238004046,2.79221158735288));
#183034=CARTESIAN_POINT('Ctrl Pts',(20.4509313371465,17.9714173740454,2.78859636504929));
#183035=CARTESIAN_POINT('Ctrl Pts',(20.4810002635095,18.0141669515479,2.78559573874627));
#183036=CARTESIAN_POINT('Ctrl Pts',(20.5206592624741,18.075235686476,2.78149688959111));
#183037=CARTESIAN_POINT('Ctrl Pts',(20.5316079174643,18.0926450880233,2.78034875500697));
#183038=CARTESIAN_POINT('Ctrl Pts',(20.5487952701639,18.1208793198539,2.77851473769732));
#183039=CARTESIAN_POINT('Ctrl Pts',(20.5551946814923,18.1316043780944,2.77782443729203));
#183040=CARTESIAN_POINT('Ctrl Pts',(20.5789341107609,18.1722025378972,2.77523300453677));
#183041=CARTESIAN_POINT('Ctrl Pts',(20.5956373334435,18.202442333369,2.77334633899373));
#183042=CARTESIAN_POINT('Ctrl Pts',(20.6620628127469,18.3299780843604,2.76551783587323));
#183043=CARTESIAN_POINT('Ctrl Pts',(20.7049545171909,18.4306390435408,2.75963434543949));
#183044=CARTESIAN_POINT('Ctrl Pts',(20.7574677469185,18.5862665206151,2.75050070207175));
#183045=CARTESIAN_POINT('Ctrl Pts',(20.7730128620427,18.6390388566448,2.74739931386417));
#183046=CARTESIAN_POINT('Ctrl Pts',(20.7948776477617,18.7255663593186,2.74226454337338));
#183047=CARTESIAN_POINT('Ctrl Pts',(20.8024623955705,18.7589760836889,2.74027036343095));
#183048=CARTESIAN_POINT('Ctrl Pts',(20.8113682688386,18.803143676172,2.73761306896901));
#183049=CARTESIAN_POINT('Ctrl Pts',(20.8134224719187,18.8137495978667,2.73697340715607));
#183050=CARTESIAN_POINT('Ctrl Pts',(20.8166549636292,18.8311515177807,2.73592112264613));
#183051=CARTESIAN_POINT('Ctrl Pts',(20.8178813906035,18.8379384566335,2.7355100388059));
#183052=CARTESIAN_POINT('Ctrl Pts',(20.8201918274489,18.8510911830156,2.73471201337094));
#183053=CARTESIAN_POINT('Ctrl Pts',(20.8212799202028,18.8574561827116,2.73432520660659));
#183054=CARTESIAN_POINT('Ctrl Pts',(20.8237259079851,18.8721694142643,2.73342960032452));
#183055=CARTESIAN_POINT('Ctrl Pts',(20.8250629208647,18.8805209627288,2.73292014362793));
#183056=CARTESIAN_POINT('Ctrl Pts',(20.8285258528103,18.9030146598345,2.73154496279444));
#183057=CARTESIAN_POINT('Ctrl Pts',(20.8305585464184,18.9171705196317,2.73067630480479));
#183058=CARTESIAN_POINT('Ctrl Pts',(20.8479987464014,19.0480368635027,2.72261485166742));
#183059=CARTESIAN_POINT('Ctrl Pts',(20.8537869932468,19.1658025193757,2.71511551805553));
#183060=CARTESIAN_POINT('Ctrl Pts',(20.8441655421086,19.4468842640558,2.69673882015871));
#183061=CARTESIAN_POINT('Ctrl Pts',(20.8196468082345,19.6091428873323,2.68572280871913));
#183062=CARTESIAN_POINT('Ctrl Pts',(20.7685576537369,19.7968531555824,2.67337937413454));
#183063=CARTESIAN_POINT('Ctrl Pts',(20.7597660458441,19.8265655353611,2.67143976672973));
#183064=CARTESIAN_POINT('Ctrl Pts',(20.7481515739078,19.8628690874357,2.66909643757592));
#183065=CARTESIAN_POINT('Ctrl Pts',(20.7459439199124,19.8696513009897,2.66865981095885));
#183066=CARTESIAN_POINT('Ctrl Pts',(20.742417659472,19.8803012780622,2.66797614568826));
#183067=CARTESIAN_POINT('Ctrl Pts',(20.7411220831046,19.8841765294935,2.66772778741347));
#183068=CARTESIAN_POINT('Ctrl Pts',(20.7386717732674,19.8914357911763,2.66726335549497));
#183069=CARTESIAN_POINT('Ctrl Pts',(20.7375197000254,19.894820587778,2.66704713523161));
#183070=CARTESIAN_POINT('Ctrl Pts',(20.7348600112227,19.9025703437701,2.66655282442242));
#183071=CARTESIAN_POINT('Ctrl Pts',(20.7333466878332,19.9069332925427,2.66627507533625));
#183072=CARTESIAN_POINT('Ctrl Pts',(20.7286147903333,19.9204326393194,2.66541726054301));
#183073=CARTESIAN_POINT('Ctrl Pts',(20.7253477241292,19.9295520727174,2.66483999282337));
#183074=CARTESIAN_POINT('Ctrl Pts',(20.6861083649967,20.0367583787596,2.65807647922563));
#183075=CARTESIAN_POINT('Ctrl Pts',(20.6429800471054,20.132089065604,2.65228377325281));
#183076=CARTESIAN_POINT('Ctrl Pts',(20.5861536156766,20.2363875671937,2.6457939407797));
#183077=CARTESIAN_POINT('Ctrl Pts',(20.5791989267153,20.2488504730284,2.64501593719248));
#183078=CARTESIAN_POINT('Ctrl Pts',(20.5179708720893,20.356010932262,2.63829728610142));
#183079=CARTESIAN_POINT('Ctrl Pts',(20.4565755615971,20.4464491632975,2.63241910913415));
#183080=CARTESIAN_POINT('Ctrl Pts',(20.3414554341051,20.5906587606872,2.62215688926952));
#183081=CARTESIAN_POINT('Ctrl Pts',(20.2913185062113,20.6470113559695,2.61788302091295));
#183082=CARTESIAN_POINT('Ctrl Pts',(20.2250211086304,20.7139639102609,2.6123816884117));
#183083=CARTESIAN_POINT('Ctrl Pts',(20.2115771960438,20.7271827256754,2.61127338883033));
#183084=CARTESIAN_POINT('Ctrl Pts',(20.191773460551,20.7461413158502,2.60965027835564));
#183085=CARTESIAN_POINT('Ctrl Pts',(20.1855522875329,20.7520250728618,2.60914172239043));
#183086=CARTESIAN_POINT('Ctrl Pts',(20.1745822689646,20.7622747456841,2.6082471957929));
#183087=CARTESIAN_POINT('Ctrl Pts',(20.1698488161687,20.7666570270911,2.60786193390164));
#183088=CARTESIAN_POINT('Ctrl Pts',(20.1606186148432,20.7751244311557,2.60711202438315));
#183089=CARTESIAN_POINT('Ctrl Pts',(20.1561241601204,20.7792119692059,2.60674748500489));
#183090=CARTESIAN_POINT('Ctrl Pts',(20.1453377017581,20.7889373453293,2.60587403444309));
#183091=CARTESIAN_POINT('Ctrl Pts',(20.1390294582118,20.794556943248,2.6053643625018));
#183092=CARTESIAN_POINT('Ctrl Pts',(20.1161438441494,20.814699824562,2.60351932210781));
#183093=CARTESIAN_POINT('Ctrl Pts',(20.0993740074318,20.8290013891903,2.60217480871766));
#183094=CARTESIAN_POINT('Ctrl Pts',(19.9387498973498,20.9617084909908,2.58936234635044));
#183095=CARTESIAN_POINT('Ctrl Pts',(19.7801029760675,21.060876529379,2.57708792910508));
#183096=CARTESIAN_POINT('Ctrl Pts',(19.5380529547054,21.170983708993,2.55953281888367));
#183097=CARTESIAN_POINT('Ctrl Pts',(19.4637182092824,21.1998565383836,2.55429901582396));
#183098=CARTESIAN_POINT('Ctrl Pts',(19.3537815583048,21.2355613872426,2.54693145611749));
#183099=CARTESIAN_POINT('Ctrl Pts',(19.3193557845428,21.2457817944272,2.54467599502686));
#183100=CARTESIAN_POINT('Ctrl Pts',(19.2774826602851,21.2570623714443,2.54200806441007));
#183101=CARTESIAN_POINT('Ctrl Pts',(19.270270550552,21.2589644846257,2.54155122687397));
#183102=CARTESIAN_POINT('Ctrl Pts',(19.2590227187892,21.2618674824414,2.54084308459988));
#183103=CARTESIAN_POINT('Ctrl Pts',(19.254993928983,21.2628946397,2.54059030235616));
#183104=CARTESIAN_POINT('Ctrl Pts',(19.2475040386427,21.264780737758,2.54012199252891));
#183105=CARTESIAN_POINT('Ctrl Pts',(19.2440438268648,21.2656427941227,2.53990629178585));
#183106=CARTESIAN_POINT('Ctrl Pts',(19.2361998145247,21.2675759675739,2.53941877651676));
#183107=CARTESIAN_POINT('Ctrl Pts',(19.231814768706,21.2686418106745,2.53914726804829));
#183108=CARTESIAN_POINT('Ctrl Pts',(19.2204800439872,21.2713585098487,2.53844803035721));
#183109=CARTESIAN_POINT('Ctrl Pts',(19.2135252930803,21.2729882441161,2.53802148695486));
#183110=CARTESIAN_POINT('Ctrl Pts',(19.1706847542736,21.2827987661309,2.53540860718437));
#183111=CARTESIAN_POINT('Ctrl Pts',(19.1345965599149,21.2900782731145,2.53327039006495));
#183112=CARTESIAN_POINT('Ctrl Pts',(18.9307422692366,21.3256928685882,2.52145078262881));
#183113=CARTESIAN_POINT('Ctrl Pts',(18.760216978574,21.3346661905985,2.51249778701761));
#183114=CARTESIAN_POINT('Ctrl Pts',(18.4950797422142,21.3166453258894,2.49788079193117));
#183115=CARTESIAN_POINT('Ctrl Pts',(18.4002755236487,21.3037135529063,2.49252208513441));
#183116=CARTESIAN_POINT('Ctrl Pts',(18.285702472139,21.2801005024953,2.48571044944164));
#183117=CARTESIAN_POINT('Ctrl Pts',(18.2647965717284,21.2754601367662,2.48445395046341));
#183118=CARTESIAN_POINT('Ctrl Pts',(18.2351964026625,21.2684171226172,2.48265413419981));
#183119=CARTESIAN_POINT('Ctrl Pts',(18.2264411174744,21.2662747315379,2.48211917921149));
#183120=CARTESIAN_POINT('Ctrl Pts',(18.2113698566549,21.2624846664033,2.48119372497678));
#183121=CARTESIAN_POINT('Ctrl Pts',(18.2050472819514,21.2608635622447,2.4808040882778));
#183122=CARTESIAN_POINT('Ctrl Pts',(18.1929620932719,21.2577052922725,2.48005660600392));
#183123=CARTESIAN_POINT('Ctrl Pts',(18.18719827188,21.2561729606385,2.47969892040922));
#183124=CARTESIAN_POINT('Ctrl Pts',(18.1722407381353,21.2521286989304,2.47876757638189));
#183125=CARTESIAN_POINT('Ctrl Pts',(18.16305745215,21.2495790238047,2.47819269623891));
#183126=CARTESIAN_POINT('Ctrl Pts',(18.1318712516456,21.2406931399928,2.47622976472061));
#183127=CARTESIAN_POINT('Ctrl Pts',(18.1099546469103,21.2340621851066,2.47483215411796));
#183128=CARTESIAN_POINT('Ctrl Pts',(17.919796046112,21.173144962901,2.46254277184201));
#183129=CARTESIAN_POINT('Ctrl Pts',(17.7588900937194,21.0983467255474,2.45093552725517));
#183130=CARTESIAN_POINT('Ctrl Pts',(17.5362340003908,20.9587014880308,2.43357159237093));
#183131=CARTESIAN_POINT('Ctrl Pts',(17.4661392761633,20.9085379110295,2.42789867378549));
#183132=CARTESIAN_POINT('Ctrl Pts',(17.3701107109149,20.8305395294917,2.42000161146651));
#183133=CARTESIAN_POINT('Ctrl Pts',(17.3415644532976,20.8060629868257,2.41763723257203));
#183134=CARTESIAN_POINT('Ctrl Pts',(17.3080783589006,20.7757663102908,2.41485850290126));
#183135=CARTESIAN_POINT('Ctrl Pts',(17.3025004690122,20.7706651015895,2.41439546462145));
#183136=CARTESIAN_POINT('Ctrl Pts',(17.2938809534938,20.7626970062596,2.41367982591775));
#183137=CARTESIAN_POINT('Ctrl Pts',(17.2908203595503,20.759850862231,2.41342569804632));
#183138=CARTESIAN_POINT('Ctrl Pts',(17.2851655001153,20.754560913545,2.41295615827412));
#183139=CARTESIAN_POINT('Ctrl Pts',(17.2825689998551,20.752119642985,2.41274056526535));
#183140=CARTESIAN_POINT('Ctrl Pts',(17.2767198206098,20.7465922576952,2.41225488784691));
#183141=CARTESIAN_POINT('Ctrl Pts',(17.273470782648,20.7435023684316,2.41198509970045));
#183142=CARTESIAN_POINT('Ctrl Pts',(17.2639302387924,20.7343712533102,2.41119277204724));
#183143=CARTESIAN_POINT('Ctrl Pts',(17.2576661354987,20.7283013559205,2.41067239826115));
#183144=CARTESIAN_POINT('Ctrl Pts',(17.2133343546395,20.6848095244402,2.40698701006873));
#183145=CARTESIAN_POINT('Ctrl Pts',(17.1766531837023,20.6459949249099,2.40392351029271));
#183146=CARTESIAN_POINT('Ctrl Pts',(17.1324646051439,20.5955434004643,2.40015191131375));
#183147=CARTESIAN_POINT('Ctrl Pts',(17.1235532642104,20.5851678832804,2.39938689994671));
#183148=CARTESIAN_POINT('Ctrl Pts',(17.081112484665,20.5347739555129,2.39571810976276));
#183149=CARTESIAN_POINT('Ctrl Pts',(17.0489694635835,20.4936094878229,2.39286152408738));
#183150=CARTESIAN_POINT('Ctrl Pts',(16.954269844877,20.362617898944,2.38406088147274));
#183151=CARTESIAN_POINT('Ctrl Pts',(16.8971323282311,20.269101834365,2.37816902432726));
#183152=CARTESIAN_POINT('Ctrl Pts',(16.8130787893629,20.1040280832914,2.36786971009912));
#183153=CARTESIAN_POINT('Ctrl Pts',(16.7823335528736,20.0346709197077,2.36357207598258));
#183154=CARTESIAN_POINT('Ctrl Pts',(16.7519971962846,19.9549382833464,2.35859153550039));
#183155=CARTESIAN_POINT('Ctrl Pts',(16.7486782177562,19.946035166375,2.35803489614114));
#183156=CARTESIAN_POINT('Ctrl Pts',(16.7454193622815,19.9371102170409,2.35747630371138));
#183157=CARTESIAN_POINT('',(16.6180380291883,19.2128841872923,2.8890562790225));
#183158=CARTESIAN_POINT('Ctrl Pts',(16.6180380291883,19.2128841872923,2.8890562790225));
#183159=CARTESIAN_POINT('Ctrl Pts',(16.6223668818157,18.7070050427869,2.85866010167885));
#183160=CARTESIAN_POINT('Ctrl Pts',(17.0578065161,17.488911989304,2.78587198877473));
#183161=CARTESIAN_POINT('Ctrl Pts',(19.0938031543631,16.7337290395393,2.67069194031012));
#183162=CARTESIAN_POINT('Ctrl Pts',(21.0117474691636,18.1726377106278,2.54351613362868));
#183163=CARTESIAN_POINT('Ctrl Pts',(20.8399998558895,20.5641793786163,2.41634032694726));
#183164=CARTESIAN_POINT('Ctrl Pts',(18.736128084209,21.7142628689015,2.28916452026583));
#183165=CARTESIAN_POINT('Ctrl Pts',(17.1750895426501,20.864363812569,2.19488963230201));
#183166=CARTESIAN_POINT('Ctrl Pts',(16.7978195750248,20.0858831573232,2.14300667989868));
#183167=CARTESIAN_POINT('Ctrl Pts',(16.7452305776443,19.937179123763,2.13351566305583));
#183168=CARTESIAN_POINT('Ctrl Pts',(16.6170008744739,19.2129241938202,2.88845972389577));
#183169=CARTESIAN_POINT('Ctrl Pts',(16.6170483110913,19.2651139869398,2.89187890939447));
#183170=CARTESIAN_POINT('Ctrl Pts',(16.6190256614439,19.3172837811673,2.8953255352823));
#183171=CARTESIAN_POINT('Ctrl Pts',(16.6324061683838,19.4956946961602,2.90714885683369));
#183172=CARTESIAN_POINT('Ctrl Pts',(16.6532119485831,19.6209701165616,2.91552733173334));
#183173=CARTESIAN_POINT('Ctrl Pts',(16.6881017065402,19.7551794554187,2.92412675351169));
#183174=CARTESIAN_POINT('Ctrl Pts',(16.6911984993194,19.7666915967566,2.92486114697043));
#183175=CARTESIAN_POINT('Ctrl Pts',(16.6957386595639,19.7830183180294,2.92589745161739));
#183176=CARTESIAN_POINT('Ctrl Pts',(16.6971021146366,19.7878546210914,2.92620377127852));
#183177=CARTESIAN_POINT('Ctrl Pts',(16.6994812574396,19.7961800500058,2.92672989900691));
#183178=CARTESIAN_POINT('Ctrl Pts',(16.7004887290258,19.7996714842374,2.92695018057992));
#183179=CARTESIAN_POINT('Ctrl Pts',(16.7024593753537,19.8064354093843,2.9273762108653));
#183180=CARTESIAN_POINT('Ctrl Pts',(16.7034214694763,19.809708166049,2.92758202330274));
#183181=CARTESIAN_POINT('Ctrl Pts',(16.7060381584365,19.8185304964909,2.92813598952883));
#183182=CARTESIAN_POINT('Ctrl Pts',(16.7077076345177,19.8240756775356,2.92848328119213));
#183183=CARTESIAN_POINT('Ctrl Pts',(16.713985996204,19.844623501642,2.92976708448758));
#183184=CARTESIAN_POINT('Ctrl Pts',(16.718739047464,19.8595820249649,2.93069553929684));
#183185=CARTESIAN_POINT('Ctrl Pts',(16.7305868663345,19.8954805026194,2.9329119712285));
#183186=CARTESIAN_POINT('Ctrl Pts',(16.7378417059312,19.9163574730357,2.93419125178592));
#183187=CARTESIAN_POINT('Ctrl Pts',(16.7454193815904,19.9371102699218,2.93545674419276));
#183188=CARTESIAN_POINT('Origin',(18.734,19.211,0.));
#183189=CARTESIAN_POINT('',(16.7454192928009,19.9371100267559,3.95421654644109));
#183190=CARTESIAN_POINT('',(16.7454193623262,19.9371102171633,3.73234496441554));
#183191=CARTESIAN_POINT('',(16.7454193623258,19.9371102171621,0.));
#183192=CARTESIAN_POINT('Ctrl Pts',(16.7454192928009,19.9371100267559,3.95421654644109));
#183193=CARTESIAN_POINT('Ctrl Pts',(16.7247484919563,19.8804993834,3.95029629217742));
#183194=CARTESIAN_POINT('Ctrl Pts',(16.7064930186527,19.8230004891677,3.94643456633113));
#183195=CARTESIAN_POINT('Ctrl Pts',(16.6875909795291,19.7532558190289,3.94195338903305));
#183196=CARTESIAN_POINT('Ctrl Pts',(16.6845683668796,19.7417176730903,3.94121861484773));
#183197=CARTESIAN_POINT('Ctrl Pts',(16.6804108714473,19.7252819748228,3.94018187021498));
#183198=CARTESIAN_POINT('Ctrl Pts',(16.6791957316872,19.7204052204843,3.93987548630145));
#183199=CARTESIAN_POINT('Ctrl Pts',(16.6771318962641,19.7119948202375,3.93934928327177));
#183200=CARTESIAN_POINT('Ctrl Pts',(16.676274915089,19.7084632466605,3.93912899029159));
#183201=CARTESIAN_POINT('Ctrl Pts',(16.6746311950773,19.7016126371222,3.93870296551654));
#183202=CARTESIAN_POINT('Ctrl Pts',(16.6738433838447,19.6982939068827,3.93849716986552));
#183203=CARTESIAN_POINT('Ctrl Pts',(16.6717400398632,19.6893370934564,3.93794330716889));
#183204=CARTESIAN_POINT('Ctrl Pts',(16.6704395973557,19.6836954459169,3.93759610167184));
#183205=CARTESIAN_POINT('Ctrl Pts',(16.6657019231336,19.6627500211767,3.93631295334329));
#183206=CARTESIAN_POINT('Ctrl Pts',(16.662411560615,19.6474130918184,3.93538505674119));
#183207=CARTESIAN_POINT('Ctrl Pts',(16.6325545485702,19.5002904636277,3.92658314420798));
#183208=CARTESIAN_POINT('Ctrl Pts',(16.6184239864913,19.36627406199,3.91931201409377));
#183209=CARTESIAN_POINT('Ctrl Pts',(16.6170404626411,19.2255206712854,3.91166808709353));
#183210=CARTESIAN_POINT('Ctrl Pts',(16.6170066729792,19.21923322756,3.91132665166106));
#183211=CARTESIAN_POINT('Ctrl Pts',(16.6168668543953,19.0671072358186,3.90306442079204));
#183212=CARTESIAN_POINT('Ctrl Pts',(16.631802104662,18.9216640300942,3.89510370491612));
#183213=CARTESIAN_POINT('Ctrl Pts',(16.6664676940301,18.7553942943312,3.88524444627758));
#183214=CARTESIAN_POINT('Ctrl Pts',(16.6717720439157,18.7319570133412,3.8838376637426));
#183215=CARTESIAN_POINT('Ctrl Pts',(16.6797804434919,18.6991743721309,3.88184393431146));
#183216=CARTESIAN_POINT('Ctrl Pts',(16.6821518236525,18.6897490852592,3.88126768217143));
#183217=CARTESIAN_POINT('Ctrl Pts',(16.6860916184554,18.6745335581911,3.88033237414389));
#183218=CARTESIAN_POINT('Ctrl Pts',(16.6876199075611,18.6687330007115,3.87997461950769));
#183219=CARTESIAN_POINT('Ctrl Pts',(16.6908553258924,18.6566615851086,3.87922758648507));
#183220=CARTESIAN_POINT('Ctrl Pts',(16.6925667183177,18.6503919439243,3.87883817304001));
#183221=CARTESIAN_POINT('Ctrl Pts',(16.6966783629367,18.6355975501918,3.87791587509186));
#183222=CARTESIAN_POINT('Ctrl Pts',(16.6991032787632,18.6270798322828,3.87738219263228));
#183223=CARTESIAN_POINT('Ctrl Pts',(16.7073169386805,18.598901295646,3.87560761763461));
#183224=CARTESIAN_POINT('Ctrl Pts',(16.7133376069263,18.5793098055459,3.87435918433686));
#183225=CARTESIAN_POINT('Ctrl Pts',(16.7467230035331,18.4760372034541,3.86769848665262));
#183226=CARTESIAN_POINT('Ctrl Pts',(16.7790003195529,18.3940464914149,3.86212556696613));
#183227=CARTESIAN_POINT('Ctrl Pts',(16.8711049339375,18.1970656689088,3.84804779674571));
#183228=CARTESIAN_POINT('Ctrl Pts',(16.9365619977143,18.0850986568205,3.83941386772588));
#183229=CARTESIAN_POINT('Ctrl Pts',(17.0275745884516,17.9577902590976,3.82914895403899));
#183230=CARTESIAN_POINT('Ctrl Pts',(17.0437452682531,17.936064175417,3.8273808935106));
#183231=CARTESIAN_POINT('Ctrl Pts',(17.0955041292582,17.8692399588405,3.82190406589159));
#183232=CARTESIAN_POINT('Ctrl Pts',(17.1325169023024,17.8252720778985,3.81824351413873));
#183233=CARTESIAN_POINT('Ctrl Pts',(17.1772637435692,17.7763083903759,3.8141505490437));
#183234=CARTESIAN_POINT('Ctrl Pts',(17.1832929408898,17.7697937656368,3.81360563789021));
#183235=CARTESIAN_POINT('Ctrl Pts',(17.192451711867,17.7600216143737,3.81278800044979));
#183236=CARTESIAN_POINT('Ctrl Pts',(17.1955509415179,17.7567359608619,3.81251304570616));
#183237=CARTESIAN_POINT('Ctrl Pts',(17.2011160620806,17.7508737892577,3.81202244275113));
#183238=CARTESIAN_POINT('Ctrl Pts',(17.2035779612589,17.7482935693127,3.81180649487585));
#183239=CARTESIAN_POINT('Ctrl Pts',(17.2089220942576,17.7427208566224,3.81134007798083));
#183240=CARTESIAN_POINT('Ctrl Pts',(17.2118066115013,17.7397306330404,3.81108979089212));
#183241=CARTESIAN_POINT('Ctrl Pts',(17.2198846347658,17.7314057682022,3.81039287430154));
#183242=CARTESIAN_POINT('Ctrl Pts',(17.2250975657347,17.7260899429216,3.80994773226656));
#183243=CARTESIAN_POINT('Ctrl Pts',(17.2554564554609,17.6954567773669,3.80738100367323));
#183244=CARTESIAN_POINT('Ctrl Pts',(17.2812128712832,17.670749315593,3.8053046399847));
#183245=CARTESIAN_POINT('Ctrl Pts',(17.3658597101237,17.5935634073009,3.79874964410138));
#183246=CARTESIAN_POINT('Ctrl Pts',(17.4270649057938,17.5437173060126,3.79440809052466));
#183247=CARTESIAN_POINT('Ctrl Pts',(17.5646431049824,17.443914775174,3.78513861471452));
#183248=CARTESIAN_POINT('Ctrl Pts',(17.6417468694929,17.3952443130942,3.78023168271004));
#183249=CARTESIAN_POINT('Ctrl Pts',(17.8150644189032,17.3008858550108,3.76938604393385));
#183250=CARTESIAN_POINT('Ctrl Pts',(17.9120641973599,17.2571842640412,3.7634234586998));
#183251=CARTESIAN_POINT('Ctrl Pts',(18.0251857159193,17.2161390364554,3.75637195120753));
#183252=CARTESIAN_POINT('Ctrl Pts',(18.0384924579377,17.2114607536288,3.75554117881114));
#183253=CARTESIAN_POINT('Ctrl Pts',(18.0597976434987,17.2042088400867,3.75420857474409));
#183254=CARTESIAN_POINT('Ctrl Pts',(18.0677665199581,17.2015491984163,3.75370958840416));
#183255=CARTESIAN_POINT('Ctrl Pts',(18.0818794455598,17.1969321359447,3.75282483126966));
#183256=CARTESIAN_POINT('Ctrl Pts',(18.0880170368992,17.1949552116812,3.75243970890136));
#183257=CARTESIAN_POINT('Ctrl Pts',(18.1007603303273,17.1909147508947,3.75163932766964));
#183258=CARTESIAN_POINT('Ctrl Pts',(18.1073673029933,17.1888555061092,3.75122393312121));
#183259=CARTESIAN_POINT('Ctrl Pts',(18.124416130665,17.1836333479322,3.7501508906198));
#183260=CARTESIAN_POINT('Ctrl Pts',(18.1348724570303,17.1805187230742,3.74949167123378));
#183261=CARTESIAN_POINT('Ctrl Pts',(18.1791654826141,17.1676970858416,3.74669424986871));
#183262=CARTESIAN_POINT('Ctrl Pts',(18.2132158765687,17.1587544484412,3.74453138797352));
#183263=CARTESIAN_POINT('Ctrl Pts',(18.3030456885866,17.1375420061864,3.73878988404235));
#183264=CARTESIAN_POINT('Ctrl Pts',(18.359123449435,17.1266736494679,3.73516955598228));
#183265=CARTESIAN_POINT('Ctrl Pts',(18.5659650864189,17.095203200325,3.72169996848368));
#183266=CARTESIAN_POINT('Ctrl Pts',(18.7183859622587,17.0886001209964,3.71151209603572));
#183267=CARTESIAN_POINT('Ctrl Pts',(18.892616792953,17.0998308026269,3.70010856489985));
#183268=CARTESIAN_POINT('Ctrl Pts',(18.9150333607664,17.1016347781115,3.69864695010285));
#183269=CARTESIAN_POINT('Ctrl Pts',(18.9885486252538,17.1087315212321,3.6938798584984));
#183270=CARTESIAN_POINT('Ctrl Pts',(19.0394879421606,17.1155273052977,3.69061826221014));
#183271=CARTESIAN_POINT('Ctrl Pts',(19.097897583569,17.1254953651646,3.68696361486686));
#183272=CARTESIAN_POINT('Ctrl Pts',(19.1056541397384,17.126863670949,3.68648004763279));
#183273=CARTESIAN_POINT('Ctrl Pts',(19.1180092285927,17.129114356253,3.68571279068866));
#183274=CARTESIAN_POINT('Ctrl Pts',(19.1226126963703,17.1299687425523,3.68542757795243));
#183275=CARTESIAN_POINT('Ctrl Pts',(19.1307437978061,17.1315057662041,3.68492502876699));
#183276=CARTESIAN_POINT('Ctrl Pts',(19.1342725760946,17.1321821207567,3.68470733863894));
#183277=CARTESIAN_POINT('Ctrl Pts',(19.1417294329537,17.133631054568,3.68424820497023));
#183278=CARTESIAN_POINT('Ctrl Pts',(19.1456570398177,17.1344057911757,3.68400688603866));
#183279=CARTESIAN_POINT('Ctrl Pts',(19.1562098319579,17.1365184888115,3.68335982343204));
#183280=CARTESIAN_POINT('Ctrl Pts',(19.1628309110881,17.1378770574379,3.68295524001349));
#183281=CARTESIAN_POINT('Ctrl Pts',(19.1951330106125,17.1446664483656,3.68098774818565));
#183282=CARTESIAN_POINT('Ctrl Pts',(19.2207192523852,17.1505431302219,3.67944890677708));
#183283=CARTESIAN_POINT('Ctrl Pts',(19.2936960197621,17.1687398749753,3.67509903816515));
#183284=CARTESIAN_POINT('Ctrl Pts',(19.3407791790556,17.1822304933156,3.67234024881934));
#183285=CARTESIAN_POINT('Ctrl Pts',(19.4792647697274,17.2271637842869,3.66425653601295));
#183286=CARTESIAN_POINT('Ctrl Pts',(19.5690283484965,17.2632436453111,3.65905330180025));
#183287=CARTESIAN_POINT('Ctrl Pts',(19.782982813211,17.3667607798955,3.64612001393885));
#183288=CARTESIAN_POINT('Ctrl Pts',(19.9034744994948,17.4407160945882,3.63834020669294));
#183289=CARTESIAN_POINT('Ctrl Pts',(20.0270791540754,17.5347424712454,3.62924194329472));
#183290=CARTESIAN_POINT('Ctrl Pts',(20.0383587969921,17.5435045381674,3.62840084155293));
#183291=CARTESIAN_POINT('Ctrl Pts',(20.0561711904685,17.5576325904661,3.627054790234));
#183292=CARTESIAN_POINT('Ctrl Pts',(20.0627620755106,17.562924822304,3.62655277820123));
#183293=CARTESIAN_POINT('Ctrl Pts',(20.0743311130781,17.5723288329612,3.6256645038507));
#183294=CARTESIAN_POINT('Ctrl Pts',(20.0793225079471,17.5764242034842,3.62527890689492));
#183295=CARTESIAN_POINT('Ctrl Pts',(20.0896084815458,17.5849427313107,3.62447935857138));
#183296=CARTESIAN_POINT('Ctrl Pts',(20.094900323121,17.589369060152,3.62406528049336));
#183297=CARTESIAN_POINT('Ctrl Pts',(20.108430224941,17.6007989344874,3.62299948651327));
#183298=CARTESIAN_POINT('Ctrl Pts',(20.1166363606182,17.6078398077196,3.62234623953733));
#183299=CARTESIAN_POINT('Ctrl Pts',(20.1506783955552,17.6375036984667,3.61960735803053));
#183300=CARTESIAN_POINT('Ctrl Pts',(20.1760146505218,17.6606897671486,3.61749833195349));
#183301=CARTESIAN_POINT('Ctrl Pts',(20.240566403812,17.7227151087219,3.61193372246401));
#183302=CARTESIAN_POINT('Ctrl Pts',(20.2788449608135,17.7624878428033,3.60843957879383));
#183303=CARTESIAN_POINT('Ctrl Pts',(20.3882887482446,17.8854814578889,3.5978564865706));
#183304=CARTESIAN_POINT('Ctrl Pts',(20.4545968905746,17.9727699954585,3.59061919264036));
#183305=CARTESIAN_POINT('Ctrl Pts',(20.5427431078368,18.109644338915,3.57986512411882));
#183306=CARTESIAN_POINT('Ctrl Pts',(20.5699267616361,18.1555810368668,3.5763483951389));
#183307=CARTESIAN_POINT('Ctrl Pts',(20.6014103935018,18.2136888882982,3.57204734140284));
#183308=CARTESIAN_POINT('Ctrl Pts',(20.6073733705971,18.2249354710971,3.57122155100634));
#183309=CARTESIAN_POINT('Ctrl Pts',(20.6377306323513,18.2834607935749,3.56696093570361));
#183310=CARTESIAN_POINT('Ctrl Pts',(20.6604400707671,18.3315973715193,3.5635792945492));
#183311=CARTESIAN_POINT('Ctrl Pts',(20.6847307402026,18.3885557957642,3.55975955703126));
#183312=CARTESIAN_POINT('Ctrl Pts',(20.6880986552157,18.3965901882168,3.55922487991935));
#183313=CARTESIAN_POINT('Ctrl Pts',(20.6931238587743,18.4087888131844,3.55841956124402));
#183314=CARTESIAN_POINT('Ctrl Pts',(20.6948176301499,18.4129377816118,3.55814678779655));
#183315=CARTESIAN_POINT('Ctrl Pts',(20.6978347087636,18.420395840351,3.55765852519533));
#183316=CARTESIAN_POINT('Ctrl Pts',(20.6991628401168,18.4237029067717,3.55744274853947));
#183317=CARTESIAN_POINT('Ctrl Pts',(20.7020310591701,18.4308972936601,3.55697492361436));
#183318=CARTESIAN_POINT('Ctrl Pts',(20.7035679785706,18.4347858151385,3.55672306686164));
#183319=CARTESIAN_POINT('Ctrl Pts',(20.7078539039617,18.4457242178443,3.55601733176051));
#183320=CARTESIAN_POINT('Ctrl Pts',(20.7105766793615,18.4527844030483,3.5555650024852));
#183321=CARTESIAN_POINT('Ctrl Pts',(20.7266512509448,18.495141016074,3.55286949437965));
#183322=CARTESIAN_POINT('Ctrl Pts',(20.7390960763351,18.5307770848804,3.55067700937348));
#183323=CARTESIAN_POINT('Ctrl Pts',(20.7769592981543,18.6492898371242,3.54357305343723));
#183324=CARTESIAN_POINT('Ctrl Pts',(20.7982434195186,18.7333992435162,3.5388264408764));
#183325=CARTESIAN_POINT('Ctrl Pts',(20.8469274614126,18.9914865692923,3.52453497306496));
#183326=CARTESIAN_POINT('Ctrl Pts',(20.8578578809586,19.1677608205669,3.51507770062637));
#183327=CARTESIAN_POINT('Ctrl Pts',(20.8454234299451,19.3662649488753,3.50351993292604));
#183328=CARTESIAN_POINT('Ctrl Pts',(20.8436154784559,19.3891532409696,3.50217485171648));
#183329=CARTESIAN_POINT('Ctrl Pts',(20.8405298003198,19.4215046981011,3.50025429114793));
#183330=CARTESIAN_POINT('Ctrl Pts',(20.8395597234778,19.4309960770034,3.49968846918349));
#183331=CARTESIAN_POINT('Ctrl Pts',(20.837878837021,19.4464111955738,3.4987655483667));
#183332=CARTESIAN_POINT('Ctrl Pts',(20.8372070789874,19.4523391257998,3.49840968335445));
#183333=CARTESIAN_POINT('Ctrl Pts',(20.8357481046758,19.4647449242833,3.49766290957519));
#183334=CARTESIAN_POINT('Ctrl Pts',(20.83495597707,19.4712221417209,3.49727184941826));
#183335=CARTESIAN_POINT('Ctrl Pts',(20.8329995246018,19.4866285194698,3.49633888498889));
#183336=CARTESIAN_POINT('Ctrl Pts',(20.8318081577149,19.4955540625825,3.49579613164263));
#183337=CARTESIAN_POINT('Ctrl Pts',(20.8275986363043,19.5256268633829,3.49395969721455));
#183338=CARTESIAN_POINT('Ctrl Pts',(20.8243174357203,19.546735429376,3.49265773505246));
#183339=CARTESIAN_POINT('Ctrl Pts',(20.8046822388433,19.6615735476362,3.4855015985071));
#183340=CARTESIAN_POINT('Ctrl Pts',(20.7823451858166,19.7541567335689,3.47945876524308));
#183341=CARTESIAN_POINT('Ctrl Pts',(20.7028197990833,20.0075510695226,3.46220185014897));
#183342=CARTESIAN_POINT('Ctrl Pts',(20.6323262092714,20.1634176745352,3.45070097342028));
#183343=CARTESIAN_POINT('Ctrl Pts',(20.5247189806277,20.3407713406864,3.43745842720362));
#183344=CARTESIAN_POINT('Ctrl Pts',(20.5047006626247,20.3718950410325,3.43513089479241));
#183345=CARTESIAN_POINT('Ctrl Pts',(20.479848698957,20.4083940497345,3.43241164604575));
#183346=CARTESIAN_POINT('Ctrl Pts',(20.4757918931156,20.4142876607039,3.4319728904228));
#183347=CARTESIAN_POINT('Ctrl Pts',(20.4691256952143,20.423867766163,3.43126038115275));
#183348=CARTESIAN_POINT('Ctrl Pts',(20.4665342860802,20.4275666216122,3.43098545245011));
#183349=CARTESIAN_POINT('Ctrl Pts',(20.4618754101895,20.4341714046122,3.43049487757375));
#183350=CARTESIAN_POINT('Ctrl Pts',(20.459812426369,20.4370804165301,3.43027893188099));
#183351=CARTESIAN_POINT('Ctrl Pts',(20.4553299466865,20.4433674284323,3.42981249880882));
#183352=CARTESIAN_POINT('Ctrl Pts',(20.4529078617229,20.4467435120645,3.42956219347246));
#183353=CARTESIAN_POINT('Ctrl Pts',(20.4461172525281,20.4561501775378,3.42886517455947));
#183354=CARTESIAN_POINT('Ctrl Pts',(20.4417267765237,20.4621649417681,3.42841994915767));
#183355=CARTESIAN_POINT('Ctrl Pts',(20.4161009846095,20.4968849851605,3.42585177339696));
#183356=CARTESIAN_POINT('Ctrl Pts',(20.3941725331796,20.5250743577092,3.42377410555496));
#183357=CARTESIAN_POINT('Ctrl Pts',(20.3215027755959,20.6137677138162,3.4172131149315));
#183358=CARTESIAN_POINT('Ctrl Pts',(20.2680842483836,20.6719961611282,3.4128671598357));
#183359=CARTESIAN_POINT('Ctrl Pts',(20.0773207152058,20.8579061193029,3.39834043935836));
#183360=CARTESIAN_POINT('Ctrl Pts',(19.9263513766985,20.9702903852687,3.38832616818643));
#183361=CARTESIAN_POINT('Ctrl Pts',(19.7434051941618,21.0719864758411,3.3761502372197));
#183362=CARTESIAN_POINT('Ctrl Pts',(19.7240821422682,21.0823382398379,3.37486508147468));
#183363=CARTESIAN_POINT('Ctrl Pts',(19.6971109976387,21.0962525727129,3.37307099928795));
#183364=CARTESIAN_POINT('Ctrl Pts',(19.6895967173653,21.1000725151064,3.37257113518105));
#183365=CARTESIAN_POINT('Ctrl Pts',(19.6766323688651,21.106565895805,3.37170859271869));
#183366=CARTESIAN_POINT('Ctrl Pts',(19.6711932096109,21.109260976486,3.37134667641637));
#183367=CARTESIAN_POINT('Ctrl Pts',(19.6599479645489,21.1147728360806,3.37059831377293));
#183368=CARTESIAN_POINT('Ctrl Pts',(19.6541404456095,21.1175865318348,3.37021176479006));
#183369=CARTESIAN_POINT('Ctrl Pts',(19.6405818309121,21.1240791927197,3.36930911250736));
#183370=CARTESIAN_POINT('Ctrl Pts',(19.6328210949539,21.127737658011,3.36879230482829));
#183371=CARTESIAN_POINT('Ctrl Pts',(19.6078518244859,21.1393233550017,3.36712895246425));
#183372=CARTESIAN_POINT('Ctrl Pts',(19.5905594037489,21.1470666114114,3.36597610701792));
#183373=CARTESIAN_POINT('Ctrl Pts',(19.5033261630397,21.1847307589193,3.36015446677587));
#183374=CARTESIAN_POINT('Ctrl Pts',(19.4319196699335,21.2110954369028,3.35536690731971));
#183375=CARTESIAN_POINT('Ctrl Pts',(19.2545090469346,21.2659403409532,3.34342815692353));
#183376=CARTESIAN_POINT('Ctrl Pts',(19.1474119403767,21.2901336131556,3.33617805675904));
#183377=CARTESIAN_POINT('Ctrl Pts',(18.9768280022155,21.3149634754282,3.32479162502947));
#183378=CARTESIAN_POINT('Ctrl Pts',(18.9143492319995,21.3212375516556,3.3206573973919));
#183379=CARTESIAN_POINT('Ctrl Pts',(18.8373596320936,21.3255239533143,3.31566596817692));
#183380=CARTESIAN_POINT('Ctrl Pts',(18.8230293662747,21.3261757729558,3.31474131932889));
#183381=CARTESIAN_POINT('Ctrl Pts',(18.7661724182169,21.3281830850558,3.31109280204313));
#183382=CARTESIAN_POINT('Ctrl Pts',(18.7236124982658,21.3284021685191,3.30840623374989));
#183383=CARTESIAN_POINT('Ctrl Pts',(18.6736080669189,21.3271515910924,3.30532379751994));
#183384=CARTESIAN_POINT('Ctrl Pts',(18.6661452524241,21.326925442702,3.30486570986411));
#183385=CARTESIAN_POINT('Ctrl Pts',(18.654076088554,21.3264957870548,3.30412818775641));
#183386=CARTESIAN_POINT('Ctrl Pts',(18.6494690095676,21.3263167066074,3.3038474403075));
#183387=CARTESIAN_POINT('Ctrl Pts',(18.6412909463146,21.3259720589247,3.30335051562821));
#183388=CARTESIAN_POINT('Ctrl Pts',(18.637719764109,21.3258124965392,3.30313400657374));
#183389=CARTESIAN_POINT('Ctrl Pts',(18.6300627564796,21.3254509413526,3.30267084153737));
#183390=CARTESIAN_POINT('Ctrl Pts',(18.6259771188513,21.3252461521255,3.3024243438694));
#183391=CARTESIAN_POINT('Ctrl Pts',(18.6147485609045,21.3246506966316,3.30174858745225));
#183392=CARTESIAN_POINT('Ctrl Pts',(18.6076069109588,21.3242356620749,3.30132067296169));
#183393=CARTESIAN_POINT('Ctrl Pts',(18.5692538596805,21.3218116650463,3.29903209819803));
#183394=CARTESIAN_POINT('Ctrl Pts',(18.5380859935346,21.3191473175594,3.29720596567535));
#183395=CARTESIAN_POINT('Ctrl Pts',(18.3441682524776,21.2982322516267,3.28599160251349));
#183396=CARTESIAN_POINT('Ctrl Pts',(18.1839199038445,21.2618367735806,3.27733779268349));
#183397=CARTESIAN_POINT('Ctrl Pts',(17.9189817596118,21.1683346937134,3.26195873073173));
#183398=CARTESIAN_POINT('Ctrl Pts',(17.811948499755,21.1202484320958,3.25541971901464));
#183399=CARTESIAN_POINT('Ctrl Pts',(17.6958251729989,21.0560269397287,3.24764591143057));
#183400=CARTESIAN_POINT('Ctrl Pts',(17.6822851307129,21.0483424270285,3.24672870003757));
#183401=CARTESIAN_POINT('Ctrl Pts',(17.6618321281323,21.0364343728368,3.24532617168034));
#183402=CARTESIAN_POINT('Ctrl Pts',(17.6548564343652,21.0323192353244,3.24484477588477));
#183403=CARTESIAN_POINT('Ctrl Pts',(17.6425640469567,21.0249722353528,3.2439909858391));
#183404=CARTESIAN_POINT('Ctrl Pts',(17.6372376368637,21.0217567555465,3.24361919289713));
#183405=CARTESIAN_POINT('Ctrl Pts',(17.6260012659012,21.0149057484972,3.24283094018733));
#183406=CARTESIAN_POINT('Ctrl Pts',(17.6200948595312,21.0112645584687,3.24241427518402));
#183407=CARTESIAN_POINT('Ctrl Pts',(17.6080445688555,21.0037537720816,3.24155938694752));
#183408=CARTESIAN_POINT('Ctrl Pts',(17.601902484024,20.9998814752524,3.24112106738305));
#183409=CARTESIAN_POINT('Ctrl Pts',(17.5867627192464,20.9902273627482,3.24003418996783));
#183410=CARTESIAN_POINT('Ctrl Pts',(17.5777887767252,20.9844088607213,3.23938427290224));
#183411=CARTESIAN_POINT('Ctrl Pts',(17.4713805459955,20.9142651807854,3.23160918159758));
#183412=CARTESIAN_POINT('Ctrl Pts',(17.3794004148437,20.8420647772176,3.22418040724886));
#183413=CARTESIAN_POINT('Ctrl Pts',(17.1577437695693,20.6363380216564,3.2044361289185));
#183414=CARTESIAN_POINT('Ctrl Pts',(17.0388511505898,20.4926569312126,3.19186383498346));
#183415=CARTESIAN_POINT('Ctrl Pts',(16.9326662375027,20.3232447509699,3.17941672835761));
#183416=CARTESIAN_POINT('Ctrl Pts',(16.9252264936724,20.3111046031519,3.17853708500483));
#183417=CARTESIAN_POINT('Ctrl Pts',(16.9150503854746,20.2941169173346,3.17732423590825));
#183418=CARTESIAN_POINT('Ctrl Pts',(16.9122099917785,20.2893325666758,3.17698462158532));
#183419=CARTESIAN_POINT('Ctrl Pts',(16.9076809613787,20.2816349083197,3.17644142984464));
#183420=CARTESIAN_POINT('Ctrl Pts',(16.9059803786263,20.2787287117915,3.1762370850464));
#183421=CARTESIAN_POINT('Ctrl Pts',(16.9024426117123,20.272649648161,3.17581119511931));
#183422=CARTESIAN_POINT('Ctrl Pts',(16.9006067300006,20.2694760553603,3.17558973909762));
#183423=CARTESIAN_POINT('Ctrl Pts',(16.8961856382146,20.2617875328341,3.17505531800721));
#183424=CARTESIAN_POINT('Ctrl Pts',(16.8936087875205,20.2572677735092,3.17474289135675));
#183425=CARTESIAN_POINT('Ctrl Pts',(16.8846534276858,20.2414247448557,3.17365364772372));
#183426=CARTESIAN_POINT('Ctrl Pts',(16.878362399302,20.2300520168971,3.17288224902732));
#183427=CARTESIAN_POINT('Ctrl Pts',(16.8418446088517,20.1625766114885,3.16836284648239));
#183428=CARTESIAN_POINT('Ctrl Pts',(16.8140559972057,20.1051849070304,3.16475095998148));
#183429=CARTESIAN_POINT('Ctrl Pts',(16.7733771411984,20.0104954526878,3.15902267577751));
#183430=CARTESIAN_POINT('Ctrl Pts',(16.7588808356048,19.9739768425109,3.15686676387554));
#183431=CARTESIAN_POINT('Ctrl Pts',(16.7454192904822,19.9371100204058,3.15472448980525));
#183432=CARTESIAN_POINT('Ctrl Pts',(16.7454193815904,19.9371102699218,2.93545674419276));
#183433=CARTESIAN_POINT('Ctrl Pts',(16.7888438165966,20.0560357188456,2.9427087427267));
#183434=CARTESIAN_POINT('Ctrl Pts',(16.842869814061,20.1708827553276,2.94951932184116));
#183435=CARTESIAN_POINT('Ctrl Pts',(16.9474347316042,20.3495612776988,2.9607700351766));
#183436=CARTESIAN_POINT('Ctrl Pts',(16.9919020020283,20.4165002381309,2.96515171230137));
#183437=CARTESIAN_POINT('Ctrl Pts',(17.0691830410257,20.5195988133736,2.97235633827638));
#183438=CARTESIAN_POINT('Ctrl Pts',(17.0996305576116,20.5574332223459,2.97510777916505));
#183439=CARTESIAN_POINT('Ctrl Pts',(17.1516600481911,20.6177179978778,2.97970139741259));
#183440=CARTESIAN_POINT('Ctrl Pts',(17.1724847726145,20.6407990403733,2.98151393278074));
#183441=CARTESIAN_POINT('Ctrl Pts',(17.2008236769895,20.6708506399273,2.98395107201981));
#183442=CARTESIAN_POINT('Ctrl Pts',(17.2078917018916,20.6782378761561,2.98455657376902));
#183443=CARTESIAN_POINT('Ctrl Pts',(17.2198177092573,20.690523090417,2.98557450218282));
#183444=CARTESIAN_POINT('Ctrl Pts',(17.2246466703181,20.6954490928025,2.98598566080853));
#183445=CARTESIAN_POINT('Ctrl Pts',(17.2340420891884,20.7049400779573,2.9867837288943));
#183446=CARTESIAN_POINT('Ctrl Pts',(17.2386055310559,20.7095079484448,2.98717050298134));
#183447=CARTESIAN_POINT('Ctrl Pts',(17.2491925704219,20.7200087408093,2.98806588421118));
#183448=CARTESIAN_POINT('Ctrl Pts',(17.2552309254785,20.7259265671207,2.98857514749535));
#183449=CARTESIAN_POINT('Ctrl Pts',(17.2715701678263,20.7417488988815,2.98994946803813));
#183450=CARTESIAN_POINT('Ctrl Pts',(17.2819360220103,20.751585406125,2.99081745344438));
#183451=CARTESIAN_POINT('Ctrl Pts',(17.3779765191944,20.8408910269106,2.99882522204315));
#183452=CARTESIAN_POINT('Ctrl Pts',(17.4699800068057,20.9132309151536,3.00626682640924));
#183453=CARTESIAN_POINT('Ctrl Pts',(17.7032741064157,21.0672808535762,3.02452801992163));
#183454=CARTESIAN_POINT('Ctrl Pts',(17.8489648297749,21.1409967095266,3.03548771682661));
#183455=CARTESIAN_POINT('Ctrl Pts',(18.0321397643256,21.2085325933386,3.0478926931446));
#183456=CARTESIAN_POINT('Ctrl Pts',(18.0628753890759,21.2190677967933,3.04992865328473));
#183457=CARTESIAN_POINT('Ctrl Pts',(18.1007423661343,21.2310807306317,3.05237155595379));
#183458=CARTESIAN_POINT('Ctrl Pts',(18.1076528430853,21.2332340694463,3.05281473115043));
#183459=CARTESIAN_POINT('Ctrl Pts',(18.1185038250503,21.2365543303391,3.05350633405705));
#183460=CARTESIAN_POINT('Ctrl Pts',(18.1224368393167,21.2377452695619,3.05375613172592));
#183461=CARTESIAN_POINT('Ctrl Pts',(18.1297949762233,21.2399499865597,3.05422179533168));
#183462=CARTESIAN_POINT('Ctrl Pts',(18.1332191590904,21.2409665367053,3.05443781659813));
#183463=CARTESIAN_POINT('Ctrl Pts',(18.1410416518625,21.2432673029967,3.05492977965259));
#183464=CARTESIAN_POINT('Ctrl Pts',(18.1454415598256,21.244545907242,3.05520539208649));
#183465=CARTESIAN_POINT('Ctrl Pts',(18.1589788682761,21.2484322047206,3.0560500916804));
#183466=CARTESIAN_POINT('Ctrl Pts',(18.1681298472089,21.2509927128683,3.05661650285559));
#183467=CARTESIAN_POINT('Ctrl Pts',(18.2505207023821,21.2734491864912,3.06167757166063));
#183468=CARTESIAN_POINT('Ctrl Pts',(18.3247723504347,21.2894571714883,3.06596582529913));
#183469=CARTESIAN_POINT('Ctrl Pts',(18.549793353905,21.3254387841469,3.0785782444002));
#183470=CARTESIAN_POINT('Ctrl Pts',(18.7020030680415,21.3332069250289,3.08663340571346));
#183471=CARTESIAN_POINT('Ctrl Pts',(18.9087591576203,21.321494113719,3.09814821965788));
#183472=CARTESIAN_POINT('Ctrl Pts',(18.9636353790275,21.3162299433859,3.10125575987805));
#183473=CARTESIAN_POINT('Ctrl Pts',(19.0522382603209,21.3042248893456,3.10639980685562));
#183474=CARTESIAN_POINT('Ctrl Pts',(19.086116913803,21.2987929758776,3.10839692523103));
#183475=CARTESIAN_POINT('Ctrl Pts',(19.1304751697484,21.2905704539348,3.11105757975755));
#183476=CARTESIAN_POINT('Ctrl Pts',(19.1410876609821,21.2885190643706,3.11169758741297));
#183477=CARTESIAN_POINT('Ctrl Pts',(19.1584464133113,21.2850255126441,3.11275029581444));
#183478=CARTESIAN_POINT('Ctrl Pts',(19.1652022408267,21.2836314700511,3.11316145526646));
#183479=CARTESIAN_POINT('Ctrl Pts',(19.1782682275935,21.2808686993638,3.1139595238048));
#183480=CARTESIAN_POINT('Ctrl Pts',(19.1845791825267,21.2795040704567,3.11434629751201));
#183481=CARTESIAN_POINT('Ctrl Pts',(19.1991392101263,21.2762859359822,3.11524167618479));
#183482=CARTESIAN_POINT('Ctrl Pts',(19.2073835778841,21.2744118510644,3.11575093728024));
#183483=CARTESIAN_POINT('Ctrl Pts',(19.2295316229063,21.2692375015141,3.11712524811891));
#183484=CARTESIAN_POINT('Ctrl Pts',(19.2434132902838,21.2658458058707,3.1179932259456));
#183485=CARTESIAN_POINT('Ctrl Pts',(19.3704809799966,21.2334327510907,3.12600041891884));
#183486=CARTESIAN_POINT('Ctrl Pts',(19.4810985669252,21.195232394466,3.13344140493276));
#183487=CARTESIAN_POINT('Ctrl Pts',(19.7368748262521,21.0824719579531,3.1517000702034));
#183488=CARTESIAN_POINT('Ctrl Pts',(19.8776957779812,20.9998893889129,3.16265778499397));
#183489=CARTESIAN_POINT('Ctrl Pts',(20.0336423808164,20.8824293663801,3.17506348767464));
#183490=CARTESIAN_POINT('Ctrl Pts',(20.0591645165765,20.862267912132,3.17710161022173));
#183491=CARTESIAN_POINT('Ctrl Pts',(20.089790084121,20.8369073375529,3.17954674175958));
#183492=CARTESIAN_POINT('Ctrl Pts',(20.0953429998953,20.832260824986,3.17999005981816));
#183493=CARTESIAN_POINT('Ctrl Pts',(20.1040104120163,20.8249322667531,3.18068183581329));
#183494=CARTESIAN_POINT('Ctrl Pts',(20.1071410616139,20.8222695355754,3.18093166481558));
#183495=CARTESIAN_POINT('Ctrl Pts',(20.1129780390042,20.8172756071552,3.18139735556651));
#183496=CARTESIAN_POINT('Ctrl Pts',(20.1156861914198,20.8149467032504,3.18161337283364));
#183497=CARTESIAN_POINT('Ctrl Pts',(20.1218543161038,20.8096151455945,3.18210528630179));
#183498=CARTESIAN_POINT('Ctrl Pts',(20.1253104376405,20.8066081140022,3.18238085340561));
#183499=CARTESIAN_POINT('Ctrl Pts',(20.1359022115561,20.7973320604515,3.18322527600377));
#183500=CARTESIAN_POINT('Ctrl Pts',(20.1430055698759,20.7910261163809,3.18379145806017));
#183501=CARTESIAN_POINT('Ctrl Pts',(20.2063661541298,20.734011205562,3.1888430881696));
#183502=CARTESIAN_POINT('Ctrl Pts',(20.2599132867403,20.680359199217,3.19312298397862));
#183503=CARTESIAN_POINT('Ctrl Pts',(20.339024856642,20.592091623838,3.19968395834863));
#183504=CARTESIAN_POINT('Ctrl Pts',(20.3666040791301,20.5593779038406,3.20202237579589));
#183505=CARTESIAN_POINT('Ctrl Pts',(20.4610725903443,20.4401706605752,3.21030324339247));
#183506=CARTESIAN_POINT('Ctrl Pts',(20.5222319092832,20.3493611012446,3.21618996196601));
#183507=CARTESIAN_POINT('Ctrl Pts',(20.6032437751801,20.2063140731562,3.22533110955767));
#183508=CARTESIAN_POINT('Ctrl Pts',(20.6285026711613,20.1573516153469,3.2284367983729));
#183509=CARTESIAN_POINT('Ctrl Pts',(20.6663441304474,20.076396514243,3.23357805384042));
#183510=CARTESIAN_POINT('Ctrl Pts',(20.6801078982327,20.0449837033386,3.23557428814808));
#183511=CARTESIAN_POINT('Ctrl Pts',(20.6971975823155,20.003250621606,3.23823393176517));
#183512=CARTESIAN_POINT('Ctrl Pts',(20.7012163274404,19.9932184535927,3.23887383539348));
#183513=CARTESIAN_POINT('Ctrl Pts',(20.7076739312553,19.9767334997025,3.23992641627247));
#183514=CARTESIAN_POINT('Ctrl Pts',(20.7101584072572,19.9702987074785,3.24033755296232));
#183515=CARTESIAN_POINT('Ctrl Pts',(20.7149076159217,19.9578170524806,3.24113560847535));
#183516=CARTESIAN_POINT('Ctrl Pts',(20.717176221123,19.9517717376032,3.24152239208429));
#183517=CARTESIAN_POINT('Ctrl Pts',(20.7223517018704,19.9377860813852,3.24241783907507));
#183518=CARTESIAN_POINT('Ctrl Pts',(20.7252387172747,19.9298385535096,3.24292715890185));
#183519=CARTESIAN_POINT('Ctrl Pts',(20.7328775826639,19.9084107156541,3.24430173100157));
#183520=CARTESIAN_POINT('Ctrl Pts',(20.7375405874086,19.8948994046376,3.24516991309015));
#183521=CARTESIAN_POINT('Ctrl Pts',(20.7791461011179,19.7702665896041,3.25319285228735));
#183522=CARTESIAN_POINT('Ctrl Pts',(20.8069399457499,19.6563243978833,3.2606507587467));
#183523=CARTESIAN_POINT('Ctrl Pts',(20.850637683637,19.3791524371772,3.27898078895461));
#183524=CARTESIAN_POINT('Ctrl Pts',(20.8573023189426,19.2152173779122,3.2899950743259));
#183525=CARTESIAN_POINT('Ctrl Pts',(20.8426631836432,19.0206710324036,3.30238089400103));
#183526=CARTESIAN_POINT('Ctrl Pts',(20.8395905040362,18.9892469513951,3.30435813089164));
#183527=CARTESIAN_POINT('Ctrl Pts',(20.834958191279,18.950778653771,3.30674040830874));
#183528=CARTESIAN_POINT('Ctrl Pts',(20.8340642497277,18.943660102215,3.30717963553787));
#183529=CARTESIAN_POINT('Ctrl Pts',(20.8326031973522,18.9324853836982,3.30786645376848));
#183530=CARTESIAN_POINT('Ctrl Pts',(20.8320604846544,18.928426160412,3.30811538428804));
#183531=CARTESIAN_POINT('Ctrl Pts',(20.8310220832004,18.9208273680417,3.30858030213779));
#183532=CARTESIAN_POINT('Ctrl Pts',(20.8305292158416,18.9172875196588,3.30879643955997));
#183533=CARTESIAN_POINT('Ctrl Pts',(20.8293810128716,18.909191117324,3.30928979997919));
#183534=CARTESIAN_POINT('Ctrl Pts',(20.828719779366,18.9046354498058,3.30956668640284));
#183535=CARTESIAN_POINT('Ctrl Pts',(20.8269506547889,18.892720336281,3.31028907731625));
#183536=CARTESIAN_POINT('Ctrl Pts',(20.8258187953795,18.8853644388208,3.31073326151981));
#183537=CARTESIAN_POINT('Ctrl Pts',(20.8180275874156,18.8364473642736,3.31367609690752));
#183538=CARTESIAN_POINT('Ctrl Pts',(20.8101683034888,18.7950836971355,3.31611160469689));
#183539=CARTESIAN_POINT('Ctrl Pts',(20.7652809927486,18.592060953506,3.32792429780905));
#183540=CARTESIAN_POINT('Ctrl Pts',(20.7105787554934,18.4348978885238,3.33666241121533));
#183541=CARTESIAN_POINT('Ctrl Pts',(20.5968915197295,18.2009466375424,3.35097834868492));
#183542=CARTESIAN_POINT('Ctrl Pts',(20.5500855008844,18.1190278970036,3.35626638273926));
#183543=CARTESIAN_POINT('Ctrl Pts',(20.4862296072675,18.0227945539469,3.36299242362801));
#183544=CARTESIAN_POINT('Ctrl Pts',(20.474211886118,18.005262333014,3.36423973092433));
#183545=CARTESIAN_POINT('Ctrl Pts',(20.4567405101453,17.9805793826487,3.366028640662));
#183546=CARTESIAN_POINT('Ctrl Pts',(20.4515018963831,17.9732774975678,3.3665620203287));
#183547=CARTESIAN_POINT('Ctrl Pts',(20.4423813400599,17.9607341337148,3.3674856091723));
#183548=CARTESIAN_POINT('Ctrl Pts',(20.4385213458098,17.9554767944505,3.36787496513259));
#183549=CARTESIAN_POINT('Ctrl Pts',(20.4310819709702,17.9454418541281,3.36862250979981));
#183550=CARTESIAN_POINT('Ctrl Pts',(20.4275065508397,17.94066138455,3.36898054142496));
#183551=CARTESIAN_POINT('Ctrl Pts',(20.4181518870015,17.9282635323524,3.36991410798059));
#183552=CARTESIAN_POINT('Ctrl Pts',(20.4123412186485,17.9206701301538,3.37049087620771));
#183553=CARTESIAN_POINT('Ctrl Pts',(20.3923265260562,17.8948787864966,3.37246716158348));
#183554=CARTESIAN_POINT('Ctrl Pts',(20.3778767688503,17.8768744368385,3.37387641519409));
#183555=CARTESIAN_POINT('Ctrl Pts',(20.2518700904684,17.7250262209856,3.38602298372876));
#183556=CARTESIAN_POINT('Ctrl Pts',(20.1244962580515,17.6052151820562,3.39745268855204));
#183557=CARTESIAN_POINT('Ctrl Pts',(19.912987640556,17.4504881924912,3.41476834823958));
#183558=CARTESIAN_POINT('Ctrl Pts',(19.8388846301562,17.4030604063571,3.42056300459969));
#183559=CARTESIAN_POINT('Ctrl Pts',(19.7287863473539,17.3418995489147,3.42860559252335));
#183560=CARTESIAN_POINT('Ctrl Pts',(19.695034526667,17.3243231785901,3.43099903614493));
#183561=CARTESIAN_POINT('Ctrl Pts',(19.6540061279172,17.3043444866022,3.43380724197334));
#183562=CARTESIAN_POINT('Ctrl Pts',(19.647169350151,17.3010606648069,3.43427187573751));
#183563=CARTESIAN_POINT('Ctrl Pts',(19.6365328792941,17.2960219542045,3.43498944221276));
#183564=CARTESIAN_POINT('Ctrl Pts',(19.6327454618046,17.2942415098216,3.43524391533606));
#183565=CARTESIAN_POINT('Ctrl Pts',(19.6257233363084,17.2909658362382,3.43571377399474));
#183566=CARTESIAN_POINT('Ctrl Pts',(19.622490160452,17.2894675559306,3.43592934266991));
#183567=CARTESIAN_POINT('Ctrl Pts',(19.615186898773,17.2861055385664,3.43641456369887));
#183568=CARTESIAN_POINT('Ctrl Pts',(19.6111146874282,17.2842465481617,3.43668392223838));
#183569=CARTESIAN_POINT('Ctrl Pts',(19.5991211358053,17.2788173188329,3.43747382049991));
#183570=CARTESIAN_POINT('Ctrl Pts',(19.5911835665603,17.275282863615,3.43799221431717));
#183571=CARTESIAN_POINT('Ctrl Pts',(19.5351571805879,17.2507475382872,3.44162204726622));
#183572=CARTESIAN_POINT('Ctrl Pts',(19.4863196592021,17.2314903013438,3.4446354357532));
#183573=CARTESIAN_POINT('Ctrl Pts',(19.4341006648784,17.2131120337244,3.44775095004734));
#183574=CARTESIAN_POINT('Ctrl Pts',(19.4313865855177,17.2121630338578,3.44791257927123));
#183575=CARTESIAN_POINT('Ctrl Pts',(19.289263182848,17.1627931413185,3.45636107009442));
#183576=CARTESIAN_POINT('Ctrl Pts',(19.145167404338,17.1290740964683,3.46418617869217));
#183577=CARTESIAN_POINT('Ctrl Pts',(18.9017617407453,17.0983957175669,3.47766680584885));
#183578=CARTESIAN_POINT('Ctrl Pts',(18.8040761375589,17.0929048787396,3.48313954024638));
#183579=CARTESIAN_POINT('Ctrl Pts',(18.6847008455892,17.0944631785398,3.49008936849941));
#183580=CARTESIAN_POINT('Ctrl Pts',(18.6630404484748,17.0950786370934,3.49136057142821));
#183581=CARTESIAN_POINT('Ctrl Pts',(18.6323461929285,17.0964226140365,3.4931778207493));
#183582=CARTESIAN_POINT('Ctrl Pts',(18.6233012429599,17.09687682501,3.49371527921302));
#183583=CARTESIAN_POINT('Ctrl Pts',(18.60773510642,17.0977586786699,3.49464370211374));
#183584=CARTESIAN_POINT('Ctrl Pts',(18.6012124251245,17.0981585094925,3.49503378913057));
#183585=CARTESIAN_POINT('Ctrl Pts',(18.5887492823287,17.0989804225382,3.49578119034145));
#183586=CARTESIAN_POINT('Ctrl Pts',(18.5828085370981,17.0993973842161,3.49613833999094));
#183587=CARTESIAN_POINT('Ctrl Pts',(18.5674132512408,17.1005432308385,3.49706622752736));
#183588=CARTESIAN_POINT('Ctrl Pts',(18.5579617840153,17.101310577052,3.49763816916063));
#183589=CARTESIAN_POINT('Ctrl Pts',(18.525997458932,17.1041219906394,3.49958037701081));
#183590=CARTESIAN_POINT('Ctrl Pts',(18.5035128963335,17.1064630826981,3.50095993055254));
#183591=CARTESIAN_POINT('Ctrl Pts',(18.3020350935236,17.1307083678691,3.51344598240394));
#183592=CARTESIAN_POINT('Ctrl Pts',(18.1265177986523,17.1750366007595,3.52530095125202));
#183593=CARTESIAN_POINT('Ctrl Pts',(17.880919245885,17.2716847736613,3.54273407999321));
#183594=CARTESIAN_POINT('Ctrl Pts',(17.8049370367176,17.3069164525899,3.54824059718542));
#183595=CARTESIAN_POINT('Ctrl Pts',(17.6986806013986,17.3640649292396,3.55593786556592));
#183596=CARTESIAN_POINT('Ctrl Pts',(17.6665872811858,17.3824251764925,3.55826173456031));
#183597=CARTESIAN_POINT('Ctrl Pts',(17.6285601012713,17.4055227191648,3.56099931786265));
#183598=CARTESIAN_POINT('Ctrl Pts',(17.6221518101811,17.4094619937365,3.56146009139507));
#183599=CARTESIAN_POINT('Ctrl Pts',(17.6122225237722,17.4156388400008,3.56217299284663));
#183600=CARTESIAN_POINT('Ctrl Pts',(17.6086869903064,17.4178527578826,3.56242662989085));
#183601=CARTESIAN_POINT('Ctrl Pts',(17.6021423738702,17.4219779148723,3.5628957184863));
#183602=CARTESIAN_POINT('Ctrl Pts',(17.5991316014956,17.4238862864196,3.56311134825268));
#183603=CARTESIAN_POINT('Ctrl Pts',(17.5923358773359,17.4282178406188,3.56359768455261));
#183604=CARTESIAN_POINT('Ctrl Pts',(17.5885538231774,17.4306454696761,3.56386809129828));
#183605=CARTESIAN_POINT('Ctrl Pts',(17.5774135313311,17.4378464061516,3.56466392390217));
#183606=CARTESIAN_POINT('Ctrl Pts',(17.5700770904319,17.4426534860251,3.56518715528834));
#183607=CARTESIAN_POINT('Ctrl Pts',(17.5172400435089,17.4777453588312,3.56895081489696));
#183608=CARTESIAN_POINT('Ctrl Pts',(17.4728934029473,17.5097393842686,3.5720847551078));
#183609=CARTESIAN_POINT('Ctrl Pts',(17.297250717459,17.6471044830489,3.58461109107506));
#183610=CARTESIAN_POINT('Ctrl Pts',(17.17750277928,17.7662364824458,3.59346953724732));
#183611=CARTESIAN_POINT('Ctrl Pts',(17.0365790409051,17.9445386110824,3.60606881828863));
#183612=CARTESIAN_POINT('Ctrl Pts',(17.001983831978,17.9922787063494,3.60938273608767));
#183613=CARTESIAN_POINT('Ctrl Pts',(16.9495309651219,18.0714140607528,3.61483688368836));
#183614=CARTESIAN_POINT('Ctrl Pts',(16.9304052176692,18.1019321552546,3.61693119722609));
#183615=CARTESIAN_POINT('Ctrl Pts',(16.9064660224197,18.1423889545513,3.61970280990592));
#183616=CARTESIAN_POINT('Ctrl Pts',(16.9009381182918,18.1518993737209,3.62035400213238));
#183617=CARTESIAN_POINT('Ctrl Pts',(16.8920438745124,18.1674796124726,3.62142042870922));
#183618=CARTESIAN_POINT('Ctrl Pts',(16.888632778462,18.1735237432517,3.62183404219457));
#183619=CARTESIAN_POINT('Ctrl Pts',(16.8821134430049,18.1852092487347,3.62263358139292));
#183620=CARTESIAN_POINT('Ctrl Pts',(16.879001103691,18.1908482570564,3.62301935422731));
#183621=CARTESIAN_POINT('Ctrl Pts',(16.8719106580075,18.2038346258148,3.62390768443774));
#183622=CARTESIAN_POINT('Ctrl Pts',(16.8679502372614,18.2111914741425,3.62441086542054));
#183623=CARTESIAN_POINT('Ctrl Pts',(16.8574948764112,18.2308918094754,3.62575822270598));
#183624=CARTESIAN_POINT('Ctrl Pts',(16.8510782839663,18.2432762064191,3.62660515107105));
#183625=CARTESIAN_POINT('Ctrl Pts',(16.800137530275,18.3440198034776,3.633495157055));
#183626=CARTESIAN_POINT('Ctrl Pts',(16.7617417211774,18.4353253610798,3.63975148057327));
#183627=CARTESIAN_POINT('Ctrl Pts',(16.6860055179091,18.6578740565154,3.65499319268893));
#183628=CARTESIAN_POINT('Ctrl Pts',(16.6546777558883,18.7907082759852,3.66409684657822));
#183629=CARTESIAN_POINT('Ctrl Pts',(16.6262468700561,18.9996860794504,3.67787830996548));
#183630=CARTESIAN_POINT('Ctrl Pts',(16.6200989475176,19.0742460100602,3.68268510272746));
#183631=CARTESIAN_POINT('Ctrl Pts',(16.6176490858976,19.1578371891601,3.68784414803085));
#183632=CARTESIAN_POINT('Ctrl Pts',(16.6174451480605,19.1666937802207,3.68838785452539));
#183633=CARTESIAN_POINT('Ctrl Pts',(16.6172222390665,19.1800041618254,3.68920035751529));
#183634=CARTESIAN_POINT('Ctrl Pts',(16.6171617202339,19.1844570287512,3.68947139586155));
#183635=CARTESIAN_POINT('Ctrl Pts',(16.6170816555811,19.1921296594547,3.68993703801595));
#183636=CARTESIAN_POINT('Ctrl Pts',(16.6170554039638,19.1953492978433,3.69013201417728));
#183637=CARTESIAN_POINT('Ctrl Pts',(16.6170125976395,19.2026391212519,3.69057251818924));
#183638=CARTESIAN_POINT('Ctrl Pts',(16.617000435401,19.2067092918388,3.69081779729758));
#183639=CARTESIAN_POINT('Ctrl Pts',(16.6169992761378,19.2178398538869,3.69148678276288));
#183640=CARTESIAN_POINT('Ctrl Pts',(16.6170338608861,19.2249002690473,3.69190918932611));
#183641=CARTESIAN_POINT('Ctrl Pts',(16.6174008065008,19.2619597899229,3.69411674934474));
#183642=CARTESIAN_POINT('Ctrl Pts',(16.6183355257014,19.2919511380406,3.69587020382201));
#183643=CARTESIAN_POINT('Ctrl Pts',(16.6230423747871,19.3816665828137,3.7010431490907));
#183644=CARTESIAN_POINT('Ctrl Pts',(16.6287093229192,19.4412636993934,3.70438374006535));
#183645=CARTESIAN_POINT('Ctrl Pts',(16.6574679249874,19.6495557923784,3.7159609047263));
#183646=CARTESIAN_POINT('Ctrl Pts',(16.693857304765,19.7958984467168,3.72394888923627));
#183647=CARTESIAN_POINT('Ctrl Pts',(16.7454193623262,19.9371102171632,3.73234496441554));
#183648=CARTESIAN_POINT('Origin',(18.734,19.211,0.));
#183649=CARTESIAN_POINT('',(16.745419360568,19.9371102123481,4.75730092050388));
#183650=CARTESIAN_POINT('',(16.7454193895773,19.9371102917951,4.53222340700496));
#183651=CARTESIAN_POINT('',(16.7454193623258,19.9371102171621,0.));
#183652=CARTESIAN_POINT('',(16.6170000778091,19.2104260280332,4.70909169803339));
#183653=CARTESIAN_POINT('Ctrl Pts',(16.745419360568,19.9371102123481,4.75730092050388));
#183654=CARTESIAN_POINT('Ctrl Pts',(16.7278325677703,19.8889456843294,4.7540835371879));
#183655=CARTESIAN_POINT('Ctrl Pts',(16.7120013965261,19.8401580434368,4.75081295266123));
#183656=CARTESIAN_POINT('Ctrl Pts',(16.6441871892237,19.6020374009016,4.73481653533855));
#183657=CARTESIAN_POINT('Ctrl Pts',(16.6169468631223,19.4066995299123,4.72148364047144));
#183658=CARTESIAN_POINT('Ctrl Pts',(16.6170000778091,19.2104260280332,4.70909169803339));
#183659=CARTESIAN_POINT('Ctrl Pts',(16.6170000784465,19.2104236820643,4.70909154991813));
#183660=CARTESIAN_POINT('Ctrl Pts',(16.6170043637984,19.1946822152069,4.7080976958813));
#183661=CARTESIAN_POINT('Ctrl Pts',(16.61718422352,19.1789407204702,4.70711096664662));
#183662=CARTESIAN_POINT('Ctrl Pts',(16.6177851446148,19.1523322925812,4.70545671999246));
#183663=CARTESIAN_POINT('Ctrl Pts',(16.6181143693901,19.1414642294231,4.70478490712336));
#183664=CARTESIAN_POINT('Ctrl Pts',(16.6187085002863,19.1258317544558,4.70382459025789));
#183665=CARTESIAN_POINT('Ctrl Pts',(16.6189057981698,19.1210651502801,4.70353257788567));
#183666=CARTESIAN_POINT('Ctrl Pts',(16.6192791186639,19.1127280680581,4.70302328572276));
#183667=CARTESIAN_POINT('Ctrl Pts',(16.6194480743017,19.1091573148174,4.70280562422508));
#183668=CARTESIAN_POINT('Ctrl Pts',(16.6197955283655,19.1021880828528,4.7023817372304));
#183669=CARTESIAN_POINT('Ctrl Pts',(16.6199731789515,19.0987895650075,4.70217546500797));
#183670=CARTESIAN_POINT('Ctrl Pts',(16.6203449449137,19.0919920226564,4.70176377589654));
#183671=CARTESIAN_POINT('Ctrl Pts',(16.620539064392,19.0885930369605,4.70155835900012));
#183672=CARTESIAN_POINT('Ctrl Pts',(16.6210263189945,19.0804082195942,4.7010647413133));
#183673=CARTESIAN_POINT('Ctrl Pts',(16.6213275168543,19.0756228611888,4.70077698963592));
#183674=CARTESIAN_POINT('Ctrl Pts',(16.6224923818642,19.0580673362408,4.69972432499825));
#183675=CARTESIAN_POINT('Ctrl Pts',(16.6234556168969,19.045303753542,4.69896478033461));
#183676=CARTESIAN_POINT('Ctrl Pts',(16.6267051775263,19.0068906935396,4.69669420547832));
#183677=CARTESIAN_POINT('Ctrl Pts',(16.629343849213,18.9812725791769,4.695200552628));
#183678=CARTESIAN_POINT('Ctrl Pts',(16.6544361109332,18.7747145114139,4.68327865541669));
#183679=CARTESIAN_POINT('Ctrl Pts',(16.6997133937434,18.5973029667728,4.67373447942496));
#183680=CARTESIAN_POINT('Ctrl Pts',(16.7997460845995,18.3460701586725,4.65880486824974));
#183681=CARTESIAN_POINT('Ctrl Pts',(16.837386179554,18.2663861571441,4.6538477966998));
#183682=CARTESIAN_POINT('Ctrl Pts',(16.8897666853855,18.1713305359165,4.6475220897332));
#183683=CARTESIAN_POINT('Ctrl Pts',(16.8999188137765,18.1535241033014,4.64631864737917));
#183684=CARTESIAN_POINT('Ctrl Pts',(16.9148254325188,18.1282390247297,4.64458188054752));
#183685=CARTESIAN_POINT('Ctrl Pts',(16.9193710093483,18.1206381063182,4.64405612911386));
#183686=CARTESIAN_POINT('Ctrl Pts',(16.9273346985559,18.1075092992296,4.64314154097948));
#183687=CARTESIAN_POINT('Ctrl Pts',(16.9307308433286,18.1019681766182,4.64275351260169));
#183688=CARTESIAN_POINT('Ctrl Pts',(16.9373104942306,18.0913429982608,4.64200553083691));
#183689=CARTESIAN_POINT('Ctrl Pts',(16.9404902033203,18.0862566560551,4.64164572019096));
#183690=CARTESIAN_POINT('Ctrl Pts',(16.9488782202422,18.0729649895568,4.64070083322307));
#183691=CARTESIAN_POINT('Ctrl Pts',(16.9541214456695,18.0647819664361,4.6401144641528));
#183692=CARTESIAN_POINT('Ctrl Pts',(16.972522401082,18.0364945825453,4.63807108359136));
#183693=CARTESIAN_POINT('Ctrl Pts',(16.9859655294557,18.0165789175181,4.63660342561447));
#183694=CARTESIAN_POINT('Ctrl Pts',(17.0837213670924,17.8769419853157,4.62610101572627));
#183695=CARTESIAN_POINT('Ctrl Pts',(17.179902504675,17.7660441907809,4.61659536390066));
#183696=CARTESIAN_POINT('Ctrl Pts',(17.3663203626474,17.591421911081,4.59973664771492));
#183697=CARTESIAN_POINT('Ctrl Pts',(17.4515512190127,17.5231291555232,4.59248962796451));
#183698=CARTESIAN_POINT('Ctrl Pts',(17.5653061675201,17.4455929327199,4.58366375732444));
#183699=CARTESIAN_POINT('Ctrl Pts',(17.5892701213525,17.4299606816151,4.5818487576108));
#183700=CARTESIAN_POINT('Ctrl Pts',(17.6237470527143,17.4084540271461,4.57930746203041));
#183701=CARTESIAN_POINT('Ctrl Pts',(17.6340037024147,17.4021766943717,4.57856003645289));
#183702=CARTESIAN_POINT('Ctrl Pts',(17.6498689037046,17.3926516416282,4.57741771911225));
#183703=CARTESIAN_POINT('Ctrl Pts',(17.655439637811,17.3893418174921,4.5770192118189));
#183704=CARTESIAN_POINT('Ctrl Pts',(17.6646954088453,17.3838998892428,4.57636149151379));
#183705=CARTESIAN_POINT('Ctrl Pts',(17.6683717933226,17.3817532563253,4.57610138842673));
#183706=CARTESIAN_POINT('Ctrl Pts',(17.6755037846931,17.3776176998128,4.57559904941793));
#183707=CARTESIAN_POINT('Ctrl Pts',(17.6789585811857,17.3756274215703,4.5753567281989));
#183708=CARTESIAN_POINT('Ctrl Pts',(17.6854556785708,17.3719089071104,4.57490295328743));
#183709=CARTESIAN_POINT('Ctrl Pts',(17.6884966058051,17.3701784728348,4.57469136268995));
#183710=CARTESIAN_POINT('Ctrl Pts',(17.6955301546883,17.3661990952099,4.57420378054315));
#183711=CARTESIAN_POINT('Ctrl Pts',(17.6995257914741,17.3639555742385,4.57392813911222));
#183712=CARTESIAN_POINT('Ctrl Pts',(17.7118313607079,17.3570985433665,4.57308326245629));
#183713=CARTESIAN_POINT('Ctrl Pts',(17.7201652351334,17.3525279353114,4.57251670484441));
#183714=CARTESIAN_POINT('Ctrl Pts',(17.8341057564339,17.2910332323665,4.5648432674565));
#183715=CARTESIAN_POINT('Ctrl Pts',(17.9443507123299,17.2431218460717,4.55825736830397));
#183716=CARTESIAN_POINT('Ctrl Pts',(18.1612061090215,17.1700591808931,4.5458024745412));
#183717=CARTESIAN_POINT('Ctrl Pts',(18.2668613705971,17.1433170391643,4.53993996763126));
#183718=CARTESIAN_POINT('Ctrl Pts',(18.4478899559138,17.1120866870742,4.52972021388724));
#183719=CARTESIAN_POINT('Ctrl Pts',(18.5222968787215,17.1032817678786,4.52547353616279));
#183720=CARTESIAN_POINT('Ctrl Pts',(18.6157555105095,17.0972213564375,4.52000497375922));
#183721=CARTESIAN_POINT('Ctrl Pts',(18.6345170069107,17.096255331323,4.51890059880665));
#183722=CARTESIAN_POINT('Ctrl Pts',(18.6618325982199,17.0952131546314,4.51728219362356));
#183723=CARTESIAN_POINT('Ctrl Pts',(18.6703785558973,17.0949389381465,4.51677436661677));
#183724=CARTESIAN_POINT('Ctrl Pts',(18.6853723407897,17.0945487399419,4.51588068232854));
#183725=CARTESIAN_POINT('Ctrl Pts',(18.6918195127689,17.0944104340902,4.51549552961081));
#183726=CARTESIAN_POINT('Ctrl Pts',(18.7043451869666,17.0941989831386,4.5147455051637));
#183727=CARTESIAN_POINT('Ctrl Pts',(18.7104235761975,17.0941225581145,4.51438074014408));
#183728=CARTESIAN_POINT('Ctrl Pts',(18.7249640896626,17.0940023709399,4.51350621890186));
#183729=CARTESIAN_POINT('Ctrl Pts',(18.7334262632324,17.0939831657035,4.51299569770762));
#183730=CARTESIAN_POINT('Ctrl Pts',(18.7640159917895,17.0940971479788,4.51114440738714));
#183731=CARTESIAN_POINT('Ctrl Pts',(18.7861404089094,17.094526526485,4.50979441237954));
#183732=CARTESIAN_POINT('Ctrl Pts',(18.9935807666004,17.1018069392241,4.4970291282802));
#183733=CARTESIAN_POINT('Ctrl Pts',(19.1772172861537,17.1326332277532,4.48481601825516));
#183734=CARTESIAN_POINT('Ctrl Pts',(19.4311711120825,17.2104796833393,4.46727914861177));
#183735=CARTESIAN_POINT('Ctrl Pts',(19.5065033666126,17.238344590235,4.46200621723894));
#183736=CARTESIAN_POINT('Ctrl Pts',(19.6131283199232,17.2848321621284,4.45459117425866));
#183737=CARTESIAN_POINT('Ctrl Pts',(19.6458097224811,17.3000859434502,4.45232574053615));
#183738=CARTESIAN_POINT('Ctrl Pts',(19.6847718454635,17.3194985677729,4.44964764225537));
#183739=CARTESIAN_POINT('Ctrl Pts',(19.6914385166342,17.3228643425514,4.44919022194102));
#183740=CARTESIAN_POINT('Ctrl Pts',(19.7017906431506,17.3281597056926,4.44848137483088));
#183741=CARTESIAN_POINT('Ctrl Pts',(19.7054883812649,17.3300649589653,4.44822846586572));
#183742=CARTESIAN_POINT('Ctrl Pts',(19.7123454784386,17.3336236818843,4.44776004112421));
#183743=CARTESIAN_POINT('Ctrl Pts',(19.7155062457025,17.335274219155,4.44754435143771));
#183744=CARTESIAN_POINT('Ctrl Pts',(19.7226552535959,17.339030414641,4.44705701340235));
#183745=CARTESIAN_POINT('Ctrl Pts',(19.7266409346933,17.3411408302741,4.44678567017114));
#183746=CARTESIAN_POINT('Ctrl Pts',(19.7386829809241,17.3475664400183,4.44596683792301));
#183747=CARTESIAN_POINT('Ctrl Pts',(19.7467182970182,17.3519211468294,4.44542179232326));
#183748=CARTESIAN_POINT('Ctrl Pts',(19.8089338868011,17.3861617147272,4.44121009058585));
#183749=CARTESIAN_POINT('Ctrl Pts',(19.8618139611038,17.4183609351148,4.43768016365321));
#183750=CARTESIAN_POINT('Ctrl Pts',(20.0480478728177,17.5432690828335,4.42515321751982));
#183751=CARTESIAN_POINT('Ctrl Pts',(20.172036699504,17.6489167148348,4.41658701722823));
#183752=CARTESIAN_POINT('Ctrl Pts',(20.3221663732146,17.810014105773,4.40436897578582));
#183753=CARTESIAN_POINT('Ctrl Pts',(20.3598434748568,17.8539199835302,4.40111432068953));
#183754=CARTESIAN_POINT('Ctrl Pts',(20.4176865683165,17.927196780438,4.39574900570804));
#183755=CARTESIAN_POINT('Ctrl Pts',(20.4389925446789,17.9556309817743,4.39368233019728));
#183756=CARTESIAN_POINT('Ctrl Pts',(20.4659137578264,17.9935093158942,4.39094223313347));
#183757=CARTESIAN_POINT('Ctrl Pts',(20.4721859738856,18.0024809294799,4.39029417112524));
#183758=CARTESIAN_POINT('Ctrl Pts',(20.4823139372084,18.0172096579666,4.38923158516815));
#183759=CARTESIAN_POINT('Ctrl Pts',(20.4862115481139,18.0229378414109,4.38881865966345));
#183760=CARTESIAN_POINT('Ctrl Pts',(20.4936804701436,18.0340313584589,4.38801954543776));
#183761=CARTESIAN_POINT('Ctrl Pts',(20.4972555405954,18.0393940776393,4.3876335047431));
#183762=CARTESIAN_POINT('Ctrl Pts',(20.505423717685,18.0517686706659,4.38674325918683));
#183763=CARTESIAN_POINT('Ctrl Pts',(20.5099997566758,18.0587916318574,4.38623842187732));
#183764=CARTESIAN_POINT('Ctrl Pts',(20.5221290586714,18.077650710054,4.38488374041003));
#183765=CARTESIAN_POINT('Ctrl Pts',(20.5296063806551,18.0895349518028,4.38403109688649));
#183766=CARTESIAN_POINT('Ctrl Pts',(20.5910212853854,18.1893350058202,4.37687823262409));
#183767=CARTESIAN_POINT('Ctrl Pts',(20.638577948641,18.2809974257249,4.37034549701392));
#183768=CARTESIAN_POINT('Ctrl Pts',(20.7316506892097,18.4977595110238,4.35502184278328));
#183769=CARTESIAN_POINT('Ctrl Pts',(20.7724409863092,18.6244203378445,4.3461467261345));
#183770=CARTESIAN_POINT('Ctrl Pts',(20.8119977476574,18.803367633546,4.33417612650166));
#183771=CARTESIAN_POINT('Ctrl Pts',(20.8211299772893,18.8530503887307,4.33091401355052));
#183772=CARTESIAN_POINT('Ctrl Pts',(20.8323766311793,18.9295342342943,4.32602948191945));
#183773=CARTESIAN_POINT('Ctrl Pts',(20.8357723597768,18.9561263708105,4.32435641887075));
#183774=CARTESIAN_POINT('Ctrl Pts',(20.8393960422988,18.9895438402612,4.32229140049602));
#183775=CARTESIAN_POINT('Ctrl Pts',(20.8400971679454,18.9963140719649,4.32187495998678));
#183776=CARTESIAN_POINT('Ctrl Pts',(20.841159838324,19.007082059948,4.32121579789918));
#183777=CARTESIAN_POINT('Ctrl Pts',(20.8415426791791,19.0110775986074,4.32097190695017));
#183778=CARTESIAN_POINT('Ctrl Pts',(20.8422464399204,19.0186491769008,4.32051108075974));
#183779=CARTESIAN_POINT('Ctrl Pts',(20.8425696222616,19.0222248988379,4.32029402647977));
#183780=CARTESIAN_POINT('Ctrl Pts',(20.8432916071484,19.0304462515227,4.31979626683849));
#183781=CARTESIAN_POINT('Ctrl Pts',(20.8436841594525,19.0350923867969,4.31951591494739));
#183782=CARTESIAN_POINT('Ctrl Pts',(20.8446931466348,19.0475239106681,4.31876822860451));
#183783=CARTESIAN_POINT('Ctrl Pts',(20.8452818630818,19.0553115614127,4.31830240627529));
#183784=CARTESIAN_POINT('Ctrl Pts',(20.8493029369268,19.1127284213935,4.31488568765646));
#183785=CARTESIAN_POINT('Ctrl Pts',(20.8510283644945,19.1624658313344,4.31202326432112));
#183786=CARTESIAN_POINT('Ctrl Pts',(20.8509850454862,19.2375215172516,4.3077892818664));
#183787=CARTESIAN_POINT('Ctrl Pts',(20.8505169199288,19.2628196153999,4.30637685608441));
#183788=CARTESIAN_POINT('Ctrl Pts',(20.847966376092,19.3328020407431,4.30249608983154));
#183789=CARTESIAN_POINT('Ctrl Pts',(20.8449211244965,19.3774385824156,4.30005056331034));
#183790=CARTESIAN_POINT('Ctrl Pts',(20.8295689236847,19.5307423897801,4.29166236447816));
#183791=CARTESIAN_POINT('Ctrl Pts',(20.8102614474233,19.6385299134605,4.28577473614214));
#183792=CARTESIAN_POINT('Ctrl Pts',(20.7636491584859,19.8175816022643,4.27548688946047));
#183793=CARTESIAN_POINT('Ctrl Pts',(20.7406700897837,19.8897417442096,4.27119660343082));
#183794=CARTESIAN_POINT('Ctrl Pts',(20.7071894594262,19.978182741616,4.26567548336885));
#183795=CARTESIAN_POINT('Ctrl Pts',(20.7002638680072,19.9957626194925,4.26456481947438));
#183796=CARTESIAN_POINT('Ctrl Pts',(20.689856297566,20.0211781245116,4.26293887504148));
#183797=CARTESIAN_POINT('Ctrl Pts',(20.6865604452736,20.0290893315671,4.26242988068077));
#183798=CARTESIAN_POINT('Ctrl Pts',(20.6806994275023,20.0429206477881,4.26153484715167));
#183799=CARTESIAN_POINT('Ctrl Pts',(20.678155051288,20.0488494855182,4.26114951923809));
#183800=CARTESIAN_POINT('Ctrl Pts',(20.6731631215181,20.0603363703092,4.26039967737386));
#183801=CARTESIAN_POINT('Ctrl Pts',(20.6707186724163,20.0658957038753,4.26003527259443));
#183802=CARTESIAN_POINT('Ctrl Pts',(20.6648199476168,20.0791558408141,4.25916246134555));
#183803=CARTESIAN_POINT('Ctrl Pts',(20.6613434940297,20.0868466114845,4.25865329663248));
#183804=CARTESIAN_POINT('Ctrl Pts',(20.6486451341995,20.1144967788622,4.25681196863498));
#183805=CARTESIAN_POINT('Ctrl Pts',(20.6391586573169,20.1343324713022,4.25547070827276));
#183806=CARTESIAN_POINT('Ctrl Pts',(20.5461444221216,20.321281475077,4.24263087342255));
#183807=CARTESIAN_POINT('Ctrl Pts',(20.4411625535529,20.4767646797961,4.23032076965095));
#183808=CARTESIAN_POINT('Ctrl Pts',(20.2645101541816,20.6757604232352,4.2127549692487));
#183809=CARTESIAN_POINT('Ctrl Pts',(20.2085379075336,20.7320930542604,4.20754382136202));
#183810=CARTESIAN_POINT('Ctrl Pts',(20.1229024828073,20.8090993150867,4.2002037819797));
#183811=CARTESIAN_POINT('Ctrl Pts',(20.0956679702627,20.8323673916213,4.19795411955092));
#183812=CARTESIAN_POINT('Ctrl Pts',(20.0620668102219,20.8596306728855,4.19529210312768));
#183813=CARTESIAN_POINT('Ctrl Pts',(20.0562543606948,20.8642960888521,4.19483560586379));
#183814=CARTESIAN_POINT('Ctrl Pts',(20.0471621908427,20.8715153827546,4.19412787514434));
#183815=CARTESIAN_POINT('Ctrl Pts',(20.0438994494595,20.8740904090923,4.19387516690331));
#183816=CARTESIAN_POINT('Ctrl Pts',(20.0378232721616,20.8788568860486,4.193406924065));
#183817=CARTESIAN_POINT('Ctrl Pts',(20.0350119097749,20.8810508160734,4.19319121674709));
#183818=CARTESIAN_POINT('Ctrl Pts',(20.0286290682728,20.886005956539,4.19270359746959));
#183819=CARTESIAN_POINT('Ctrl Pts',(20.0250543020063,20.8887628464704,4.19243199211841));
#183820=CARTESIAN_POINT('Ctrl Pts',(20.0144334222189,20.8968997128722,4.19162934855027));
#183821=CARTESIAN_POINT('Ctrl Pts',(20.007362202665,20.9022469652986,4.19110056120902));
#183822=CARTESIAN_POINT('Ctrl Pts',(19.9544652561465,20.9417277724259,4.18718469241085));
#183823=CARTESIAN_POINT('Ctrl Pts',(19.9073036182297,20.9740410972697,4.18391410124965));
#183824=CARTESIAN_POINT('Ctrl Pts',(19.7306439796643,21.084848107821,4.17222252573817));
#183825=CARTESIAN_POINT('Ctrl Pts',(19.5941366166486,21.1513032000611,4.16420726557329));
#183826=CARTESIAN_POINT('Ctrl Pts',(19.3644837038337,21.2340605367309,4.15076198119429));
#183827=CARTESIAN_POINT('Ctrl Pts',(19.2753056437404,21.25972373936,4.14555620143176));
#183828=CARTESIAN_POINT('Ctrl Pts',(19.1641535764797,21.2839449564784,4.13892973150984));
#183829=CARTESIAN_POINT('Ctrl Pts',(19.1435026764916,21.2881231072552,4.13769319852282));
#183830=CARTESIAN_POINT('Ctrl Pts',(19.1139907029175,21.2936368521036,4.13591708175391));
#183831=CARTESIAN_POINT('Ctrl Pts',(19.1051777748455,21.2952255750641,4.13538555869002));
#183832=CARTESIAN_POINT('Ctrl Pts',(19.089934784856,21.2978737129783,4.13446416541299));
#183833=CARTESIAN_POINT('Ctrl Pts',(19.0835093761036,21.2989594487302,4.13407513744572));
#183834=CARTESIAN_POINT('Ctrl Pts',(19.0711817060508,21.3009840225588,4.13332750714668));
#183835=CARTESIAN_POINT('Ctrl Pts',(19.0652802731353,21.3019275685541,4.13296905845384));
#183836=CARTESIAN_POINT('Ctrl Pts',(19.0498903480064,21.3043213853953,4.13203282292778));
#183837=CARTESIAN_POINT('Ctrl Pts',(19.0403959264125,21.3057321227421,4.13145378884814));
#183838=CARTESIAN_POINT('Ctrl Pts',(19.007813275751,21.3103471890729,4.12946154353478));
#183839=CARTESIAN_POINT('Ctrl Pts',(18.9846825382579,21.3132346508188,4.12803838230219));
#183840=CARTESIAN_POINT('Ctrl Pts',(18.7917169114187,21.3340930616151,4.11608809622742));
#183841=CARTESIAN_POINT('Ctrl Pts',(18.6203576101351,21.3318298199412,4.10489913059937));
#183842=CARTESIAN_POINT('Ctrl Pts',(18.3616269040043,21.2969508424641,4.08764705330503));
#183843=CARTESIAN_POINT('Ctrl Pts',(18.2729430385332,21.2791588707252,4.08168387113909));
#183844=CARTESIAN_POINT('Ctrl Pts',(18.1483262681061,21.2457406615571,4.07344069716556));
#183845=CARTESIAN_POINT('Ctrl Pts',(18.1112679907923,21.2347066389032,4.07100779510073));
#183846=CARTESIAN_POINT('Ctrl Pts',(18.0672905625408,21.2202898173554,4.06815963130051));
#183847=CARTESIAN_POINT('Ctrl Pts',(18.0600637171953,21.2178774090351,4.06769286947869));
#183848=CARTESIAN_POINT('Ctrl Pts',(18.0488804371117,21.2140770731554,4.06697273236148));
#183849=CARTESIAN_POINT('Ctrl Pts',(18.0449149223821,21.2127163467786,4.06671779928892));
#183850=CARTESIAN_POINT('Ctrl Pts',(18.0375868579237,21.2101774383176,4.06624751356651));
#183851=CARTESIAN_POINT('Ctrl Pts',(18.0342232680884,21.2090025575856,4.06603197507602));
#183852=CARTESIAN_POINT('Ctrl Pts',(18.0266492763542,21.2063355374058,4.06554735206495));
#183853=CARTESIAN_POINT('Ctrl Pts',(18.0224406340152,21.2048385648285,4.06527855813702));
#183854=CARTESIAN_POINT('Ctrl Pts',(18.0101012265045,21.2004055128176,4.06449184810243));
#183855=CARTESIAN_POINT('Ctrl Pts',(18.0019835573429,21.1974328989824,4.06397605202905));
#183856=CARTESIAN_POINT('Ctrl Pts',(17.9455380684285,21.1763700891682,4.06040025890264));
#183857=CARTESIAN_POINT('Ctrl Pts',(17.8978634089018,21.1565663282831,4.05743505752371));
#183858=CARTESIAN_POINT('Ctrl Pts',(17.8310742971141,21.1259132445387,4.05329618696102));
#183859=CARTESIAN_POINT('Ctrl Pts',(17.8113344211655,21.1164804733937,4.05207488749926));
#183860=CARTESIAN_POINT('Ctrl Pts',(17.6684448828543,21.045458962789,4.04322466702742));
#183861=CARTESIAN_POINT('Ctrl Pts',(17.551416570879,20.9722911392629,4.03590130831542));
#183862=CARTESIAN_POINT('Ctrl Pts',(17.3704325365416,20.8329140651624,4.02330709170845));
#183863=CARTESIAN_POINT('Ctrl Pts',(17.3021867902169,20.7729954100742,4.01820659106598));
#183864=CARTESIAN_POINT('Ctrl Pts',(17.2232621122057,20.6941702018384,4.0117074889394));
#183865=CARTESIAN_POINT('Ctrl Pts',(17.2087434996877,20.6792354633583,4.01048486823811));
#183866=CARTESIAN_POINT('Ctrl Pts',(17.1883296402444,20.6576069246604,4.00872528437738));
#183867=CARTESIAN_POINT('Ctrl Pts',(17.1822523782327,20.6510860287288,4.00819617505904));
#183868=CARTESIAN_POINT('Ctrl Pts',(17.1718088669142,20.6397372861871,4.00727763160153));
#183869=CARTESIAN_POINT('Ctrl Pts',(17.1674233367316,20.6349272895329,4.0068890254886));
#183870=CARTESIAN_POINT('Ctrl Pts',(17.1590478571406,20.6256556376418,4.00614126433629));
#183871=CARTESIAN_POINT('Ctrl Pts',(17.1550545045477,20.6211971304241,4.00578225841507));
#183872=CARTESIAN_POINT('Ctrl Pts',(17.144673732083,20.6095078110725,4.00484247169327));
#183873=CARTESIAN_POINT('Ctrl Pts',(17.1383167941504,20.6022502238171,4.00426042502176));
#183874=CARTESIAN_POINT('Ctrl Pts',(17.1165780819839,20.5770865861418,4.00224710074462));
#183875=CARTESIAN_POINT('Ctrl Pts',(17.1014467602915,20.5589673847883,4.00080558837357));
#183876=CARTESIAN_POINT('Ctrl Pts',(16.9829322115398,20.4121274881097,3.98918378689565));
#183877=CARTESIAN_POINT('Ctrl Pts',(16.8946452062152,20.2719900612155,3.9783899723475));
#183878=CARTESIAN_POINT('Ctrl Pts',(16.7945495531224,20.0623225585219,3.96303632113798));
#183879=CARTESIAN_POINT('Ctrl Pts',(16.7684811856473,20.0002690983787,3.95859027556942));
#183880=CARTESIAN_POINT('Ctrl Pts',(16.7454192928009,19.9371100267559,3.95421654644109));
#183881=CARTESIAN_POINT('',(16.6170007560323,19.2092108548856,4.48828854928401));
#183882=CARTESIAN_POINT('Ctrl Pts',(16.7454193623262,19.9371102171632,3.73234496441554));
#183883=CARTESIAN_POINT('Ctrl Pts',(16.7511301821152,19.9527503023585,3.73327488216032));
#183884=CARTESIAN_POINT('Ctrl Pts',(16.7570271402811,19.9683274681955,3.73420935652883));
#183885=CARTESIAN_POINT('Ctrl Pts',(16.7847361246994,20.0389908547596,3.73849007279982));
#183886=CARTESIAN_POINT('Ctrl Pts',(16.8086666919897,20.09320702465,3.74189144616012));
#183887=CARTESIAN_POINT('Ctrl Pts',(16.8402460982925,20.1573271180286,3.74609042516054));
#183888=CARTESIAN_POINT('Ctrl Pts',(16.8457497773428,20.1682616892724,3.74681280859572));
#183889=CARTESIAN_POINT('Ctrl Pts',(16.8549744682823,20.1861999470631,3.74800862032513));
#183890=CARTESIAN_POINT('Ctrl Pts',(16.8586405989902,20.1932316427534,3.74848011759585));
#183891=CARTESIAN_POINT('Ctrl Pts',(16.8653238737509,20.2058764463867,3.74933303018163));
#183892=CARTESIAN_POINT('Ctrl Pts',(16.868327032131,20.2114968685499,3.74971394621964));
#183893=CARTESIAN_POINT('Ctrl Pts',(16.8748001947079,20.2234809233867,3.7505300649941));
#183894=CARTESIAN_POINT('Ctrl Pts',(16.8782775889256,20.2298404522894,3.75096552794722));
#183895=CARTESIAN_POINT('Ctrl Pts',(16.8877881929084,20.2470234112969,3.75214863950455));
#183896=CARTESIAN_POINT('Ctrl Pts',(16.8938838139386,20.2578118058947,3.75289851996892));
#183897=CARTESIAN_POINT('Ctrl Pts',(16.9256758973077,20.3129435392721,3.75676757530466));
#183898=CARTESIAN_POINT('Ctrl Pts',(16.9528799516673,20.3563935066497,3.75994114839642));
#183899=CARTESIAN_POINT('Ctrl Pts',(17.0774339827088,20.5401470878826,3.77392296576256));
#183900=CARTESIAN_POINT('Ctrl Pts',(17.1899739660393,20.6693586488334,3.78529469876379));
#183901=CARTESIAN_POINT('Ctrl Pts',(17.3851491458625,20.8452464628246,3.80257303113745));
#183902=CARTESIAN_POINT('Ctrl Pts',(17.4574748771101,20.9023449443682,3.80854929797737));
#183903=CARTESIAN_POINT('Ctrl Pts',(17.5412586065262,20.9600427229839,3.81483427810208));
#183904=CARTESIAN_POINT('Ctrl Pts',(17.5492591626678,20.9654718963341,3.8154283180293));
#183905=CARTESIAN_POINT('Ctrl Pts',(17.5611326750265,20.973410999223,3.81630059436935));
#183906=CARTESIAN_POINT('Ctrl Pts',(17.5649769621597,20.9759632942649,3.81658157941001));
#183907=CARTESIAN_POINT('Ctrl Pts',(17.5718145081591,20.9804707299225,3.81707876634139));
#183908=CARTESIAN_POINT('Ctrl Pts',(17.5748044019134,20.9824308757475,3.81729530137233));
#183909=CARTESIAN_POINT('Ctrl Pts',(17.5812240084211,20.9866162950421,3.81775834667016));
#183910=CARTESIAN_POINT('Ctrl Pts',(17.5846551961659,20.9888392043517,3.81800469954061));
#183911=CARTESIAN_POINT('Ctrl Pts',(17.5940984741114,20.9949183069583,3.81867965074302));
#183912=CARTESIAN_POINT('Ctrl Pts',(17.600123737696,20.9987540769686,3.81910691013807));
#183913=CARTESIAN_POINT('Ctrl Pts',(17.6325052762639,21.0191390688196,3.82138566464375));
#183914=CARTESIAN_POINT('Ctrl Pts',(17.6592061385684,21.0351370302697,3.82320298173722));
#183915=CARTESIAN_POINT('Ctrl Pts',(17.8286691088471,21.1316581314889,3.83441819100461));
#183916=CARTESIAN_POINT('Ctrl Pts',(17.9800399028227,21.1959705874623,3.84307890089296));
#183917=CARTESIAN_POINT('Ctrl Pts',(18.2497877737525,21.2752106474579,3.85846828558921));
#183918=CARTESIAN_POINT('Ctrl Pts',(18.364779672467,21.2988453318533,3.86501034735576));
#183919=CARTESIAN_POINT('Ctrl Pts',(18.4953201014908,21.314550628943,3.87271294160433));
#183920=CARTESIAN_POINT('Ctrl Pts',(18.5095292597716,21.3161142995894,3.87355473649914));
#183921=CARTESIAN_POINT('Ctrl Pts',(18.532167243713,21.318373731634,3.8749016897327));
#183922=CARTESIAN_POINT('Ctrl Pts',(18.540586438649,21.3191631097741,3.87540390428919));
#183923=CARTESIAN_POINT('Ctrl Pts',(18.555442409567,21.3204662549038,3.87629241448077));
#183924=CARTESIAN_POINT('Ctrl Pts',(18.5618772661775,21.3210010561028,3.87667804361802));
#183925=CARTESIAN_POINT('Ctrl Pts',(18.575190856235,21.3220462412589,3.87747753837022));
#183926=CARTESIAN_POINT('Ctrl Pts',(18.5820698311541,21.3225524617967,3.87789153010235));
#183927=CARTESIAN_POINT('Ctrl Pts',(18.599731997879,21.3237654578034,3.87895684845167));
#183928=CARTESIAN_POINT('Ctrl Pts',(18.6105182519822,21.3244232957944,3.87960970350795));
#183929=CARTESIAN_POINT('Ctrl Pts',(18.6555452821222,21.326823555215,3.88234478651855));
#183930=CARTESIAN_POINT('Ctrl Pts',(18.6898192381527,21.3278165494257,3.88445032496534));
#183931=CARTESIAN_POINT('Ctrl Pts',(18.7791605186645,21.3282343230201,3.89000354071703));
#183932=CARTESIAN_POINT('Ctrl Pts',(18.8342053197233,21.3263436425017,3.89348958172809));
#183933=CARTESIAN_POINT('Ctrl Pts',(18.9981747699146,21.3142973973527,3.90405711093055));
#183934=CARTESIAN_POINT('Ctrl Pts',(19.1064469642927,21.297846434864,3.91128699662245));
#183935=CARTESIAN_POINT('Ctrl Pts',(19.2565082286312,21.2629925501149,3.92146357903006));
#183936=CARTESIAN_POINT('Ctrl Pts',(19.299731676814,21.251498988194,3.92441190518347));
#183937=CARTESIAN_POINT('Ctrl Pts',(19.3667225416407,21.2313929390796,3.92898244881481));
#183938=CARTESIAN_POINT('Ctrl Pts',(19.3907546696953,21.2237093227024,3.93062221528891));
#183939=CARTESIAN_POINT('Ctrl Pts',(19.4618699183207,21.1995627370261,3.9354647701689));
#183940=CARTESIAN_POINT('Ctrl Pts',(19.5085183824853,21.1818623794304,3.93862853329498));
#183941=CARTESIAN_POINT('Ctrl Pts',(19.5617057662208,21.1595002531938,3.94218669749329));
#183942=CARTESIAN_POINT('Ctrl Pts',(19.5688931004567,21.1564314655755,3.94266645739698));
#183943=CARTESIAN_POINT('Ctrl Pts',(19.5803426983136,21.1514676733282,3.94342883303313));
#183944=CARTESIAN_POINT('Ctrl Pts',(19.5846158989509,21.14959829455,3.94371294225333));
#183945=CARTESIAN_POINT('Ctrl Pts',(19.5921676628061,21.1462648795954,3.94421423489702));
#183946=CARTESIAN_POINT('Ctrl Pts',(19.5954487225084,21.1448066063882,3.94443176603009));
#183947=CARTESIAN_POINT('Ctrl Pts',(19.6023890420888,21.141700799033,3.94489131938518));
#183948=CARTESIAN_POINT('Ctrl Pts',(19.6060473249025,21.1400512091579,3.94513321315618));
#183949=CARTESIAN_POINT('Ctrl Pts',(19.6158941963951,21.1355773304388,3.94578345193418));
#183950=CARTESIAN_POINT('Ctrl Pts',(19.6220739601781,21.1327335711796,3.94619061688297));
#183951=CARTESIAN_POINT('Ctrl Pts',(19.6524951793011,21.1185564708656,3.94819096060612));
#183952=CARTESIAN_POINT('Ctrl Pts',(19.6765351380951,21.1067934350036,3.94975909388299));
#183953=CARTESIAN_POINT('Ctrl Pts',(19.745164350161,21.0715840345379,3.95421742031739));
#183954=CARTESIAN_POINT('Ctrl Pts',(19.7891500424924,21.0469971016158,3.957052200249));
#183955=CARTESIAN_POINT('Ctrl Pts',(19.9451763115874,20.9523208244569,3.96717294494502));
#183956=CARTESIAN_POINT('Ctrl Pts',(20.051470904392,20.8733534911066,3.97421147531152));
#183957=CARTESIAN_POINT('Ctrl Pts',(20.2269856781593,20.7154880447386,3.98719791917516));
#183958=CARTESIAN_POINT('Ctrl Pts',(20.2990255553218,20.6403989932548,3.993036777261));
#183959=CARTESIAN_POINT('Ctrl Pts',(20.3742161634738,20.5494982460048,3.99994988372352));
#183960=CARTESIAN_POINT('Ctrl Pts',(20.3830679244672,20.538577336266,4.00077790081263));
#183961=CARTESIAN_POINT('Ctrl Pts',(20.3970261306588,20.521001310588,4.0021069158685));
#183962=CARTESIAN_POINT('Ctrl Pts',(20.4022030170933,20.5144024841423,4.00260509286901));
#183963=CARTESIAN_POINT('Ctrl Pts',(20.4112889757448,20.5026780721383,4.0034889114461));
#183964=CARTESIAN_POINT('Ctrl Pts',(20.4152141281474,20.4975650407565,4.00387390911743));
#183965=CARTESIAN_POINT('Ctrl Pts',(20.4233084062267,20.4869208765084,4.00467452443063));
#183966=CARTESIAN_POINT('Ctrl Pts',(20.4274738556524,20.481387056336,4.00509028019656));
#183967=CARTESIAN_POINT('Ctrl Pts',(20.4381465718692,20.4670625310526,4.006165309773));
#183968=CARTESIAN_POINT('Ctrl Pts',(20.4446129458923,20.4582417418618,4.00682616614534));
#183969=CARTESIAN_POINT('Ctrl Pts',(20.4717422470376,20.4206267756346,4.00963984808525));
#183970=CARTESIAN_POINT('Ctrl Pts',(20.4917477587546,20.391367583306,4.01181769228642));
#183971=CARTESIAN_POINT('Ctrl Pts',(20.5423374306959,20.3132373819067,4.01760876797445));
#183972=CARTESIAN_POINT('Ctrl Pts',(20.5716747307795,20.263597815947,4.02126458655133));
#183973=CARTESIAN_POINT('Ctrl Pts',(20.6748472495638,20.0715371932385,4.03530635020058));
#183974=CARTESIAN_POINT('Ctrl Pts',(20.734436356534,19.9220972779059,4.04607404844624));
#183975=CARTESIAN_POINT('Ctrl Pts',(20.7803420205634,19.7535662092129,4.05743444086405));
#183976=CARTESIAN_POINT('Ctrl Pts',(20.7839626653809,19.7397218938321,4.05836171553017));
#183977=CARTESIAN_POINT('Ctrl Pts',(20.7900540294908,19.7154265284647,4.05997749123066));
#183978=CARTESIAN_POINT('Ctrl Pts',(20.7925860980395,19.7049914764026,4.06066779031244));
#183979=CARTESIAN_POINT('Ctrl Pts',(20.804329950576,19.6549342693205,4.0639601981538));
#183980=CARTESIAN_POINT('Ctrl Pts',(20.8124785173306,19.6150684232819,4.06652563870022));
#183981=CARTESIAN_POINT('Ctrl Pts',(20.8207403122214,19.5677325877238,4.0694861224246));
#183982=CARTESIAN_POINT('Ctrl Pts',(20.8219690674966,19.56046880634,4.06993804565851));
#183983=CARTESIAN_POINT('Ctrl Pts',(20.82390032049,19.5486782967923,4.07066760133132));
#183984=CARTESIAN_POINT('Ctrl Pts',(20.8246260750177,19.5441555148515,4.07094650206992));
#183985=CARTESIAN_POINT('Ctrl Pts',(20.8258916127203,19.5361018889429,4.07144139573215));
#183986=CARTESIAN_POINT('Ctrl Pts',(20.8264371442872,19.5325720065961,4.07165771024461));
#183987=CARTESIAN_POINT('Ctrl Pts',(20.8275912306148,19.5249771530222,4.07212184025405));
#183988=CARTESIAN_POINT('Ctrl Pts',(20.8281968799802,19.5209117972402,4.07236949017658));
#183989=CARTESIAN_POINT('Ctrl Pts',(20.8298369351921,19.5096787341877,4.07305166327479));
#183990=CARTESIAN_POINT('Ctrl Pts',(20.8308464188975,19.5025073655581,4.07348479944763));
#183991=CARTESIAN_POINT('Ctrl Pts',(20.8361896723677,19.463084349893,4.07585353081452));
#183992=CARTESIAN_POINT('Ctrl Pts',(20.8398164250681,19.4307393548967,4.07775167274199));
#183993=CARTESIAN_POINT('Ctrl Pts',(20.8570905572145,19.2362829465584,4.08896056158089));
#183994=CARTESIAN_POINT('Ctrl Pts',(20.8527615479326,19.0731084315824,4.09755904451648));
#183995=CARTESIAN_POINT('Ctrl Pts',(20.8132821694725,18.796361307802,4.11286292887981));
#183996=CARTESIAN_POINT('Ctrl Pts',(20.7872378520925,18.6822763982243,4.1193853311666));
#183997=CARTESIAN_POINT('Ctrl Pts',(20.7475991240023,18.5573091158752,4.12706579577597));
#183998=CARTESIAN_POINT('Ctrl Pts',(20.7431408526149,18.5437322699136,4.12790730965704));
#183999=CARTESIAN_POINT('Ctrl Pts',(20.735826624203,18.5221962186447,4.12925389722875));
#184000=CARTESIAN_POINT('Ctrl Pts',(20.733059793352,18.5142070450861,4.12975602966671));
#184001=CARTESIAN_POINT('Ctrl Pts',(20.7280956811924,18.5001462140787,4.13064444419981));
#184002=CARTESIAN_POINT('Ctrl Pts',(20.7259183273438,18.494067599787,4.13103006025751));
#184003=CARTESIAN_POINT('Ctrl Pts',(20.7213573450474,18.4815156836372,4.1318295766242));
#184004=CARTESIAN_POINT('Ctrl Pts',(20.718969819617,18.4750438884075,4.13224360329056));
#184005=CARTESIAN_POINT('Ctrl Pts',(20.712760130278,18.4584615099707,4.13330911417358));
#184006=CARTESIAN_POINT('Ctrl Pts',(20.708892120634,18.4483684131737,4.13396212789599));
#184007=CARTESIAN_POINT('Ctrl Pts',(20.6924249575182,18.4063648691136,4.13669874835442));
#184008=CARTESIAN_POINT('Ctrl Pts',(20.6791289124934,18.3747349071465,4.13880569837287));
#184009=CARTESIAN_POINT('Ctrl Pts',(20.6424863319229,18.2931731811083,4.14436352470528));
#184010=CARTESIAN_POINT('Ctrl Pts',(20.6179492061051,18.2438078183229,4.14785284419523));
#184011=CARTESIAN_POINT('Ctrl Pts',(20.539036006608,18.099468472681,4.15842667129756));
#184012=CARTESIAN_POINT('Ctrl Pts',(20.4791978374525,18.0076968944616,4.16565955547208));
#184013=CARTESIAN_POINT('Ctrl Pts',(20.3829258539305,17.8824313188052,4.17609570544941));
#184014=CARTESIAN_POINT('Ctrl Pts',(20.3519898988495,17.8449252803927,4.17929988068426));
#184015=CARTESIAN_POINT('Ctrl Pts',(20.3082127701791,17.7954264309714,4.18361043941861));
#184016=CARTESIAN_POINT('Ctrl Pts',(20.2964739656836,17.7824799597491,4.18474583892938));
#184017=CARTESIAN_POINT('Ctrl Pts',(20.248242296192,17.7305921952975,4.18932440718615));
#184018=CARTESIAN_POINT('Ctrl Pts',(20.2104400998258,17.6928884530024,4.19271695928357));
#184019=CARTESIAN_POINT('Ctrl Pts',(20.1648465366104,17.650729750702,4.19654762693061));
#184020=CARTESIAN_POINT('Ctrl Pts',(20.1584064595039,17.6448482492715,4.19708291812731));
#184021=CARTESIAN_POINT('Ctrl Pts',(20.1486008733891,17.6360036602078,4.19788897655025));
#184022=CARTESIAN_POINT('Ctrl Pts',(20.1452620866617,17.6330112722332,4.19816188140133));
#184023=CARTESIAN_POINT('Ctrl Pts',(20.1392522501189,17.6276592864699,4.19865028426725));
#184024=CARTESIAN_POINT('Ctrl Pts',(20.1365847376583,17.6252958170394,4.19886607051818));
#184025=CARTESIAN_POINT('Ctrl Pts',(20.130775933192,17.620175226162,4.19933380738383));
#184026=CARTESIAN_POINT('Ctrl Pts',(20.1276324510737,17.617420676399,4.19958556707161));
#184027=CARTESIAN_POINT('Ctrl Pts',(20.1187807147261,17.6097103588029,4.200290755988));
#184028=CARTESIAN_POINT('Ctrl Pts',(20.1130539785424,17.6047757718627,4.20074263999201));
#184029=CARTESIAN_POINT('Ctrl Pts',(20.078681222448,17.575476963071,4.20342992675701));
#184030=CARTESIAN_POINT('Ctrl Pts',(20.0494146553293,17.5518472427578,4.20561499482981));
#184031=CARTESIAN_POINT('Ctrl Pts',(19.9510800007609,17.4766908967316,4.21268292987606));
#184032=CARTESIAN_POINT('Ctrl Pts',(19.8794923075859,17.4285967028176,4.21740284219613));
#184033=CARTESIAN_POINT('Ctrl Pts',(19.652760223261,17.2955914476036,4.23170833242908));
#184034=CARTESIAN_POINT('Ctrl Pts',(19.4897789349949,17.225628037314,4.24120189414262));
#184035=CARTESIAN_POINT('Ctrl Pts',(19.2979991984338,17.1703828406183,4.25280013293854));
#184036=CARTESIAN_POINT('Ctrl Pts',(19.275891651757,17.1644011471386,4.25414192076161));
#184037=CARTESIAN_POINT('Ctrl Pts',(19.2444522316823,17.1564396168952,4.25605858487251));
#184038=CARTESIAN_POINT('Ctrl Pts',(19.2351968555555,17.1541622436083,4.25662385775803));
#184039=CARTESIAN_POINT('Ctrl Pts',(19.2201255907791,17.1505615802483,4.25754612771147));
#184040=CARTESIAN_POINT('Ctrl Pts',(19.2143188677942,17.1492002144439,4.25790189445531));
#184041=CARTESIAN_POINT('Ctrl Pts',(19.202145593783,17.1464004493345,4.25864866184819));
#184042=CARTESIAN_POINT('Ctrl Pts',(19.1957779970397,17.1449669214759,4.25903981477013));
#184043=CARTESIAN_POINT('Ctrl Pts',(19.1806020097951,17.1416240366475,4.25997337020758));
#184044=CARTESIAN_POINT('Ctrl Pts',(19.1717879087025,17.1397414512135,4.26051662463915));
#184045=CARTESIAN_POINT('Ctrl Pts',(19.1419962260148,17.1335769640033,4.26235652089195));
#184046=CARTESIAN_POINT('Ctrl Pts',(19.1209663205808,17.1295571339028,4.2636614863055));
#184047=CARTESIAN_POINT('Ctrl Pts',(19.0707591494819,17.1207472907047,4.26679266250234));
#184048=CARTESIAN_POINT('Ctrl Pts',(19.0415360081633,17.1162483247721,4.26862772596779));
#184049=CARTESIAN_POINT('Ctrl Pts',(18.8433399762533,17.0899722470197,4.28116047324447));
#184050=CARTESIAN_POINT('Ctrl Pts',(18.6723859150249,17.0880539624159,4.29247013483993));
#184051=CARTESIAN_POINT('Ctrl Pts',(18.4039177274325,17.1175130311433,4.31026446637037));
#184052=CARTESIAN_POINT('Ctrl Pts',(18.3056290285557,17.1353928516231,4.31676737978444));
#184053=CARTESIAN_POINT('Ctrl Pts',(18.1995669030097,17.1625458891058,4.32353171879714));
#184054=CARTESIAN_POINT('Ctrl Pts',(18.1901918947276,17.1650147281953,4.32412736837289));
#184055=CARTESIAN_POINT('Ctrl Pts',(18.1763750873564,17.168754961962,4.32500154770153));
#184056=CARTESIAN_POINT('Ctrl Pts',(18.1719201139787,17.1699765946331,4.32528284306209));
#184057=CARTESIAN_POINT('Ctrl Pts',(18.1640238944989,17.1721696921031,4.32578037289907));
#184058=CARTESIAN_POINT('Ctrl Pts',(18.1605810787145,17.1731353021771,4.32599694223401));
#184059=CARTESIAN_POINT('Ctrl Pts',(18.1532101312084,17.1752227979552,4.3264598328136));
#184060=CARTESIAN_POINT('Ctrl Pts',(18.1492828063066,17.1763473288778,4.32670599785414));
#184061=CARTESIAN_POINT('Ctrl Pts',(18.1385117411464,17.1794652247564,4.32737990468372));
#184062=CARTESIAN_POINT('Ctrl Pts',(18.1316747023671,17.1814818186134,4.32780631442492));
#184063=CARTESIAN_POINT('Ctrl Pts',(18.0952340580444,17.1924304039529,4.3300724069481));
#184064=CARTESIAN_POINT('Ctrl Pts',(18.0658169643747,17.2019761572843,4.33187835986588));
#184065=CARTESIAN_POINT('Ctrl Pts',(17.9774234879568,17.2328161143402,4.33726332377545));
#184066=CARTESIAN_POINT('Ctrl Pts',(17.9191712243516,17.2560895879849,4.3407556046472));
#184067=CARTESIAN_POINT('Ctrl Pts',(17.7219704824632,17.3452263591626,4.35264921063547));
#184068=CARTESIAN_POINT('Ctrl Pts',(17.5892222465102,17.4235998150079,4.36081661934816));
#184069=CARTESIAN_POINT('Ctrl Pts',(17.4622379451329,17.5185656955367,4.36970909194733));
#184070=CARTESIAN_POINT('Ctrl Pts',(17.4583576730518,17.5214884574539,4.36998190656997));
#184071=CARTESIAN_POINT('Ctrl Pts',(17.4040559894782,17.5626841724968,4.37381531045745));
#184072=CARTESIAN_POINT('Ctrl Pts',(17.3553699636836,17.6031833921581,4.37744243492799));
#184073=CARTESIAN_POINT('Ctrl Pts',(17.2993257763103,17.6542227687575,4.38189394337219));
#184074=CARTESIAN_POINT('Ctrl Pts',(17.2901522356764,17.6627270591928,4.38263190245978));
#184075=CARTESIAN_POINT('Ctrl Pts',(17.2752274300407,17.6768110331675,4.38384822353941));
#184076=CARTESIAN_POINT('Ctrl Pts',(17.2694314413727,17.6823430302392,4.38432453714664));
#184077=CARTESIAN_POINT('Ctrl Pts',(17.2590770538952,17.6923387458035,4.38518268539031));
#184078=CARTESIAN_POINT('Ctrl Pts',(17.2545071441326,17.6967904405254,4.38556399370994));
#184079=CARTESIAN_POINT('Ctrl Pts',(17.2456932667028,17.7054543113126,4.38630444032412));
#184080=CARTESIAN_POINT('Ctrl Pts',(17.2414468806048,17.7096639490957,4.38666346498749));
#184081=CARTESIAN_POINT('Ctrl Pts',(17.2299423096576,17.7211660077224,4.38764244923022));
#184082=CARTESIAN_POINT('Ctrl Pts',(17.2227194320461,17.7284933728659,4.38826395954503));
#184083=CARTESIAN_POINT('Ctrl Pts',(17.1934249002735,17.7586482486085,4.3908132405388));
#184084=CARTESIAN_POINT('Ctrl Pts',(17.1718156648956,17.7819173645032,4.39276088741411));
#184085=CARTESIAN_POINT('Ctrl Pts',(17.1176146314886,17.8429805655847,4.39782553338901));
#184086=CARTESIAN_POINT('Ctrl Pts',(17.0858224785269,17.8814553148506,4.40097334406224));
#184087=CARTESIAN_POINT('Ctrl Pts',(17.0102401862086,17.979805947295,4.40891137003979));
#184088=CARTESIAN_POINT('Ctrl Pts',(16.9681823525145,18.0409259369875,4.4137521554419));
#184089=CARTESIAN_POINT('Ctrl Pts',(16.8493473163932,18.2346666673104,4.4287220229877));
#184090=CARTESIAN_POINT('Ctrl Pts',(16.7836721177527,18.3735217592032,4.43897492035189));
#184091=CARTESIAN_POINT('Ctrl Pts',(16.7284957692046,18.5328550914531,4.44949009444052));
#184092=CARTESIAN_POINT('Ctrl Pts',(16.7235995322683,18.5475109436552,4.45044586116425));
#184093=CARTESIAN_POINT('Ctrl Pts',(16.7171006633379,18.5676966703732,4.45174534234653));
#184094=CARTESIAN_POINT('Ctrl Pts',(16.7153596036074,18.5731810131652,4.45209670097354));
#184095=CARTESIAN_POINT('Ctrl Pts',(16.7126241714508,18.5819210329939,4.45265385356486));
#184096=CARTESIAN_POINT('Ctrl Pts',(16.7116152683634,18.5851720806839,4.45286048780106));
#184097=CARTESIAN_POINT('Ctrl Pts',(16.7095441622783,18.591903238379,4.45328703080189));
#184098=CARTESIAN_POINT('Ctrl Pts',(16.7084830888906,18.5953836567293,4.45350686751352));
#184099=CARTESIAN_POINT('Ctrl Pts',(16.7059703322528,18.603702556673,4.454030656143));
#184100=CARTESIAN_POINT('Ctrl Pts',(16.7045269724976,18.608543570224,4.45433412242644));
#184101=CARTESIAN_POINT('Ctrl Pts',(16.6996912589511,18.624977100747,4.45535988326835));
#184102=CARTESIAN_POINT('Ctrl Pts',(16.6963807210238,18.6365937138202,4.45607756803336));
#184103=CARTESIAN_POINT('Ctrl Pts',(16.6886498122196,18.6646295124094,4.45779325749149));
#184104=CARTESIAN_POINT('Ctrl Pts',(16.684327409838,18.6810750893408,4.45878621427896));
#184105=CARTESIAN_POINT('Ctrl Pts',(16.6687721137264,18.743298771819,4.46249873032591));
#184106=CARTESIAN_POINT('Ctrl Pts',(16.658870342443,18.7893981275048,4.46515906548827));
#184107=CARTESIAN_POINT('Ctrl Pts',(16.6283221861243,18.9590285268923,4.47474467553596));
#184108=CARTESIAN_POINT('Ctrl Pts',(16.6171065839527,19.0839903651149,4.48142927455064));
#184109=CARTESIAN_POINT('Ctrl Pts',(16.6170007560323,19.2092108548856,4.48828854928401));
#184110=CARTESIAN_POINT('Ctrl Pts',(16.6170007544018,19.2092127851992,4.48828865502192));
#184111=CARTESIAN_POINT('Ctrl Pts',(16.6169304738953,19.2924617484522,4.49284883231375));
#184112=CARTESIAN_POINT('Ctrl Pts',(16.6217706715984,19.3756377283516,4.49747292236368));
#184113=CARTESIAN_POINT('Ctrl Pts',(16.6354867602422,19.4922448590161,4.50419755621686));
#184114=CARTESIAN_POINT('Ctrl Pts',(16.6402991600693,19.5260763260431,4.5061771050553));
#184115=CARTESIAN_POINT('Ctrl Pts',(16.6476158018074,19.5698801127746,4.50878346735209));
#184116=CARTESIAN_POINT('Ctrl Pts',(16.6493769518854,19.5799724916309,4.50938697016501));
#184117=CARTESIAN_POINT('Ctrl Pts',(16.6524781189089,19.5970125896926,4.5104111770559));
#184118=CARTESIAN_POINT('Ctrl Pts',(16.6537798505403,19.6039671599484,4.51083066787339));
#184119=CARTESIAN_POINT('Ctrl Pts',(16.6564245897503,19.6177153434414,4.51166293430155));
#184120=CARTESIAN_POINT('Ctrl Pts',(16.657766117681,19.6245091534948,4.51207565819799));
#184121=CARTESIAN_POINT('Ctrl Pts',(16.6604207799739,19.6376143163115,4.51287464958691));
#184122=CARTESIAN_POINT('Ctrl Pts',(16.6617294578774,19.6439265011883,4.51326077048213));
#184123=CARTESIAN_POINT('Ctrl Pts',(16.6648077495934,19.658440307149,4.51415158556389));
#184124=CARTESIAN_POINT('Ctrl Pts',(16.6665973239782,19.6666375419306,4.51465691482729));
#184125=CARTESIAN_POINT('Ctrl Pts',(16.6715178769922,19.6885504292253,4.51601377451863));
#184126=CARTESIAN_POINT('Ctrl Pts',(16.6747368856452,19.702245693152,4.51686811845724));
#184127=CARTESIAN_POINT('Ctrl Pts',(16.6964948357784,19.7908407974831,4.52243687467858));
#184128=CARTESIAN_POINT('Ctrl Pts',(16.7189735904053,19.8646838242807,4.52727680304563));
#184129=CARTESIAN_POINT('Ctrl Pts',(16.7454193895773,19.9371102917951,4.53222340700496));
#184130=CARTESIAN_POINT('Origin',(18.734,19.211,0.));
#184131=CARTESIAN_POINT('',(16.7454193397875,19.9371101554369,5.55626850699162));
#184132=CARTESIAN_POINT('',(16.7454193775548,19.9371102588694,5.33540091894091));
#184133=CARTESIAN_POINT('',(16.7454193623258,19.9371102171621,0.));
#184134=CARTESIAN_POINT('Ctrl Pts',(16.7454193397875,19.9371101554369,5.55626850699162));
#184135=CARTESIAN_POINT('Ctrl Pts',(16.7359008819459,19.9110421807129,5.55474534815383));
#184136=CARTESIAN_POINT('Ctrl Pts',(16.7268931592987,19.8847819920176,5.55321402040514));
#184137=CARTESIAN_POINT('Ctrl Pts',(16.6925866569971,19.7779638736276,5.54697988012083));
#184138=CARTESIAN_POINT('Ctrl Pts',(16.6716050363402,19.6961196255081,5.54218747023461));
#184139=CARTESIAN_POINT('Ctrl Pts',(16.6528673383292,19.5993009577569,5.53639852339288));
#184140=CARTESIAN_POINT('Ctrl Pts',(16.6503087151907,19.5853279366274,5.5355603115109));
#184141=CARTESIAN_POINT('Ctrl Pts',(16.6465902595183,19.5638001875872,5.53426429491335));
#184142=CARTESIAN_POINT('Ctrl Pts',(16.6453303607485,19.5562629906949,5.53380967379834));
#184143=CARTESIAN_POINT('Ctrl Pts',(16.643106864124,19.5425034523681,5.53297809749433));
#184144=CARTESIAN_POINT('Ctrl Pts',(16.6421301614704,19.5362832948531,5.53260156320738));
#184145=CARTESIAN_POINT('Ctrl Pts',(16.6400580227851,19.5226914144666,5.53177741361028));
#184146=CARTESIAN_POINT('Ctrl Pts',(16.6389737391049,19.5153180995955,5.5313294499617));
#184147=CARTESIAN_POINT('Ctrl Pts',(16.6361094454234,19.4950992708156,5.53009858026596));
#184148=CARTESIAN_POINT('Ctrl Pts',(16.6344085220797,19.4822430437229,5.52931318575209));
#184149=CARTESIAN_POINT('Ctrl Pts',(16.6263685191507,19.416858900476,5.52530434253773));
#184150=CARTESIAN_POINT('Ctrl Pts',(16.6218825839194,19.3641260429436,5.52202306422395));
#184151=CARTESIAN_POINT('Ctrl Pts',(16.6177663610251,19.2773299077746,5.51653980109578));
#184152=CARTESIAN_POINT('Ctrl Pts',(16.6169742107429,19.2433434160845,5.51437224371054));
#184153=CARTESIAN_POINT('Ctrl Pts',(16.6171022078051,19.0787312575047,5.5037810304143));
#184154=CARTESIAN_POINT('Ctrl Pts',(16.6292932816139,18.9484055300888,5.49508949079167));
#184155=CARTESIAN_POINT('Ctrl Pts',(16.6709615176535,18.7266531037098,5.48023958195372));
#184156=CARTESIAN_POINT('Ctrl Pts',(16.6947819154142,18.6345335505787,5.4740597931356));
#184157=CARTESIAN_POINT('Ctrl Pts',(16.7277657519504,18.5351250513358,5.46758872593254));
#184158=CARTESIAN_POINT('Ctrl Pts',(16.7308789341621,18.5259534263594,5.46699363907557));
#184159=CARTESIAN_POINT('Ctrl Pts',(16.7355692047248,18.5124409982922,5.46612012492284));
#184160=CARTESIAN_POINT('Ctrl Pts',(16.7370976766334,18.5080836221592,5.46583893796131));
#184161=CARTESIAN_POINT('Ctrl Pts',(16.7398349366883,18.5003612139772,5.46534152791239));
#184162=CARTESIAN_POINT('Ctrl Pts',(16.7410380036105,18.496994211817,5.46512497056685));
#184163=CARTESIAN_POINT('Ctrl Pts',(16.743634281157,18.4897857444874,5.46466202601852));
#184164=CARTESIAN_POINT('Ctrl Pts',(16.745030081249,18.4859452709947,5.4644157954359));
#184165=CARTESIAN_POINT('Ctrl Pts',(16.7488929555607,18.4754118658669,5.46374152435155));
#184166=CARTESIAN_POINT('Ctrl Pts',(16.7513827768849,18.4687272530499,5.46331481829826));
#184167=CARTESIAN_POINT('Ctrl Pts',(16.7648702447291,18.4330684826696,5.46104432040453));
#184168=CARTESIAN_POINT('Ctrl Pts',(16.7764699587073,18.4043242258291,5.4592344139886));
#184169=CARTESIAN_POINT('Ctrl Pts',(16.8532264251643,18.2255379293045,5.44804382704229));
#184170=CARTESIAN_POINT('Ctrl Pts',(16.9349648113669,18.0832014923817,5.43939868918828));
#184171=CARTESIAN_POINT('Ctrl Pts',(17.1022876622664,17.8570979621112,5.42400417904076));
#184172=CARTESIAN_POINT('Ctrl Pts',(17.1800410611092,17.7685222165816,5.41743776600403));
#184173=CARTESIAN_POINT('Ctrl Pts',(17.2750386711216,17.676944803217,5.40970776342814));
#184174=CARTESIAN_POINT('Ctrl Pts',(17.2854344384217,17.6671245824852,5.40886563654019));
#184175=CARTESIAN_POINT('Ctrl Pts',(17.3021355840829,17.6516652608393,5.40751825127224));
#184176=CARTESIAN_POINT('Ctrl Pts',(17.3083767584939,17.6459572196154,5.40701593966362));
#184177=CARTESIAN_POINT('Ctrl Pts',(17.3194429388047,17.6359574552326,5.40612731634685));
#184178=CARTESIAN_POINT('Ctrl Pts',(17.3242537172059,17.6316500976897,5.40574167168038));
#184179=CARTESIAN_POINT('Ctrl Pts',(17.3342433775135,17.6227878084346,5.40494220223222));
#184180=CARTESIAN_POINT('Ctrl Pts',(17.3394249568205,17.618236045479,5.4045282516168));
#184181=CARTESIAN_POINT('Ctrl Pts',(17.3527797545426,17.6066196387535,5.40346316012071));
#184182=CARTESIAN_POINT('Ctrl Pts',(17.360984901458,17.5995921551588,5.40281049205809));
#184183=CARTESIAN_POINT('Ctrl Pts',(17.3954326846533,17.5705426922308,5.40007722057417));
#184184=CARTESIAN_POINT('Ctrl Pts',(17.4221529449053,17.5490975585353,5.39797334526817));
#184185=CARTESIAN_POINT('Ctrl Pts',(17.4930984235393,17.4949354732572,5.39242556030738));
#184186=CARTESIAN_POINT('Ctrl Pts',(17.5380970833765,17.4632787465323,5.38894338043964));
#184187=CARTESIAN_POINT('Ctrl Pts',(17.6611867536919,17.3836656152582,5.37952161406575));
#184188=CARTESIAN_POINT('Ctrl Pts',(17.7412415266193,17.3389669900743,5.37349485821874));
#184189=CARTESIAN_POINT('Ctrl Pts',(17.8723924390506,17.2765227868073,5.3638970371317));
#184190=CARTESIAN_POINT('Ctrl Pts',(17.9217125462298,17.2553009085088,5.36034697587555));
#184191=CARTESIAN_POINT('Ctrl Pts',(18.0061653416335,17.2227083585985,5.35441143042529));
#184192=CARTESIAN_POINT('Ctrl Pts',(18.0408861766309,17.2103400145177,5.3520108089968));
#184193=CARTESIAN_POINT('Ctrl Pts',(18.1208934790478,17.1841726711909,5.3465929024244));
#184194=CARTESIAN_POINT('Ctrl Pts',(18.1663581214309,17.1709725303705,5.34359556922666));
#184195=CARTESIAN_POINT('Ctrl Pts',(18.2196966717736,17.1574079193658,5.3402022895878));
#184196=CARTESIAN_POINT('Ctrl Pts',(18.2271731666627,17.1555499489859,5.33972943805029));
#184197=CARTESIAN_POINT('Ctrl Pts',(18.2391606598026,17.1526403426762,5.3389759282303));
#184198=CARTESIAN_POINT('Ctrl Pts',(18.2436651757001,17.1515626466134,5.33869382940661));
#184199=CARTESIAN_POINT('Ctrl Pts',(18.2516636875317,17.1496767497097,5.33819481569946));
#184200=CARTESIAN_POINT('Ctrl Pts',(18.2551562421806,17.1488626338585,5.33797756398594));
#184201=CARTESIAN_POINT('Ctrl Pts',(18.2625792611126,17.1471522008338,5.33751719855208));
#184202=CARTESIAN_POINT('Ctrl Pts',(18.2665102129466,17.1462582362916,5.33727422045448));
#184203=CARTESIAN_POINT('Ctrl Pts',(18.2771616051412,17.1438679085203,5.33661798594348));
#184204=CARTESIAN_POINT('Ctrl Pts',(18.2838868981239,17.1423930771809,5.33620594734778));
#184205=CARTESIAN_POINT('Ctrl Pts',(18.3177569515697,17.1351385020437,5.33414188419455));
#184206=CARTESIAN_POINT('Ctrl Pts',(18.3450076937946,17.129859834848,5.33251686239939));
#184207=CARTESIAN_POINT('Ctrl Pts',(18.4247510118996,17.1160341667165,5.32784450601));
#184208=CARTESIAN_POINT('Ctrl Pts',(18.477473609844,17.1089267939202,5.32485915066349));
#184209=CARTESIAN_POINT('Ctrl Pts',(18.6705416687809,17.0902732665784,5.31412753962805));
#184210=CARTESIAN_POINT('Ctrl Pts',(18.8116741229498,17.0907458170548,5.30664362646507));
#184211=CARTESIAN_POINT('Ctrl Pts',(19.0430902736284,17.1146721973172,5.29377453902092));
#184212=CARTESIAN_POINT('Ctrl Pts',(19.1337400752133,17.1300550382693,5.28858369472446));
#184213=CARTESIAN_POINT('Ctrl Pts',(19.2364890397762,17.1544535750968,5.28239262262585));
#184214=CARTESIAN_POINT('Ctrl Pts',(19.2498485700953,17.1577638537509,5.28158169977626));
#184215=CARTESIAN_POINT('Ctrl Pts',(19.2712122263524,17.1632790883111,5.28027496940906));
#184216=CARTESIAN_POINT('Ctrl Pts',(19.2792374479609,17.1654013026363,5.27978183387979));
#184217=CARTESIAN_POINT('Ctrl Pts',(19.2934589822938,17.1692517231672,5.27890383791887));
#184218=CARTESIAN_POINT('Ctrl Pts',(19.2996603222617,17.170961084384,5.27851959330443));
#184219=CARTESIAN_POINT('Ctrl Pts',(19.3125593944736,17.1745799715187,5.27771740349429));
#184220=CARTESIAN_POINT('Ctrl Pts',(19.3192556780933,17.1764943365059,5.27729930459204));
#184221=CARTESIAN_POINT('Ctrl Pts',(19.3366095470959,17.1815483069829,5.27621140438957));
#184222=CARTESIAN_POINT('Ctrl Pts',(19.34725197777,17.1847388014052,5.27553994776903));
#184223=CARTESIAN_POINT('Ctrl Pts',(19.3932530764568,17.1989250721566,5.27261866105073));
#184224=CARTESIAN_POINT('Ctrl Pts',(19.4283432210575,17.2107631755554,5.27034136810716));
#184225=CARTESIAN_POINT('Ctrl Pts',(19.5206296251234,17.2446181777198,5.2642173802715));
#184226=CARTESIAN_POINT('Ctrl Pts',(19.5772079639402,17.2682074572175,5.26032175831082));
#184227=CARTESIAN_POINT('Ctrl Pts',(19.7734704884578,17.3602246620092,5.24632255646222));
#184228=CARTESIAN_POINT('Ctrl Pts',(19.9065461192933,17.44153738527,5.23588749519248));
#184229=CARTESIAN_POINT('Ctrl Pts',(20.0418286309993,17.5462129905147,5.22476655187935));
#184230=CARTESIAN_POINT('Ctrl Pts',(20.0540398050925,17.555878721562,5.22375813015649));
#184231=CARTESIAN_POINT('Ctrl Pts',(20.1040093573971,17.5963368391654,5.2196158061706));
#184232=CARTESIAN_POINT('Ctrl Pts',(20.1408090014468,17.628295981744,5.21652733455363));
#184233=CARTESIAN_POINT('Ctrl Pts',(20.1821603104028,17.6667911302913,5.21304359419192));
#184234=CARTESIAN_POINT('Ctrl Pts',(20.1878157704311,17.6721143551931,5.21256684273039));
#184235=CARTESIAN_POINT('Ctrl Pts',(20.1968103011861,17.6806743336549,5.21180832655321));
#184236=CARTESIAN_POINT('Ctrl Pts',(20.2001681626347,17.6838911164694,5.21152509151034));
#184237=CARTESIAN_POINT('Ctrl Pts',(20.2060986058116,17.6896099866588,5.21102479143903));
#184238=CARTESIAN_POINT('Ctrl Pts',(20.2086754571095,17.692107582855,5.21080738343087));
#184239=CARTESIAN_POINT('Ctrl Pts',(20.2141260787188,17.6974175086571,5.21034748453693));
#184240=CARTESIAN_POINT('Ctrl Pts',(20.2169981854529,17.7002314705533,5.21010512519293));
#184241=CARTESIAN_POINT('Ctrl Pts',(20.2247329506738,17.707852959034,5.20945231296794));
#184242=CARTESIAN_POINT('Ctrl Pts',(20.2295804107833,17.7126759379944,5.20904305629049));
#184243=CARTESIAN_POINT('Ctrl Pts',(20.2535801101645,17.7367869501948,5.20701564236178));
#184244=CARTESIAN_POINT('Ctrl Pts',(20.2723839571762,17.7564200656637,5.20542335253164));
#184245=CARTESIAN_POINT('Ctrl Pts',(20.3257400308985,17.8143216813065,5.20087469686787));
#184246=CARTESIAN_POINT('Ctrl Pts',(20.3592806196731,17.8534985172206,5.19797646676236));
#184247=CARTESIAN_POINT('Ctrl Pts',(20.4769643503128,18.0015805239215,5.18749757438835));
#184248=CARTESIAN_POINT('Ctrl Pts',(20.551865596046,18.1173879606581,5.18017851917021));
#184249=CARTESIAN_POINT('Ctrl Pts',(20.6595464272297,18.3259094538104,5.16722919663671));
#184250=CARTESIAN_POINT('Ctrl Pts',(20.6981003208294,18.4151226120665,5.16175685041838));
#184251=CARTESIAN_POINT('Ctrl Pts',(20.735019797059,18.5197677698236,5.15525269135768));
#184252=CARTESIAN_POINT('Ctrl Pts',(20.7395152893983,18.532921365544,5.15443380410601));
#184253=CARTESIAN_POINT('Ctrl Pts',(20.7465005721551,18.5540372733794,5.15311668709294));
#184254=CARTESIAN_POINT('Ctrl Pts',(20.749073447548,18.5619718226137,5.15262119826229));
#184255=CARTESIAN_POINT('Ctrl Pts',(20.7535491497079,18.5760577273326,5.15174048946542));
#184256=CARTESIAN_POINT('Ctrl Pts',(20.7554709408655,18.582202980662,5.15135589841143));
#184257=CARTESIAN_POINT('Ctrl Pts',(20.7594076994409,18.5949960198031,5.1505544686821));
#184258=CARTESIAN_POINT('Ctrl Pts',(20.7614180387775,18.6016451388369,5.15013748365921));
#184259=CARTESIAN_POINT('Ctrl Pts',(20.7665352168011,18.6188756796934,5.14905569857016));
#184260=CARTESIAN_POINT('Ctrl Pts',(20.7695921326442,18.6294715995377,5.14838927790047));
#184261=CARTESIAN_POINT('Ctrl Pts',(20.7823462704288,18.6750132566875,5.14551961944914));
#184262=CARTESIAN_POINT('Ctrl Pts',(20.7912269607446,18.7101794639691,5.14329010684029));
#184263=CARTESIAN_POINT('Ctrl Pts',(20.812285091986,18.8036152629608,5.13732691457653));
#184264=CARTESIAN_POINT('Ctrl Pts',(20.8229152133099,18.8621971024793,5.13354743312624));
#184265=CARTESIAN_POINT('Ctrl Pts',(20.8541333448985,19.0880561249946,5.1188412943987));
#184266=CARTESIAN_POINT('Ctrl Pts',(20.8571927550826,19.2571060947732,5.10749629584318));
#184267=CARTESIAN_POINT('Ctrl Pts',(20.8347681008463,19.4780966419072,5.09313747102306));
#184268=CARTESIAN_POINT('Ctrl Pts',(20.8273244339242,19.5312516138185,5.08972633527414));
#184269=CARTESIAN_POINT('Ctrl Pts',(20.8163276155818,19.5926767452832,5.08587675846167));
#184270=CARTESIAN_POINT('Ctrl Pts',(20.8147335786007,19.6012732599647,5.0853401356639));
#184271=CARTESIAN_POINT('Ctrl Pts',(20.8122407122707,19.6142675099731,5.08453247331538));
#184272=CARTESIAN_POINT('Ctrl Pts',(20.8113811010626,19.6186725457341,5.08425928366856));
#184273=CARTESIAN_POINT('Ctrl Pts',(20.8098136987481,19.626570922788,5.08377057637449));
#184274=CARTESIAN_POINT('Ctrl Pts',(20.8091110913592,19.6300652250947,5.08355476890184));
#184275=CARTESIAN_POINT('Ctrl Pts',(20.8075661032799,19.6376498030672,5.08308722108849));
#184276=CARTESIAN_POINT('Ctrl Pts',(20.8067204466444,19.641739352605,5.08283567040323));
#184277=CARTESIAN_POINT('Ctrl Pts',(20.804313361678,19.6532086409666,5.08213165751559));
#184278=CARTESIAN_POINT('Ctrl Pts',(20.8027245665967,19.6605826610642,5.08168073226511));
#184279=CARTESIAN_POINT('Ctrl Pts',(20.7930399298121,19.7043930522184,5.07901103822222));
#184280=CARTESIAN_POINT('Ctrl Pts',(20.784020500265,19.7406210625401,5.07684184011556));
#184281=CARTESIAN_POINT('Ctrl Pts',(20.7513219864162,19.8585616835739,5.06985052443763));
#184282=CARTESIAN_POINT('Ctrl Pts',(20.7236754615083,19.9390920080005,5.06518734979452));
#184283=CARTESIAN_POINT('Ctrl Pts',(20.6233171252355,20.1825726637796,5.05085142417843));
#184284=CARTESIAN_POINT('Ctrl Pts',(20.5348400520287,20.3381384974425,5.04128048578719));
#184285=CARTESIAN_POINT('Ctrl Pts',(20.4142579818219,20.4989987847616,5.02959598716277));
#184286=CARTESIAN_POINT('Ctrl Pts',(20.4003040394721,20.5170009738923,5.02826143997338));
#184287=CARTESIAN_POINT('Ctrl Pts',(20.380115569651,20.5421960738657,5.02635334254832));
#184288=CARTESIAN_POINT('Ctrl Pts',(20.374118517069,20.5495778651999,5.02578927752239));
#184289=CARTESIAN_POINT('Ctrl Pts',(20.3642825316851,20.5615196755476,5.02486843869172));
#184290=CARTESIAN_POINT('Ctrl Pts',(20.3604736802066,20.5661043847744,5.02451288748692));
#184291=CARTESIAN_POINT('Ctrl Pts',(20.3524513615638,20.5756782900225,5.02376613093483));
#184292=CARTESIAN_POINT('Ctrl Pts',(20.348234074969,20.5806641904977,5.02337477136266));
#184293=CARTESIAN_POINT('Ctrl Pts',(20.3381296438044,20.5924986960532,5.02243990381693));
#184294=CARTESIAN_POINT('Ctrl Pts',(20.3322216470223,20.5993292564688,5.02189553761541));
#184295=CARTESIAN_POINT('Ctrl Pts',(20.3120895730855,20.6223062489225,5.0200479448339));
#184296=CARTESIAN_POINT('Ctrl Pts',(20.297663446107,20.6382731352455,5.0187362997404));
#184297=CARTESIAN_POINT('Ctrl Pts',(20.1601125469119,20.7859262285885,5.00633928592033));
#184298=CARTESIAN_POINT('Ctrl Pts',(20.0209042946421,20.901574252362,4.99450240301771));
#184299=CARTESIAN_POINT('Ctrl Pts',(19.8378303968496,21.0178178875436,4.98017594521599));
#184300=CARTESIAN_POINT('Ctrl Pts',(19.8063826533925,21.0366582239625,4.97775778460905));
#184301=CARTESIAN_POINT('Ctrl Pts',(19.7023683095064,21.0953578402881,4.96992584275602));
#184302=CARTESIAN_POINT('Ctrl Pts',(19.6279423707503,21.1317841683113,4.96457611118784));
#184303=CARTESIAN_POINT('Ctrl Pts',(19.5427055900718,21.1674704304197,4.95886775619578));
#184304=CARTESIAN_POINT('Ctrl Pts',(19.5338194325512,21.1711199350602,4.95827759503581));
#184305=CARTESIAN_POINT('Ctrl Pts',(19.520639595564,21.1764282807899,4.95740990645472));
#184306=CARTESIAN_POINT('Ctrl Pts',(19.5163649976677,21.1781337503042,4.95712967112614));
#184307=CARTESIAN_POINT('Ctrl Pts',(19.5087610876667,21.1811388351297,4.95663331104373));
#184308=CARTESIAN_POINT('Ctrl Pts',(19.5054340172229,21.1824439708978,4.95641685730301));
#184309=CARTESIAN_POINT('Ctrl Pts',(19.4982866676415,21.1852268530077,4.95595343095507));
#184310=CARTESIAN_POINT('Ctrl Pts',(19.4944654111288,21.1867019351617,4.95570661865175));
#184311=CARTESIAN_POINT('Ctrl Pts',(19.4839363224899,21.1907313026665,4.95502911153138));
#184312=CARTESIAN_POINT('Ctrl Pts',(19.47721967201,21.1932626064784,4.95459977257653));
#184313=CARTESIAN_POINT('Ctrl Pts',(19.44084965937,21.2067585254885,4.95228966477745));
#184314=CARTESIAN_POINT('Ctrl Pts',(19.4109646741078,21.2170926211615,4.95044419718279));
#184315=CARTESIAN_POINT('Ctrl Pts',(19.2252080429249,21.276702126775,4.93923155596619));
#184316=CARTESIAN_POINT('Ctrl Pts',(19.0642807074669,21.3084597640241,4.93059278410862));
#184317=CARTESIAN_POINT('Ctrl Pts',(18.7845695996124,21.3306321194186,4.91523325642181));
#184318=CARTESIAN_POINT('Ctrl Pts',(18.6673012266702,21.3301846532911,4.90869780898929));
#184319=CARTESIAN_POINT('Ctrl Pts',(18.5364402168657,21.3188101026219,4.90100265986646));
#184320=CARTESIAN_POINT('Ctrl Pts',(18.5222138389384,21.3174282336909,4.90016095812207));
#184321=CARTESIAN_POINT('Ctrl Pts',(18.499595443804,21.3149997629465,4.89881412604904));
#184322=CARTESIAN_POINT('Ctrl Pts',(18.4911936668189,21.3140467374377,4.89831193866344));
#184323=CARTESIAN_POINT('Ctrl Pts',(18.4763865460383,21.3122772308876,4.89742346006548));
#184324=CARTESIAN_POINT('Ctrl Pts',(18.4699787700267,21.3114817260348,4.89703783519828));
#184325=CARTESIAN_POINT('Ctrl Pts',(18.456733506889,21.3097758030101,4.89623833312042));
#184326=CARTESIAN_POINT('Ctrl Pts',(18.4498966371316,21.3088612577951,4.89582432971281));
#184327=CARTESIAN_POINT('Ctrl Pts',(18.4323598012534,21.306428115025,4.89475894724792));
#184328=CARTESIAN_POINT('Ctrl Pts',(18.4216668702656,21.3048609801094,4.89410603939718));
#184329=CARTESIAN_POINT('Ctrl Pts',(18.3770956153134,21.2979796918113,4.89137044558317));
#184330=CARTESIAN_POINT('Ctrl Pts',(18.3433384855378,21.2919248758422,4.88926443824005));
#184331=CARTESIAN_POINT('Ctrl Pts',(18.2557851028113,21.2740155084774,4.883709691274));
#184332=CARTESIAN_POINT('Ctrl Pts',(18.2022807515769,21.260877141984,4.88022256156937));
#184333=CARTESIAN_POINT('Ctrl Pts',(18.0415873592919,21.2147030748636,4.86947592303698));
#184334=CARTESIAN_POINT('Ctrl Pts',(17.9364595577411,21.175226779261,4.86205738668534));
#184335=CARTESIAN_POINT('Ctrl Pts',(17.7302656224575,21.0785061837106,4.84701617677167));
#184336=CARTESIAN_POINT('Ctrl Pts',(17.6297568832078,21.0208937693331,4.83942126725695));
#184337=CARTESIAN_POINT('Ctrl Pts',(17.5265596872077,20.9499274160579,4.83168481026389));
#184338=CARTESIAN_POINT('Ctrl Pts',(17.51870743511,20.9444487753917,4.83109662457768));
#184339=CARTESIAN_POINT('Ctrl Pts',(17.5071411558416,20.936261574281,4.83023127375603));
#184340=CARTESIAN_POINT('Ctrl Pts',(17.5033984731903,20.9335939760471,4.82995142134476));
#184341=CARTESIAN_POINT('Ctrl Pts',(17.4968468566269,20.9288920593997,4.82946186542343));
#184342=CARTESIAN_POINT('Ctrl Pts',(17.4940342072531,20.9268630077463,4.82925180501178));
#184343=CARTESIAN_POINT('Ctrl Pts',(17.4912136884051,20.9248177219187,4.82904127098932));
#184344=CARTESIAN_POINT('Ctrl Pts',(17.4912008812233,20.9248084346327,4.8290403150159));
#184345=CARTESIAN_POINT('Ctrl Pts',(17.4911754922149,20.9247900230455,4.82903841989492));
#184346=CARTESIAN_POINT('Ctrl Pts',(17.4911629101483,20.9247808985779,4.82903748072937));
#184347=CARTESIAN_POINT('Ctrl Pts',(17.4911379655358,20.9247628084192,4.82903561878836));
#184348=CARTESIAN_POINT('Ctrl Pts',(17.49112560336,20.9247538430037,4.82903469604046));
#184349=CARTESIAN_POINT('Ctrl Pts',(17.4911010934449,20.9247360672838,4.82903286655503));
#184350=CARTESIAN_POINT('Ctrl Pts',(17.4910889460705,20.924727257251,4.82903195984466));
#184351=CARTESIAN_POINT('Ctrl Pts',(17.4910648621215,20.9247097896798,4.82903016216265));
#184352=CARTESIAN_POINT('Ctrl Pts',(17.4910529252685,20.9247011319463,4.82902927117014));
#184353=CARTESIAN_POINT('Ctrl Pts',(17.4910292563409,20.9246839646264,4.82902750447416));
#184354=CARTESIAN_POINT('Ctrl Pts',(17.4910175247202,20.9246754553757,4.8290266288045));
#184355=CARTESIAN_POINT('Ctrl Pts',(17.4909942637492,20.924658583222,4.82902489256683));
#184356=CARTESIAN_POINT('Ctrl Pts',(17.4909827335356,20.924650219699,4.8290240319343));
#184357=CARTESIAN_POINT('Ctrl Pts',(17.4909598705549,20.9246336355199,4.82902232541063));
#184358=CARTESIAN_POINT('Ctrl Pts',(17.4909485375622,20.9246254147063,4.82902147950257));
#184359=CARTESIAN_POINT('Ctrl Pts',(17.4909260627822,20.9246091114369,4.82901980196182));
#184360=CARTESIAN_POINT('Ctrl Pts',(17.4909149219083,20.9246010296493,4.82901897039723));
#184361=CARTESIAN_POINT('Ctrl Pts',(17.4908928295068,20.9245850031006,4.82901732140444));
#184362=CARTESIAN_POINT('Ctrl Pts',(17.4908818774258,20.9245770579436,4.82901650393489));
#184363=CARTESIAN_POINT('Ctrl Pts',(17.4908601572638,20.924561300794,4.82901488273295));
#184364=CARTESIAN_POINT('Ctrl Pts',(17.4908493895367,20.9245534890635,4.82901407902693));
#184365=CARTESIAN_POINT('Ctrl Pts',(17.4908280346943,20.9245379963249,4.82901248509899));
#184366=CARTESIAN_POINT('Ctrl Pts',(17.4908174475402,20.9245303152938,4.82901169487413));
#184367=CARTESIAN_POINT('Ctrl Pts',(17.49079645014,20.924515081282,4.82901012763189));
#184368=CARTESIAN_POINT('Ctrl Pts',(17.4907860398119,20.9245075282469,4.82900935060835));
#184369=CARTESIAN_POINT('Ctrl Pts',(17.4907659469026,20.9244929499015,4.82900785088297));
#184370=CARTESIAN_POINT('Ctrl Pts',(17.4907562643268,20.9244859246146,4.82900712818133));
#184371=CARTESIAN_POINT('Ctrl Pts',(17.4907369361321,20.9244719006053,4.82900568553909));
#184372=CARTESIAN_POINT('Ctrl Pts',(17.4907272900563,20.9244649015522,4.82900496556438));
#184373=CARTESIAN_POINT('Ctrl Pts',(17.4907080349746,20.9244509300953,4.82900352838439));
#184374=CARTESIAN_POINT('Ctrl Pts',(17.4906984255579,20.9244439573942,4.82900281114845));
#184375=CARTESIAN_POINT('Ctrl Pts',(17.4906792409346,20.924430036569,4.82900137923252));
#184376=CARTESIAN_POINT('Ctrl Pts',(17.4906696668138,20.9244230892337,4.82900066463357));
#184377=CARTESIAN_POINT('Ctrl Pts',(17.490650555025,20.9244092207699,4.828999238159));
#184378=CARTESIAN_POINT('Ctrl Pts',(17.4906410168137,20.9244022992481,4.82899852624281));
#184379=CARTESIAN_POINT('Ctrl Pts',(17.487336924626,20.9220046015104,4.82875191474831));
#184380=CARTESIAN_POINT('Ctrl Pts',(17.4840492417595,20.9196043054218,4.82850667846364));
#184381=CARTESIAN_POINT('Ctrl Pts',(17.4772523840218,20.9146118873096,4.82799995013629));
#184382=CARTESIAN_POINT('Ctrl Pts',(17.4737442537365,20.9120183678084,4.8277385550803));
#184383=CARTESIAN_POINT('Ctrl Pts',(17.4648413934178,20.9053939275923,4.82707549844687));
#184384=CARTESIAN_POINT('Ctrl Pts',(17.4594577891916,20.9013480428791,4.82667483237144));
#184385=CARTESIAN_POINT('Ctrl Pts',(17.4439801747168,20.889600325604,4.82552347555291));
#184386=CARTESIAN_POINT('Ctrl Pts',(17.4339358474377,20.8818331509788,4.82477696000542));
#184387=CARTESIAN_POINT('Ctrl Pts',(17.3996896973846,20.8548551492021,4.82223168832354));
#184388=CARTESIAN_POINT('Ctrl Pts',(17.37583792717,20.8352043317,4.82045889576232));
#184389=CARTESIAN_POINT('Ctrl Pts',(17.2566464335356,20.7325433010826,4.81155040995274));
#184390=CARTESIAN_POINT('Ctrl Pts',(17.1684428879449,20.6416304561368,4.80477952094794));
#184391=CARTESIAN_POINT('Ctrl Pts',(17.0581895207994,20.5054980196726,4.79524214939786));
#184392=CARTESIAN_POINT('Ctrl Pts',(17.0288241449381,20.4665640012752,4.79257592184906));
#184393=CARTESIAN_POINT('Ctrl Pts',(16.948992145448,20.352746517156,4.78487975546769));
#184394=CARTESIAN_POINT('Ctrl Pts',(16.901940447921,20.2756093575782,4.77977469201102));
#184395=CARTESIAN_POINT('Ctrl Pts',(16.8535750200627,20.1835632133618,4.77367864978252));
#184396=CARTESIAN_POINT('Ctrl Pts',(16.847310418368,20.1713539547953,4.77287010304112));
#184397=CARTESIAN_POINT('Ctrl Pts',(16.8374528503508,20.1516734917865,4.77156647275801));
#184398=CARTESIAN_POINT('Ctrl Pts',(16.8337842369422,20.1442404619583,4.77107404079419));
#184399=CARTESIAN_POINT('Ctrl Pts',(16.8273471399922,20.1310028407844,4.77019685407985));
#184400=CARTESIAN_POINT('Ctrl Pts',(16.8245612602085,20.1252067890809,4.76981271123662));
#184401=CARTESIAN_POINT('Ctrl Pts',(16.8188109965202,20.11310235761,4.76901028530552));
#184402=CARTESIAN_POINT('Ctrl Pts',(16.815851276527,20.1067918594664,4.76859184628077));
#184403=CARTESIAN_POINT('Ctrl Pts',(16.808244173595,20.0903619825484,4.76750207988746));
#184404=CARTESIAN_POINT('Ctrl Pts',(16.8036454185036,20.0802204447428,4.76682908655037));
#184405=CARTESIAN_POINT('Ctrl Pts',(16.7840055964983,20.0359845319037,4.76389185826396));
#184406=CARTESIAN_POINT('Ctrl Pts',(16.7697869657525,20.001534332524,4.76159978792033));
#184407=CARTESIAN_POINT('Ctrl Pts',(16.7527228285433,19.9568826108312,4.75862125090952));
#184408=CARTESIAN_POINT('Ctrl Pts',(16.7490340127606,19.9470095736933,4.75796219637102));
#184409=CARTESIAN_POINT('Ctrl Pts',(16.745419360568,19.9371102123481,4.75730092050388));
#184410=CARTESIAN_POINT('Ctrl Pts',(16.7454193895773,19.9371102917951,4.53222340700496));
#184411=CARTESIAN_POINT('Ctrl Pts',(16.7547724031316,19.9627251627221,4.5339728589152));
#184412=CARTESIAN_POINT('Ctrl Pts',(16.7646216281624,19.9881628702676,4.53573529112474));
#184413=CARTESIAN_POINT('Ctrl Pts',(16.8069143125145,20.0914181420184,4.54298757155657));
#184414=CARTESIAN_POINT('Ctrl Pts',(16.8434960439116,20.1674460000309,4.54856267278766));
#184415=CARTESIAN_POINT('Ctrl Pts',(16.9297171882361,20.3222534345793,4.5602691081327));
#184416=CARTESIAN_POINT('Ctrl Pts',(16.9802211974873,20.4003624888217,4.56638699544503));
#184417=CARTESIAN_POINT('Ctrl Pts',(17.0541350598679,20.4996801506508,4.57424155302913));
#184418=CARTESIAN_POINT('Ctrl Pts',(17.0731139875003,20.5240501261232,4.5761749357766));
#184419=CARTESIAN_POINT('Ctrl Pts',(17.0971204775874,20.5535219546146,4.57851181434706));
#184420=CARTESIAN_POINT('Ctrl Pts',(17.101648400782,20.5590237495591,4.57894800520774));
#184421=CARTESIAN_POINT('Ctrl Pts',(17.1088155012202,20.5676432942862,4.5796311420402));
#184422=CARTESIAN_POINT('Ctrl Pts',(17.1114360225727,20.5707763870626,4.57987940431196));
#184423=CARTESIAN_POINT('Ctrl Pts',(17.1163676776681,20.5766381131326,4.58034375514298));
#184424=CARTESIAN_POINT('Ctrl Pts',(17.1186766300381,20.5793684434234,4.58055998973853));
#184425=CARTESIAN_POINT('Ctrl Pts',(17.1239849536179,20.5856133631342,4.58105446202591));
#184426=CARTESIAN_POINT('Ctrl Pts',(17.126988915279,20.5891239865106,4.58133235742921));
#184427=CARTESIAN_POINT('Ctrl Pts',(17.134898392322,20.5983064843049,4.58205911693098));
#184428=CARTESIAN_POINT('Ctrl Pts',(17.1398226420926,20.6039622350875,4.58250663461414));
#184429=CARTESIAN_POINT('Ctrl Pts',(17.1733079994211,20.6420117237219,4.58551752225174));
#184430=CARTESIAN_POINT('Ctrl Pts',(17.2028266717027,20.6735535495631,4.58801438268116));
#184431=CARTESIAN_POINT('Ctrl Pts',(17.2842045091331,20.7553420801205,4.59456222978682));
#184432=CARTESIAN_POINT('Ctrl Pts',(17.3377044100379,20.8038777115785,4.59852795480883));
#184433=CARTESIAN_POINT('Ctrl Pts',(17.4624081722022,20.9058893944541,4.60730940827461));
#184434=CARTESIAN_POINT('Ctrl Pts',(17.534711715258,20.9577980077863,4.61210237594066));
#184435=CARTESIAN_POINT('Ctrl Pts',(17.6709782681035,21.0431682831148,4.62094043598707));
#184436=CARTESIAN_POINT('Ctrl Pts',(17.7337916214673,21.0782005235154,4.62494614642702));
#184437=CARTESIAN_POINT('Ctrl Pts',(17.822789608461,21.1220552925393,4.63062060121498));
#184438=CARTESIAN_POINT('Ctrl Pts',(17.8475487036928,21.1336650026921,4.63219883417538));
#184439=CARTESIAN_POINT('Ctrl Pts',(17.8907913189896,21.1529289372445,4.63495900587287));
#184440=CARTESIAN_POINT('Ctrl Pts',(17.90917157596,21.160806889793,4.63613334678326));
#184441=CARTESIAN_POINT('Ctrl Pts',(17.9357429790224,21.1717526987597,4.63783378020182));
#184442=CARTESIAN_POINT('Ctrl Pts',(17.9438461872591,21.1750321702946,4.63835270503047));
#184443=CARTESIAN_POINT('Ctrl Pts',(17.9580191020464,21.1806662226505,4.63926105522602));
#184444=CARTESIAN_POINT('Ctrl Pts',(17.9640798291557,21.1830431820084,4.63964972040308));
#184445=CARTESIAN_POINT('Ctrl Pts',(17.9757324035469,21.1875513052105,4.6403974615899));
#184446=CARTESIAN_POINT('Ctrl Pts',(17.9813225198315,21.1896867917042,4.64075638784115));
#184447=CARTESIAN_POINT('Ctrl Pts',(17.9959422523476,21.1952007733782,4.64169566810272));
#184448=CARTESIAN_POINT('Ctrl Pts',(18.0049859501767,21.1985413098335,4.64227728532399));
#184449=CARTESIAN_POINT('Ctrl Pts',(18.0362110509937,21.2098333647504,4.64428761315423));
#184450=CARTESIAN_POINT('Ctrl Pts',(18.0585015738364,21.2174760260821,4.64572651785464));
#184451=CARTESIAN_POINT('Ctrl Pts',(18.2398094051443,21.2762766970307,4.65746513332573));
#184452=CARTESIAN_POINT('Ctrl Pts',(18.40421679544,21.3088119272805,4.66839452133173));
#184453=CARTESIAN_POINT('Ctrl Pts',(18.6959959875962,21.331386176601,4.68773428716091));
#184454=CARTESIAN_POINT('Ctrl Pts',(18.8219189870175,21.3299050765897,4.69603952767565));
#184455=CARTESIAN_POINT('Ctrl Pts',(18.9588894693142,21.3160551248909,4.70457755196367));
#184456=CARTESIAN_POINT('Ctrl Pts',(18.9707915911399,21.3147495359008,4.70531519899863));
#184457=CARTESIAN_POINT('Ctrl Pts',(18.9876810792895,21.3127517092587,4.70635526248402));
#184458=CARTESIAN_POINT('Ctrl Pts',(18.9926777868767,21.3121425799167,4.7066621301672));
#184459=CARTESIAN_POINT('Ctrl Pts',(19.0012794044883,21.3110628409443,4.70718890010166));
#184460=CARTESIAN_POINT('Ctrl Pts',(19.0048853465937,21.3106007586581,4.70740927891704));
#184461=CARTESIAN_POINT('Ctrl Pts',(19.0118701489965,21.3096873993242,4.70783526238312));
#184462=CARTESIAN_POINT('Ctrl Pts',(19.0152491096885,21.3092372502806,4.70804093187515));
#184463=CARTESIAN_POINT('Ctrl Pts',(19.0243530967718,21.3080020197958,4.70859401717607));
#184464=CARTESIAN_POINT('Ctrl Pts',(19.0300760689755,21.3072016494114,4.70894057576158));
#184465=CARTESIAN_POINT('Ctrl Pts',(19.0512492589261,21.3041520900465,4.71021880974948));
#184466=CARTESIAN_POINT('Ctrl Pts',(19.0666781637117,21.3017553744563,4.71114251818596));
#184467=CARTESIAN_POINT('Ctrl Pts',(19.2162896517319,21.2768166665044,4.7200365213711));
#184468=CARTESIAN_POINT('Ctrl Pts',(19.3480498235207,21.2415553121407,4.72738866559904));
#184469=CARTESIAN_POINT('Ctrl Pts',(19.6208175470008,21.1395499936416,4.74320315406878));
#184470=CARTESIAN_POINT('Ctrl Pts',(19.7596770207882,21.069421268459,4.75165213867748));
#184471=CARTESIAN_POINT('Ctrl Pts',(19.9074470201853,20.9731474323135,4.76192312587365));
#184472=CARTESIAN_POINT('Ctrl Pts',(19.9250932403537,20.9612680727889,4.76317138994192));
#184473=CARTESIAN_POINT('Ctrl Pts',(19.9499376788251,20.943993183069,4.76496143526196));
#184474=CARTESIAN_POINT('Ctrl Pts',(19.95728550718,20.9388143347817,4.76549497927053));
#184475=CARTESIAN_POINT('Ctrl Pts',(19.9699075504003,20.929797275118,4.7664187626107));
#184476=CARTESIAN_POINT('Ctrl Pts',(19.97519745931,20.9259811694662,4.76680814775332));
#184477=CARTESIAN_POINT('Ctrl Pts',(19.9852943117695,20.9186261813015,4.76755568547137));
#184478=CARTESIAN_POINT('Ctrl Pts',(19.9901040962707,20.9150912909615,4.76791368066152));
#184479=CARTESIAN_POINT('Ctrl Pts',(20.0025768158454,20.9058431266994,4.76884701356077));
#184480=CARTESIAN_POINT('Ctrl Pts',(20.0102160580531,20.9000982595164,4.76942358334729));
#184481=CARTESIAN_POINT('Ctrl Pts',(20.0361560255342,20.8803144372035,4.77139846675003));
#184482=CARTESIAN_POINT('Ctrl Pts',(20.0542655948021,20.8660286094909,4.77280649815665));
#184483=CARTESIAN_POINT('Ctrl Pts',(20.2073526595561,20.7411534018292,4.78496747018673));
#184484=CARTESIAN_POINT('Ctrl Pts',(20.3283879088352,20.6145817154827,4.79641511794876));
#184485=CARTESIAN_POINT('Ctrl Pts',(20.4848585158912,20.4042629949358,4.81373572183579));
#184486=CARTESIAN_POINT('Ctrl Pts',(20.5327921438261,20.3307012440144,4.81951808435455));
#184487=CARTESIAN_POINT('Ctrl Pts',(20.5947541723614,20.2213102731512,4.82754600037828));
#184488=CARTESIAN_POINT('Ctrl Pts',(20.612590037135,20.1877460395428,4.82993653044006));
#184489=CARTESIAN_POINT('Ctrl Pts',(20.6328900472641,20.1469289886025,4.83274178313648));
#184490=CARTESIAN_POINT('Ctrl Pts',(20.6362298399888,20.1401222326234,4.83320625804087));
#184491=CARTESIAN_POINT('Ctrl Pts',(20.6413560478656,20.1295311187441,4.83392363258702));
#184492=CARTESIAN_POINT('Ctrl Pts',(20.6431678931797,20.1257592392439,4.8341780713481));
#184493=CARTESIAN_POINT('Ctrl Pts',(20.6465020166357,20.1187652423503,4.8346478981996));
#184494=CARTESIAN_POINT('Ctrl Pts',(20.6480273297439,20.1155446811237,4.8348634692277));
#184495=CARTESIAN_POINT('Ctrl Pts',(20.6514506913586,20.1082691295567,4.83534873537581));
#184496=CARTESIAN_POINT('Ctrl Pts',(20.6533440072738,20.1042119721746,4.83561813643903));
#184497=CARTESIAN_POINT('Ctrl Pts',(20.6588751328043,20.0922606163445,4.8364082750482));
#184498=CARTESIAN_POINT('Ctrl Pts',(20.66247726278,20.0843498746848,4.8369268647328));
#184499=CARTESIAN_POINT('Ctrl Pts',(20.6875903738253,20.0282852273785,4.84057263600805));
#184500=CARTESIAN_POINT('Ctrl Pts',(20.7073459139531,19.979360191637,4.8436007460277));
#184501=CARTESIAN_POINT('Ctrl Pts',(20.7306239365612,19.9148692673999,4.84745858327113));
#184502=CARTESIAN_POINT('Ctrl Pts',(20.7358262865938,19.8999344131664,4.84834285558233));
#184503=CARTESIAN_POINT('Ctrl Pts',(20.7570370098401,19.8367732732829,4.85204951361411));
#184504=CARTESIAN_POINT('Ctrl Pts',(20.7714741991618,19.7880356728824,4.85482939570848));
#184505=CARTESIAN_POINT('Ctrl Pts',(20.8114224450757,19.6328710624809,4.86355299253518));
#184506=CARTESIAN_POINT('Ctrl Pts',(20.8304458556555,19.5249635426065,4.86944395434718));
#184507=CARTESIAN_POINT('Ctrl Pts',(20.8463892184264,19.3611523036757,4.87859496729409));
#184508=CARTESIAN_POINT('Ctrl Pts',(20.8495848999776,19.306046346207,4.88170631117984));
#184509=CARTESIAN_POINT('Ctrl Pts',(20.851271223758,19.2165476221695,4.88685609271407));
#184510=CARTESIAN_POINT('Ctrl Pts',(20.851082629538,19.1822049718464,4.88885502671365));
#184511=CARTESIAN_POINT('Ctrl Pts',(20.84973654013,19.137075681761,4.89151775727164));
#184512=CARTESIAN_POINT('Ctrl Pts',(20.849331380304,19.1262706839147,4.89215797844407));
#184513=CARTESIAN_POINT('Ctrl Pts',(20.8485321514039,19.1085774604239,4.89321094859615));
#184514=CARTESIAN_POINT('Ctrl Pts',(20.8481871467756,19.1016871342869,4.89362215477677));
#184515=CARTESIAN_POINT('Ctrl Pts',(20.847454076057,19.0883519063292,4.89442025010244));
#184516=CARTESIAN_POINT('Ctrl Pts',(20.8470701933843,19.0819068441732,4.89480700353001));
#184517=CARTESIAN_POINT('Ctrl Pts',(20.8461156684166,19.0670282942449,4.89570224216919));
#184518=CARTESIAN_POINT('Ctrl Pts',(20.8455239900448,19.0585963089127,4.89621138286472));
#184519=CARTESIAN_POINT('Ctrl Pts',(20.8437967253615,19.0359263433742,4.89758515815393));
#184520=CARTESIAN_POINT('Ctrl Pts',(20.8425675317957,19.0216961285327,4.89845271728173));
#184521=CARTESIAN_POINT('Ctrl Pts',(20.8276340102067,18.8670784543557,4.90793751289946));
#184522=CARTESIAN_POINT('Ctrl Pts',(20.800078219931,18.7284102787073,4.91700442466364));
#184523=CARTESIAN_POINT('Ctrl Pts',(20.7307663204369,18.5011051192184,4.93263823563054));
#184524=CARTESIAN_POINT('Ctrl Pts',(20.6962868452609,18.4107144161009,4.93906604169451));
#184525=CARTESIAN_POINT('Ctrl Pts',(20.6352164816006,18.2785505635589,4.94856667560684));
#184526=CARTESIAN_POINT('Ctrl Pts',(20.6131425756001,18.2348289723727,4.9517261918189));
#184527=CARTESIAN_POINT('Ctrl Pts',(20.5769352273177,18.1689022368994,4.95647581505038));
#184528=CARTESIAN_POINT('Ctrl Pts',(20.5638719655971,18.1461306483408,4.95811352970189));
#184529=CARTESIAN_POINT('Ctrl Pts',(20.5469161901493,18.1178076244426,4.96014129394114));
#184530=CARTESIAN_POINT('Ctrl Pts',(20.5434166961062,18.1120250661705,4.96055479985511));
#184531=CARTESIAN_POINT('Ctrl Pts',(20.5378004520503,18.1028443452635,4.96121039597595));
#184532=CARTESIAN_POINT('Ctrl Pts',(20.535701687957,18.0994353126474,4.96145363432592));
#184533=CARTESIAN_POINT('Ctrl Pts',(20.5317008918475,18.0929779012346,4.9619139649244));
#184534=CARTESIAN_POINT('Ctrl Pts',(20.5298007934423,18.0899284499628,4.96213117210257));
#184535=CARTESIAN_POINT('Ctrl Pts',(20.5254067744917,18.0829163641073,4.96263024086052));
#184536=CARTESIAN_POINT('Ctrl Pts',(20.5229074662741,18.0789571565812,4.9629117425935));
#184537=CARTESIAN_POINT('Ctrl Pts',(20.5161686509784,18.0683601036956,4.96366452260831));
#184538=CARTESIAN_POINT('Ctrl Pts',(20.5119051549568,18.0617374984379,4.96413425617177));
#184539=CARTESIAN_POINT('Ctrl Pts',(20.4795578579187,18.0121023734511,4.96765064419475));
#184540=CARTESIAN_POINT('Ctrl Pts',(20.4499513632432,17.970097266647,4.9706029164804));
#184541=CARTESIAN_POINT('Ctrl Pts',(20.4053233164184,17.9114362331128,4.97475500542819));
#184542=CARTESIAN_POINT('Ctrl Pts',(20.3915226035269,17.8938794741043,4.97600161911873));
#184543=CARTESIAN_POINT('Ctrl Pts',(20.3484989233046,17.8408937569714,4.97978676898204));
#184544=CARTESIAN_POINT('Ctrl Pts',(20.3183982674685,17.8061938704881,4.98229791694414));
#184545=CARTESIAN_POINT('Ctrl Pts',(20.2128871495548,17.6922703497104,4.99075189548715));
#184546=CARTESIAN_POINT('Ctrl Pts',(20.1324782965989,17.617919800404,4.99664011503158));
#184547=CARTESIAN_POINT('Ctrl Pts',(20.0034505804157,17.5159419791502,5.00578475207915));
#184548=CARTESIAN_POINT('Ctrl Pts',(19.9588963326422,17.4834714766529,5.00889244094536));
#184549=CARTESIAN_POINT('Ctrl Pts',(19.8846336801858,17.4336682225758,5.0140367120459));
#184550=CARTESIAN_POINT('Ctrl Pts',(19.8556800741764,17.4152551050896,5.01603390139742));
#184551=CARTESIAN_POINT('Ctrl Pts',(19.8170338138094,17.3919772969146,5.01869463708521));
#184552=CARTESIAN_POINT('Ctrl Pts',(19.8077321923982,17.3864712913622,5.01933465309387));
#184553=CARTESIAN_POINT('Ctrl Pts',(19.7924260363541,17.3775685420849,5.02038737173758));
#184554=CARTESIAN_POINT('Ctrl Pts',(19.7864462696531,17.3741294457512,5.02079853301977));
#184555=CARTESIAN_POINT('Ctrl Pts',(19.7748370282912,17.3675280118672,5.02159660261079));
#184556=CARTESIAN_POINT('Ctrl Pts',(19.7692096780856,17.3643620789506,5.02198337552727));
#184557=CARTESIAN_POINT('Ctrl Pts',(19.7561805459115,17.3571101941001,5.02287874872795));
#184558=CARTESIAN_POINT('Ctrl Pts',(19.7487686313392,17.3530427608607,5.02338800511676));
#184559=CARTESIAN_POINT('Ctrl Pts',(19.7287643488092,17.3422204290836,5.02476229501168));
#184560=CARTESIAN_POINT('Ctrl Pts',(19.7161277915873,17.3355485397878,5.02563025646234));
#184561=CARTESIAN_POINT('Ctrl Pts',(19.5995665721896,17.2755072745005,5.0336362051208));
#184562=CARTESIAN_POINT('Ctrl Pts',(19.4914753091594,17.2307068564076,5.04107585443661));
#184563=CARTESIAN_POINT('Ctrl Pts',(19.225366708625,17.145399820272,5.05932908809907));
#184564=CARTESIAN_POINT('Ctrl Pts',(19.0652748172525,17.1137631505918,5.07028255410712));
#184565=CARTESIAN_POINT('Ctrl Pts',(18.8706538886571,17.0981637836033,5.08268982397046));
#184566=CARTESIAN_POINT('Ctrl Pts',(18.8381093147782,17.0963102630211,5.08473259130549));
#184567=CARTESIAN_POINT('Ctrl Pts',(18.7982917953702,17.0949640694958,5.08718250958665));
#184568=CARTESIAN_POINT('Ctrl Pts',(18.791049318659,17.0947564240208,5.08762613395383));
#184569=CARTESIAN_POINT('Ctrl Pts',(18.7796960202292,17.0944892456281,5.08831828107385));
#184570=CARTESIAN_POINT('Ctrl Pts',(18.7755859278407,17.0944044999324,5.08856817726714));
#184571=CARTESIAN_POINT('Ctrl Pts',(18.767904427225,17.0942684990994,5.08903392629171));
#184572=CARTESIAN_POINT('Ctrl Pts',(18.764333175357,17.0942143103766,5.08924993504588));
#184573=CARTESIAN_POINT('Ctrl Pts',(18.7561826254542,17.0941112682525,5.08974174246457));
#184574=CARTESIAN_POINT('Ctrl Pts',(18.7516033043237,17.0940682353811,5.09001721258166));
#184575=CARTESIAN_POINT('Ctrl Pts',(18.737534086303,17.0939816796058,5.09086104268522));
#184576=CARTESIAN_POINT('Ctrl Pts',(18.7280438570151,17.0939871066532,5.09142673467748));
#184577=CARTESIAN_POINT('Ctrl Pts',(18.6431550663979,17.0946064950797,5.09645796986016));
#184578=CARTESIAN_POINT('Ctrl Pts',(18.5678307116975,17.0991845255335,5.10071979605209));
#184579=CARTESIAN_POINT('Ctrl Pts',(18.4500663849144,17.1126840444024,5.10728229417409));
#184580=CARTESIAN_POINT('Ctrl Pts',(18.4073879595804,17.1189022693486,5.10963942608538));
#184581=CARTESIAN_POINT('Ctrl Pts',(18.2572775361348,17.1454790906703,5.11793904403986));
#184582=CARTESIAN_POINT('Ctrl Pts',(18.1512660163912,17.1728485943846,5.12382591689914));
#184583=CARTESIAN_POINT('Ctrl Pts',(17.9957398930832,17.2261335489584,5.13296742314825));
#184584=CARTESIAN_POINT('Ctrl Pts',(17.9443529376154,17.2460115302313,5.13607331751969));
#184585=CARTESIAN_POINT('Ctrl Pts',(17.8623244775952,17.2814801460156,5.1412148829299));
#184586=CARTESIAN_POINT('Ctrl Pts',(17.8311837804071,17.295853070767,5.14321121540479));
#184587=CARTESIAN_POINT('Ctrl Pts',(17.7907074571016,17.3157414483959,5.14587097127644));
#184588=CARTESIAN_POINT('Ctrl Pts',(17.7810445468789,17.3205816080224,5.14651088645943));
#184589=CARTESIAN_POINT('Ctrl Pts',(17.7652757054991,17.3286318581835,5.14756348150383));
#184590=CARTESIAN_POINT('Ctrl Pts',(17.7591475790864,17.3317982184476,5.14797462072292));
#184591=CARTESIAN_POINT('Ctrl Pts',(17.7473131683997,17.3379864419036,5.14877267768463));
#184592=CARTESIAN_POINT('Ctrl Pts',(17.741605013278,17.3410045771814,5.14915946019479));
#184593=CARTESIAN_POINT('Ctrl Pts',(17.7284539628243,17.3480352489271,5.1500548995994));
#184594=CARTESIAN_POINT('Ctrl Pts',(17.7210211588868,17.3520663376988,5.15056421290376));
#184595=CARTESIAN_POINT('Ctrl Pts',(17.7010897570283,17.3630309211966,5.15193875598499));
#184596=CARTESIAN_POINT('Ctrl Pts',(17.6886370645698,17.3700465503574,5.15280691538503));
#184597=CARTESIAN_POINT('Ctrl Pts',(17.574844574266,17.4356820841356,5.16082808391067));
#184598=CARTESIAN_POINT('Ctrl Pts',(17.4784761341347,17.5024781312564,5.16828408716822));
#184599=CARTESIAN_POINT('Ctrl Pts',(17.2619797984708,17.6807857422063,5.18660583212604));
#184600=CARTESIAN_POINT('Ctrl Pts',(17.1482848611456,17.7989423417665,5.19761347861307));
#184601=CARTESIAN_POINT('Ctrl Pts',(17.0301307043909,17.9542096716946,5.21000153862169));
#184602=CARTESIAN_POINT('Ctrl Pts',(17.011514269283,17.9798478310744,5.21198583008886));
#184603=CARTESIAN_POINT('Ctrl Pts',(16.9893908034225,18.0118005448169,5.21437540053925));
#184604=CARTESIAN_POINT('Ctrl Pts',(16.9853324120053,18.0177262459109,5.21481510907938));
#184605=CARTESIAN_POINT('Ctrl Pts',(16.9790063682987,18.0270645549086,5.21550251074813));
#184606=CARTESIAN_POINT('Ctrl Pts',(16.9767183761698,18.0304632235029,5.21575154709066));
#184607=CARTESIAN_POINT('Ctrl Pts',(16.9724530902216,18.0368389137305,5.21621655535392));
#184608=CARTESIAN_POINT('Ctrl Pts',(16.9704734906456,18.0398142662742,5.21643267800726));
#184609=CARTESIAN_POINT('Ctrl Pts',(16.965962634248,18.0466314846174,5.21692586518573));
#184610=CARTESIAN_POINT('Ctrl Pts',(16.9634363651837,18.0504765912347,5.21720259403024));
#184611=CARTESIAN_POINT('Ctrl Pts',(16.9568611826751,18.0605557899601,5.21792430339818));
#184612=CARTESIAN_POINT('Ctrl Pts',(16.9528324936584,18.0668030875385,5.21836796768994));
#184613=CARTESIAN_POINT('Ctrl Pts',(16.926302248451,18.1084232971088,5.22130035610816));
#184614=CARTESIAN_POINT('Ctrl Pts',(16.9048211309003,18.1444392942485,5.22372644549766));
#184615=CARTESIAN_POINT('Ctrl Pts',(16.8738463903104,18.2000647307905,5.22734415302085));
#184616=CARTESIAN_POINT('Ctrl Pts',(16.8635633226522,18.2192196524102,5.22856741894502));
#184617=CARTESIAN_POINT('Ctrl Pts',(16.8457315551936,18.2537001718309,5.23073542111984));
#184618=CARTESIAN_POINT('Ctrl Pts',(16.8380699937973,18.268964909688,5.23168355708691));
#184619=CARTESIAN_POINT('Ctrl Pts',(16.7722507276487,18.4041582023236,5.23999251826942));
#184620=CARTESIAN_POINT('Ctrl Pts',(16.7253544921118,18.5292383492191,5.24709266696999));
#184621=CARTESIAN_POINT('Ctrl Pts',(16.6648838067213,18.7526521436461,5.25986483911706));
#184622=CARTESIAN_POINT('Ctrl Pts',(16.6458617353918,18.8490613194394,5.26540003990553));
#184623=CARTESIAN_POINT('Ctrl Pts',(16.6317631834271,18.9609907874177,5.27201864742314));
#184624=CARTESIAN_POINT('Ctrl Pts',(16.6300811152861,18.9755651902119,5.27288398401178));
#184625=CARTESIAN_POINT('Ctrl Pts',(16.627743251156,18.9978535302092,5.27421314617396));
#184626=CARTESIAN_POINT('Ctrl Pts',(16.6269780363235,19.005555720974,5.27467352386008));
#184627=CARTESIAN_POINT('Ctrl Pts',(16.6257184970672,19.018981494221,5.27547792086462));
#184628=CARTESIAN_POINT('Ctrl Pts',(16.6252051970251,19.0247032471825,5.27582133899206));
#184629=CARTESIAN_POINT('Ctrl Pts',(16.6241033853434,19.0375735783999,5.27659519862606));
#184630=CARTESIAN_POINT('Ctrl Pts',(16.6235279049997,19.0447231750921,5.27702604581187));
#184631=CARTESIAN_POINT('Ctrl Pts',(16.6220830311232,19.0638914665212,5.27818379777301));
#184632=CARTESIAN_POINT('Ctrl Pts',(16.6212799116562,19.0759147567252,5.27891277405855));
#184633=CARTESIAN_POINT('Ctrl Pts',(16.6181723376119,19.1292856913703,5.28216140879962));
#184634=CARTESIAN_POINT('Ctrl Pts',(16.6169788915335,19.1706865691505,5.28471558063671));
#184635=CARTESIAN_POINT('Ctrl Pts',(16.6170878346041,19.3815723324421,5.29790820293532));
#184636=CARTESIAN_POINT('Ctrl Pts',(16.6375272207745,19.5504051819816,5.30913937631477));
#184637=CARTESIAN_POINT('Ctrl Pts',(16.6963015727514,19.7902026215764,5.325418800653));
#184638=CARTESIAN_POINT('Ctrl Pts',(16.7188568487697,19.8643641030618,5.33048898654639));
#184639=CARTESIAN_POINT('Ctrl Pts',(16.7454193775548,19.9371102588694,5.3354009189409));
#184640=CARTESIAN_POINT('Origin',(18.734,19.211,0.));
#184641=CARTESIAN_POINT('',(16.7454193623257,19.9371102171619,6.35350368608372));
#184642=CARTESIAN_POINT('',(16.7454193623258,19.9371102171621,6.13370787675019));
#184643=CARTESIAN_POINT('',(16.7454193623258,19.9371102171621,0.));
#184644=CARTESIAN_POINT('',(16.6170004208961,19.2123349433974,6.31236855845777));
#184645=CARTESIAN_POINT('Ctrl Pts',(16.7454193623257,19.9371102171619,6.35350368608372));
#184646=CARTESIAN_POINT('Ctrl Pts',(16.7415068896361,19.9263952220385,6.3528225148824));
#184647=CARTESIAN_POINT('Ctrl Pts',(16.7376809777106,19.9156484895932,6.35214624380759));
#184648=CARTESIAN_POINT('Ctrl Pts',(16.7125808673215,19.8432983391641,6.34763638594729));
#184649=CARTESIAN_POINT('Ctrl Pts',(16.6940722989538,19.7807658436308,6.34394655327977));
#184650=CARTESIAN_POINT('Ctrl Pts',(16.6377481840861,19.5521743616963,6.33087426327147));
#184651=CARTESIAN_POINT('Ctrl Pts',(16.6171077708269,19.3825741900344,6.32190080849233));
#184652=CARTESIAN_POINT('Ctrl Pts',(16.6170004208961,19.2123349433974,6.31236855845777));
#184653=CARTESIAN_POINT('Ctrl Pts',(16.6170004192108,19.2123322681752,6.31236840866332));
#184654=CARTESIAN_POINT('Ctrl Pts',(16.6169565155957,19.1425685851102,6.30846211078004));
#184655=CARTESIAN_POINT('Ctrl Pts',(16.6203610680012,19.0728499211983,6.30447846496045));
#184656=CARTESIAN_POINT('Ctrl Pts',(16.6282130558034,18.9931538165595,6.29977938873572));
#184657=CARTESIAN_POINT('Ctrl Pts',(16.6293006053898,18.9828858472482,6.29917122396499));
#184658=CARTESIAN_POINT('Ctrl Pts',(16.6312636169845,18.9655631792681,6.29814040880299));
#184659=CARTESIAN_POINT('Ctrl Pts',(16.6320995838046,18.9585041228973,6.29771899770064));
#184660=CARTESIAN_POINT('Ctrl Pts',(16.6337050914328,18.9455077401542,6.29694059639473));
#184661=CARTESIAN_POINT('Ctrl Pts',(16.634464299231,18.9395691928747,6.29658393470745));
#184662=CARTESIAN_POINT('Ctrl Pts',(16.6360836208655,18.9273162371326,6.29584597873218));
#184663=CARTESIAN_POINT('Ctrl Pts',(16.6369470759956,18.9210023384499,6.29546458234972));
#184664=CARTESIAN_POINT('Ctrl Pts',(16.6389493188803,18.9068379206268,6.29460638823001));
#184665=CARTESIAN_POINT('Ctrl Pts',(16.6401037459456,18.8989897412374,6.29412909998424));
#184666=CARTESIAN_POINT('Ctrl Pts',(16.6431530579818,18.8790389677552,6.29291117245185));
#184667=CARTESIAN_POINT('Ctrl Pts',(16.6451089122256,18.8669461155635,6.29216861091687));
#184668=CARTESIAN_POINT('Ctrl Pts',(16.6571576857211,18.7963431733557,6.28780731602315));
#184669=CARTESIAN_POINT('Ctrl Pts',(16.669602709355,18.7382664482567,6.28411436415114));
#184670=CARTESIAN_POINT('Ctrl Pts',(16.6998137463031,18.621484745341,6.27646813719084));
#184671=CARTESIAN_POINT('Ctrl Pts',(16.717722832186,18.5628739506456,6.27251385443586));
#184672=CARTESIAN_POINT('Ctrl Pts',(16.7924559939099,18.3515665971345,6.25787329615711));
#184673=CARTESIAN_POINT('Ctrl Pts',(16.8643036033861,18.2047920773384,6.24690410269838));
#184674=CARTESIAN_POINT('Ctrl Pts',(16.9697240495311,18.0405025951793,6.23450257797181));
#184675=CARTESIAN_POINT('Ctrl Pts',(16.987802329498,18.0136998020795,6.23247694995395));
#184676=CARTESIAN_POINT('Ctrl Pts',(17.0106658357274,17.9814225980431,6.23004470045211));
#184677=CARTESIAN_POINT('Ctrl Pts',(17.0148734519403,17.9755465834849,6.22960221030077));
#184678=CARTESIAN_POINT('Ctrl Pts',(17.0215192307861,17.9663653220214,6.22891143743443));
#184679=CARTESIAN_POINT('Ctrl Pts',(17.0239370153296,17.9630454913432,6.22866179006326));
#184680=CARTESIAN_POINT('Ctrl Pts',(17.028475893849,17.9568511712821,6.2281962564559));
#184681=CARTESIAN_POINT('Ctrl Pts',(17.0305945790737,17.9539750466186,6.22798021579625));
#184682=CARTESIAN_POINT('Ctrl Pts',(17.0354495871139,17.9474191667884,6.22748801396749));
#184683=CARTESIAN_POINT('Ctrl Pts',(17.038190586786,17.9437429376256,6.22721218338876));
#184684=CARTESIAN_POINT('Ctrl Pts',(17.0466593324388,17.9324613345757,6.22636615020504));
#184685=CARTESIAN_POINT('Ctrl Pts',(17.0524265475302,17.9248855498061,6.2257986358639));
#184686=CARTESIAN_POINT('Ctrl Pts',(17.131399595986,17.8225863412034,6.21813967631868));
#184687=CARTESIAN_POINT('Ctrl Pts',(17.2124720665144,17.7341853090147,6.21156686849477));
#184688=CARTESIAN_POINT('Ctrl Pts',(17.3807398236116,17.579363810668,6.19912101925036));
#184689=CARTESIAN_POINT('Ctrl Pts',(17.4664542438363,17.5119189009061,6.19325458438613));
#184690=CARTESIAN_POINT('Ctrl Pts',(17.602337401369,17.4210258510781,6.18416056430124));
#184691=CARTESIAN_POINT('Ctrl Pts',(17.6488553017149,17.3924489159956,6.18108186558282));
#184692=CARTESIAN_POINT('Ctrl Pts',(17.7161508456552,17.3546098654913,6.17663925726683));
#184693=CARTESIAN_POINT('Ctrl Pts',(17.7360547168734,17.3438346648476,6.17532671917997));
#184694=CARTESIAN_POINT('Ctrl Pts',(17.7713963088992,17.3254285944372,6.17299628147911));
#184695=CARTESIAN_POINT('Ctrl Pts',(17.7867617135374,17.3176630003485,6.1719831268734));
#184696=CARTESIAN_POINT('Ctrl Pts',(17.8095970250455,17.3064697062356,6.17047677323766));
#184697=CARTESIAN_POINT('Ctrl Pts',(17.8169951643321,17.3028965886442,6.16998864911109));
#184698=CARTESIAN_POINT('Ctrl Pts',(17.8299402229467,17.2967371196819,6.16913429260064));
#184699=CARTESIAN_POINT('Ctrl Pts',(17.8354779406155,17.2941315738855,6.16876873132942));
#184700=CARTESIAN_POINT('Ctrl Pts',(17.8465312432968,17.2889893179297,6.16803887857226));
#184701=CARTESIAN_POINT('Ctrl Pts',(17.8520465971253,17.2864522479085,6.1676746038834));
#184702=CARTESIAN_POINT('Ctrl Pts',(17.8652482178071,17.2804481515462,6.16680241094147));
#184703=CARTESIAN_POINT('Ctrl Pts',(17.8729443910845,17.277003274623,6.16629373687422));
#184704=CARTESIAN_POINT('Ctrl Pts',(17.9007359895117,17.2647622742867,6.16445598627644));
#184705=CARTESIAN_POINT('Ctrl Pts',(17.9209467244247,17.2562328756557,6.1631178586342));
#184706=CARTESIAN_POINT('Ctrl Pts',(18.1149099096541,17.1779043529848,6.15025580521359));
#184707=CARTESIAN_POINT('Ctrl Pts',(18.2970384827337,17.1311474235341,6.13791611220657));
#184708=CARTESIAN_POINT('Ctrl Pts',(18.590169829228,17.0961299255959,6.11842865333243));
#184709=CARTESIAN_POINT('Ctrl Pts',(18.6982876997502,17.0915443065402,6.11134587412142));
#184710=CARTESIAN_POINT('Ctrl Pts',(18.818076798322,17.0956373579118,6.10391453086623));
#184711=CARTESIAN_POINT('Ctrl Pts',(18.8298571490593,17.0961384354843,6.1031882747177));
#184712=CARTESIAN_POINT('Ctrl Pts',(18.8466289590057,17.0969922559585,6.10216137923623));
#184713=CARTESIAN_POINT('Ctrl Pts',(18.8516240580739,17.0972643007188,6.10185643752921));
#184714=CARTESIAN_POINT('Ctrl Pts',(18.8602421026819,17.0977643036436,6.10133192220937));
#184715=CARTESIAN_POINT('Ctrl Pts',(18.8638654965303,17.0979838783303,6.10111188277366));
#184716=CARTESIAN_POINT('Ctrl Pts',(18.8708989996912,17.098428263302,6.10068572536461));
#184717=CARTESIAN_POINT('Ctrl Pts',(18.8743091279023,17.0986520107185,6.10047954649683));
#184718=CARTESIAN_POINT('Ctrl Pts',(18.8835278942027,17.0992793007773,6.09992332590626));
#184719=CARTESIAN_POINT('Ctrl Pts',(18.8893354836968,17.0996985549199,6.09957415889668));
#184720=CARTESIAN_POINT('Ctrl Pts',(18.9109978308911,17.1013522423937,6.09827613890788));
#184721=CARTESIAN_POINT('Ctrl Pts',(18.9268407033244,17.1027413843944,6.0973355741368));
#184722=CARTESIAN_POINT('Ctrl Pts',(19.0615894733413,17.1160881985625,6.08939895648375));
#184723=CARTESIAN_POINT('Ctrl Pts',(19.1793174165336,17.1379177183873,6.08287716869521));
#184724=CARTESIAN_POINT('Ctrl Pts',(19.3146076221558,17.1750690365644,6.07525157666226));
#184725=CARTESIAN_POINT('Ctrl Pts',(19.3345474168016,17.1808613591687,6.0741244965783));
#184726=CARTESIAN_POINT('Ctrl Pts',(19.4981736546786,17.2310149241983,6.0648296390241));
#184727=CARTESIAN_POINT('Ctrl Pts',(19.6368246428032,17.2902702806385,6.05661875674878));
#184728=CARTESIAN_POINT('Ctrl Pts',(19.7866497988288,17.3741349812198,6.04662022869469));
#184729=CARTESIAN_POINT('Ctrl Pts',(19.8051179017931,17.3848425348311,6.0453676051467));
#184730=CARTESIAN_POINT('Ctrl Pts',(19.8311392445454,17.4004598819164,6.04357238647367));
#184731=CARTESIAN_POINT('Ctrl Pts',(19.8388283240229,17.4051416412863,6.04303809467623));
#184732=CARTESIAN_POINT('Ctrl Pts',(19.8520386863013,17.413301173094,6.04211342597836));
#184733=CARTESIAN_POINT('Ctrl Pts',(19.8575742217757,17.4167557181318,6.04172390769436));
#184734=CARTESIAN_POINT('Ctrl Pts',(19.8681406098919,17.4234179249885,6.04097640017878));
#184735=CARTESIAN_POINT('Ctrl Pts',(19.873174053312,17.4266213762106,6.04061856970972));
#184736=CARTESIAN_POINT('Ctrl Pts',(19.8862234551213,17.4350041693775,6.03968629443089));
#184737=CARTESIAN_POINT('Ctrl Pts',(19.894217985573,17.4402164722338,6.03911062305968));
#184738=CARTESIAN_POINT('Ctrl Pts',(19.9213380639449,17.4581608146675,6.03714209289007));
#184739=CARTESIAN_POINT('Ctrl Pts',(19.9402909418736,17.4711497231062,6.03573960073047));
#184740=CARTESIAN_POINT('Ctrl Pts',(20.1023489603674,17.5861333331857,6.02350908742361));
#184741=CARTESIAN_POINT('Ctrl Pts',(20.232424736463,17.7052542249308,6.01197518188425));
#184742=CARTESIAN_POINT('Ctrl Pts',(20.4025476063424,17.9051747710723,5.99463124731251));
#184743=CARTESIAN_POINT('Ctrl Pts',(20.4547084097663,17.9747172150472,5.98890822571665));
#184744=CARTESIAN_POINT('Ctrl Pts',(20.5232203794133,18.078830946225,5.98095120531324));
#184745=CARTESIAN_POINT('Ctrl Pts',(20.5431413093442,18.1109434268952,5.97857480656709));
#184746=CARTESIAN_POINT('Ctrl Pts',(20.5660099146122,18.1501107659587,5.97578388234448));
#184747=CARTESIAN_POINT('Ctrl Pts',(20.5697914552091,18.1566679692348,5.97532018129335));
#184748=CARTESIAN_POINT('Ctrl Pts',(20.575607443078,18.1668790719648,5.97460374172046));
#184749=CARTESIAN_POINT('Ctrl Pts',(20.5776663262049,18.1705188780772,5.97434947037159));
#184750=CARTESIAN_POINT('Ctrl Pts',(20.5814598464087,18.1772718846935,5.97387979824542));
#184751=CARTESIAN_POINT('Ctrl Pts',(20.5831973923774,18.1803833376125,5.97366421551522));
#184752=CARTESIAN_POINT('Ctrl Pts',(20.5871018201758,18.1874167253598,5.97317872850792));
#184753=CARTESIAN_POINT('Ctrl Pts',(20.5892641066467,18.191341149453,5.97290911947326));
#184754=CARTESIAN_POINT('Ctrl Pts',(20.5955921278758,18.2029129088761,5.9721178050488));
#184755=CARTESIAN_POINT('Ctrl Pts',(20.5997232136719,18.210579223666,5.97159825710449));
#184756=CARTESIAN_POINT('Ctrl Pts',(20.6287270562532,18.2652080140096,5.96792775935897));
#184757=CARTESIAN_POINT('Ctrl Pts',(20.651873235906,18.3130710726034,5.96487741648899));
#184758=CARTESIAN_POINT('Ctrl Pts',(20.6798121033316,18.376867917237,5.96095996447022));
#184759=CARTESIAN_POINT('Ctrl Pts',(20.6862522894806,18.39205428076,5.96003817743331));
#184760=CARTESIAN_POINT('Ctrl Pts',(20.7491920882494,18.5454333388108,5.95082138560431));
#184761=CARTESIAN_POINT('Ctrl Pts',(20.791101642102,18.6891623393364,5.94290867633278));
#184762=CARTESIAN_POINT('Ctrl Pts',(20.8284515169959,18.8967433226113,5.93123900740156));
#184763=CARTESIAN_POINT('Ctrl Pts',(20.8367085905795,18.9578199314932,5.92778147937456));
#184764=CARTESIAN_POINT('Ctrl Pts',(20.8456588766408,19.0561854772819,5.92211276298996));
#184765=CARTESIAN_POINT('Ctrl Pts',(20.8480514786509,19.0932848975868,5.91995236629277));
#184766=CARTESIAN_POINT('Ctrl Pts',(20.8498895661266,19.1415440858307,5.91710550848403));
#184767=CARTESIAN_POINT('Ctrl Pts',(20.8502253572454,19.1526646739699,5.91644698714222));
#184768=CARTESIAN_POINT('Ctrl Pts',(20.8506288686729,19.1707534518912,5.91537156434363));
#184769=CARTESIAN_POINT('Ctrl Pts',(20.8507498704511,19.1777203290985,5.91495633670887));
#184770=CARTESIAN_POINT('Ctrl Pts',(20.8509164123178,19.191118653724,5.91415576367178));
#184771=CARTESIAN_POINT('Ctrl Pts',(20.8509670427109,19.1975499691306,5.91377058237927));
#184772=CARTESIAN_POINT('Ctrl Pts',(20.8510158622436,19.2122751004777,5.9128865711026));
#184773=CARTESIAN_POINT('Ctrl Pts',(20.8509946200193,19.2205688361206,5.91238713746858));
#184774=CARTESIAN_POINT('Ctrl Pts',(20.8508087241339,19.242600213201,5.91105630173106));
#184775=CARTESIAN_POINT('Ctrl Pts',(20.8505590777554,19.2563365685638,5.91022225283596));
#184776=CARTESIAN_POINT('Ctrl Pts',(20.8476398587416,19.3609185330852,5.90383860603307));
#184777=CARTESIAN_POINT('Ctrl Pts',(20.8392567239194,19.4514981272216,5.8981102386584));
#184778=CARTESIAN_POINT('Ctrl Pts',(20.8031448642124,19.6801521332451,5.88315996263288));
#184779=CARTESIAN_POINT('Ctrl Pts',(20.767422157897,19.816519274104,5.87376079530364));
#184780=CARTESIAN_POINT('Ctrl Pts',(20.6996340287677,19.9989661971492,5.86102203016596));
#184781=CARTESIAN_POINT('Ctrl Pts',(20.6788842038614,20.0488747471659,5.85752348186857));
#184782=CARTESIAN_POINT('Ctrl Pts',(20.6444950821597,20.1234057475967,5.85233052105096));
#184783=CARTESIAN_POINT('Ctrl Pts',(20.632238314744,20.1486391548369,5.85057818432761));
#184784=CARTESIAN_POINT('Ctrl Pts',(20.6163414822344,20.1797761746192,5.84842992567003));
#184785=CARTESIAN_POINT('Ctrl Pts',(20.6131697982816,20.1859141523834,5.84800713607432));
#184786=CARTESIAN_POINT('Ctrl Pts',(20.608097485461,20.1956135835784,5.8473402619125));
#184787=CARTESIAN_POINT('Ctrl Pts',(20.6062166535164,20.1991852543446,5.8470949615153));
#184788=CARTESIAN_POINT('Ctrl Pts',(20.602646121178,20.2059188540867,5.84663303630614));
#184789=CARTESIAN_POINT('Ctrl Pts',(20.6009586259146,20.2090818311675,5.84641628365501));
#184790=CARTESIAN_POINT('Ctrl Pts',(20.5970768855037,20.2163133269775,5.84592122358843));
#184791=CARTESIAN_POINT('Ctrl Pts',(20.5948773467003,20.2203789517136,5.84564325642433));
#184792=CARTESIAN_POINT('Ctrl Pts',(20.588991542109,20.2311736353698,5.8449060971944));
#184793=CARTESIAN_POINT('Ctrl Pts',(20.5852819423108,20.237889985202,5.84444835095195));
#184794=CARTESIAN_POINT('Ctrl Pts',(20.5587289344699,20.2853535029882,5.84121890670733));
#184795=CARTESIAN_POINT('Ctrl Pts',(20.5345770239711,20.3253582120293,5.83852513941421));
#184796=CARTESIAN_POINT('Ctrl Pts',(20.5066902352816,20.3682718787163,5.83563022696328));
#184797=CARTESIAN_POINT('Ctrl Pts',(20.5042494338873,20.3720020731314,5.83537854795465));
#184798=CARTESIAN_POINT('Ctrl Pts',(20.488964655291,20.3952010204539,5.83381284591427));
#184799=CARTESIAN_POINT('Ctrl Pts',(20.475811128374,20.4144646014065,5.83251074399911));
#184800=CARTESIAN_POINT('Ctrl Pts',(20.436063257422,20.4706588647084,5.82869455095512));
#184801=CARTESIAN_POINT('Ctrl Pts',(20.4085930680496,20.5069545043392,5.82620629270073));
#184802=CARTESIAN_POINT('Ctrl Pts',(20.311206949939,20.6273559769229,5.81777526116459));
#184803=CARTESIAN_POINT('Ctrl Pts',(20.2359570160179,20.7069178635393,5.81188725091448));
#184804=CARTESIAN_POINT('Ctrl Pts',(20.1140504702378,20.8172959257157,5.80274310063257));
#184805=CARTESIAN_POINT('Ctrl Pts',(20.0717733010439,20.8526722727376,5.79963569084847));
#184806=CARTESIAN_POINT('Ctrl Pts',(20.0010165702779,20.9073298510568,5.79449184046196));
#184807=CARTESIAN_POINT('Ctrl Pts',(19.973362244009,20.9276382800376,5.79249478428642));
#184808=CARTESIAN_POINT('Ctrl Pts',(19.936362907771,20.9534492154566,5.78983420080694));
#184809=CARTESIAN_POINT('Ctrl Pts',(19.9274509174513,20.959565335212,5.78919420039052));
#184810=CARTESIAN_POINT('Ctrl Pts',(19.912775274409,20.9694724726168,5.78814150080957));
#184811=CARTESIAN_POINT('Ctrl Pts',(19.9070391670171,20.9733040871034,5.78773034288755));
#184812=CARTESIAN_POINT('Ctrl Pts',(19.8958978650463,20.9806677773008,5.78693227511242));
#184813=CARTESIAN_POINT('Ctrl Pts',(19.8904950303831,20.9842032974486,5.78654550062686));
#184814=CARTESIAN_POINT('Ctrl Pts',(19.877980389055,20.9923111330704,5.78565011693736));
#184815=CARTESIAN_POINT('Ctrl Pts',(19.8708572321126,20.9968656483333,5.78514085158098));
#184816=CARTESIAN_POINT('Ctrl Pts',(19.8516216677252,21.0090030635592,5.78376652196445));
#184817=CARTESIAN_POINT('Ctrl Pts',(19.8394596093548,21.016506091129,5.78289852949736));
#184818=CARTESIAN_POINT('Ctrl Pts',(19.7271457923959,21.0842346020385,5.7748902304401));
#184819=CARTESIAN_POINT('Ctrl Pts',(19.622260152372,21.1361837654899,5.76744805632574));
#184820=CARTESIAN_POINT('Ctrl Pts',(19.3623099480332,21.2391542491379,5.7491845267281));
#184821=CARTESIAN_POINT('Ctrl Pts',(19.2045759373841,21.2814447388487,5.7382229964832));
#184822=CARTESIAN_POINT('Ctrl Pts',(19.0114506289459,21.3099910378608,5.72581868878594));
#184823=CARTESIAN_POINT('Ctrl Pts',(18.979238999151,21.3139979384514,5.72378472573837));
#184824=CARTESIAN_POINT('Ctrl Pts',(18.9397468188438,21.3179906513314,5.72134388173058));
#184825=CARTESIAN_POINT('Ctrl Pts',(18.9325438129288,21.3186815974175,5.72090083859543));
#184826=CARTESIAN_POINT('Ctrl Pts',(18.9212452494466,21.3197069733,5.72020939567705));
#184827=CARTESIAN_POINT('Ctrl Pts',(18.9171520988964,21.3200664266488,5.71995962695819));
#184828=CARTESIAN_POINT('Ctrl Pts',(18.9094986848361,21.3207160877295,5.7194939883818));
#184829=CARTESIAN_POINT('Ctrl Pts',(18.9059387726566,21.3210091985323,5.71927796336941));
#184830=CARTESIAN_POINT('Ctrl Pts',(18.8978100015833,21.3216577845141,5.71878595431076));
#184831=CARTESIAN_POINT('Ctrl Pts',(18.8932407284774,21.3220074351477,5.71851029985663));
#184832=CARTESIAN_POINT('Ctrl Pts',(18.8791899587085,21.3230367504431,5.71766534360018));
#184833=CARTESIAN_POINT('Ctrl Pts',(18.8697048403569,21.323667404789,5.71709872014334));
#184834=CARTESIAN_POINT('Ctrl Pts',(18.7843133952374,21.3287675174094,5.71202896160059));
#184835=CARTESIAN_POINT('Ctrl Pts',(18.7082130956363,21.3292087594809,5.70773301599004));
#184836=CARTESIAN_POINT('Ctrl Pts',(18.5898217065979,21.3235116889203,5.7011734030744));
#184837=CARTESIAN_POINT('Ctrl Pts',(18.5474670245872,21.3201938382711,5.69885162815144));
#184838=CARTESIAN_POINT('Ctrl Pts',(18.3965610211972,21.3037910967691,5.69058743402106));
#184839=CARTESIAN_POINT('Ctrl Pts',(18.2889614934931,21.2835779791375,5.68470085103502));
#184840=CARTESIAN_POINT('Ctrl Pts',(18.130230761718,21.2408238184274,5.67556001884216));
#184841=CARTESIAN_POINT('Ctrl Pts',(18.0776354941847,21.2244316522273,5.67245451086984));
#184842=CARTESIAN_POINT('Ctrl Pts',(17.993426801835,21.1945362864908,5.66731352801543));
#184843=CARTESIAN_POINT('Ctrl Pts',(17.9613969313275,21.1822810970606,5.66531738000108));
#184844=CARTESIAN_POINT('Ctrl Pts',(17.9196834756504,21.1651479956976,5.66265783498603));
#184845=CARTESIAN_POINT('Ctrl Pts',(17.9097185978435,21.1609656290359,5.66201794143761));
#184846=CARTESIAN_POINT('Ctrl Pts',(17.8934466836655,21.1539891150937,5.66096537286275));
#184847=CARTESIAN_POINT('Ctrl Pts',(17.8871204308637,21.1512400811811,5.66055423832578));
#184848=CARTESIAN_POINT('Ctrl Pts',(17.8748983878731,21.1458579051056,5.65975618393457));
#184849=CARTESIAN_POINT('Ctrl Pts',(17.8690009810089,21.1432286067182,5.65936939927833));
#184850=CARTESIAN_POINT('Ctrl Pts',(17.8554086028623,21.1370938858025,5.65847394540759));
#184851=CARTESIAN_POINT('Ctrl Pts',(17.8477224594032,21.133569275174,5.65796461971706));
#184852=CARTESIAN_POINT('Ctrl Pts',(17.8271010186974,21.1239630273187,5.65659002170384));
#184853=CARTESIAN_POINT('Ctrl Pts',(17.8142060312325,21.1177963565797,5.6557218193945));
#184854=CARTESIAN_POINT('Ctrl Pts',(17.6962263657607,21.0599006259921,5.64769730628469));
#184855=CARTESIAN_POINT('Ctrl Pts',(17.5955588308435,20.9996731073894,5.64023770815659));
#184856=CARTESIAN_POINT('Ctrl Pts',(17.3674344252407,20.8361021302941,5.62190024360743));
#184857=CARTESIAN_POINT('Ctrl Pts',(17.2459727671715,20.7256727598796,5.61087998248642));
#184858=CARTESIAN_POINT('Ctrl Pts',(17.1177578696254,20.578640553775,5.59849615577485));
#184859=CARTESIAN_POINT('Ctrl Pts',(17.0976054600739,20.554462862586,5.59652524617231));
#184860=CARTESIAN_POINT('Ctrl Pts',(17.073533384635,20.5242368367764,5.59414951220226));
#184861=CARTESIAN_POINT('Ctrl Pts',(17.069096744174,20.5186075566984,5.59371071827025));
#184862=CARTESIAN_POINT('Ctrl Pts',(17.0621710466282,20.509727727231,5.59302442527478));
#184863=CARTESIAN_POINT('Ctrl Pts',(17.0596627311824,20.5064923657495,5.59277559001715));
#184864=CARTESIAN_POINT('Ctrl Pts',(17.0549819932017,20.5004185931482,5.59231075336545));
#184865=CARTESIAN_POINT('Ctrl Pts',(17.0528073988883,20.4975819887177,5.59209460245688));
#184866=CARTESIAN_POINT('Ctrl Pts',(17.04784704518,20.4910775077477,5.59160108525473));
#184867=CARTESIAN_POINT('Ctrl Pts',(17.0450660695357,20.4874060452441,5.59132405634155));
#184868=CARTESIAN_POINT('Ctrl Pts',(17.0378180163142,20.4777719545303,5.59060104906631));
#184869=CARTESIAN_POINT('Ctrl Pts',(17.0333703493831,20.4717947103745,5.59015639466206));
#184870=CARTESIAN_POINT('Ctrl Pts',(17.0039154534772,20.431770655083,5.58720407347442));
#184871=CARTESIAN_POINT('Ctrl Pts',(16.9798987171932,20.3970028494053,5.58476001380223));
#184872=CARTESIAN_POINT('Ctrl Pts',(16.9164818751446,20.2990523040206,5.578131728505));
#184873=CARTESIAN_POINT('Ctrl Pts',(16.8793478434617,20.2344729185197,5.57404407031446));
#184874=CARTESIAN_POINT('Ctrl Pts',(16.8077027734305,20.0931161146977,5.56540886713027));
#184875=CARTESIAN_POINT('Ctrl Pts',(16.7742226496541,20.015993096988,5.5608776586747));
#184876=CARTESIAN_POINT('Ctrl Pts',(16.7454193397875,19.9371101554369,5.55626850699162));
#184877=CARTESIAN_POINT('',(16.6170004656572,19.212404133962,6.08905627902251));
#184878=CARTESIAN_POINT('Ctrl Pts',(16.7454193775548,19.9371102588694,5.3354009189409));
#184879=CARTESIAN_POINT('Ctrl Pts',(16.7544339441791,19.961798234683,5.33706788906197));
#184880=CARTESIAN_POINT('Ctrl Pts',(16.7639100391653,19.9863232181294,5.3387164058795));
#184881=CARTESIAN_POINT('Ctrl Pts',(16.777502883358,20.0196419980515,5.34093968445625));
#184882=CARTESIAN_POINT('Ctrl Pts',(16.7812238464107,20.0285867847519,5.34153491310857));
#184883=CARTESIAN_POINT('Ctrl Pts',(16.7868091135218,20.0417574724739,5.34240859485602));
#184884=CARTESIAN_POINT('Ctrl Pts',(16.7886259932689,20.0460031744388,5.34268980911402));
#184885=CARTESIAN_POINT('Ctrl Pts',(16.7918742109988,20.0535254915758,5.34318724929614));
#184886=CARTESIAN_POINT('Ctrl Pts',(16.7932999700288,20.0568044564834,5.34340380962984));
#184887=CARTESIAN_POINT('Ctrl Pts',(16.7963728336328,20.0638227594099,5.34386674048004));
#184888=CARTESIAN_POINT('Ctrl Pts',(16.7980224537958,20.0675609354005,5.34411295448142));
#184889=CARTESIAN_POINT('Ctrl Pts',(16.8025810914609,20.0778107421036,5.34478713350902));
#184890=CARTESIAN_POINT('Ctrl Pts',(16.8055122380113,20.0843125546128,5.34521376469351));
#184891=CARTESIAN_POINT('Ctrl Pts',(16.8213484052609,20.1189714913306,5.34748314907788));
#184892=CARTESIAN_POINT('Ctrl Pts',(16.834838068308,20.1468592507548,5.34929205620498));
#184893=CARTESIAN_POINT('Ctrl Pts',(16.923351945796,20.3200448294343,5.36047870403886));
#184894=CARTESIAN_POINT('Ctrl Pts',(17.0143947027808,20.4565507925658,5.36912122011465));
#184895=CARTESIAN_POINT('Ctrl Pts',(17.1964660742112,20.6709803088658,5.38451635931984));
#184896=CARTESIAN_POINT('Ctrl Pts',(17.2800215755344,20.754209145727,5.3910866106989));
#184897=CARTESIAN_POINT('Ctrl Pts',(17.3809923330283,20.8392701814967,5.39882093310458));
#184898=CARTESIAN_POINT('Ctrl Pts',(17.3920227743076,20.8483730917581,5.39966311054418));
#184899=CARTESIAN_POINT('Ctrl Pts',(17.4097221163544,20.8626805458267,5.40101056154017));
#184900=CARTESIAN_POINT('Ctrl Pts',(17.4163315624945,20.8679581842069,5.40151288786934));
#184901=CARTESIAN_POINT('Ctrl Pts',(17.4280424976804,20.8771949765441,5.40240152827851));
#184902=CARTESIAN_POINT('Ctrl Pts',(17.4331308360002,20.8811706842279,5.40278717523398));
#184903=CARTESIAN_POINT('Ctrl Pts',(17.4436912486585,20.8893443902878,5.40358664064369));
#184904=CARTESIAN_POINT('Ctrl Pts',(17.4491658013981,20.893539047556,5.40400058488819));
#184905=CARTESIAN_POINT('Ctrl Pts',(17.463267746161,20.9042351398811,5.40506564150212));
#184906=CARTESIAN_POINT('Ctrl Pts',(17.4719245040262,20.9106973658753,5.40571828086096));
#184907=CARTESIAN_POINT('Ctrl Pts',(17.5082358078944,20.9373732223715,5.40845127515022));
#184908=CARTESIAN_POINT('Ctrl Pts',(17.5363281845071,20.9569794857325,5.41055489606549));
#184909=CARTESIAN_POINT('Ctrl Pts',(17.6107287427854,21.006264570175,5.41610185071595));
#184910=CARTESIAN_POINT('Ctrl Pts',(17.657737404476,21.0348342039408,5.41958344038907));
#184911=CARTESIAN_POINT('Ctrl Pts',(17.8013463601432,21.1146263085033,5.4301424167401));
#184912=CARTESIAN_POINT('Ctrl Pts',(17.9008522408567,21.1602299190793,5.43736822902282));
#184913=CARTESIAN_POINT('Ctrl Pts',(18.0393905751237,21.2111687889858,5.44711889627765));
#184914=CARTESIAN_POINT('Ctrl Pts',(18.0757096759983,21.223414317916,5.44964642969172));
#184915=CARTESIAN_POINT('Ctrl Pts',(18.1433562209983,21.2441949242656,5.4542826852589));
#184916=CARTESIAN_POINT('Ctrl Pts',(18.1745867685859,21.2530084851222,5.45639558446573));
#184917=CARTESIAN_POINT('Ctrl Pts',(18.2118473304785,21.2626047237027,5.45887544351266));
#184918=CARTESIAN_POINT('Ctrl Pts',(18.2176925584192,21.264083529621,5.45926328100635));
#184919=CARTESIAN_POINT('Ctrl Pts',(18.2659623431375,21.2760763014428,5.4624558313449));
#184920=CARTESIAN_POINT('Ctrl Pts',(18.3087003187832,21.2852999220158,5.46521773804927));
#184921=CARTESIAN_POINT('Ctrl Pts',(18.3590979538321,21.2945532355313,5.46837575808301));
#184922=CARTESIAN_POINT('Ctrl Pts',(18.3665068094078,21.2958727510926,5.46883752280738));
#184923=CARTESIAN_POINT('Ctrl Pts',(18.378483504828,21.297939971009,5.46957979256732));
#184924=CARTESIAN_POINT('Ctrl Pts',(18.3830469602571,21.2987122372992,5.46986163757989));
#184925=CARTESIAN_POINT('Ctrl Pts',(18.3911413482667,21.3000547472274,5.47035977569178));
#184926=CARTESIAN_POINT('Ctrl Pts',(18.3946712274194,21.3006310145012,5.47057640669311));
#184927=CARTESIAN_POINT('Ctrl Pts',(18.4022305204748,21.3018454402684,5.47103902740408));
#184928=CARTESIAN_POINT('Ctrl Pts',(18.406260312497,21.3024808965223,5.47128486300602));
#184929=CARTESIAN_POINT('Ctrl Pts',(18.417311301048,21.3041907984623,5.47195693892841));
#184930=CARTESIAN_POINT('Ctrl Pts',(18.4243361816774,21.3052415748165,5.47238185924092));
#184931=CARTESIAN_POINT('Ctrl Pts',(18.4616276349388,21.3106278588738,5.47462595942983));
#184932=CARTESIAN_POINT('Ctrl Pts',(18.4919818765301,21.3143428866531,5.47641218036499));
#184933=CARTESIAN_POINT('Ctrl Pts',(18.5837084845961,21.3235570210265,5.48171692871855));
#184934=CARTESIAN_POINT('Ctrl Pts',(18.6452535225245,21.3270363587743,5.48515173512579));
#184935=CARTESIAN_POINT('Ctrl Pts',(18.8536821800759,21.3297079786138,5.4966153542393));
#184936=CARTESIAN_POINT('Ctrl Pts',(19.0002920681909,21.3163115321248,5.50442430786287));
#184937=CARTESIAN_POINT('Ctrl Pts',(19.2182167426875,21.2732546711824,5.51682320696274));
#184938=CARTESIAN_POINT('Ctrl Pts',(19.2912573007736,21.2547276470172,5.52111291021559));
#184939=CARTESIAN_POINT('Ctrl Pts',(19.3756992513807,21.22844486701,5.52630186679595));
#184940=CARTESIAN_POINT('Ctrl Pts',(19.3882109231852,21.2244224040183,5.52707667602534));
#184941=CARTESIAN_POINT('Ctrl Pts',(19.4084717195492,21.2176998337835,5.52834142768108));
#184942=CARTESIAN_POINT('Ctrl Pts',(19.4162441413564,21.2150706704276,5.52882903187015));
#184943=CARTESIAN_POINT('Ctrl Pts',(19.4300522611925,21.2103101859927,5.52969968542841));
#184944=CARTESIAN_POINT('Ctrl Pts',(19.4360939776225,21.2081965389819,5.53008214501264));
#184945=CARTESIAN_POINT('Ctrl Pts',(19.4487990135421,21.2036870074794,5.53088963247527));
#184946=CARTESIAN_POINT('Ctrl Pts',(19.4554600727451,21.201285030109,5.53131485938503));
#184947=CARTESIAN_POINT('Ctrl Pts',(19.4730348307368,21.1948477538988,5.53244181401085));
#184948=CARTESIAN_POINT('Ctrl Pts',(19.4839274124168,21.1907558585156,5.53314542521417));
#184949=CARTESIAN_POINT('Ctrl Pts',(19.5342445656523,21.1713789310356,5.53641997972027));
#184950=CARTESIAN_POINT('Ctrl Pts',(19.5732370464033,21.1550055800021,5.53902727968113));
#184951=CARTESIAN_POINT('Ctrl Pts',(19.67913488542,21.1067580669465,5.54630760249952));
#184952=CARTESIAN_POINT('Ctrl Pts',(19.7448932123074,21.072524016115,5.55105562465965));
#184953=CARTESIAN_POINT('Ctrl Pts',(19.9390830510809,20.9581004435283,5.56573480162282));
#184954=CARTESIAN_POINT('Ctrl Pts',(20.0608313137524,20.8675330209865,5.5758983571092));
#184955=CARTESIAN_POINT('Ctrl Pts',(20.1775357144198,20.7595325185273,5.58614714506126));
#184956=CARTESIAN_POINT('Ctrl Pts',(20.1831599882141,20.7542704399681,5.58664232532725));
#184957=CARTESIAN_POINT('Ctrl Pts',(20.2194393197498,20.7199542367006,5.58984406147554));
#184958=CARTESIAN_POINT('Ctrl Pts',(20.2492501853195,20.6900166628813,5.59251041666071));
#184959=CARTESIAN_POINT('Ctrl Pts',(20.2832437881245,20.6537710093413,5.59557253997606));
#184960=CARTESIAN_POINT('Ctrl Pts',(20.2883114837023,20.6483100973081,5.5960296214916));
#184961=CARTESIAN_POINT('Ctrl Pts',(20.2964653202647,20.6394300244387,5.59676584392753));
#184962=CARTESIAN_POINT('Ctrl Pts',(20.2995692646553,20.6360273998208,5.59704629050407));
#184963=CARTESIAN_POINT('Ctrl Pts',(20.3050622913947,20.629966191165,5.59754288331927));
#184964=CARTESIAN_POINT('Ctrl Pts',(20.3074557664947,20.627311662971,5.5977593597154));
#184965=CARTESIAN_POINT('Ctrl Pts',(20.3125762639162,20.6216036787313,5.59822267757644));
#184966=CARTESIAN_POINT('Ctrl Pts',(20.3153011478019,20.6185483792976,5.59846935956072));
#184967=CARTESIAN_POINT('Ctrl Pts',(20.3227724308758,20.6101220597984,5.59914614156427));
#184968=CARTESIAN_POINT('Ctrl Pts',(20.3275004929135,20.6047347515774,5.59957489053217));
#184969=CARTESIAN_POINT('Ctrl Pts',(20.352841915982,20.5755623765655,5.60187605075979));
#184970=CARTESIAN_POINT('Ctrl Pts',(20.3729514447264,20.5513425043393,5.60371348328004));
#184971=CARTESIAN_POINT('Ctrl Pts',(20.4941830292005,20.3985210911496,5.61492681533108));
#184972=CARTESIAN_POINT('Ctrl Pts',(20.5806646642349,20.2589945132311,5.62357181833333));
#184973=CARTESIAN_POINT('Ctrl Pts',(20.7000036850133,20.0048738229282,5.63893985945491));
#184974=CARTESIAN_POINT('Ctrl Pts',(20.740899144624,19.8949273872549,5.64547722215058));
#184975=CARTESIAN_POINT('Ctrl Pts',(20.7763488702799,19.7684086490178,5.65317452707047));
#184976=CARTESIAN_POINT('Ctrl Pts',(20.7800657826988,19.7546065745385,5.65401625584826));
#184977=CARTESIAN_POINT('Ctrl Pts',(20.7857585983334,19.7325813981316,5.65536312304965));
#184978=CARTESIAN_POINT('Ctrl Pts',(20.7878255276099,19.7243821185877,5.65586531828621));
#184979=CARTESIAN_POINT('Ctrl Pts',(20.7913840660744,19.7099002882774,5.65675380597149));
#184980=CARTESIAN_POINT('Ctrl Pts',(20.7928961655522,19.7036228486671,5.65713943203073));
#184981=CARTESIAN_POINT('Ctrl Pts',(20.7959641268665,19.6906253936564,5.65793893186394));
#184982=CARTESIAN_POINT('Ctrl Pts',(20.797515909362,19.6839045028146,5.65835293181163));
#184983=CARTESIAN_POINT('Ctrl Pts',(20.801414550597,19.6666345742438,5.65941829544049));
#184984=CARTESIAN_POINT('Ctrl Pts',(20.8037135071726,19.6560750281829,5.66007118781147));
#184985=CARTESIAN_POINT('Ctrl Pts',(20.8129693057928,19.6119382111154,5.66280663231842));
#184986=CARTESIAN_POINT('Ctrl Pts',(20.8191903550209,19.5782135494089,5.66491250265455));
#184987=CARTESIAN_POINT('Ctrl Pts',(20.8332613485152,19.4899690549339,5.67046680233092));
#184988=CARTESIAN_POINT('Ctrl Pts',(20.8398071948404,19.4352703315242,5.67395361405182));
#184989=CARTESIAN_POINT('Ctrl Pts',(20.8529635413892,19.2713646702355,5.68452262388142));
#184990=CARTESIAN_POINT('Ctrl Pts',(20.8532522858017,19.1618404059941,5.69175321458659));
#184991=CARTESIAN_POINT('Ctrl Pts',(20.8362256226136,18.9346389345337,5.70680369492273));
#184992=CARTESIAN_POINT('Ctrl Pts',(20.8174659751763,18.8174214523578,5.71459553302059));
#184993=CARTESIAN_POINT('Ctrl Pts',(20.7867042156931,18.6931340863944,5.72250388821097));
#184994=CARTESIAN_POINT('Ctrl Pts',(20.7843536763835,18.6839046470247,5.7230889294212));
#184995=CARTESIAN_POINT('Ctrl Pts',(20.7807790666248,18.6702546951491,5.72395055742379));
#184996=CARTESIAN_POINT('Ctrl Pts',(20.7796028246828,18.6658219402288,5.72422979880039));
#184997=CARTESIAN_POINT('Ctrl Pts',(20.7774847484513,18.6579431817837,5.7247250660459));
#184998=CARTESIAN_POINT('Ctrl Pts',(20.7765485891865,18.6544957117868,5.72494141539265));
#184999=CARTESIAN_POINT('Ctrl Pts',(20.7745175056721,18.6470902797724,5.72540536258519));
#185000=CARTESIAN_POINT('Ctrl Pts',(20.7734197935278,18.6431331406509,5.72565279621374));
#185001=CARTESIAN_POINT('Ctrl Pts',(20.7703589450192,18.6322224503572,5.72633376374208));
#185002=CARTESIAN_POINT('Ctrl Pts',(20.768371692712,18.62527564141,5.72676591871478));
#185003=CARTESIAN_POINT('Ctrl Pts',(20.7573066343994,18.5873314203549,5.7291193285026));
#185004=CARTESIAN_POINT('Ctrl Pts',(20.7475553830188,18.5565328807234,5.73100369901553));
#185005=CARTESIAN_POINT('Ctrl Pts',(20.6843962882601,18.3718494027736,5.74221343752147));
#185006=CARTESIAN_POINT('Ctrl Pts',(20.614074331491,18.22431269161,5.75082235854827));
#185007=CARTESIAN_POINT('Ctrl Pts',(20.4654124816059,17.9872492355572,5.76614076296446));
#185008=CARTESIAN_POINT('Ctrl Pts',(20.3952170693221,17.893537402391,5.77266665988033));
#185009=CARTESIAN_POINT('Ctrl Pts',(20.3081689198856,17.7954133933833,5.78035105834047));
#185010=CARTESIAN_POINT('Ctrl Pts',(20.2985772955844,17.7848194011992,5.7811926230152));
#185011=CARTESIAN_POINT('Ctrl Pts',(20.283141441435,17.7681135591141,5.78253927668147));
#185012=CARTESIAN_POINT('Ctrl Pts',(20.2773664779897,17.7619380971408,5.78304142396317));
#185013=CARTESIAN_POINT('Ctrl Pts',(20.2671163535548,17.7511079020324,5.78392985578684));
#185014=CARTESIAN_POINT('Ctrl Pts',(20.2626565749767,17.7464387122417,5.78431547420809));
#185015=CARTESIAN_POINT('Ctrl Pts',(20.2533882466162,17.736823640348,5.78511498666415));
#185016=CARTESIAN_POINT('Ctrl Pts',(20.2485767494453,17.7318807175891,5.78552900701293));
#185017=CARTESIAN_POINT('Ctrl Pts',(20.2361644093598,17.7192534031328,5.78659448307867));
#185018=CARTESIAN_POINT('Ctrl Pts',(20.2285287879964,17.7116036157582,5.7872474681084));
#185019=CARTESIAN_POINT('Ctrl Pts',(20.1964160945631,17.6799203501212,5.78998381047682));
#185020=CARTESIAN_POINT('Ctrl Pts',(20.1714163933101,17.6564262243667,5.79209050516523));
#185021=CARTESIAN_POINT('Ctrl Pts',(20.1048001871039,17.5968029857849,5.79764749742325));
#185022=CARTESIAN_POINT('Ctrl Pts',(20.0623263445061,17.5616748484905,5.80113622378542));
#185023=CARTESIAN_POINT('Ctrl Pts',(19.9315800736052,17.4618694595021,5.81170891158752));
#185024=CARTESIAN_POINT('Ctrl Pts',(19.839618516701,17.4023375356375,5.81894125339262));
#185025=CARTESIAN_POINT('Ctrl Pts',(19.6394028114315,17.2937222205111,5.83398776902141));
#185026=CARTESIAN_POINT('Ctrl Pts',(19.5307617774594,17.2460863805988,5.84177389430751));
#185027=CARTESIAN_POINT('Ctrl Pts',(19.4096763066952,17.2046995755835,5.84967776725404));
#185028=CARTESIAN_POINT('Ctrl Pts',(19.4006354397178,17.2016774617389,5.85026333987533));
#185029=CARTESIAN_POINT('Ctrl Pts',(19.3872134359228,17.1972914176112,5.85112559716426));
#185030=CARTESIAN_POINT('Ctrl Pts',(19.382847927206,17.1958805454932,5.85140494192802));
#185031=CARTESIAN_POINT('Ctrl Pts',(19.3750749252734,17.1933962969234,5.85190032265486));
#185032=CARTESIAN_POINT('Ctrl Pts',(19.3716692737196,17.1923173452727,5.85211668266914));
#185033=CARTESIAN_POINT('Ctrl Pts',(19.364343997581,17.1900169968107,5.85258057481106));
#185034=CARTESIAN_POINT('Ctrl Pts',(19.360423558012,17.1887983826798,5.85282794313175));
#185035=CARTESIAN_POINT('Ctrl Pts',(19.3495984784688,17.1854680585505,5.85350854675179));
#185036=CARTESIAN_POINT('Ctrl Pts',(19.3426864672293,17.1833802327474,5.85394040555768));
#185037=CARTESIAN_POINT('Ctrl Pts',(19.3048667245644,17.1721673129081,5.85628921467593));
#185038=CARTESIAN_POINT('Ctrl Pts',(19.2737625921487,17.1637129799851,5.8581694506292));
#185039=CARTESIAN_POINT('Ctrl Pts',(19.0843022717943,17.1168348102409,5.86937946215354));
#185040=CARTESIAN_POINT('Ctrl Pts',(18.922122912842,17.0960859944393,5.87799152997459));
#185041=CARTESIAN_POINT('Ctrl Pts',(18.6422407799329,17.0927601708337,5.89331429747746));
#185042=CARTESIAN_POINT('Ctrl Pts',(18.5254286145577,17.1010586652293,5.89984123212194));
#185043=CARTESIAN_POINT('Ctrl Pts',(18.3957845772126,17.1211426928271,5.90752679872677));
#185044=CARTESIAN_POINT('Ctrl Pts',(18.3816846858559,17.1234734394357,5.90836837841499));
#185045=CARTESIAN_POINT('Ctrl Pts',(18.3592822518201,17.1274100457792,5.90971505161746));
#185046=CARTESIAN_POINT('Ctrl Pts',(18.3509637133369,17.128923227144,5.91021720328667));
#185047=CARTESIAN_POINT('Ctrl Pts',(18.336308949015,17.1316797939301,5.911105640221));
#185048=CARTESIAN_POINT('Ctrl Pts',(18.3299688934815,17.1329024192921,5.91149125934095));
#185049=CARTESIAN_POINT('Ctrl Pts',(18.3168673866617,17.1354911549738,5.91229077064141));
#185050=CARTESIAN_POINT('Ctrl Pts',(18.3101068282682,17.1368613450159,5.9127047891231));
#185051=CARTESIAN_POINT('Ctrl Pts',(18.2927708556483,17.1404631949202,5.91377025489896));
#185052=CARTESIAN_POINT('Ctrl Pts',(18.2822057128759,17.142742826834,5.91442323144883));
#185053=CARTESIAN_POINT('Ctrl Pts',(18.2381844175133,17.1525946576822,5.91715949163572));
#185054=CARTESIAN_POINT('Ctrl Pts',(18.2048988724773,17.1608981913747,5.91926611086932));
#185055=CARTESIAN_POINT('Ctrl Pts',(18.1187107604473,17.184637739353,5.92482285665088));
#185056=CARTESIAN_POINT('Ctrl Pts',(18.0661857487322,17.2013363055365,5.92831140774156));
#185057=CARTESIAN_POINT('Ctrl Pts',(17.818462093011,17.2908761186209,5.94524253761476));
#185058=CARTESIAN_POINT('Ctrl Pts',(17.6341001254976,17.3902054662756,5.95943301121613));
#185059=CARTESIAN_POINT('Ctrl Pts',(17.4635919657424,17.517549995586,5.97284947871786));
#185060=CARTESIAN_POINT('Ctrl Pts',(17.4599738058426,17.5202703503359,5.9731342582316));
#185061=CARTESIAN_POINT('Ctrl Pts',(17.4399959625427,17.5353914637245,5.97470702341874));
#185062=CARTESIAN_POINT('Ctrl Pts',(17.423807913869,17.548018585342,5.97598271335687));
#185063=CARTESIAN_POINT('Ctrl Pts',(17.4027810304423,17.5649178010054,5.97763860875498));
#185064=CARTESIAN_POINT('Ctrl Pts',(17.3977750243699,17.5689788771942,5.97803275318776));
#185065=CARTESIAN_POINT('Ctrl Pts',(17.389744211289,17.5755548475165,5.97866480676073));
#185066=CARTESIAN_POINT('Ctrl Pts',(17.3867077738271,17.5780553805645,5.9789037278657));
#185067=CARTESIAN_POINT('Ctrl Pts',(17.3810359176436,17.5827527942161,5.97934987943894));
#185068=CARTESIAN_POINT('Ctrl Pts',(17.3783988696818,17.5849476186522,5.97955725237127));
#185069=CARTESIAN_POINT('Ctrl Pts',(17.3721624883266,17.5901638960603,5.98004755583311));
#185070=CARTESIAN_POINT('Ctrl Pts',(17.3685678356643,17.5931909600925,5.98033007749987));
#185071=CARTESIAN_POINT('Ctrl Pts',(17.3573349172615,17.6027143308701,5.98121275565799));
#185072=CARTESIAN_POINT('Ctrl Pts',(17.3497325782802,17.6092530606816,5.98180989252141));
#185073=CARTESIAN_POINT('Ctrl Pts',(17.3319067386628,17.624806676322,5.98321024261232));
#185074=CARTESIAN_POINT('Ctrl Pts',(17.3217231600871,17.6338668663948,5.98401038981313));
#185075=CARTESIAN_POINT('Ctrl Pts',(17.2863073361184,17.6659939691311,5.98679657916471));
#185076=CARTESIAN_POINT('Ctrl Pts',(17.2615458444858,17.6895741242838,5.98875091696551));
#185077=CARTESIAN_POINT('Ctrl Pts',(17.1836732667198,17.7674144459385,5.99496003022765));
#185078=CARTESIAN_POINT('Ctrl Pts',(17.1329039396452,17.823936557484,5.99910803434806));
#185079=CARTESIAN_POINT('Ctrl Pts',(16.977365641622,18.0170482054406,6.01259282767885));
#185080=CARTESIAN_POINT('Ctrl Pts',(16.886198618141,18.1636660640111,6.02185804178627));
#185081=CARTESIAN_POINT('Ctrl Pts',(16.8039951984994,18.3407643153645,6.03320082330143));
#185082=CARTESIAN_POINT('Ctrl Pts',(16.7945621927219,18.361994929621,6.03456160905432));
#185083=CARTESIAN_POINT('Ctrl Pts',(16.7817332891331,18.3921986961956,6.03650075907808));
#185084=CARTESIAN_POINT('Ctrl Pts',(16.7780458554875,18.401046751076,6.03706920654468));
#185085=CARTESIAN_POINT('Ctrl Pts',(16.7721580869819,18.4154492489627,6.03799524114108));
#185086=CARTESIAN_POINT('Ctrl Pts',(16.7699209238234,18.4209885630262,6.03835157757218));
#185087=CARTESIAN_POINT('Ctrl Pts',(16.7652917997284,18.4325916797842,6.03909839166055));
#185088=CARTESIAN_POINT('Ctrl Pts',(16.7629043426113,18.4386572012724,6.03948901651778));
#185089=CARTESIAN_POINT('Ctrl Pts',(16.7572996268585,18.4530916780653,6.04041919582516));
#185090=CARTESIAN_POINT('Ctrl Pts',(16.7541074665818,18.4614701861268,6.04095958597292));
#185091=CARTESIAN_POINT('Ctrl Pts',(16.7435701496538,18.4896646874311,6.04277975918914));
#185092=CARTESIAN_POINT('Ctrl Pts',(16.73646869792,18.509569840471,6.04406762519122));
#185093=CARTESIAN_POINT('Ctrl Pts',(16.6996529283538,18.6178595830961,6.05109143770911));
#185094=CARTESIAN_POINT('Ctrl Pts',(16.6755085002152,18.7080165786977,6.05700832119098));
#185095=CARTESIAN_POINT('Ctrl Pts',(16.6304385570914,18.9354384303446,6.0720588793899));
#185096=CARTESIAN_POINT('Ctrl Pts',(16.6169140925405,19.0737188024872,6.08133516956679));
#185097=CARTESIAN_POINT('Ctrl Pts',(16.6170004105532,19.2123184392235,6.09037076723679));
#185098=CARTESIAN_POINT('Ctrl Pts',(16.7454193623258,19.9371102171621,6.13370787675019));
#185099=CARTESIAN_POINT('Ctrl Pts',(16.7204253462621,19.868659704792,6.12932687783769));
#185100=CARTESIAN_POINT('Ctrl Pts',(16.6989958950762,19.7989890746744,6.12494587892519));
#185101=CARTESIAN_POINT('Ctrl Pts',(16.6812266631735,19.7285042295617,6.12056488001268));
#185102=CARTESIAN_POINT('Ctrl Pts',(16.6634283576886,19.6579040588712,6.11617671301702));
#185103=CARTESIAN_POINT('Ctrl Pts',(16.6493023095371,19.5864874879226,6.11178854602136));
#185104=CARTESIAN_POINT('Ctrl Pts',(16.6388927491981,19.514668581907,6.1074003790257));
#185105=CARTESIAN_POINT('Ctrl Pts',(16.6365508783606,19.4985112615104,6.10641315958675));
#185106=CARTESIAN_POINT('Ctrl Pts',(16.6343969009588,19.4823335858048,6.1054259401478));
#185107=CARTESIAN_POINT('Ctrl Pts',(16.6324309574259,19.4661402737595,6.10443872070886));
#185108=CARTESIAN_POINT('Ctrl Pts',(16.6222201199426,19.3820344615431,6.09931124014674));
#185109=CARTESIAN_POINT('Ctrl Pts',(16.6170567766291,19.2973036553198,6.09418375958462));
#185110=CARTESIAN_POINT('Ctrl Pts',(16.6170004656572,19.212404133962,6.08905627902251));
#185111=CARTESIAN_POINT('Origin',(18.734,19.211,0.));
#185112=CARTESIAN_POINT('',(16.7454193167441,19.9371100923286,7.15616136059514));
#185113=CARTESIAN_POINT('',(16.7486737101886,19.9359290495398,6.93361858560548));
#185114=CARTESIAN_POINT('',(16.7454193623258,19.9371102171621,0.));
#185115=CARTESIAN_POINT('Ctrl Pts',(16.7454193167441,19.9371100923285,7.15616136059514));
#185116=CARTESIAN_POINT('Ctrl Pts',(16.72058404148,19.8690943063269,7.15141135633731));
#185117=CARTESIAN_POINT('Ctrl Pts',(16.6992295000541,19.7997804030581,7.14660724357929));
#185118=CARTESIAN_POINT('Ctrl Pts',(16.6631797956417,19.6570555067128,7.13689818809369));
#185119=CARTESIAN_POINT('Ctrl Pts',(16.6487382401048,19.5837556281975,7.13200641828163));
#185120=CARTESIAN_POINT('Ctrl Pts',(16.6333272127491,19.47567679551,7.12505655919908));
#185121=CARTESIAN_POINT('Ctrl Pts',(16.6292914383807,19.4413956454038,7.12289060683243));
#185122=CARTESIAN_POINT('Ctrl Pts',(16.6254128246439,19.3996888120896,7.12031414819974));
#185123=CARTESIAN_POINT('Ctrl Pts',(16.6247685443226,19.3923450135598,7.11986268382579));
#185124=CARTESIAN_POINT('Ctrl Pts',(16.6238224665814,19.3808732058643,7.11916104264327));
#185125=CARTESIAN_POINT('Ctrl Pts',(16.6234943985934,19.3767475059353,7.11890943103365));
#185126=CARTESIAN_POINT('Ctrl Pts',(16.6229060239836,19.3690631386444,7.11844217309981));
#185127=CARTESIAN_POINT('Ctrl Pts',(16.6226426179176,19.3655048114267,7.11822636057523));
#185128=CARTESIAN_POINT('Ctrl Pts',(16.6220645668203,19.3574183333609,7.11773716432519));
#185129=CARTESIAN_POINT('Ctrl Pts',(16.6217554882611,19.3528898367541,7.11746409552394));
#185130=CARTESIAN_POINT('Ctrl Pts',(16.6209918950657,19.341146123027,7.11675816258681));
#185131=CARTESIAN_POINT('Ctrl Pts',(16.6205597664386,19.3339294407798,7.11632652246368));
#185132=CARTESIAN_POINT('Ctrl Pts',(16.6180743367168,19.2885248652664,7.11362363845074));
#185133=CARTESIAN_POINT('Ctrl Pts',(16.6170190194794,19.2502868211829,7.11140439779203));
#185134=CARTESIAN_POINT('Ctrl Pts',(16.6169207094246,19.0499008549758,7.09997624691515));
#185135=CARTESIAN_POINT('Ctrl Pts',(16.6354677186578,18.8882767757765,7.0914146059987));
#185136=CARTESIAN_POINT('Ctrl Pts',(16.697373120192,18.6227424401113,7.07645433449783));
#185137=CARTESIAN_POINT('Ctrl Pts',(16.7308397008735,18.5172852405246,7.07026706865739));
#185138=CARTESIAN_POINT('Ctrl Pts',(16.7777126662261,18.4017842718485,7.06296366851757));
#185139=CARTESIAN_POINT('Ctrl Pts',(16.7831788072558,18.3886941649711,7.06212822733765));
#185140=CARTESIAN_POINT('Ctrl Pts',(16.7921001450349,18.3679193848153,7.06078954377303));
#185141=CARTESIAN_POINT('Ctrl Pts',(16.7954704366286,18.360198554762,7.06028918822827));
#185142=CARTESIAN_POINT('Ctrl Pts',(16.8015031073124,18.3466005629783,7.05940284113164));
#185143=CARTESIAN_POINT('Ctrl Pts',(16.8041464536104,18.3407150380274,7.05901750566348));
#185144=CARTESIAN_POINT('Ctrl Pts',(16.8096767358687,18.3285507197677,7.05821750961661));
#185145=CARTESIAN_POINT('Ctrl Pts',(16.8125675913427,18.3222738024234,7.05780271744179));
#185146=CARTESIAN_POINT('Ctrl Pts',(16.8200827135533,18.306164277913,7.05673299011719));
#185147=CARTESIAN_POINT('Ctrl Pts',(16.824751998384,18.2963530053862,7.05607650203869));
#185148=CARTESIAN_POINT('Ctrl Pts',(16.8446948525917,18.2552665261635,7.05330600340075));
#185149=CARTESIAN_POINT('Ctrl Pts',(16.8606622769423,18.2243359423953,7.05116792072756));
#185150=CARTESIAN_POINT('Ctrl Pts',(16.9043949506372,18.1445129749468,7.04550807459811));
#185151=CARTESIAN_POINT('Ctrl Pts',(16.9333567136985,18.0963107614082,7.04194608537279));
#185152=CARTESIAN_POINT('Ctrl Pts',(17.0332356239815,17.9441467814891,7.03023621556654));
#185153=CARTESIAN_POINT('Ctrl Pts',(17.1115050815964,17.8453418741352,7.02187672784344));
#185154=CARTESIAN_POINT('Ctrl Pts',(17.2668985763519,17.6815216670981,7.00699923935122));
#185155=CARTESIAN_POINT('Ctrl Pts',(17.3407876934438,17.6139230516734,7.00047970527239));
#185156=CARTESIAN_POINT('Ctrl Pts',(17.4267853731384,17.5457754225334,6.99370036427314));
#185157=CARTESIAN_POINT('Ctrl Pts',(17.4344245188285,17.5398068480811,6.99310473240185));
#185158=CARTESIAN_POINT('Ctrl Pts',(17.445764028739,17.5310719002186,6.9922305739691));
#185159=CARTESIAN_POINT('Ctrl Pts',(17.4494327556196,17.5282649246882,6.99194928198737));
#185160=CARTESIAN_POINT('Ctrl Pts',(17.455957562755,17.523306510706,6.99145175585015));
#185161=CARTESIAN_POINT('Ctrl Pts',(17.4588099325777,17.5211502795125,6.99123518685502));
#185162=CARTESIAN_POINT('Ctrl Pts',(17.4649328365295,17.5165460398849,6.99077229448187));
#185163=CARTESIAN_POINT('Ctrl Pts',(17.46820498821,17.5141002748762,6.99052612732118));
#185164=CARTESIAN_POINT('Ctrl Pts',(17.4772061329195,17.5074129058347,6.98985220883767));
#185165=CARTESIAN_POINT('Ctrl Pts',(17.4829495621978,17.5031906965051,6.9894257896391));
#185166=CARTESIAN_POINT('Ctrl Pts',(17.5137221177872,17.48080718736,6.98715955739938));
#185167=CARTESIAN_POINT('Ctrl Pts',(17.5391270012329,17.4631659052984,6.98535347914509));
#185168=CARTESIAN_POINT('Ctrl Pts',(17.6171834293574,17.4114608591055,6.97996800388284));
#185169=CARTESIAN_POINT('Ctrl Pts',(17.670972582829,17.3791718881716,6.97647535634526));
#185170=CARTESIAN_POINT('Ctrl Pts',(17.8443351544451,17.2853166413613,6.96564098423607));
#185171=CARTESIAN_POINT('Ctrl Pts',(17.9683763529019,17.2327227022298,6.95847223548385));
#185172=CARTESIAN_POINT('Ctrl Pts',(18.1354765541806,17.1799600069948,6.94874719054158));
#185173=CARTESIAN_POINT('Ctrl Pts',(18.1747300614653,17.1688024927326,6.94645995771917));
#185174=CARTESIAN_POINT('Ctrl Pts',(18.2613895425818,17.1468561114473,6.9413792172179));
#185175=CARTESIAN_POINT('Ctrl Pts',(18.3088928602563,17.1365521158754,6.93857391154233));
#185176=CARTESIAN_POINT('Ctrl Pts',(18.3691073390532,17.1256460298272,6.93497489479974));
#185177=CARTESIAN_POINT('Ctrl Pts',(18.3815281470229,17.1235107383621,6.9342302503282));
#185178=CARTESIAN_POINT('Ctrl Pts',(18.4012400739608,17.1203029562274,6.93304464393182));
#185179=CARTESIAN_POINT('Ctrl Pts',(18.4085191240394,17.1191573925135,6.9326060047524));
#185180=CARTESIAN_POINT('Ctrl Pts',(18.4220931091327,17.1170937080767,6.93178642830714));
#185181=CARTESIAN_POINT('Ctrl Pts',(18.428386505449,17.1161659114605,6.93140580268591));
#185182=CARTESIAN_POINT('Ctrl Pts',(18.4423736284573,17.1141682478164,6.93055839823835));
#185183=CARTESIAN_POINT('Ctrl Pts',(18.4500692266565,17.1131123359472,6.93009118311778));
#185184=CARTESIAN_POINT('Ctrl Pts',(18.4724466641256,17.1101673135602,6.92872967234074));
#185185=CARTESIAN_POINT('Ctrl Pts',(18.4871424980571,17.1083898411278,6.92783186836276));
#185186=CARTESIAN_POINT('Ctrl Pts',(18.6040636929105,17.0954907892379,6.92065848821028));
#185187=CARTESIAN_POINT('Ctrl Pts',(18.7069423435795,17.0916781480667,6.91415209084858));
#185188=CARTESIAN_POINT('Ctrl Pts',(18.965371521894,17.1009223843318,6.89736582808211));
#185189=CARTESIAN_POINT('Ctrl Pts',(19.1199627036541,17.1236597310998,6.88689546229996));
#185190=CARTESIAN_POINT('Ctrl Pts',(19.3214692027319,17.1764660605136,6.87343959309171));
#185191=CARTESIAN_POINT('Ctrl Pts',(19.3717750386442,17.1916703067092,6.8701018920468));
#185192=CARTESIAN_POINT('Ctrl Pts',(19.429685172763,17.2115534175109,6.86632508261371));
#185193=CARTESIAN_POINT('Ctrl Pts',(19.4378858248511,17.2144256218839,6.86579181222299));
#185194=CARTESIAN_POINT('Ctrl Pts',(19.4502843412951,17.2188539759944,6.864988188491));
#185195=CARTESIAN_POINT('Ctrl Pts',(19.4544952206672,17.2203730443919,6.86471571638991));
#185196=CARTESIAN_POINT('Ctrl Pts',(19.4620494720616,17.2231253398173,6.86422777520277));
#185197=CARTESIAN_POINT('Ctrl Pts',(19.4653945612495,17.2243536563548,6.86401202029746));
#185198=CARTESIAN_POINT('Ctrl Pts',(19.4726614368855,17.2270428947367,6.86354399216831));
#185199=CARTESIAN_POINT('Ctrl Pts',(19.4765819850835,17.2285069962313,6.86329191181828));
#185200=CARTESIAN_POINT('Ctrl Pts',(19.4875952580573,17.2326570804441,6.86258491770412));
#185201=CARTESIAN_POINT('Ctrl Pts',(19.4946780103472,17.2353695971053,6.86213156190185));
#185202=CARTESIAN_POINT('Ctrl Pts',(19.5371985711972,17.2519164726156,6.85941696991385));
#185203=CARTESIAN_POINT('Ctrl Pts',(19.5722751929878,17.2666668704421,6.8572072664197));
#185204=CARTESIAN_POINT('Ctrl Pts',(19.6869985088795,17.3185926140793,6.85001915537283));
#185205=CARTESIAN_POINT('Ctrl Pts',(19.7647320449535,17.3597826245643,6.84521009801362));
#185206=CARTESIAN_POINT('Ctrl Pts',(19.98826417719,17.4966876199193,6.83095043571922));
#185207=CARTESIAN_POINT('Ctrl Pts',(20.1250238703399,17.6056678226495,6.82157748275048));
#185208=CARTESIAN_POINT('Ctrl Pts',(20.2630317362106,17.7466626675632,6.81011395802333));
#185209=CARTESIAN_POINT('Ctrl Pts',(20.2789075541949,17.7634218636427,6.8087616492396));
#185210=CARTESIAN_POINT('Ctrl Pts',(20.3009668510425,17.7874848757765,6.80683253601301));
#185211=CARTESIAN_POINT('Ctrl Pts',(20.3073800916207,17.7945765096935,6.80626550795652));
#185212=CARTESIAN_POINT('Ctrl Pts',(20.3177189800645,17.8061659070707,6.8053411571013));
#185213=CARTESIAN_POINT('Ctrl Pts',(20.3216740757082,17.8106373095968,6.80498507587772));
#185214=CARTESIAN_POINT('Ctrl Pts',(20.3299107168838,17.8200289278672,6.80423828567563));
#185215=CARTESIAN_POINT('Ctrl Pts',(20.3341885365228,17.8249523147171,6.80384742723879));
#185216=CARTESIAN_POINT('Ctrl Pts',(20.3443063993688,17.8367063402064,6.80291575077307));
#185217=CARTESIAN_POINT('Ctrl Pts',(20.3501257979505,17.8435545113228,6.80237408985919));
#185218=CARTESIAN_POINT('Ctrl Pts',(20.3695621301139,17.8667242359223,6.8005451855747));
#185219=CARTESIAN_POINT('Ctrl Pts',(20.3829764661924,17.8832133553978,6.79924975319571));
#185220=CARTESIAN_POINT('Ctrl Pts',(20.4545179737507,17.9739097947823,6.79215508146419));
#185221=CARTESIAN_POINT('Ctrl Pts',(20.5078802888537,18.0517248447993,6.78617079225643));
#185222=CARTESIAN_POINT('Ctrl Pts',(20.6403886364046,18.2756349235806,6.76927211376361));
#185223=CARTESIAN_POINT('Ctrl Pts',(20.7078124104089,18.427873873447,6.75808958983998));
#185224=CARTESIAN_POINT('Ctrl Pts',(20.7691588946154,18.6265503484748,6.74476063580065));
#185225=CARTESIAN_POINT('Ctrl Pts',(20.78035455319,18.6670453071644,6.74210947671535));
#185226=CARTESIAN_POINT('Ctrl Pts',(20.7921063400594,18.7150739865797,6.73906263416479));
#185227=CARTESIAN_POINT('Ctrl Pts',(20.7938359889531,18.7223078472805,6.73860631468141));
#185228=CARTESIAN_POINT('Ctrl Pts',(20.7965740799067,18.7340321366793,6.73787107670368));
#185229=CARTESIAN_POINT('Ctrl Pts',(20.7976060491156,18.7385169286411,6.73759085810142));
#185230=CARTESIAN_POINT('Ctrl Pts',(20.7994134524236,18.7464905350783,6.73709451644182));
#185231=CARTESIAN_POINT('Ctrl Pts',(20.8001946831632,18.7499779784092,6.73687806449015));
#185232=CARTESIAN_POINT('Ctrl Pts',(20.8018523809055,18.7574668593314,6.73641462952675));
#185233=CARTESIAN_POINT('Ctrl Pts',(20.8027260645061,18.7614688558192,6.73616780688422));
#185234=CARTESIAN_POINT('Ctrl Pts',(20.8050988503836,18.7724910698027,6.73549024221721));
#185235=CARTESIAN_POINT('Ctrl Pts',(20.8065738863647,18.77951649065,6.73506085643686));
#185236=CARTESIAN_POINT('Ctrl Pts',(20.814354203185,18.8175338226194,6.73275003662018));
#185237=CARTESIAN_POINT('Ctrl Pts',(20.8200004830739,18.8486583518741,6.73090392956567));
#185238=CARTESIAN_POINT('Ctrl Pts',(20.850512431848,19.0413457455191,6.71969134208865));
#185239=CARTESIAN_POINT('Ctrl Pts',(20.8572960915736,19.2052265383463,6.71105306525506));
#185240=CARTESIAN_POINT('Ctrl Pts',(20.8364523929681,19.4850271143387,6.69569421480608));
#185241=CARTESIAN_POINT('Ctrl Pts',(20.8180853299,19.6008460941183,6.68915892052927));
#185242=CARTESIAN_POINT('Ctrl Pts',(20.7868423677917,19.7284277810049,6.68146394380357));
#185243=CARTESIAN_POINT('Ctrl Pts',(20.7833021722063,19.7422757171445,6.68062224423412));
#185244=CARTESIAN_POINT('Ctrl Pts',(20.7774449147178,19.7642570639177,6.67927541499106));
#185245=CARTESIAN_POINT('Ctrl Pts',(20.7752188370284,19.7724144230931,6.67877322824099));
#185246=CARTESIAN_POINT('Ctrl Pts',(20.7712067843076,19.7867770494357,6.67788475038332));
#185247=CARTESIAN_POINT('Ctrl Pts',(20.7694411670793,19.7929879265233,6.67749912561736));
#185248=CARTESIAN_POINT('Ctrl Pts',(20.7657306844781,19.8058167829792,6.67669962337227));
#185249=CARTESIAN_POINT('Ctrl Pts',(20.7637818348715,19.8124335213782,6.6762856196943));
#185250=CARTESIAN_POINT('Ctrl Pts',(20.7586966832466,19.8293923803066,6.67522023573953));
#185251=CARTESIAN_POINT('Ctrl Pts',(20.7555134893519,19.839720129117,6.67456732666094));
#185252=CARTESIAN_POINT('Ctrl Pts',(20.7419000625379,19.8827159553579,6.67183172095038));
#185253=CARTESIAN_POINT('Ctrl Pts',(20.7307563882289,19.9151510461723,6.66972570268485));
#185254=CARTESIAN_POINT('Ctrl Pts',(20.6996742824258,19.9989385344372,6.66417092004486));
#185255=CARTESIAN_POINT('Ctrl Pts',(20.6785117211371,20.0498062143585,6.66068376497394));
#185256=CARTESIAN_POINT('Ctrl Pts',(20.6094732749493,20.1990543145289,6.65011409545868));
#185257=CARTESIAN_POINT('Ctrl Pts',(20.5559344351494,20.2946063773585,6.64288319061463));
#185258=CARTESIAN_POINT('Ctrl Pts',(20.4696794884061,20.4239432277173,6.63261385179871));
#185259=CARTESIAN_POINT('Ctrl Pts',(20.44285269472,20.4614548073539,6.62957403903283));
#185260=CARTESIAN_POINT('Ctrl Pts',(20.4015499634587,20.5153936039311,6.62513734810568));
#185261=CARTESIAN_POINT('Ctrl Pts',(20.3880103889407,20.5325200466475,6.62371844666039));
#185262=CARTESIAN_POINT('Ctrl Pts',(20.3415173540985,20.5894957558536,6.61897087062038));
#185263=CARTESIAN_POINT('Ctrl Pts',(20.3073668783397,20.628349714408,6.61568714388755));
#185264=CARTESIAN_POINT('Ctrl Pts',(20.2658807413723,20.672199917883,6.61196387318168));
#185265=CARTESIAN_POINT('Ctrl Pts',(20.2598980920147,20.6784463616942,6.61143307505074));
#185266=CARTESIAN_POINT('Ctrl Pts',(20.2507671154801,20.6878637307102,6.61063243109202));
#185267=CARTESIAN_POINT('Ctrl Pts',(20.2476468387929,20.6910615561349,6.6103604894806));
#185268=CARTESIAN_POINT('Ctrl Pts',(20.242020096377,20.6967917362461,6.60987311294294));
#185269=CARTESIAN_POINT('Ctrl Pts',(20.2395173531268,20.6993276502774,6.60965739516212));
#185270=CARTESIAN_POINT('Ctrl Pts',(20.2340562560055,20.7048332567298,6.60918900400131));
#185271=CARTESIAN_POINT('Ctrl Pts',(20.231095490396,20.7078004754904,6.60893652590478));
#185272=CARTESIAN_POINT('Ctrl Pts',(20.2227310420603,20.7161335074382,6.60822729039273));
#185273=CARTESIAN_POINT('Ctrl Pts',(20.2173071287359,20.7214790487259,6.60777210682142));
#185274=CARTESIAN_POINT('Ctrl Pts',(20.1842213334862,20.7537366946136,6.60502308558937));
#185275=CARTESIAN_POINT('Ctrl Pts',(20.1558547321966,20.7799193631107,6.60278231242563));
#185276=CARTESIAN_POINT('Ctrl Pts',(20.0589354533622,20.864587669963,6.59544042493736));
#185277=CARTESIAN_POINT('Ctrl Pts',(19.9873644081435,20.9194748687773,6.5905170281054));
#185278=CARTESIAN_POINT('Ctrl Pts',(19.770353960458,21.0648991689962,6.57631228003958));
#185279=CARTESIAN_POINT('Ctrl Pts',(19.6171923558013,21.1425631124966,6.56709194761994));
#185280=CARTESIAN_POINT('Ctrl Pts',(19.4344703438857,21.2088920312135,6.55579964131705));
#185281=CARTESIAN_POINT('Ctrl Pts',(19.412452264007,21.2164759368467,6.55443564420814));
#185282=CARTESIAN_POINT('Ctrl Pts',(19.3811920168881,21.2266695055422,6.55249268978683));
#185283=CARTESIAN_POINT('Ctrl Pts',(19.3720498497566,21.2295820386886,6.55192370271024));
#185284=CARTESIAN_POINT('Ctrl Pts',(19.3571823527064,21.2342074694699,6.55099702771811));
#185285=CARTESIAN_POINT('Ctrl Pts',(19.3514689484114,21.2359584701578,6.55064059397496));
#185286=CARTESIAN_POINT('Ctrl Pts',(19.3395091927779,21.2395684829232,6.54989376929634));
#185287=CARTESIAN_POINT('Ctrl Pts',(19.333261525781,21.2414228856798,6.54950323201497));
#185288=CARTESIAN_POINT('Ctrl Pts',(19.3184058901224,21.2457577263047,6.54857361618221));
#185289=CARTESIAN_POINT('Ctrl Pts',(19.3097905953382,21.2482124178963,6.54803370463748));
#185290=CARTESIAN_POINT('Ctrl Pts',(19.2808434871231,21.2562618124179,6.54621681249706));
#185291=CARTESIAN_POINT('Ctrl Pts',(19.2604442186606,21.2616072551544,6.54493178864399));
#185292=CARTESIAN_POINT('Ctrl Pts',(19.1497962395621,21.2888417250806,6.53793449411119));
#185293=CARTESIAN_POINT('Ctrl Pts',(19.0582726050505,21.3050764277848,6.53204281257723));
#185294=CARTESIAN_POINT('Ctrl Pts',(18.8139508063882,21.3320123496317,6.51608926787609));
#185295=CARTESIAN_POINT('Ctrl Pts',(18.6605552268599,21.3322467211271,6.50581704810741));
#185296=CARTESIAN_POINT('Ctrl Pts',(18.5039746660936,21.3154709224792,6.49562541670175));
#185297=CARTESIAN_POINT('Ctrl Pts',(18.499472319018,21.3149739269096,6.4953326543284));
#185298=CARTESIAN_POINT('Ctrl Pts',(18.4885904756535,21.3137373610616,6.49462581937674));
#185299=CARTESIAN_POINT('Ctrl Pts',(18.4822126514723,21.3129832008865,6.49421216893194));
#185300=CARTESIAN_POINT('Ctrl Pts',(18.4308574777154,21.3066735023005,6.49088690304002));
#185301=CARTESIAN_POINT('Ctrl Pts',(18.3860619035265,21.2997035613455,6.48802024245565));
#185302=CARTESIAN_POINT('Ctrl Pts',(18.3340481782807,21.2898904190966,6.48475743232259));
#185303=CARTESIAN_POINT('Ctrl Pts',(18.3265826491635,21.2884402375357,6.48429072076943));
#185304=CARTESIAN_POINT('Ctrl Pts',(18.3146117237332,21.2860478685214,6.48354510019041));
#185305=CARTESIAN_POINT('Ctrl Pts',(18.3101013822464,21.2851311785215,6.48326479697567));
#185306=CARTESIAN_POINT('Ctrl Pts',(18.3020856641791,21.283474810614,6.48276780705407));
#185307=CARTESIAN_POINT('Ctrl Pts',(18.2985791368152,21.2827409362016,6.48255079324164));
#185308=CARTESIAN_POINT('Ctrl Pts',(18.2911140330452,21.281158788451,6.48208964836945));
#185309=CARTESIAN_POINT('Ctrl Pts',(18.2871560316332,21.2803080625399,6.48184565953584));
#185310=CARTESIAN_POINT('Ctrl Pts',(18.2763982219499,21.2779634928785,6.48118382920562));
#185311=CARTESIAN_POINT('Ctrl Pts',(18.269603233573,21.2764474368937,6.48076724122038));
#185312=CARTESIAN_POINT('Ctrl Pts',(18.234820074199,21.2685065026646,6.47864159410593));
#185313=CARTESIAN_POINT('Ctrl Pts',(18.2069557717729,21.2615458230706,6.47696150413894));
#185314=CARTESIAN_POINT('Ctrl Pts',(18.1252214153121,21.2393517498978,6.47207754846553));
#185315=CARTESIAN_POINT('Ctrl Pts',(18.0718017058866,21.2225457941321,6.46894254634176));
#185316=CARTESIAN_POINT('Ctrl Pts',(17.8360824269301,21.1379776622748,6.45511667775489));
#185317=CARTESIAN_POINT('Ctrl Pts',(17.6629847613231,21.0474170405242,6.44488900683143));
#185318=CARTESIAN_POINT('Ctrl Pts',(17.471835043354,20.9110752380083,6.43145748909968));
#185319=CARTESIAN_POINT('Ctrl Pts',(17.4396724908183,20.886718406742,6.4291186621684));
#185320=CARTESIAN_POINT('Ctrl Pts',(17.3989225789456,20.8539849986759,6.42604110602431));
#185321=CARTESIAN_POINT('Ctrl Pts',(17.3896819009965,20.8464327457826,6.42533534593917));
#185322=CARTESIAN_POINT('Ctrl Pts',(17.37501017457,20.8342334198388,6.42420186880182));
#185323=CARTESIAN_POINT('Ctrl Pts',(17.3695378641247,20.829636203334,6.42377618270377));
#185324=CARTESIAN_POINT('Ctrl Pts',(17.3593292881262,20.8209715553607,6.42297652386949));
#185325=CARTESIAN_POINT('Ctrl Pts',(17.3545875207941,20.8169107030192,6.42260282429352));
#185326=CARTESIAN_POINT('Ctrl Pts',(17.3439205614068,20.8076934116243,6.42175698184209));
#185327=CARTESIAN_POINT('Ctrl Pts',(17.338005989974,20.802524871845,6.4212843391931));
#185328=CARTESIAN_POINT('Ctrl Pts',(17.3206339557985,20.7871727073747,6.4198852180242));
#185329=CARTESIAN_POINT('Ctrl Pts',(17.3092583675527,20.7768975827782,6.41895491115518));
#185330=CARTESIAN_POINT('Ctrl Pts',(17.2835628868592,20.7531760639361,6.4168205525066));
#185331=CARTESIAN_POINT('Ctrl Pts',(17.2693167107258,20.7396522341121,6.4156132496631));
#185332=CARTESIAN_POINT('Ctrl Pts',(17.2233142577662,20.6947488369198,6.41163455384641));
#185333=CARTESIAN_POINT('Ctrl Pts',(17.1923637336177,20.6625643951854,6.40882909873871));
#185334=CARTESIAN_POINT('Ctrl Pts',(17.1124879833172,20.5740661702069,6.40123614976628));
#185335=CARTESIAN_POINT('Ctrl Pts',(17.0654846546327,20.5161075018084,6.39638472645276));
#185336=CARTESIAN_POINT('Ctrl Pts',(16.9257448224572,20.3238790190281,6.38075997451635));
#185337=CARTESIAN_POINT('Ctrl Pts',(16.8454098971218,20.1813194608543,6.36980564684395));
#185338=CARTESIAN_POINT('Ctrl Pts',(16.7767895748611,20.0179784053648,6.35877883394721));
#185339=CARTESIAN_POINT('Ctrl Pts',(16.771471575353,20.0049578084932,6.35791007378176));
#185340=CARTESIAN_POINT('Ctrl Pts',(16.7642416473625,19.9867394384101,6.35670968001164));
#185341=CARTESIAN_POINT('Ctrl Pts',(16.7622198869111,19.9815860310856,6.35637180607979));
#185342=CARTESIAN_POINT('Ctrl Pts',(16.7590028507478,19.9732903396895,6.35583067912908));
#185343=CARTESIAN_POINT('Ctrl Pts',(16.7577948213683,19.970153076694,6.3556266693372));
#185344=CARTESIAN_POINT('Ctrl Pts',(16.7552832777342,19.963583955137,6.35520083715555));
#185345=CARTESIAN_POINT('Ctrl Pts',(16.7539812120649,19.9601515708852,6.35497910651347));
#185346=CARTESIAN_POINT('Ctrl Pts',(16.7508467966457,19.95182366009,6.35444294816883));
#185347=CARTESIAN_POINT('Ctrl Pts',(16.7490236221209,19.9469246591297,6.35412906756367));
#185348=CARTESIAN_POINT('Ctrl Pts',(16.7466168276675,19.9403834130632,6.35371193039897));
#185349=CARTESIAN_POINT('Ctrl Pts',(16.7460170848424,19.9387471854834,6.35360775105671));
#185350=CARTESIAN_POINT('Ctrl Pts',(16.7454193623257,19.9371102171619,6.35350368608372));
#185351=CARTESIAN_POINT('',(16.6170007251258,19.2092478064746,6.8890562790225));
#185352=CARTESIAN_POINT('Ctrl Pts',(16.6170007251258,19.2092478064745,6.8890562790225));
#185353=CARTESIAN_POINT('Ctrl Pts',(16.6170993834536,19.0900488678703,6.88186870628082));
#185354=CARTESIAN_POINT('Ctrl Pts',(16.6272689227094,18.9712546433195,6.87468113353914));
#185355=CARTESIAN_POINT('Ctrl Pts',(16.6472858251195,18.8541905938,6.86749356079746));
#185356=CARTESIAN_POINT('Ctrl Pts',(16.6595066892529,18.7827198030267,6.86310535186656));
#185357=CARTESIAN_POINT('Ctrl Pts',(16.6754275106646,18.7117380828086,6.85871714293566));
#185358=CARTESIAN_POINT('Ctrl Pts',(16.6949957094315,18.6416578330712,6.85432893400476));
#185359=CARTESIAN_POINT('Ctrl Pts',(16.7145348657469,18.571681594044,6.84994723790349));
#185360=CARTESIAN_POINT('Ctrl Pts',(16.7377105245955,18.5026046302857,6.84556554180222));
#185361=CARTESIAN_POINT('Ctrl Pts',(16.7644188550043,18.4348304867638,6.84118384570095));
#185362=CARTESIAN_POINT('Ctrl Pts',(16.7910958009993,18.3671359832542,6.83680729844131));
#185363=CARTESIAN_POINT('Ctrl Pts',(16.8212969962485,18.3007417053631,6.83243075118166));
#185364=CARTESIAN_POINT('Ctrl Pts',(16.8548689277715,18.2360356860965,6.82805420392202));
#185365=CARTESIAN_POINT('Ctrl Pts',(16.8884195684635,18.171370702447,6.82368043220504));
#185366=CARTESIAN_POINT('Ctrl Pts',(16.9253364824029,18.1083922801994,6.81930666048807));
#185367=CARTESIAN_POINT('Ctrl Pts',(16.9654187837194,18.0474668112084,6.81493288877109));
#185368=CARTESIAN_POINT('Ctrl Pts',(17.005488887857,17.9865598820423,6.81056044800753));
#185369=CARTESIAN_POINT('Ctrl Pts',(17.048722202085,17.9277050686151,6.80618800724398));
#185370=CARTESIAN_POINT('Ctrl Pts',(17.0948736736056,17.87124110896,6.80181556648042));
#185371=CARTESIAN_POINT('Ctrl Pts',(17.1410263252243,17.8147757055153,6.79744301391308));
#185372=CARTESIAN_POINT('Ctrl Pts',(17.1900969754574,17.7607016494436,6.79307046134574));
#185373=CARTESIAN_POINT('Ctrl Pts',(17.24180038849,17.7093244959681,6.7886979087784));
#185374=CARTESIAN_POINT('Ctrl Pts',(17.2935574612749,17.6578940213448,6.78432081821107));
#185375=CARTESIAN_POINT('Ctrl Pts',(17.3479524093388,17.6091663783432,6.77994372764374));
#185376=CARTESIAN_POINT('Ctrl Pts',(17.4046638348792,17.5634095290085,6.77556663707641));
#185377=CARTESIAN_POINT('Ctrl Pts',(17.4614062326339,17.5176276901602,6.77118715601746));
#185378=CARTESIAN_POINT('Ctrl Pts',(17.5204672358497,17.4748201585677,6.76680767495852));
#185379=CARTESIAN_POINT('Ctrl Pts',(17.5814953303095,17.435212291308,6.76242819389957));
#185380=CARTESIAN_POINT('Ctrl Pts',(17.6426315966571,17.3955342193695,6.75804095023985));
#185381=CARTESIAN_POINT('Ctrl Pts',(17.7057414989266,17.3590673788383,6.75365370658012));
#185382=CARTESIAN_POINT('Ctrl Pts',(17.7704482580139,17.3259915012087,6.7492664629204));
#185383=CARTESIAN_POINT('Ctrl Pts',(17.8144426190643,17.3035030916047,6.7462835599856));
#185384=CARTESIAN_POINT('Ctrl Pts',(17.8591746727796,17.2825812380498,6.74330065705081));
#185385=CARTESIAN_POINT('Ctrl Pts',(17.9045214391032,17.2632694444527,6.74031775411601));
#185386=CARTESIAN_POINT('Ctrl Pts',(17.971231985614,17.2348594737004,6.73592954518512));
#185387=CARTESIAN_POINT('Ctrl Pts',(18.0395340178844,17.2098253061038,6.73154133625423));
#185388=CARTESIAN_POINT('Ctrl Pts',(18.1090523123257,17.1883459545264,6.72715312732333));
#185389=CARTESIAN_POINT('Ctrl Pts',(18.1784674300917,17.1668984818681,6.72277143122207));
#185390=CARTESIAN_POINT('Ctrl Pts',(18.2490947695194,17.1489954929982,6.7183897351208));
#185391=CARTESIAN_POINT('Ctrl Pts',(18.3205388114172,17.1347681137369,6.71400803901954));
#185392=CARTESIAN_POINT('Ctrl Pts',(18.39189890088,17.1205574527785,6.7096314917599));
#185393=CARTESIAN_POINT('Ctrl Pts',(18.4640733156415,17.1100139151849,6.70525494450027));
#185394=CARTESIAN_POINT('Ctrl Pts',(18.5366526876863,17.1032184557401,6.70087839724063));
#185395=CARTESIAN_POINT('Ctrl Pts',(18.6091860309483,17.096427305877,6.69650462552366));
#185396=CARTESIAN_POINT('Ctrl Pts',(18.6821233428378,17.0933795627893,6.69213085380669));
#185397=CARTESIAN_POINT('Ctrl Pts',(18.7550478100762,17.0941046342129,6.68775708208972));
#185398=CARTESIAN_POINT('Ctrl Pts',(18.8279500861543,17.0948294849947,6.68338464132617));
#185399=CARTESIAN_POINT('Ctrl Pts',(18.9008390432773,17.0993248662018,6.67901220056263));
#185400=CARTESIAN_POINT('Ctrl Pts',(18.973297213934,17.1075680796842,6.67463975979908));
#185401=CARTESIAN_POINT('Ctrl Pts',(19.0457572373541,17.1158115039465,6.67026720723174));
#185402=CARTESIAN_POINT('Ctrl Pts',(19.1177859733783,17.1278028942377,6.66589465466439));
#185403=CARTESIAN_POINT('Ctrl Pts',(19.1889721056822,17.1434678036241,6.66152210209705));
#185404=CARTESIAN_POINT('Ctrl Pts',(19.2602321176392,17.1591489706443,6.65714501152973));
#185405=CARTESIAN_POINT('Ctrl Pts',(19.330647307792,17.1785111648148,6.6527679209624));
#185406=CARTESIAN_POINT('Ctrl Pts',(19.3998183959317,17.2014291842189,6.64839083039508));
#185407=CARTESIAN_POINT('Ctrl Pts',(19.4690272609699,17.2243597200041,6.64401134933614));
#185408=CARTESIAN_POINT('Ctrl Pts',(19.5369902214606,17.2508497721601,6.6396318682772));
#185409=CARTESIAN_POINT('Ctrl Pts',(19.6033275197868,17.2807257543703,6.63525238721827));
#185410=CARTESIAN_POINT('Ctrl Pts',(19.6697824005289,17.3106546915584,6.63086514355855));
#185411=CARTESIAN_POINT('Ctrl Pts',(19.7346054355376,17.3439813228772,6.62647789989883));
#185412=CARTESIAN_POINT('Ctrl Pts',(19.7974415556861,17.3804861219756,6.62209065623912));
#185413=CARTESIAN_POINT('Ctrl Pts',(19.8401640625133,17.4053058677686,6.61910775330427));
#185414=CARTESIAN_POINT('Ctrl Pts',(19.8819686426642,17.4315938434276,6.61612485036943));
#185415=CARTESIAN_POINT('Ctrl Pts',(19.922752149464,17.4592701900279,6.61314194743459));
#185416=CARTESIAN_POINT('Ctrl Pts',(19.982749592452,17.4999854241401,6.60875373850369));
#185417=CARTESIAN_POINT('Ctrl Pts',(20.0407699602753,17.5438661041391,6.60436552957279));
#185418=CARTESIAN_POINT('Ctrl Pts',(20.0964596300332,17.590693622635,6.5999773206419));
#185419=CARTESIAN_POINT('Ctrl Pts',(20.1520666470877,17.6374516413292,6.59559562454063));
#185420=CARTESIAN_POINT('Ctrl Pts',(20.2053494667967,17.6871475084509,6.59121392843937));
#185421=CARTESIAN_POINT('Ctrl Pts',(20.2559837460597,17.7395196308717,6.5868322323381));
#185422=CARTESIAN_POINT('Ctrl Pts',(20.306558526015,17.7918302118807,6.58245568507846));
#185423=CARTESIAN_POINT('Ctrl Pts',(20.3544906143945,17.8468104559209,6.57807913781883));
#185424=CARTESIAN_POINT('Ctrl Pts',(20.3994903578941,17.9041599685647,6.57370259055919));
#185425=CARTESIAN_POINT('Ctrl Pts',(20.4444615632103,17.961473110981,6.56932881884221));
#185426=CARTESIAN_POINT('Ctrl Pts',(20.4865038163914,18.0211521621719,6.56495504712524));
#185427=CARTESIAN_POINT('Ctrl Pts',(20.5253667770635,18.0828625659818,6.56058127540827));
#185428=CARTESIAN_POINT('Ctrl Pts',(20.5642179116062,18.1445541911086,6.55620883464472));
#185429=CARTESIAN_POINT('Ctrl Pts',(20.5998914174628,18.2082755337073,6.55183639388117));
#185430=CARTESIAN_POINT('Ctrl Pts',(20.6321804129395,18.2736632835887,6.54746395311761));
#185431=CARTESIAN_POINT('Ctrl Pts',(20.6644702340494,18.339052705442,6.54309140055027));
#185432=CARTESIAN_POINT('Ctrl Pts',(20.69337516117,18.4061081857736,6.53871884798293));
#185433=CARTESIAN_POINT('Ctrl Pts',(20.7187351546659,18.4744435759338,6.53434629541559));
#185434=CARTESIAN_POINT('Ctrl Pts',(20.7441214677198,18.5428498871395,6.52996920484826));
#185435=CARTESIAN_POINT('Ctrl Pts',(20.765955333456,18.6125383070841,6.52559211428094));
#185436=CARTESIAN_POINT('Ctrl Pts',(20.7841259040689,18.6831053348765,6.52121502371361));
#185437=CARTESIAN_POINT('Ctrl Pts',(20.8023063983048,18.7537109019418,6.51683554265467));
#185438=CARTESIAN_POINT('Ctrl Pts',(20.8168195180773,18.8251955591513,6.51245606159573));
#185439=CARTESIAN_POINT('Ctrl Pts',(20.8276056664128,18.8971460314662,6.50807658053679));
#185440=CARTESIAN_POINT('Ctrl Pts',(20.8384109331237,18.9692240355102,6.50368933687707));
#185441=CARTESIAN_POINT('Ctrl Pts',(20.8454759896224,19.0417690229281,6.49930209321735));
#185442=CARTESIAN_POINT('Ctrl Pts',(20.8487932306455,19.1143636113251,6.49491484955763));
#185443=CARTESIAN_POINT('Ctrl Pts',(20.8510486348926,19.1637209362373,6.4919319466228));
#185444=CARTESIAN_POINT('Ctrl Pts',(20.8515726338748,19.213101155059,6.48894904368798));
#185445=CARTESIAN_POINT('Ctrl Pts',(20.8503765449711,19.2623743116388,6.48596614075315));
#185446=CARTESIAN_POINT('Ctrl Pts',(20.8486169543561,19.33486105039,6.48157793182225));
#185447=CARTESIAN_POINT('Ctrl Pts',(20.8431255714045,19.4073987776277,6.47718972289135));
#185448=CARTESIAN_POINT('Ctrl Pts',(20.8338948009668,19.4795718244205,6.47280151396045));
#185449=CARTESIAN_POINT('Ctrl Pts',(20.8246777305229,19.5516377544454,6.46841981785919));
#185450=CARTESIAN_POINT('Ctrl Pts',(20.8117323505349,19.623339603948,6.46403812175792));
#185451=CARTESIAN_POINT('Ctrl Pts',(20.7951030586571,19.6942630563103,6.45965642565665));
#185452=CARTESIAN_POINT('Ctrl Pts',(20.7784933075206,19.7651031679718,6.45527987839701));
#185453=CARTESIAN_POINT('Ctrl Pts',(20.7582083534309,19.8351662321977,6.45090333113737));
#185454=CARTESIAN_POINT('Ctrl Pts',(20.7343439967233,19.9040460985916,6.44652678387773));
#185455=CARTESIAN_POINT('Ctrl Pts',(20.7104947744439,19.9728822823753,6.44215301216075));
#185456=CARTESIAN_POINT('Ctrl Pts',(20.6830708110594,20.0405363024768,6.43777924044378));
#185457=CARTESIAN_POINT('Ctrl Pts',(20.6522179108558,20.1066165733571,6.4334054687268));
#185458=CARTESIAN_POINT('Ctrl Pts',(20.6213743992934,20.172676735789,6.42903302796325));
#185459=CARTESIAN_POINT('Ctrl Pts',(20.5871042264077,20.2371636629376,6.4246605871997));
#185460=CARTESIAN_POINT('Ctrl Pts',(20.5496008974355,20.2997067471232,6.42028814643614));
#185461=CARTESIAN_POINT('Ctrl Pts',(20.512096609499,20.3622514305424,6.4159155938688));
#185462=CARTESIAN_POINT('Ctrl Pts',(20.471359251125,20.4228517596427,6.41154304130145));
#185463=CARTESIAN_POINT('Ctrl Pts',(20.4276268857992,20.4811641514774,6.40717048873411));
#185464=CARTESIAN_POINT('Ctrl Pts',(20.3838491333751,20.5395370621118,6.40279339816678));
#185465=CARTESIAN_POINT('Ctrl Pts',(20.3370704580442,20.5956169078824,6.39841630759945));
#185466=CARTESIAN_POINT('Ctrl Pts',(20.2875701403857,20.6490920759472,6.39403921703212));
#185467=CARTESIAN_POINT('Ctrl Pts',(20.2380427887665,20.7025964487859,6.38965973597318));
#185468=CARTESIAN_POINT('Ctrl Pts',(20.1857911812153,20.7534929748974,6.38528025491424));
#185469=CARTESIAN_POINT('Ctrl Pts',(20.1311305579261,20.8015078447179,6.38090077385529));
#185470=CARTESIAN_POINT('Ctrl Pts',(20.076373049049,20.8496078205729,6.37651353019557));
#185471=CARTESIAN_POINT('Ctrl Pts',(20.0191983762069,20.8948156407836,6.37212628653585));
#185472=CARTESIAN_POINT('Ctrl Pts',(19.9599533753571,20.9368989893533,6.36773904287613));
#185473=CARTESIAN_POINT('Ctrl Pts',(19.919672483614,20.9655116112387,6.36475613994132));
#185474=CARTESIAN_POINT('Ctrl Pts',(19.878435164885,20.9926807873361,6.36177323700652));
#185475=CARTESIAN_POINT('Ctrl Pts',(19.8363568176098,21.0183456909704,6.35879033407171));
#185476=CARTESIAN_POINT('Ctrl Pts',(19.7744545085685,21.0561018505907,6.35440212514082));
#185477=CARTESIAN_POINT('Ctrl Pts',(19.7104893778665,21.0907477625256,6.35001391620992));
#185478=CARTESIAN_POINT('Ctrl Pts',(19.6448068261836,21.1220520467474,6.34562570727902));
#185479=CARTESIAN_POINT('Ctrl Pts',(19.5792217582976,21.1533098702211,6.34124401117775));
#185480=CARTESIAN_POINT('Ctrl Pts',(19.5119247612707,21.1812357055046,6.33686231507649));
#185481=CARTESIAN_POINT('Ctrl Pts',(19.4432882414197,21.2056426222719,6.33248061897522));
#185482=CARTESIAN_POINT('Ctrl Pts',(19.3747323749418,21.2300208589696,6.32810407171558));
#185483=CARTESIAN_POINT('Ctrl Pts',(19.3048405647339,21.2508882305582,6.32372752445594));
#185484=CARTESIAN_POINT('Ctrl Pts',(19.2340061739094,21.2681054484524,6.3193509771963));
#185485=CARTESIAN_POINT('Ctrl Pts',(19.163216705226,21.2853117474372,6.31497720547933));
#185486=CARTESIAN_POINT('Ctrl Pts',(19.0914863095581,21.2988723720882,6.31060343376236));
#185487=CARTESIAN_POINT('Ctrl Pts',(19.0192231694687,21.3086979629104,6.30622966204538));
#185488=CARTESIAN_POINT('Ctrl Pts',(18.9469820192955,21.3185205637722,6.30185722128183));
#185489=CARTESIAN_POINT('Ctrl Pts',(18.8742089242432,21.324610322322,6.29748478051827));
#185490=CARTESIAN_POINT('Ctrl Pts',(18.801320247435,21.3269293429331,6.29311233975472));
#185491=CARTESIAN_POINT('Ctrl Pts',(18.7284297068553,21.3292484228418,6.28873978718738));
#185492=CARTESIAN_POINT('Ctrl Pts',(18.6554240608492,21.3277965600419,6.28436723462003));
#185493=CARTESIAN_POINT('Ctrl Pts',(18.5827210675513,21.3225879533179,6.27999468205269));
#185494=CARTESIAN_POINT('Ctrl Pts',(18.5099426203447,21.3173739409054,6.27561759148536));
#185495=CARTESIAN_POINT('Ctrl Pts',(18.4374679351509,21.3083954347152,6.27124050091803));
#185496=CARTESIAN_POINT('Ctrl Pts',(18.3657101983365,21.2957185953962,6.26686341035071));
#185497=CARTESIAN_POINT('Ctrl Pts',(18.2939132719587,21.2830348327847,6.26248392929177));
#185498=CARTESIAN_POINT('Ctrl Pts',(18.2228345439115,21.2666488240855,6.25810444823283));
#185499=CARTESIAN_POINT('Ctrl Pts',(18.1528748782446,21.2466774284903,6.25372496717389));
#185500=CARTESIAN_POINT('Ctrl Pts',(18.0827912095399,21.2266706337304,6.24933772351416));
#185501=CARTESIAN_POINT('Ctrl Pts',(18.0138310210294,21.2030659176044,6.24495047985444));
#185502=CARTESIAN_POINT('Ctrl Pts',(17.9463773894269,21.1760291660212,6.24056323619472));
#185503=CARTESIAN_POINT('Ctrl Pts',(17.9005154197537,21.1576467801999,6.23758033325991));
#185504=CARTESIAN_POINT('Ctrl Pts',(17.8553494637706,21.1376788808132,6.23459743032509));
#185505=CARTESIAN_POINT('Ctrl Pts',(17.810993130072,21.1161895753614,6.23161452739028));
#185506=CARTESIAN_POINT('Ctrl Pts',(17.7457580547162,21.0845851494857,6.22722755755968));
#185507=CARTESIAN_POINT('Ctrl Pts',(17.6820207921133,21.0495646312793,6.22284058772908));
#185508=CARTESIAN_POINT('Ctrl Pts',(17.6201625345974,21.0112930596615,6.21845361789848));
#185509=CARTESIAN_POINT('Ctrl Pts',(17.5583882674481,20.973073452704,6.21407260464052));
#185510=CARTESIAN_POINT('Ctrl Pts',(17.4984883504397,20.9316118007434,6.20969159138257));
#185511=CARTESIAN_POINT('Ctrl Pts',(17.4408213800117,20.8871199410559,6.20531057812461));
#185512=CARTESIAN_POINT('Ctrl Pts',(17.3832136794392,20.8426738099037,6.20093406765258));
#185513=CARTESIAN_POINT('Ctrl Pts',(17.3278347507055,20.7952039448586,6.19655755718055));
#185514=CARTESIAN_POINT('Ctrl Pts',(17.2750146386712,20.744965682611,6.19218104670852));
#185515=CARTESIAN_POINT('Ctrl Pts',(17.2222313878241,20.694762479774,6.18780759044001));
#185516=CARTESIAN_POINT('Ctrl Pts',(17.1720037564642,20.641795047518,6.18343413417149));
#185517=CARTESIAN_POINT('Ctrl Pts',(17.1246277766866,20.5863581522015,6.17906067790298));
#185518=CARTESIAN_POINT('Ctrl Pts',(17.0772569743077,20.5309273152064,6.17468769957978));
#185519=CARTESIAN_POINT('Ctrl Pts',(17.032737527321,20.4730279095102,6.17031472125657));
#185520=CARTESIAN_POINT('Ctrl Pts',(16.9913267830634,20.4129896251515,6.16594174293336));
#185521=CARTESIAN_POINT('Ctrl Pts',(16.9499189762244,20.3529555995323,6.16156907480182));
#185522=CARTESIAN_POINT('Ctrl Pts',(16.9116197015745,20.290783398272,6.15719640667029));
#185523=CARTESIAN_POINT('Ctrl Pts',(16.8766431790035,20.2268319937361,6.15282373853875));
#185524=CARTESIAN_POINT('Ctrl Pts',(16.8416426205659,20.1628366417943,6.14844806550962));
#185525=CARTESIAN_POINT('Ctrl Pts',(16.8099695961625,20.0970600736454,6.14407239248049));
#185526=CARTESIAN_POINT('Ctrl Pts',(16.7817919876605,20.0298851424696,6.13969671945136));
#185527=CARTESIAN_POINT('Ctrl Pts',(16.7689367260135,19.9992384211085,6.13770043855097));
#185528=CARTESIAN_POINT('Ctrl Pts',(16.7568083349981,19.9683009234817,6.13570415765058));
#185529=CARTESIAN_POINT('Ctrl Pts',(16.7454193623258,19.9371102171621,6.13370787675019));
#185530=CARTESIAN_POINT('Ctrl Pts',(16.7486737101886,19.9359290495398,6.93361858560548));
#185531=CARTESIAN_POINT('Ctrl Pts',(16.6638908325239,19.7029525058723,6.91876473928283));
#185532=CARTESIAN_POINT('Ctrl Pts',(16.617844370368,19.4557557402532,6.90391089296018));
#185533=CARTESIAN_POINT('Ctrl Pts',(16.6156461087368,19.2092594235966,6.88905704663753));
#185534=CARTESIAN_POINT('Origin',(18.734,19.211,0.));
#185535=CARTESIAN_POINT('',(16.7454193311435,19.9371101317641,7.95734462820299));
#185536=CARTESIAN_POINT('',(16.7454193726884,19.9371102455419,7.73405220823975));
#185537=CARTESIAN_POINT('',(16.7454193623258,19.9371102171621,0.));
#185538=CARTESIAN_POINT('',(16.617000799818,19.2090893184087,7.91072951538306));
#185539=CARTESIAN_POINT('Ctrl Pts',(16.7454193311435,19.9371101317641,7.95734462820299));
#185540=CARTESIAN_POINT('Ctrl Pts',(16.7388878108518,19.9192224114001,7.95624410831949));
#185541=CARTESIAN_POINT('Ctrl Pts',(16.732595939587,19.9012418899709,7.95513586263103));
#185542=CARTESIAN_POINT('Ctrl Pts',(16.7220479121879,19.8697400685245,7.95318935666933));
#185543=CARTESIAN_POINT('Ctrl Pts',(16.7176850003347,19.8562623413191,7.95235503299141));
#185544=CARTESIAN_POINT('Ctrl Pts',(16.7109454732511,19.8347068686673,7.95101780437524));
#185545=CARTESIAN_POINT('Ctrl Pts',(16.7084811681145,19.8266568319897,7.95051777631579));
#185546=CARTESIAN_POINT('Ctrl Pts',(16.7042134956983,19.8124128052234,7.94963180975945));
#185547=CARTESIAN_POINT('Ctrl Pts',(16.7023902911245,19.8062248354304,7.94924652551381));
#185548=CARTESIAN_POINT('Ctrl Pts',(16.698671963352,19.7933886782359,7.94844643859772));
#185549=CARTESIAN_POINT('Ctrl Pts',(16.6967810667854,19.7867393556909,7.94803150335748));
#185550=CARTESIAN_POINT('Ctrl Pts',(16.6919990780092,19.7696049843739,7.94696098844802));
#185551=CARTESIAN_POINT('Ctrl Pts',(16.6891561857431,19.7591067983157,7.94630385146098));
#185552=CARTESIAN_POINT('Ctrl Pts',(16.6831808743635,19.7363475538504,7.94487640696553));
#185553=CARTESIAN_POINT('Ctrl Pts',(16.6800772595627,19.724079432261,7.94410519509892));
#185554=CARTESIAN_POINT('Ctrl Pts',(16.6713661718758,19.688299612147,7.94185059233987));
#185555=CARTESIAN_POINT('Ctrl Pts',(16.6660512902545,19.6647193927235,7.94035798085899));
#185556=CARTESIAN_POINT('Ctrl Pts',(16.631655769437,19.4989331522908,7.92981457930352));
#185557=CARTESIAN_POINT('Ctrl Pts',(16.6168699507311,19.3541831232757,7.92031685552876));
#185558=CARTESIAN_POINT('Ctrl Pts',(16.6170008616849,19.2090899284988,7.91072944747406));
#185559=CARTESIAN_POINT('Ctrl Pts',(16.617000862229,19.2090893255851,7.91072940763498));
#185560=CARTESIAN_POINT('Ctrl Pts',(16.6171115217323,19.0864802242008,7.90262769413136));
#185561=CARTESIAN_POINT('Ctrl Pts',(16.6278735760837,18.9640980518275,7.8945060011454));
#185562=CARTESIAN_POINT('Ctrl Pts',(16.6513555110906,18.8309489058585,7.88604138153807));
#185563=CARTESIAN_POINT('Ctrl Pts',(16.6536481219582,18.8185933470417,7.88525964032872));
#185564=CARTESIAN_POINT('Ctrl Pts',(16.6573287545432,18.7996969149763,7.88407053382136));
#185565=CARTESIAN_POINT('Ctrl Pts',(16.6586379308329,18.793141203293,7.88365919776567));
#185566=CARTESIAN_POINT('Ctrl Pts',(16.6608486749733,18.782337616983,7.88298343355589));
#185567=CARTESIAN_POINT('Ctrl Pts',(16.6617322869808,18.7780861732261,7.88271804429092));
#185568=CARTESIAN_POINT('Ctrl Pts',(16.6634789751564,18.7698099859251,7.88220250717016));
#185569=CARTESIAN_POINT('Ctrl Pts',(16.66434072053,18.7657849840704,7.88195228641702));
#185570=CARTESIAN_POINT('Ctrl Pts',(16.6659719859702,18.7582728359787,7.88148625496955));
#185571=CARTESIAN_POINT('Ctrl Pts',(16.6667385813809,18.7547851611577,7.88127028640043));
#185572=CARTESIAN_POINT('Ctrl Pts',(16.6685067296264,18.7468368285494,7.88077898700932));
#185573=CARTESIAN_POINT('Ctrl Pts',(16.669513906878,18.7423774739779,7.88050398209707));
#185574=CARTESIAN_POINT('Ctrl Pts',(16.672647297999,18.7287103141891,7.8796629908247));
#185575=CARTESIAN_POINT('Ctrl Pts',(16.6748207597799,18.719513309208,7.87909964645304));
#185576=CARTESIAN_POINT('Ctrl Pts',(16.7060513545,18.591205808496,7.87127263433017));
#185577=CARTESIAN_POINT('Ctrl Pts',(16.7453452243574,18.4748060097416,7.86455349602807));
#185578=CARTESIAN_POINT('Ctrl Pts',(16.8230773833356,18.2971367491519,7.85400318070861));
#185579=CARTESIAN_POINT('Ctrl Pts',(16.854933174031,18.2333093464563,7.85014914108799));
#185580=CARTESIAN_POINT('Ctrl Pts',(16.9337303111766,18.0935635691121,7.84135922203372));
#185581=CARTESIAN_POINT('Ctrl Pts',(16.9823694337745,18.0187654453276,7.83640085431816));
#185582=CARTESIAN_POINT('Ctrl Pts',(17.0559433438922,17.9198845367816,7.82930991886426));
#185583=CARTESIAN_POINT('Ctrl Pts',(17.0769701061936,17.8930072010336,7.82732372237705));
#185584=CARTESIAN_POINT('Ctrl Pts',(17.1055478167489,17.8582432064424,7.8246699426616));
#185585=CARTESIAN_POINT('Ctrl Pts',(17.1125238996734,17.8498891650469,7.82402556213667));
#185586=CARTESIAN_POINT('Ctrl Pts',(17.1240368074629,17.8363162798019,7.82296749191349));
#185587=CARTESIAN_POINT('Ctrl Pts',(17.1285353880166,17.8310651501514,7.82255537444089));
#185588=CARTESIAN_POINT('Ctrl Pts',(17.1372800805119,17.8209582359015,7.82175674696685));
#185589=CARTESIAN_POINT('Ctrl Pts',(17.1415228233908,17.8160996280098,7.82137037924043));
#185590=CARTESIAN_POINT('Ctrl Pts',(17.1513515164192,17.8049475159386,7.82047782489024));
#185591=CARTESIAN_POINT('Ctrl Pts',(17.1569528912002,17.7986678068003,7.81997099516518));
#185592=CARTESIAN_POINT('Ctrl Pts',(17.1720751254772,17.7819163817515,7.81860748511263));
#185593=CARTESIAN_POINT('Ctrl Pts',(17.1816636786611,17.7715066058566,7.81774794787695));
#185594=CARTESIAN_POINT('Ctrl Pts',(17.2658241721346,17.6819569003964,7.81024558095259));
#185595=CARTESIAN_POINT('Ctrl Pts',(17.3462751126359,17.6085873372018,7.80334315202871));
#185596=CARTESIAN_POINT('Ctrl Pts',(17.5090293811134,17.4816414482223,7.78990320663323));
#185597=CARTESIAN_POINT('Ctrl Pts',(17.5901303824558,17.4269610761572,7.78341790655111));
#185598=CARTESIAN_POINT('Ctrl Pts',(17.73695210681,17.3421093970625,7.77224084308671));
#185599=CARTESIAN_POINT('Ctrl Pts',(17.8009879643803,17.3093305855095,7.7675369343157));
#185600=CARTESIAN_POINT('Ctrl Pts',(17.8972779810167,17.2660788198424,7.76082201600904));
#185601=CARTESIAN_POINT('Ctrl Pts',(17.9283111977942,17.2530194117084,7.7587104101043));
#185602=CARTESIAN_POINT('Ctrl Pts',(17.9664251261026,17.2380400689219,7.75619157376596));
#185603=CARTESIAN_POINT('Ctrl Pts',(17.9732194597741,17.2354102020303,7.75574540180616));
#185604=CARTESIAN_POINT('Ctrl Pts',(17.9839075088589,17.2313365191189,7.75504814815731));
#185605=CARTESIAN_POINT('Ctrl Pts',(17.9877920522528,17.2298690244703,7.75479568550417));
#185606=CARTESIAN_POINT('Ctrl Pts',(17.9950210375755,17.2271623520456,7.75432766455028));
#185607=CARTESIAN_POINT('Ctrl Pts',(17.9983642606297,17.2259202082591,7.75411193498586));
#185608=CARTESIAN_POINT('Ctrl Pts',(18.0059514155221,17.2231230705309,7.75362396853561));
#185609=CARTESIAN_POINT('Ctrl Pts',(18.0101971870373,17.2215732190168,7.75335204009516));
#185610=CARTESIAN_POINT('Ctrl Pts',(18.0228092672688,17.2170150990527,7.75254755588709));
#185611=CARTESIAN_POINT('Ctrl Pts',(18.031189718727,17.2140458797639,7.75201726636002));
#185612=CARTESIAN_POINT('Ctrl Pts',(18.0942308656191,17.1921562230908,7.74805845901932));
#185613=CARTESIAN_POINT('Ctrl Pts',(18.1496329269367,17.1754285487274,7.74474933848112));
#185614=CARTESIAN_POINT('Ctrl Pts',(18.3637038705559,17.1202565307368,7.73236201565668));
#185615=CARTESIAN_POINT('Ctrl Pts',(18.5259378756946,17.0979349238789,7.72375541159319));
#185616=CARTESIAN_POINT('Ctrl Pts',(18.7491666387576,17.0932029041039,7.71138758736893));
#185617=CARTESIAN_POINT('Ctrl Pts',(18.809222593072,17.0944850986797,7.70801388948652));
#185618=CARTESIAN_POINT('Ctrl Pts',(18.8932766284678,17.0998616995016,7.70317726402674));
#185619=CARTESIAN_POINT('Ctrl Pts',(18.9173844496788,17.101819105777,7.70177689500875));
#185620=CARTESIAN_POINT('Ctrl Pts',(18.9594310889119,17.1059593405741,7.69930852682522));
#185621=CARTESIAN_POINT('Ctrl Pts',(18.9773855763199,17.1079596330659,7.69824619818415));
#185622=CARTESIAN_POINT('Ctrl Pts',(19.0037823945268,17.1112430332052,7.69667127659739));
#185623=CARTESIAN_POINT('Ctrl Pts',(19.0122463789486,17.1123478588993,7.69616430280104));
#185624=CARTESIAN_POINT('Ctrl Pts',(19.0270904075126,17.1143768651399,7.6952716034625));
#185625=CARTESIAN_POINT('Ctrl Pts',(19.0334733817576,17.115279062278,7.69488657759882));
#185626=CARTESIAN_POINT('Ctrl Pts',(19.0458714900072,17.1170892618334,7.69413641485472));
#185627=CARTESIAN_POINT('Ctrl Pts',(19.0518870325934,17.1179940661822,7.69377138287367));
#185628=CARTESIAN_POINT('Ctrl Pts',(19.0662773475747,17.1202219985307,7.69289559644162));
#185629=CARTESIAN_POINT('Ctrl Pts',(19.0746481857973,17.1215695279861,7.69238407203286));
#185630=CARTESIAN_POINT('Ctrl Pts',(19.1049399112946,17.1266327310313,7.69052533810902));
#185631=CARTESIAN_POINT('Ctrl Pts',(19.1268094194446,17.1306432924681,7.68916880568582));
#185632=CARTESIAN_POINT('Ctrl Pts',(19.3293663327736,17.1710971629178,7.67646435629404));
#185633=CARTESIAN_POINT('Ctrl Pts',(19.5046006152226,17.230643392469,7.6643295609358));
#185634=CARTESIAN_POINT('Ctrl Pts',(19.7425193903469,17.3479010943798,7.64681543233594));
#185635=CARTESIAN_POINT('Ctrl Pts',(19.813058936558,17.3878482103719,7.6414918430162));
#185636=CARTESIAN_POINT('Ctrl Pts',(19.9116121747825,17.4513883595351,7.63401541462695));
#185637=CARTESIAN_POINT('Ctrl Pts',(19.9415771187918,17.471815873412,7.63173714904231));
#185638=CARTESIAN_POINT('Ctrl Pts',(19.9770746693954,17.4973750946249,7.62904597482545));
#185639=CARTESIAN_POINT('Ctrl Pts',(19.983121743143,17.5017780060331,7.62858780921532));
#185640=CARTESIAN_POINT('Ctrl Pts',(19.9924972828569,17.5086807251005,7.62787806080525));
#185641=CARTESIAN_POINT('Ctrl Pts',(19.9958418576696,17.5111584039757,7.62762498986248));
#185642=CARTESIAN_POINT('Ctrl Pts',(20.0020378979272,17.5157768280971,7.62715641797254));
#185643=CARTESIAN_POINT('Ctrl Pts',(20.004891235833,17.5179148928367,7.62694074215626));
#185644=CARTESIAN_POINT('Ctrl Pts',(20.0113386264253,17.5227715378399,7.62645362944522));
#185645=CARTESIAN_POINT('Ctrl Pts',(20.014929399265,17.5254943838816,7.62618249647196));
#185646=CARTESIAN_POINT('Ctrl Pts',(20.0257620281744,17.5337632652889,7.62536492688483));
#185647=CARTESIAN_POINT('Ctrl Pts',(20.0329768693489,17.5393447420737,7.62482092260802));
#185648=CARTESIAN_POINT('Ctrl Pts',(20.0884419541667,17.5828290430669,7.62064090594019));
#185649=CARTESIAN_POINT('Ctrl Pts',(20.13506466225,17.6227704920059,7.61713931927677));
#185650=CARTESIAN_POINT('Ctrl Pts',(20.2871628311835,17.7649907104421,7.60550236185031));
#185651=CARTESIAN_POINT('Ctrl Pts',(20.3837105533619,17.8761901608859,7.59771483652045));
#185652=CARTESIAN_POINT('Ctrl Pts',(20.5211889403105,18.0724706617717,7.58451615750585));
#185653=CARTESIAN_POINT('Ctrl Pts',(20.5693478086943,18.1518546352064,7.57930758455341));
#185654=CARTESIAN_POINT('Ctrl Pts',(20.621868403324,18.2528319295006,7.57267773426654));
#185655=CARTESIAN_POINT('Ctrl Pts',(20.6313132485968,18.2716728210836,7.5714408340411));
#185656=CARTESIAN_POINT('Ctrl Pts',(20.6443685774546,18.2987165409098,7.56966428107178));
#185657=CARTESIAN_POINT('Ctrl Pts',(20.6482108964007,18.3068065186023,7.56913269454303));
#185658=CARTESIAN_POINT('Ctrl Pts',(20.6547601013541,18.3208246798685,7.56821122626327));
#185659=CARTESIAN_POINT('Ctrl Pts',(20.6574911809295,18.3267414727883,7.56782218713267));
#185660=CARTESIAN_POINT('Ctrl Pts',(20.6626743495707,18.3381082724853,7.56707455997072));
#185661=CARTESIAN_POINT('Ctrl Pts',(20.6651307685882,18.3435562449766,7.56671612569652));
#185662=CARTESIAN_POINT('Ctrl Pts',(20.6714718677267,18.3577802910612,7.56577998228425));
#185663=CARTESIAN_POINT('Ctrl Pts',(20.675319962232,18.3665724368256,7.56520102638198));
#185664=CARTESIAN_POINT('Ctrl Pts',(20.6883056100073,18.3968000533151,7.56320933012567));
#185665=CARTESIAN_POINT('Ctrl Pts',(20.6971487157824,18.4183594622264,7.56178664714834));
#185666=CARTESIAN_POINT('Ctrl Pts',(20.767889126694,18.5992738699959,7.54982639601299));
#185667=CARTESIAN_POINT('Ctrl Pts',(20.8106187325848,18.7654141573428,7.5386255028857));
#185668=CARTESIAN_POINT('Ctrl Pts',(20.8446806213586,19.0242991131105,7.5213705177817));
#185669=CARTESIAN_POINT('Ctrl Pts',(20.850720229395,19.1144216858848,7.51541595429194));
#185670=CARTESIAN_POINT('Ctrl Pts',(20.8511061913673,19.2432841143112,7.50718301448861));
#185671=CARTESIAN_POINT('Ctrl Pts',(20.8501647886522,19.2819077673746,7.50475210883007));
#185672=CARTESIAN_POINT('Ctrl Pts',(20.847772964345,19.3280934375659,7.50190596508729));
#185673=CARTESIAN_POINT('Ctrl Pts',(20.8473379745091,19.335698145387,7.50143930989417));
#185674=CARTESIAN_POINT('Ctrl Pts',(20.8465999622099,19.34748433243,7.50071930156148));
#185675=CARTESIAN_POINT('Ctrl Pts',(20.8463255532801,19.3516674482284,7.50046439151679));
#185676=CARTESIAN_POINT('Ctrl Pts',(20.8457949338566,19.3594043526174,7.49999412722952));
#185677=CARTESIAN_POINT('Ctrl Pts',(20.8455421795424,19.3629582799989,7.49977858728144));
#185678=CARTESIAN_POINT('Ctrl Pts',(20.8449522826184,19.3709669272546,7.49929393457597));
#185679=CARTESIAN_POINT('Ctrl Pts',(20.8446100118803,19.3754212148685,7.49902511257149));
#185680=CARTESIAN_POINT('Ctrl Pts',(20.8435638821703,19.3884936438664,7.4982382441403));
#185681=CARTESIAN_POINT('Ctrl Pts',(20.842821310256,19.3971087149146,7.49772231902875));
#185682=CARTESIAN_POINT('Ctrl Pts',(20.8372749144414,19.4571538914986,7.49414336576038));
#185683=CARTESIAN_POINT('Ctrl Pts',(20.8306425576144,19.508402124951,7.49117532414625));
#185684=CARTESIAN_POINT('Ctrl Pts',(20.818558109384,19.5808386602369,7.48703943721064));
#185685=CARTESIAN_POINT('Ctrl Pts',(20.8146437154506,19.6022606810319,7.48582377884594));
#185686=CARTESIAN_POINT('Ctrl Pts',(20.8014014616075,19.6688989338518,7.48205537020718));
#185687=CARTESIAN_POINT('Ctrl Pts',(20.7909245083259,19.7138737909944,7.47953089308716));
#185688=CARTESIAN_POINT('Ctrl Pts',(20.7507051736267,19.8641062288232,7.47106355087913));
#185689=CARTESIAN_POINT('Ctrl Pts',(20.7142829559303,19.9673901340052,7.46517520783333));
#185690=CARTESIAN_POINT('Ctrl Pts',(20.6477507209412,20.1177993070939,7.45603028383809));
#185691=CARTESIAN_POINT('Ctrl Pts',(20.62349585473,20.1673114422871,7.45292243056156));
#185692=CARTESIAN_POINT('Ctrl Pts',(20.5810528881634,20.2460177949139,7.44777791150813));
#185693=CARTESIAN_POINT('Ctrl Pts',(20.5640366640107,20.2758153920733,7.44578064358734));
#185694=CARTESIAN_POINT('Ctrl Pts',(20.5407177382325,20.3144386498558,7.4431198179861));
#185695=CARTESIAN_POINT('Ctrl Pts',(20.5350602042157,20.3236490793917,7.442479792659));
#185696=CARTESIAN_POINT('Ctrl Pts',(20.5256770236963,20.338665743276,7.44142706254048));
#185697=CARTESIAN_POINT('Ctrl Pts',(20.5219930483793,20.3444978795811,7.44101589916724));
#185698=CARTESIAN_POINT('Ctrl Pts',(20.5148057905447,20.3557538716646,7.44021782827049));
#185699=CARTESIAN_POINT('Ctrl Pts',(20.5113060651358,20.3611799162423,7.43983105615398));
#185700=CARTESIAN_POINT('Ctrl Pts',(20.5031665828489,20.373673678029,7.43893568881556));
#185701=CARTESIAN_POINT('Ctrl Pts',(20.4985092233637,20.38072974523,7.43842643751659));
#185702=CARTESIAN_POINT('Ctrl Pts',(20.4858668726533,20.3996360446069,7.43705217043222));
#185703=CARTESIAN_POINT('Ctrl Pts',(20.4778040668347,20.4114334828779,7.43618422685429));
#185704=CARTESIAN_POINT('Ctrl Pts',(20.4027425062564,20.5189108887095,7.42817964133331));
#185705=CARTESIAN_POINT('Ctrl Pts',(20.3280628889221,20.6089585661001,7.4207414564302));
#185706=CARTESIAN_POINT('Ctrl Pts',(20.1325800255432,20.8085286218215,7.40249413492387));
#185707=CARTESIAN_POINT('Ctrl Pts',(20.0058104253225,20.9111829546335,7.39154528262807));
#185708=CARTESIAN_POINT('Ctrl Pts',(19.840960471985,21.0158254276689,7.37913629671011));
#185709=CARTESIAN_POINT('Ctrl Pts',(19.8129750421383,21.0326941130961,7.37708847206117));
#185710=CARTESIAN_POINT('Ctrl Pts',(19.7783138738562,21.0525075630719,7.37463334315315));
#185711=CARTESIAN_POINT('Ctrl Pts',(19.7720005465251,21.0560735597522,7.37418938613217));
#185712=CARTESIAN_POINT('Ctrl Pts',(19.7620781518832,21.0616110404315,7.37349683595615));
#185713=CARTESIAN_POINT('Ctrl Pts',(19.7584815188524,21.0636045254023,7.37324686678025));
#185714=CARTESIAN_POINT('Ctrl Pts',(19.7517502342958,21.0673098384949,7.37278105434074));
#185715=CARTESIAN_POINT('Ctrl Pts',(19.7486170936688,21.0690241950441,7.37256505471529));
#185716=CARTESIAN_POINT('Ctrl Pts',(19.7414581716295,21.0729178251686,7.37207336199177));
#185717=CARTESIAN_POINT('Ctrl Pts',(19.7374296588107,21.0750919709032,7.37179799684584));
#185718=CARTESIAN_POINT('Ctrl Pts',(19.7250361318013,21.0817288080202,7.37095480790449));
#185719=CARTESIAN_POINT('Ctrl Pts',(19.7166480329933,21.0861484577258,7.37038964621793));
#185720=CARTESIAN_POINT('Ctrl Pts',(19.600814257824,21.146189999056,7.36265694598139));
#185721=CARTESIAN_POINT('Ctrl Pts',(19.4888059933062,21.192565989635,7.35601945123444));
#185722=CARTESIAN_POINT('Ctrl Pts',(19.2028080485743,21.2831834214849,7.33969349807363));
#185723=CARTESIAN_POINT('Ctrl Pts',(19.0260365066536,21.3153841779623,7.3300748064758));
#185724=CARTESIAN_POINT('Ctrl Pts',(18.825876394855,21.3261144537818,7.31840383786235));
#185725=CARTESIAN_POINT('Ctrl Pts',(18.8044107518769,21.326937782776,7.31714348267743));
#185726=CARTESIAN_POINT('Ctrl Pts',(18.7739144161655,21.3276429286495,7.31533909279303));
#185727=CARTESIAN_POINT('Ctrl Pts',(18.7648908388861,21.3277938492569,7.31480347927301));
#185728=CARTESIAN_POINT('Ctrl Pts',(18.7493378589372,21.3279545059123,7.31387724462313));
#185729=CARTESIAN_POINT('Ctrl Pts',(18.7428088206236,21.3279917414165,7.31348748994748));
#185730=CARTESIAN_POINT('Ctrl Pts',(18.7303180282448,21.3280051925998,7.31274003109429));
#185731=CARTESIAN_POINT('Ctrl Pts',(18.72435633362,21.3279864290967,7.31238248810251));
#185732=CARTESIAN_POINT('Ctrl Pts',(18.7088771927129,21.3278723237779,7.31145206210931));
#185733=CARTESIAN_POINT('Ctrl Pts',(18.6993602462742,21.3277379794054,7.31087796217541));
#185734=CARTESIAN_POINT('Ctrl Pts',(18.6670303154439,21.3270635107927,7.30892054943378));
#185735=CARTESIAN_POINT('Ctrl Pts',(18.644225905441,21.3262187282526,7.3075277502134));
#185736=CARTESIAN_POINT('Ctrl Pts',(18.443924244538,21.3155537144721,7.29518344662956));
#185737=CARTESIAN_POINT('Ctrl Pts',(18.2683373114805,21.2837817564082,7.28350739668497));
#185738=CARTESIAN_POINT('Ctrl Pts',(18.0173334272621,21.2048344707143,7.26612445155826));
#185739=CARTESIAN_POINT('Ctrl Pts',(17.9374623963021,21.1742922843585,7.26049814855331));
#185740=CARTESIAN_POINT('Ctrl Pts',(17.8255729331779,21.1235505079833,7.25265695315812));
#185741=CARTESIAN_POINT('Ctrl Pts',(17.7919077536558,21.1071940245427,7.2503038307596));
#185742=CARTESIAN_POINT('Ctrl Pts',(17.7519919185655,21.0864749020348,7.24753652703278));
#185743=CARTESIAN_POINT('Ctrl Pts',(17.7453107277643,21.082961406406,7.24707411322727));
#185744=CARTESIAN_POINT('Ctrl Pts',(17.7349616588027,21.0774481889057,7.24635922919027));
#185745=CARTESIAN_POINT('Ctrl Pts',(17.7312807434323,21.075473261341,7.24610523657316));
#185746=CARTESIAN_POINT('Ctrl Pts',(17.7244699968971,21.0717930771755,7.24563582142066));
#185747=CARTESIAN_POINT('Ctrl Pts',(17.7213386542546,21.0700908268173,7.24542021857355));
#185748=CARTESIAN_POINT('Ctrl Pts',(17.7142752472196,21.0662278990293,7.24493436089347));
#185749=CARTESIAN_POINT('Ctrl Pts',(17.7103457545654,21.0640626312742,7.24466440328963));
#185750=CARTESIAN_POINT('Ctrl Pts',(17.6987856650467,21.0576446844923,7.24387111611506));
#185751=CARTESIAN_POINT('Ctrl Pts',(17.6911743656914,21.0533571891559,7.24334996011801));
#185752=CARTESIAN_POINT('Ctrl Pts',(17.6369037098926,21.0223420881912,7.23964067176655));
#185753=CARTESIAN_POINT('Ctrl Pts',(17.5912469084544,20.9938900257312,7.23655556861603));
#185754=CARTESIAN_POINT('Ctrl Pts',(17.4071719361634,20.869199431522,7.2240564880901));
#185755=CARTESIAN_POINT('Ctrl Pts',(17.2794064816617,20.758340788342,7.21518661704685));
#185756=CARTESIAN_POINT('Ctrl Pts',(17.1115464622912,20.5733265776952,7.20134223797042));
#185757=CARTESIAN_POINT('Ctrl Pts',(17.0604711026317,20.5100720264524,7.19675113267809));
#185758=CARTESIAN_POINT('Ctrl Pts',(17.001725980964,20.4280871239444,7.19086728302855));
#185759=CARTESIAN_POINT('Ctrl Pts',(16.9905151956153,20.4119725404251,7.18971399732614));
#185760=CARTESIAN_POINT('Ctrl Pts',(16.9746597429538,20.3884916612127,7.18803704947961));
#185761=CARTESIAN_POINT('Ctrl Pts',(16.9698336758503,20.3812486614289,7.1875202499984));
#185762=CARTESIAN_POINT('Ctrl Pts',(16.9614964370298,20.3685672856567,7.18661614934196));
#185763=CARTESIAN_POINT('Ctrl Pts',(16.9579652675324,20.3631421479998,7.1862296043861));
#185764=CARTESIAN_POINT('Ctrl Pts',(16.9511894718605,20.3526269340715,7.18548079708145));
#185765=CARTESIAN_POINT('Ctrl Pts',(16.9479416216304,20.3475390022895,7.18511865992843));
#185766=CARTESIAN_POINT('Ctrl Pts',(16.9402801549648,20.3354229593679,7.18425669190227));
#185767=CARTESIAN_POINT('Ctrl Pts',(16.9358860431447,20.3283826869616,7.18375614515876));
#185768=CARTESIAN_POINT('Ctrl Pts',(16.9204543794961,20.3033312277729,7.18197604682077));
#185769=CARTESIAN_POINT('Ctrl Pts',(16.9096454194235,20.2851813358992,7.18068816509537));
#185770=CARTESIAN_POINT('Ctrl Pts',(16.8384380874289,20.1614376846218,7.171916957869));
#185771=CARTESIAN_POINT('Ctrl Pts',(16.7870403045226,20.0510965155842,7.16412180665666));
#185772=CARTESIAN_POINT('Ctrl Pts',(16.7454193167441,19.9371100923285,7.15616136059514));
#185773=CARTESIAN_POINT('',(16.620191220251,19.2105385357295,7.68893962574679));
#185774=CARTESIAN_POINT('Ctrl Pts',(16.6203930058439,19.2105314190313,7.68905589348729));
#185775=CARTESIAN_POINT('Ctrl Pts',(16.6197601561406,18.8850442238484,7.66955339595354));
#185776=CARTESIAN_POINT('Ctrl Pts',(16.8436653936273,17.852883318867,7.60765896285932));
#185777=CARTESIAN_POINT('Ctrl Pts',(18.4531255372358,16.7235436104772,7.50337259420462));
#185778=CARTESIAN_POINT('Ctrl Pts',(20.6735251555922,17.6284160608558,7.3761967875232));
#185779=CARTESIAN_POINT('Ctrl Pts',(21.1145308242001,19.9852110491624,7.24902098084175));
#185780=CARTESIAN_POINT('Ctrl Pts',(19.3715472140107,21.6317154528194,7.12184517416032));
#185781=CARTESIAN_POINT('Ctrl Pts',(17.4471161472743,21.1569083566678,7.0167110424149));
#185782=CARTESIAN_POINT('Ctrl Pts',(16.8648290560492,20.2551146180475,6.95396884622995));
#185783=CARTESIAN_POINT('Ctrl Pts',(16.7486737101886,19.9359290495398,6.93361858560548));
#185784=CARTESIAN_POINT('Ctrl Pts',(16.6170000287534,19.2106510846316,7.68710087888888));
#185785=CARTESIAN_POINT('Ctrl Pts',(16.6169985639082,19.2195388482347,7.68762144435747));
#185786=CARTESIAN_POINT('Ctrl Pts',(16.6170530690843,19.2284264531445,7.68814369819107));
#185787=CARTESIAN_POINT('Ctrl Pts',(16.6172707415968,19.2459375900539,7.68917616888034));
#185788=CARTESIAN_POINT('Ctrl Pts',(16.6174306467683,19.2545609712539,7.6896862739212));
#185789=CARTESIAN_POINT('Ctrl Pts',(16.6177963854112,19.2693940177211,7.69056666315363));
#185790=CARTESIAN_POINT('Ctrl Pts',(16.6179768690834,19.2756042403467,7.69093615259663));
#185791=CARTESIAN_POINT('Ctrl Pts',(16.6183911393839,19.2879820933756,7.69167441523271));
#185792=CARTESIAN_POINT('Ctrl Pts',(16.6186245666227,19.2941496748977,7.69204317358488));
#185793=CARTESIAN_POINT('Ctrl Pts',(16.6191442764776,19.3064570434667,7.69278085951651));
#185794=CARTESIAN_POINT('Ctrl Pts',(16.6194303341968,19.3125967799123,7.69314977649579));
#185795=CARTESIAN_POINT('Ctrl Pts',(16.6202771216571,19.3292146291735,7.69415079514975));
#185796=CARTESIAN_POINT('Ctrl Pts',(16.6208890187398,19.3396898583877,7.69478449629605));
#185797=CARTESIAN_POINT('Ctrl Pts',(16.6234852736182,19.3791005045457,7.69717906122481));
#185798=CARTESIAN_POINT('Ctrl Pts',(16.6259862430463,19.4079976126318,7.69895602824457));
#185799=CARTESIAN_POINT('Ctrl Pts',(16.6474323195092,19.6078897788231,7.71140096947303));
#185800=CARTESIAN_POINT('Ctrl Pts',(16.6865492345595,19.7758840172537,7.7227154079209));
#185801=CARTESIAN_POINT('Ctrl Pts',(16.7454193726886,19.9371102455424,7.73405220823978));
#185802=CARTESIAN_POINT('Origin',(18.734,19.211,0.));
#185803=CARTESIAN_POINT('',(16.7454192421517,19.937109888044,8.75434672885778));
#185804=CARTESIAN_POINT('',(16.7454193934539,19.9371103024118,8.53521106676425));
#185805=CARTESIAN_POINT('',(16.7454193623258,19.9371102171621,0.));
#185806=CARTESIAN_POINT('Ctrl Pts',(16.7454192421517,19.937109888044,8.75434672885778));
#185807=CARTESIAN_POINT('Ctrl Pts',(16.7157810170557,19.8559403500813,8.7495860167213));
#185808=CARTESIAN_POINT('Ctrl Pts',(16.6911130986906,19.7729578545092,8.74492439956724));
#185809=CARTESIAN_POINT('Ctrl Pts',(16.6409703545629,19.5564352327739,8.7328222373515));
#185810=CARTESIAN_POINT('Ctrl Pts',(16.6231411496415,19.4216337344176,8.72532551982903));
#185811=CARTESIAN_POINT('Ctrl Pts',(16.6177334388092,19.2692153742373,8.71640094755641));
#185812=CARTESIAN_POINT('Ctrl Pts',(16.6173369769536,19.2523619417785,8.71540844565238));
#185813=CARTESIAN_POINT('Ctrl Pts',(16.6170471059452,19.2273224546209,8.71392475548325));
#185814=CARTESIAN_POINT('Ctrl Pts',(16.6169998255527,19.2191385925516,8.71343838487837));
#185815=CARTESIAN_POINT('Ctrl Pts',(16.6170001372476,19.20455648059,8.71256911172884));
#185816=CARTESIAN_POINT('Ctrl Pts',(16.6170292805018,19.1981583009378,8.71218679202135));
#185817=CARTESIAN_POINT('Ctrl Pts',(16.6171518843134,19.1846683310924,8.71137874831071));
#185818=CARTESIAN_POINT('Ctrl Pts',(16.6172519794828,19.1775766936962,8.71095282096323));
#185819=CARTESIAN_POINT('Ctrl Pts',(16.6176113756871,19.1588005197579,8.70982203094684));
#185820=CARTESIAN_POINT('Ctrl Pts',(16.6179318028125,19.1471175209732,8.70911526177061));
#185821=CARTESIAN_POINT('Ctrl Pts',(16.6198779961695,19.092626327482,8.70580361777299));
#185822=CARTESIAN_POINT('Ctrl Pts',(16.6227060712719,19.0498736487773,8.70316137440709));
#185823=CARTESIAN_POINT('Ctrl Pts',(16.6340979484588,18.932066147754,8.69575359139213));
#185824=CARTESIAN_POINT('Ctrl Pts',(16.6453836934642,18.8573438162893,8.69090977847032));
#185825=CARTESIAN_POINT('Ctrl Pts',(16.6865619342682,18.6576816958607,8.67762193719792));
#185826=CARTESIAN_POINT('Ctrl Pts',(16.7238651788393,18.534597802203,8.66904374240272));
#185827=CARTESIAN_POINT('Ctrl Pts',(16.7783252999815,18.4002587320868,8.65959211326805));
#185828=CARTESIAN_POINT('Ctrl Pts',(16.7847471862453,18.3849380020785,8.6585131872796));
#185829=CARTESIAN_POINT('Ctrl Pts',(16.8125068533598,18.3208384232824,8.65399898077157));
#185830=CARTESIAN_POINT('Ctrl Pts',(16.835502363072,18.2727935733103,8.65061472031495));
#185831=CARTESIAN_POINT('Ctrl Pts',(16.8643428399077,18.2179506392627,8.64679236635273));
#185832=CARTESIAN_POINT('Ctrl Pts',(16.8684462209151,18.2102632551545,8.64625754915743));
#185833=CARTESIAN_POINT('Ctrl Pts',(16.8747318686502,18.1986605794638,8.64545206171907));
#185834=CARTESIAN_POINT('Ctrl Pts',(16.8768792380025,18.1947266298691,8.64517925828317));
#185835=CARTESIAN_POINT('Ctrl Pts',(16.8807565432377,18.1876767906512,8.64469096367063));
#185836=CARTESIAN_POINT('Ctrl Pts',(16.8824818607172,18.1845584374576,8.64447518482431));
#185837=CARTESIAN_POINT('Ctrl Pts',(16.8862483287793,18.1777912889107,8.64400738000286));
#185838=CARTESIAN_POINT('Ctrl Pts',(16.888292409414,18.1741441903925,8.64375554540963));
#185839=CARTESIAN_POINT('Ctrl Pts',(16.8940655214934,18.1639148336062,8.64304993504256));
#185840=CARTESIAN_POINT('Ctrl Pts',(16.8978190937605,18.1573463973602,8.64259770746247));
#185841=CARTESIAN_POINT('Ctrl Pts',(16.920491720224,18.1181603300801,8.63990408020139));
#185842=CARTESIAN_POINT('Ctrl Pts',(16.9402455404157,18.0860305961332,8.63771329206219));
#185843=CARTESIAN_POINT('Ctrl Pts',(17.0081342721693,17.9819483347955,8.6306175892307));
#185844=CARTESIAN_POINT('Ctrl Pts',(17.0598254413951,17.9124152229069,8.62587709572191));
#185845=CARTESIAN_POINT('Ctrl Pts',(17.2291734117859,17.7115983654371,8.61158244377948));
#185846=CARTESIAN_POINT('Ctrl Pts',(17.359056748435,17.5916690556861,8.60211687411541));
#185847=CARTESIAN_POINT('Ctrl Pts',(17.5209475325225,17.4758575769542,8.59054984392107));
#185848=CARTESIAN_POINT('Ctrl Pts',(17.5398251272281,17.4628118437123,8.58920550140768));
#185849=CARTESIAN_POINT('Ctrl Pts',(17.5668448509374,17.4447812011437,8.58728581481007));
#185850=CARTESIAN_POINT('Ctrl Pts',(17.5748147779222,17.4395402618726,8.58672011599731));
#185851=CARTESIAN_POINT('Ctrl Pts',(17.5878261804781,17.4311095082105,8.58579734116235));
#185852=CARTESIAN_POINT('Ctrl Pts',(17.5928462560111,17.4278867902518,8.58544149819128));
#185853=CARTESIAN_POINT('Ctrl Pts',(17.6033863121168,17.4211831727129,8.58469472588016));
#185854=CARTESIAN_POINT('Ctrl Pts',(17.608908893192,17.4177064974271,8.58430364495242));
#185855=CARTESIAN_POINT('Ctrl Pts',(17.6220914791847,17.4094924203722,8.58337054817236));
#185856=CARTESIAN_POINT('Ctrl Pts',(17.6297657685229,17.4047782870772,8.58282768260985));
#185857=CARTESIAN_POINT('Ctrl Pts',(17.6557517782801,17.3890432085181,8.58099047340844));
#185858=CARTESIAN_POINT('Ctrl Pts',(17.6741997808944,17.3782509116931,8.57968783918529));
#185859=CARTESIAN_POINT('Ctrl Pts',(17.7757285137036,17.3209009128484,8.57252536000152));
#185860=CARTESIAN_POINT('Ctrl Pts',(17.861704493767,17.279716716662,8.56647648154496));
#185861=CARTESIAN_POINT('Ctrl Pts',(18.1086082070268,17.1813024573805,8.54920487185127));
#185862=CARTESIAN_POINT('Ctrl Pts',(18.2741081412925,17.137528675116,8.53769527547674));
#185863=CARTESIAN_POINT('Ctrl Pts',(18.4795040648143,17.109030822944,8.52446033264503));
#185864=CARTESIAN_POINT('Ctrl Pts',(18.516074543654,17.1049251022296,8.52214603687204));
#185865=CARTESIAN_POINT('Ctrl Pts',(18.5598517151202,17.1011629484618,8.51944028791996));
#185866=CARTESIAN_POINT('Ctrl Pts',(18.5669707224031,17.1005874259013,8.51900231736309));
#185867=CARTESIAN_POINT('Ctrl Pts',(18.5785921108759,17.0997070905289,8.51829082567716));
#185868=CARTESIAN_POINT('Ctrl Pts',(18.5830927276043,17.0993806314596,8.51801613495573));
#185869=CARTESIAN_POINT('Ctrl Pts',(18.5911518306737,17.0988219495888,8.51752581653014));
#185870=CARTESIAN_POINT('Ctrl Pts',(18.5947098785228,17.0985843262311,8.51730989063227));
#185871=CARTESIAN_POINT('Ctrl Pts',(18.602417861842,17.0980891101583,8.51684330903261));
#185872=CARTESIAN_POINT('Ctrl Pts',(18.6065679477215,17.0978347532129,8.51659283640032));
#185873=CARTESIAN_POINT('Ctrl Pts',(18.6181656265467,17.097158226854,8.5158948791704));
#185874=CARTESIAN_POINT('Ctrl Pts',(18.6256148258465,17.0967631869273,8.51544888925012));
#185875=CARTESIAN_POINT('Ctrl Pts',(18.6689433369407,17.0946950265628,8.51286739279311));
#185876=CARTESIAN_POINT('Ctrl Pts',(18.7048607989835,17.0938957600832,8.51077771975786));
#185877=CARTESIAN_POINT('Ctrl Pts',(18.8205156815905,17.0942663562862,8.50416137048909));
#185878=CARTESIAN_POINT('Ctrl Pts',(18.9001762731438,17.0990261098268,8.4997747462917));
#185879=CARTESIAN_POINT('Ctrl Pts',(19.1643338362318,17.1298526834424,8.48527478373422));
#185880=CARTESIAN_POINT('Ctrl Pts',(19.345606585014,17.1757376606257,8.47531866330219));
#185881=CARTESIAN_POINT('Ctrl Pts',(19.5390168233056,17.2529083166128,8.46320680919834));
#185882=CARTESIAN_POINT('Ctrl Pts',(19.5593656917881,17.2613983618914,8.46191427765178));
#185883=CARTESIAN_POINT('Ctrl Pts',(19.5873241350491,17.2735794678152,8.4601115200669));
#185884=CARTESIAN_POINT('Ctrl Pts',(19.5950502078706,17.2770007925624,8.45961047305527));
#185885=CARTESIAN_POINT('Ctrl Pts',(19.6082959568594,17.2829614908691,8.45874643214269));
#185886=CARTESIAN_POINT('Ctrl Pts',(19.613825602712,17.2854785588051,8.45838420642187));
#185887=CARTESIAN_POINT('Ctrl Pts',(19.6252035291611,17.2907169798876,8.45763571096));
#185888=CARTESIAN_POINT('Ctrl Pts',(19.6310503546376,17.2934413261813,8.45724934083109));
#185889=CARTESIAN_POINT('Ctrl Pts',(19.6446284388797,17.2998437671049,8.4563479781304));
#185890=CARTESIAN_POINT('Ctrl Pts',(19.6523499770234,17.3035421062137,8.4558322873104));
#185891=CARTESIAN_POINT('Ctrl Pts',(19.6769967860088,17.3155313866904,8.4541761279058));
#185892=CARTESIAN_POINT('Ctrl Pts',(19.6938334934141,17.3240013695471,8.45302943476264));
#185893=CARTESIAN_POINT('Ctrl Pts',(19.7773918526518,17.3674444097246,8.44725987905308));
#185894=CARTESIAN_POINT('Ctrl Pts',(19.8423195681874,17.4057328901836,8.44252062808619));
#185895=CARTESIAN_POINT('Ctrl Pts',(19.9960048664068,17.5077825723649,8.43066534842997));
#185896=CARTESIAN_POINT('Ctrl Pts',(20.0821329796339,17.5751088404482,8.42344948268122));
#185897=CARTESIAN_POINT('Ctrl Pts',(20.1730469185298,17.6582507056954,8.4153109194896));
#185898=CARTESIAN_POINT('Ctrl Pts',(20.1833205019861,17.6678355596029,8.41438324490779));
#185899=CARTESIAN_POINT('Ctrl Pts',(20.2693745607069,17.7497380859648,8.40654865238302));
#185900=CARTESIAN_POINT('Ctrl Pts',(20.3397961775604,17.8274952925357,8.39970425921115));
#185901=CARTESIAN_POINT('Ctrl Pts',(20.4101292728072,17.9177971998412,8.39263247832015));
#185902=CARTESIAN_POINT('Ctrl Pts',(20.4160287886,17.9254798780245,8.39203733616778));
#185903=CARTESIAN_POINT('Ctrl Pts',(20.4246627373285,17.9368846863119,8.39116375664565));
#185904=CARTESIAN_POINT('Ctrl Pts',(20.4274379581797,17.9405755800935,8.39088255902664));
#185905=CARTESIAN_POINT('Ctrl Pts',(20.43234052854,17.9471403427675,8.39038513719908));
#185906=CARTESIAN_POINT('Ctrl Pts',(20.4344726942659,17.9500105469131,8.39016857867322));
#185907=CARTESIAN_POINT('Ctrl Pts',(20.4390259579952,17.9561724505841,8.3897056394285));
#185908=CARTESIAN_POINT('Ctrl Pts',(20.4414447939497,17.9594657525763,8.38945941528889));
#185909=CARTESIAN_POINT('Ctrl Pts',(20.4480596526018,17.9685269092461,8.38878518002722));
#185910=CARTESIAN_POINT('Ctrl Pts',(20.4522361292553,17.9743090598927,8.38835850311727));
#185911=CARTESIAN_POINT('Ctrl Pts',(20.4743984684497,18.0053208609879,8.38608843904006));
#185912=CARTESIAN_POINT('Ctrl Pts',(20.4918590539263,18.030923396526,8.3842789219611));
#185913=CARTESIAN_POINT('Ctrl Pts',(20.5979130315293,18.1940113308806,8.37308987090836));
#185914=CARTESIAN_POINT('Ctrl Pts',(20.6708945644685,18.3410060131363,8.36444575549577));
#185915=CARTESIAN_POINT('Ctrl Pts',(20.7660370281603,18.6057165134807,8.34905100060105));
#185916=CARTESIAN_POINT('Ctrl Pts',(20.7965363340944,18.7195927261857,8.34248309119627));
#185917=CARTESIAN_POINT('Ctrl Pts',(20.8199519706694,18.8494783661356,8.33475140450648));
#185918=CARTESIAN_POINT('Ctrl Pts',(20.8223464956857,18.8635774694906,8.33390925781615));
#185919=CARTESIAN_POINT('Ctrl Pts',(20.825929558127,18.8860519121019,8.33256184678198));
#185920=CARTESIAN_POINT('Ctrl Pts',(20.8272110876084,18.8944121361446,8.33205952938785));
#185921=CARTESIAN_POINT('Ctrl Pts',(20.8293826154467,18.9091682715513,8.33117089933053));
#185922=CARTESIAN_POINT('Ctrl Pts',(20.8302935176405,18.9155610318745,8.33078525374142));
#185923=CARTESIAN_POINT('Ctrl Pts',(20.8321168089426,18.9287901080542,8.32998578581025));
#185924=CARTESIAN_POINT('Ctrl Pts',(20.8330250654306,18.935626907592,8.32957183765141));
#185925=CARTESIAN_POINT('Ctrl Pts',(20.8352702089983,18.9531837575925,8.32850675969558));
#185926=CARTESIAN_POINT('Ctrl Pts',(20.8365584644048,18.963909726905,8.32785410279159));
#185927=CARTESIAN_POINT('Ctrl Pts',(20.8415891915576,19.0086875503363,8.32512093933148));
#185928=CARTESIAN_POINT('Ctrl Pts',(20.8445867801644,19.042816303812,8.32301716319151));
#185929=CARTESIAN_POINT('Ctrl Pts',(20.8502361087326,19.1318891338896,8.31746970197765));
#185930=CARTESIAN_POINT('Ctrl Pts',(20.8515768176137,19.1868877189968,8.31398775225973));
#185931=CARTESIAN_POINT('Ctrl Pts',(20.8491808393078,19.3511675712616,8.30342808394179));
#185932=CARTESIAN_POINT('Ctrl Pts',(20.8391244680064,19.4601674877784,8.29620194200463));
#185933=CARTESIAN_POINT('Ctrl Pts',(20.8141428443948,19.6062308953486,8.28641310355518));
#185934=CARTESIAN_POINT('Ctrl Pts',(20.8065306075094,19.644380549066,8.28384781553478));
#185935=CARTESIAN_POINT('Ctrl Pts',(20.7916044183325,19.7097439602419,8.27945625055897));
#185936=CARTESIAN_POINT('Ctrl Pts',(20.784790282331,19.7370615832903,8.27762202758441));
#185937=CARTESIAN_POINT('Ctrl Pts',(20.7636571585287,19.8151189270608,8.27239776714489));
#185938=CARTESIAN_POINT('Ctrl Pts',(20.7479841263705,19.8654744474717,8.26904797779021));
#185939=CARTESIAN_POINT('Ctrl Pts',(20.7275548222699,19.9233929477802,8.26525958796411));
#185940=CARTESIAN_POINT('Ctrl Pts',(20.7246131989483,19.9315717449132,8.26472615454234));
#185941=CARTESIAN_POINT('Ctrl Pts',(20.7200801154302,19.9439357534643,8.26392233435536));
#185942=CARTESIAN_POINT('Ctrl Pts',(20.718525653361,19.9481342995805,8.26364982731118));
#185943=CARTESIAN_POINT('Ctrl Pts',(20.7157100019476,19.9556658088046,8.26316184887843));
#185944=CARTESIAN_POINT('Ctrl Pts',(20.7144537117193,19.9590005313757,8.26294609147541));
#185945=CARTESIAN_POINT('Ctrl Pts',(20.7117038744118,19.9662442620297,8.26247808702039));
#185946=CARTESIAN_POINT('Ctrl Pts',(20.7102071607625,19.9701520062799,8.26222603268439));
#185947=CARTESIAN_POINT('Ctrl Pts',(20.7059659163146,19.9811278559652,8.26151918508505));
#185948=CARTESIAN_POINT('Ctrl Pts',(20.7031949538382,19.9881857740329,8.26106594874796));
#185949=CARTESIAN_POINT('Ctrl Pts',(20.6863067963199,20.0305313740432,8.25835358695102));
#185950=CARTESIAN_POINT('Ctrl Pts',(20.6712783760478,20.0654509339158,8.25614589577525));
#185951=CARTESIAN_POINT('Ctrl Pts',(20.6184747587762,20.1795772223817,8.24896765860186));
#185952=CARTESIAN_POINT('Ctrl Pts',(20.5767150514121,20.2568444580941,8.24416593257567));
#185953=CARTESIAN_POINT('Ctrl Pts',(20.4379674414183,20.4793105260659,8.22990246545836));
#185954=CARTESIAN_POINT('Ctrl Pts',(20.3277314422174,20.6153254519113,8.22051951224964));
#185955=CARTESIAN_POINT('Ctrl Pts',(20.1854463175807,20.7522737337603,8.20904488838432));
#185956=CARTESIAN_POINT('Ctrl Pts',(20.1685661699803,20.7679974237718,8.20769350237637));
#185957=CARTESIAN_POINT('Ctrl Pts',(20.1443329418042,20.789841779301,8.20576548130794));
#185958=CARTESIAN_POINT('Ctrl Pts',(20.1371897818766,20.7961936166559,8.20519860740392));
#185959=CARTESIAN_POINT('Ctrl Pts',(20.1255165097517,20.8064329925923,8.20427443936026));
#185960=CARTESIAN_POINT('Ctrl Pts',(20.1210124899567,20.8103501750223,8.20391838580633));
#185961=CARTESIAN_POINT('Ctrl Pts',(20.1115522492655,20.8185078057948,8.20317159790929));
#185962=CARTESIAN_POINT('Ctrl Pts',(20.106592883472,20.8227444958528,8.20278071386163));
#185963=CARTESIAN_POINT('Ctrl Pts',(20.094752451206,20.8327652637287,8.20184887360752));
#185964=CARTESIAN_POINT('Ctrl Pts',(20.087854009665,20.8385285314606,8.20130707372926));
#185965=CARTESIAN_POINT('Ctrl Pts',(20.0645100910978,20.8577799729748,8.19947721279945));
#185966=CARTESIAN_POINT('Ctrl Pts',(20.047898515629,20.8710638604358,8.19818095107264));
#185967=CARTESIAN_POINT('Ctrl Pts',(19.9091770816075,20.9786095840789,8.18740045945979));
#185968=CARTESIAN_POINT('Ctrl Pts',(19.7773214391571,21.0594990095322,8.17738215137559));
#185969=CARTESIAN_POINT('Ctrl Pts',(19.5140008039101,21.1838290699065,8.15815538318633));
#185970=CARTESIAN_POINT('Ctrl Pts',(19.3847282058745,21.230161927364,8.149040620382));
#185971=CARTESIAN_POINT('Ctrl Pts',(19.2367732322497,21.2674898967102,8.13952316503127));
#185972=CARTESIAN_POINT('Ctrl Pts',(19.221628164573,21.2711335937323,8.13855954269121));
#185973=CARTESIAN_POINT('Ctrl Pts',(19.2008163662,21.2758982560037,8.13725116375012));
#185974=CARTESIAN_POINT('Ctrl Pts',(19.1951836479804,21.277163587916,8.13689862968871));
#185975=CARTESIAN_POINT('Ctrl Pts',(19.1862178913223,21.279139161446,8.13634007765771));
#185976=CARTESIAN_POINT('Ctrl Pts',(19.1828882407298,21.2798644131634,8.13613321199359));
#185977=CARTESIAN_POINT('Ctrl Pts',(19.1760021450707,21.281346909377,8.13570658079827));
#185978=CARTESIAN_POINT('Ctrl Pts',(19.1724454975944,21.2821030315286,8.13548688568062));
#185979=CARTESIAN_POINT('Ctrl Pts',(19.1639566851621,21.2838848561474,8.13496406611253));
#185980=CARTESIAN_POINT('Ctrl Pts',(19.1590227345578,21.2849021322771,8.13466142250815));
#185981=CARTESIAN_POINT('Ctrl Pts',(19.1423270045487,21.2882823539886,8.13364135135323));
#185982=CARTESIAN_POINT('Ctrl Pts',(19.1305485375182,21.290562981309,8.13292846449497));
#185983=CARTESIAN_POINT('Ctrl Pts',(18.9927709103271,21.3160272539301,8.12466153894752));
#185984=CARTESIAN_POINT('Ctrl Pts',(18.8649180334723,21.3278306590802,8.1176828596066));
#185985=CARTESIAN_POINT('Ctrl Pts',(18.5726319299503,21.3282127664952,8.1018012615305));
#185986=CARTESIAN_POINT('Ctrl Pts',(18.4090489091375,21.3093396780551,8.09292709736246));
#185987=CARTESIAN_POINT('Ctrl Pts',(18.2260731696542,21.2663024989553,8.08201387484432));
#185988=CARTESIAN_POINT('Ctrl Pts',(18.2029472457859,21.2604489336314,8.08061716088213));
#185989=CARTESIAN_POINT('Ctrl Pts',(18.1705739508108,21.2516699822171,8.07863539286552));
#185990=CARTESIAN_POINT('Ctrl Pts',(18.1612397076422,21.2490698054735,8.07806086093737));
#185991=CARTESIAN_POINT('Ctrl Pts',(18.1461616475604,21.2447578490723,8.07712759892786));
#185992=CARTESIAN_POINT('Ctrl Pts',(18.1404066046115,21.2430855781871,8.07677015889863));
#185993=CARTESIAN_POINT('Ctrl Pts',(18.1284216801365,21.2395478031464,8.07602318628565));
#185994=CARTESIAN_POINT('Ctrl Pts',(18.1221931463947,21.2376779871395,8.07563351600594));
#185995=CARTESIAN_POINT('Ctrl Pts',(18.1074804407252,21.2331872049731,8.07470952997878));
#185996=CARTESIAN_POINT('Ctrl Pts',(18.0990039985633,21.230541513442,8.07417440820428));
#185997=CARTESIAN_POINT('Ctrl Pts',(18.0714817365435,21.221760783892,8.07242770000741));
#185998=CARTESIAN_POINT('Ctrl Pts',(18.0525066426356,21.2154091748382,8.07120901669527));
#185999=CARTESIAN_POINT('Ctrl Pts',(18.0077194297273,21.1997078990107,8.06829733983408));
#186000=CARTESIAN_POINT('Ctrl Pts',(17.9819940261754,21.1901234120518,8.06659680007746));
#186001=CARTESIAN_POINT('Ctrl Pts',(17.7996873526842,21.1181340019909,8.05434117138343));
#186002=CARTESIAN_POINT('Ctrl Pts',(17.6508872590648,21.0377318146349,8.04317898634587));
#186003=CARTESIAN_POINT('Ctrl Pts',(17.4270801356029,20.879762041665,8.02511096216918));
#186004=CARTESIAN_POINT('Ctrl Pts',(17.3455900609167,20.8126021379574,8.01821923985443));
#186005=CARTESIAN_POINT('Ctrl Pts',(17.2624433137892,20.732940776907,8.01110491570271));
#186006=CARTESIAN_POINT('Ctrl Pts',(17.2554955209156,20.7261921735057,8.01050981322381));
#186007=CARTESIAN_POINT('Ctrl Pts',(17.245303980766,20.7161559670475,8.00963628060322));
#186008=CARTESIAN_POINT('Ctrl Pts',(17.2420243956032,20.7129051633307,8.00935509063059));
#186009=CARTESIAN_POINT('Ctrl Pts',(17.2362243313436,20.7071182541331,8.00885767725378));
#186010=CARTESIAN_POINT('Ctrl Pts',(17.233699616995,20.7045864706815,8.00864111957486));
#186011=CARTESIAN_POINT('Ctrl Pts',(17.2283032898717,20.699147544418,8.00817817652515));
#186012=CARTESIAN_POINT('Ctrl Pts',(17.2254336840742,20.6962384885776,8.00793194776295));
#186013=CARTESIAN_POINT('Ctrl Pts',(17.2195619304922,20.6902514390753,8.00742796899478));
#186014=CARTESIAN_POINT('Ctrl Pts',(17.2165606987033,20.6871725691774,8.00717028984034));
#186015=CARTESIAN_POINT('Ctrl Pts',(17.2028029611228,20.6729726422423,8.00598858882848));
#186016=CARTESIAN_POINT('Ctrl Pts',(17.1921588701945,20.6617426857487,8.00507294015027));
#186017=CARTESIAN_POINT('Ctrl Pts',(17.1270483444767,20.5915222426383,7.99945554326263));
#186018=CARTESIAN_POINT('Ctrl Pts',(17.0758455863945,20.5295833190372,7.99496505990111));
#186019=CARTESIAN_POINT('Ctrl Pts',(16.9870774679686,20.4088272838093,7.98672570890619));
#186020=CARTESIAN_POINT('Ctrl Pts',(16.9486608446298,20.3507776227368,7.98296292502071));
#186021=CARTESIAN_POINT('Ctrl Pts',(16.8464151207174,20.1783867715229,7.97206976135757));
#186022=CARTESIAN_POINT('Ctrl Pts',(16.790267739069,20.059935407336,7.96490130145217));
#186023=CARTESIAN_POINT('Ctrl Pts',(16.7454193311435,19.9371101317641,7.95734462820299));
#186024=CARTESIAN_POINT('Ctrl Pts',(16.7454193726886,19.9371102455424,7.73405220823978));
#186025=CARTESIAN_POINT('Ctrl Pts',(16.7614416071399,19.9809899528345,7.73713765832381));
#186026=CARTESIAN_POINT('Ctrl Pts',(16.7789269230783,20.0243687437115,7.74021945161001));
#186027=CARTESIAN_POINT('Ctrl Pts',(16.8241807251844,20.1267054853234,7.74752070944097));
#186028=CARTESIAN_POINT('Ctrl Pts',(16.853240883593,20.1849984452125,7.75170524900241));
#186029=CARTESIAN_POINT('Ctrl Pts',(16.8913431829543,20.2533423367608,7.75656672675373));
#186030=CARTESIAN_POINT('Ctrl Pts',(16.8978491813239,20.2647608283762,7.75737736942318));
#186031=CARTESIAN_POINT('Ctrl Pts',(16.9070905289816,20.2806345610226,7.75850128692437));
#186032=CARTESIAN_POINT('Ctrl Pts',(16.90973653366,20.2851411062559,7.75882002295505));
#186033=CARTESIAN_POINT('Ctrl Pts',(16.9142695216255,20.2927964043434,7.75936081404305));
#186034=CARTESIAN_POINT('Ctrl Pts',(16.9161480474682,20.2959501158012,7.75958341237253));
#186035=CARTESIAN_POINT('Ctrl Pts',(16.9197628321593,20.3019829523373,7.7600088436105));
#186036=CARTESIAN_POINT('Ctrl Pts',(16.921497752063,20.30486283649,7.76021176434571));
#186037=CARTESIAN_POINT('Ctrl Pts',(16.9261081646349,20.3124748169595,7.76074770715533));
#186038=CARTESIAN_POINT('Ctrl Pts',(16.9289953978466,20.3171998230673,7.76107996558489));
#186039=CARTESIAN_POINT('Ctrl Pts',(16.9392862663533,20.3338934377739,7.76225255944951));
#186040=CARTESIAN_POINT('Ctrl Pts',(16.9467908570666,20.3457997891742,7.763086533279));
#186041=CARTESIAN_POINT('Ctrl Pts',(17.0425700446124,20.4944503576821,7.77348057342281));
#186042=CARTESIAN_POINT('Ctrl Pts',(17.1462244454709,20.620668471612,7.78214130874963));
#186043=CARTESIAN_POINT('Ctrl Pts',(17.3537662764628,20.8211084582887,7.79784826975427));
#186044=CARTESIAN_POINT('Ctrl Pts',(17.4517854744826,20.9002054247221,7.8047787964754));
#186045=CARTESIAN_POINT('Ctrl Pts',(17.5701088041064,20.9794244492968,7.81304298815136));
#186046=CARTESIAN_POINT('Ctrl Pts',(17.5840913685183,20.9885482735955,7.8140177319333));
#186047=CARTESIAN_POINT('Ctrl Pts',(17.606402319916,21.0027330725957,7.81557093431809));
#186048=CARTESIAN_POINT('Ctrl Pts',(17.6146604205226,21.0079036792868,7.81614537631878));
#186049=CARTESIAN_POINT('Ctrl Pts',(17.6303732837561,21.0175915548133,7.81723768368851));
#186050=CARTESIAN_POINT('Ctrl Pts',(17.6378208442782,21.0221201588599,7.81775512124974));
#186051=CARTESIAN_POINT('Ctrl Pts',(17.6507774341252,21.0298894197626,7.81865490164893));
#186052=CARTESIAN_POINT('Ctrl Pts',(17.656273602304,21.0331513819856,7.81903646029143));
#186053=CARTESIAN_POINT('Ctrl Pts',(17.6669320886513,21.039412074421,7.81977619336423));
#186054=CARTESIAN_POINT('Ctrl Pts',(17.6720924917106,21.042413957581,7.82013424849662));
#186055=CARTESIAN_POINT('Ctrl Pts',(17.6855524729191,21.0501678137,7.82106796577067));
#186056=CARTESIAN_POINT('Ctrl Pts',(17.6938716086648,21.0548854055596,7.8216448619957));
#186057=CARTESIAN_POINT('Ctrl Pts',(17.7223434748233,21.0707771548432,7.8236187549177));
#186058=CARTESIAN_POINT('Ctrl Pts',(17.7426459997752,21.0816782649608,7.82502544470214));
#186059=CARTESIAN_POINT('Ctrl Pts',(17.9182807179758,21.1723202994331,7.83719163970475));
#186060=CARTESIAN_POINT('Ctrl Pts',(18.0827223620787,21.232877742226,7.84864683896861));
#186061=CARTESIAN_POINT('Ctrl Pts',(18.3380271012821,21.2924836278559,7.86596942371986));
#186062=CARTESIAN_POINT('Ctrl Pts',(18.4245259748775,21.3070907399696,7.87174652517322));
#186063=CARTESIAN_POINT('Ctrl Pts',(18.5494557209725,21.3202830242743,7.879768160808));
#186064=CARTESIAN_POINT('Ctrl Pts',(18.5873288471997,21.3232545905153,7.88215744255913));
#186065=CARTESIAN_POINT('Ctrl Pts',(18.6328346665505,21.3255950066018,7.88496142987693));
#186066=CARTESIAN_POINT('Ctrl Pts',(18.640407504597,21.3259437144835,7.8854258366451));
#186067=CARTESIAN_POINT('Ctrl Pts',(18.6521629158985,21.3264217544263,7.88614312887025));
#186068=CARTESIAN_POINT('Ctrl Pts',(18.6563441858421,21.3265793728105,7.8863975528922));
#186069=CARTESIAN_POINT('Ctrl Pts',(18.664087355159,21.3268482745901,7.8868673661047));
#186070=CARTESIAN_POINT('Ctrl Pts',(18.667649037583,21.3269629602339,7.88708293814638));
#186071=CARTESIAN_POINT('Ctrl Pts',(18.6756865398418,21.3272014525484,7.88756822366703));
#186072=CARTESIAN_POINT('Ctrl Pts',(18.6801624600447,21.3273200531919,7.88783764298509));
#186073=CARTESIAN_POINT('Ctrl Pts',(18.6933298308605,21.3276271549256,7.88862788478297));
#186074=CARTESIAN_POINT('Ctrl Pts',(18.7020222265683,21.3277763234453,7.889146558561));
#186075=CARTESIAN_POINT('Ctrl Pts',(18.7635129971128,21.3284526913115,7.89279601711676));
#186076=CARTESIAN_POINT('Ctrl Pts',(18.8163185965995,21.3270580231469,7.895827496855));
#186077=CARTESIAN_POINT('Ctrl Pts',(18.885088170904,21.3226629860662,7.89970463401846));
#186078=CARTESIAN_POINT('Ctrl Pts',(18.9011432035323,21.3214528827362,7.90060472921187));
#186079=CARTESIAN_POINT('Ctrl Pts',(18.9674699475352,21.3156920492803,7.90430771357342));
#186080=CARTESIAN_POINT('Ctrl Pts',(19.0175861870824,21.3095271149566,7.90706908851281));
#186081=CARTESIAN_POINT('Ctrl Pts',(19.1754742620877,21.2843448232093,7.9157741024952));
#186082=CARTESIAN_POINT('Ctrl Pts',(19.2820135694758,21.2587642760604,7.92166485657649));
#186083=CARTESIAN_POINT('Ctrl Pts',(19.4385873721785,21.2080703528659,7.9308153865112));
#186084=CARTESIAN_POINT('Ctrl Pts',(19.4903925911689,21.1890300705561,7.93392645348369));
#186085=CARTESIAN_POINT('Ctrl Pts',(19.5731344739018,21.1548933578749,7.93907581755766));
#186086=CARTESIAN_POINT('Ctrl Pts',(19.604551705176,21.1410278711995,7.94107461940823));
#186087=CARTESIAN_POINT('Ctrl Pts',(19.645399306145,21.121800149435,7.94373719886824));
#186088=CARTESIAN_POINT('Ctrl Pts',(19.655146444088,21.1171204390861,7.94437740450623));
#186089=CARTESIAN_POINT('Ctrl Pts',(19.6710533820928,21.1093328354737,7.94543035561458));
#186090=CARTESIAN_POINT('Ctrl Pts',(19.6772346703264,21.1062690970126,7.94584155839544));
#186091=CARTESIAN_POINT('Ctrl Pts',(19.6891716657971,21.1002796975685,7.94663965177085));
#186092=CARTESIAN_POINT('Ctrl Pts',(19.6949291877685,21.0973578084362,7.94702640667253));
#186093=CARTESIAN_POINT('Ctrl Pts',(19.7081933950114,21.090549861102,7.94792165549318));
#186094=CARTESIAN_POINT('Ctrl Pts',(19.7156903140597,21.0866451091015,7.94843080494301));
#186095=CARTESIAN_POINT('Ctrl Pts',(19.735792086032,21.076021618663,7.94980461916907));
#186096=CARTESIAN_POINT('Ctrl Pts',(19.7483524897321,21.0692201249031,7.95067220873737));
#186097=CARTESIAN_POINT('Ctrl Pts',(19.8612905143558,21.0065776060221,7.95855788522971));
#186098=CARTESIAN_POINT('Ctrl Pts',(19.9570208788332,20.9427896348113,7.96586707868778));
#186099=CARTESIAN_POINT('Ctrl Pts',(20.0998234888755,20.829868139343,7.97775017929054));
#186100=CARTESIAN_POINT('Ctrl Pts',(20.1505349486765,20.785686016252,7.9821913832998));
#186101=CARTESIAN_POINT('Ctrl Pts',(20.2643817514613,20.6765409158214,7.99261347857898));
#186102=CARTESIAN_POINT('Ctrl Pts',(20.3256277748713,20.6097857258951,7.99858644373108));
#186103=CARTESIAN_POINT('Ctrl Pts',(20.4066929445638,20.5091850042919,8.00684123117954));
#186104=CARTESIAN_POINT('Ctrl Pts',(20.4301409572904,20.4783958662819,8.00927639645246));
#186105=CARTESIAN_POINT('Ctrl Pts',(20.4571825945517,20.4407921855456,8.01212684999798));
#186106=CARTESIAN_POINT('Ctrl Pts',(20.4615984173786,20.4345811318094,8.01259373250377));
#186107=CARTESIAN_POINT('Ctrl Pts',(20.4683917108544,20.4249159663279,8.01331401534913));
#186108=CARTESIAN_POINT('Ctrl Pts',(20.4707925684088,20.421478481845,8.01356897445338));
#186109=CARTESIAN_POINT('Ctrl Pts',(20.475214640622,20.4151068347051,8.01403928436898));
#186110=CARTESIAN_POINT('Ctrl Pts',(20.4772386440805,20.4121747267545,8.01425482117396));
#186111=CARTESIAN_POINT('Ctrl Pts',(20.4817832703416,20.4055553935235,8.01473941048924));
#186112=CARTESIAN_POINT('Ctrl Pts',(20.4842996249741,20.4018653038604,8.01500817258838));
#186113=CARTESIAN_POINT('Ctrl Pts',(20.4916506071043,20.3910118767057,8.01579470321554));
#186114=CARTESIAN_POINT('Ctrl Pts',(20.4964531385041,20.3838267673338,8.01631035316076));
#186115=CARTESIAN_POINT('Ctrl Pts',(20.5295917244417,20.3335845952032,8.01988256980961));
#186116=CARTESIAN_POINT('Ctrl Pts',(20.5563934477622,20.2895308826218,8.02284455661355));
#186117=CARTESIAN_POINT('Ctrl Pts',(20.5884267037649,20.2322679851554,8.02654016216896));
#186118=CARTESIAN_POINT('Ctrl Pts',(20.595168852791,20.2199287444364,8.02732765445513));
#186119=CARTESIAN_POINT('Ctrl Pts',(20.6769258886446,20.0666911618065,8.03700947129375));
#186120=CARTESIAN_POINT('Ctrl Pts',(20.7358971234608,19.9178104785668,8.0454408790572));
#186121=CARTESIAN_POINT('Ctrl Pts',(20.7981774096809,19.6875368405104,8.05867901546202));
#186122=CARTESIAN_POINT('Ctrl Pts',(20.8145023666282,19.6102789790718,8.06314414533086));
#186123=CARTESIAN_POINT('Ctrl Pts',(20.8294094735106,19.5131946144835,8.06887605107643));
#186124=CARTESIAN_POINT('Ctrl Pts',(20.8320806267839,19.4940549303999,8.0700116466015));
#186125=CARTESIAN_POINT('Ctrl Pts',(20.8355673653284,19.4663006228896,8.07166744477738));
#186126=CARTESIAN_POINT('Ctrl Pts',(20.8365928017403,19.4577130027913,8.07218102705942));
#186127=CARTESIAN_POINT('Ctrl Pts',(20.838292664879,19.442696279926,8.07308138094401));
#186128=CARTESIAN_POINT('Ctrl Pts',(20.8389903239764,19.4362698828748,8.07346741491033));
#186129=CARTESIAN_POINT('Ctrl Pts',(20.8402840342536,19.4238219458645,8.07421661052226));
#186130=CARTESIAN_POINT('Ctrl Pts',(20.8408837235466,19.4178008410659,8.07457965348905));
#186131=CARTESIAN_POINT('Ctrl Pts',(20.842250039493,19.4034593146041,8.07544597038146));
#186132=CARTESIAN_POINT('Ctrl Pts',(20.8429932311686,19.3951368093399,8.07594997711387));
#186133=CARTESIAN_POINT('Ctrl Pts',(20.8454697078749,19.3654195882152,8.07775431039218));
#186134=CARTESIAN_POINT('Ctrl Pts',(20.8469268064436,19.3440037362855,8.07906326578301));
#186135=CARTESIAN_POINT('Ctrl Pts',(20.8581504002332,19.1313361615528,8.09215156258513));
#186136=CARTESIAN_POINT('Ctrl Pts',(20.8422458367224,18.9396507140996,8.1047899678711));
#186137=CARTESIAN_POINT('Ctrl Pts',(20.7842862355159,18.6782294747407,8.12245696833768));
#186138=CARTESIAN_POINT('Ctrl Pts',(20.7637389751389,18.604634298812,8.12746415437814));
#186139=CARTESIAN_POINT('Ctrl Pts',(20.7280420968685,18.499164863796,8.13455550064834));
#186140=CARTESIAN_POINT('Ctrl Pts',(20.7160046351787,18.4663046922486,8.13675213320625));
#186141=CARTESIAN_POINT('Ctrl Pts',(20.7004397330155,18.4268708228651,8.13935998860683));
#186142=CARTESIAN_POINT('Ctrl Pts',(20.6976859840595,18.4199999053433,8.13981332406851));
#186143=CARTESIAN_POINT('Ctrl Pts',(20.6933339324193,18.4093038452185,8.1405172296235));
#186144=CARTESIAN_POINT('Ctrl Pts',(20.6917603677301,18.4054687923196,8.14076924932889));
#186145=CARTESIAN_POINT('Ctrl Pts',(20.6888116828965,18.3983420089903,8.1412368719495));
#186146=CARTESIAN_POINT('Ctrl Pts',(20.6874395207544,18.3950491651095,8.14145264349615));
#186147=CARTESIAN_POINT('Ctrl Pts',(20.6843061062971,18.3875829672971,8.14194124462072));
#186148=CARTESIAN_POINT('Ctrl Pts',(20.6825397833067,18.3834117982039,8.14221376240389));
#186149=CARTESIAN_POINT('Ctrl Pts',(20.6772486821731,18.3710277183668,8.14302160940908));
#186150=CARTESIAN_POINT('Ctrl Pts',(20.6736852183593,18.3628313052719,8.14355464418467));
#186151=CARTESIAN_POINT('Ctrl Pts',(20.6461352954632,18.3005448034559,8.14759458454131));
#186152=CARTESIAN_POINT('Ctrl Pts',(20.6199401845378,18.2474539338933,8.15097649556824));
#186153=CARTESIAN_POINT('Ctrl Pts',(20.5145648575838,18.0546965162268,8.16327350820359));
#186154=CARTESIAN_POINT('Ctrl Pts',(20.4218098121438,17.923074186733,8.17174526433562));
#186155=CARTESIAN_POINT('Ctrl Pts',(20.2745672022251,17.7577104684876,8.18400229545833));
#186156=CARTESIAN_POINT('Ctrl Pts',(20.2321278241145,17.7139996790227,8.18742184792589));
#186157=CARTESIAN_POINT('Ctrl Pts',(20.1610674176161,17.6468622918725,8.19303391965465));
#186158=CARTESIAN_POINT('Ctrl Pts',(20.1336137003003,17.622249096882,8.19517696331534));
#186159=CARTESIAN_POINT('Ctrl Pts',(20.0970823207262,17.5911794410287,8.19800407675716));
#186160=CARTESIAN_POINT('Ctrl Pts',(20.0885758896502,17.5840592486395,8.19866069434043));
#186161=CARTESIAN_POINT('Ctrl Pts',(20.074641395364,17.5725806088952,8.199733779857));
#186162=CARTESIAN_POINT('Ctrl Pts',(20.0692470334847,17.5681814434018,8.20014858778615));
#186163=CARTESIAN_POINT('Ctrl Pts',(20.0588250506831,17.5597674360966,8.20094888717647));
#186164=CARTESIAN_POINT('Ctrl Pts',(20.0538006235375,17.5557487478618,8.20133421742802));
#186165=CARTESIAN_POINT('Ctrl Pts',(20.0422452825247,17.546592499537,8.20221932876906));
#186166=CARTESIAN_POINT('Ctrl Pts',(20.0357023140636,17.5414703868058,8.20271971859494));
#186167=CARTESIAN_POINT('Ctrl Pts',(20.0182196282748,17.5279494475271,8.20405476369801));
#186168=CARTESIAN_POINT('Ctrl Pts',(20.0072278408292,17.5196188877034,8.20489209239991));
#186169=CARTESIAN_POINT('Ctrl Pts',(19.9215454903605,17.4559896586959,8.21140444862869));
#186170=CARTESIAN_POINT('Ctrl Pts',(19.8433781122752,17.4055632812982,8.21726670638647));
#186171=CARTESIAN_POINT('Ctrl Pts',(19.6060027718017,17.2736790092296,8.23482233762077));
#186172=CARTESIAN_POINT('Ctrl Pts',(19.4395078250865,17.2070405250267,8.24689323081192));
#186173=CARTESIAN_POINT('Ctrl Pts',(19.2273536497098,17.1518889801362,8.26092083544492));
#186174=CARTESIAN_POINT('Ctrl Pts',(19.1877871272697,17.1428090616987,8.26347827670952));
#186175=CARTESIAN_POINT('Ctrl Pts',(19.1404077049916,17.133361577293,8.26645212279447));
#186176=CARTESIAN_POINT('Ctrl Pts',(19.1328258829396,17.1318928460762,8.26692532600845));
#186177=CARTESIAN_POINT('Ctrl Pts',(19.1210937720047,17.1296866701574,8.26765323915532));
#186178=CARTESIAN_POINT('Ctrl Pts',(19.1169491243575,17.128920094191,8.26790955993638));
#186179=CARTESIAN_POINT('Ctrl Pts',(19.1092982835531,17.1275286462994,8.26838114792434));
#186180=CARTESIAN_POINT('Ctrl Pts',(19.1057928291022,17.1269002480954,8.26859660908841));
#186181=CARTESIAN_POINT('Ctrl Pts',(19.0979144287942,17.1255084528918,8.26907949045741));
#186182=CARTESIAN_POINT('Ctrl Pts',(19.0935406718306,17.124749964489,8.26934662952876));
#186183=CARTESIAN_POINT('Ctrl Pts',(19.0823598875468,17.1228472199806,8.27002720940498));
#186184=CARTESIAN_POINT('Ctrl Pts',(19.0755495307269,17.1217224777507,8.27043956788783));
#186185=CARTESIAN_POINT('Ctrl Pts',(19.0360414860937,17.1153959995866,8.27281967177081));
#186186=CARTESIAN_POINT('Ctrl Pts',(19.0032289089566,17.1109282741121,8.27474860937124));
#186187=CARTESIAN_POINT('Ctrl Pts',(18.9516911818924,17.1051388753585,8.27772250434146));
#186188=CARTESIAN_POINT('Ctrl Pts',(18.9330318257708,17.1032934508825,8.27878781205925));
#186189=CARTESIAN_POINT('Ctrl Pts',(18.883191271059,17.0990319784527,8.28160866882729));
#186190=CARTESIAN_POINT('Ctrl Pts',(18.8519763573168,17.097058499626,8.2833497023143));
#186191=CARTESIAN_POINT('Ctrl Pts',(18.7822694129759,17.09420038032,8.28720197452944));
#186192=CARTESIAN_POINT('Ctrl Pts',(18.7437738949707,17.0936726361779,8.28930523651559));
#186193=CARTESIAN_POINT('Ctrl Pts',(18.5960095192937,17.0956771218647,8.2973505806258));
#186194=CARTESIAN_POINT('Ctrl Pts',(18.4870143169506,17.1056189340772,8.30323550977881));
#186195=CARTESIAN_POINT('Ctrl Pts',(18.3250240643611,17.133151057932,8.31237249763358));
#186196=CARTESIAN_POINT('Ctrl Pts',(18.2711534119266,17.1444836233796,8.31547580247535));
#186197=CARTESIAN_POINT('Ctrl Pts',(18.1845501288961,17.1662583447166,8.32061346317517));
#186198=CARTESIAN_POINT('Ctrl Pts',(18.1515215748684,17.17542089666,8.32260855877994));
#186199=CARTESIAN_POINT('Ctrl Pts',(18.1083928119074,17.1885209787743,8.32526690027165));
#186200=CARTESIAN_POINT('Ctrl Pts',(18.098078683079,17.1917402798983,8.32590666984632));
#186201=CARTESIAN_POINT('Ctrl Pts',(18.0812216954589,17.1971437346074,8.32695908639587));
#186202=CARTESIAN_POINT('Ctrl Pts',(18.0746639872074,17.1992811843987,8.32737019375435));
#186203=CARTESIAN_POINT('Ctrl Pts',(18.061987450785,17.2034816740516,8.32816823249805));
#186204=CARTESIAN_POINT('Ctrl Pts',(18.0558673791814,17.2055407402618,8.32855502888172));
#186205=CARTESIAN_POINT('Ctrl Pts',(18.0417538772983,17.2103611457819,8.32945056398271));
#186206=CARTESIAN_POINT('Ctrl Pts',(18.0337674220228,17.2131424342812,8.32995995955124));
#186207=CARTESIAN_POINT('Ctrl Pts',(18.012324168172,17.2207544340201,8.33133486860982));
#186208=CARTESIAN_POINT('Ctrl Pts',(17.9988994684668,17.2256736762072,8.3322033141505));
#186209=CARTESIAN_POINT('Ctrl Pts',(17.8756709986461,17.2722497730966,8.34024723633983));
#186210=CARTESIAN_POINT('Ctrl Pts',(17.769479780301,17.3228331793544,8.34772770571448));
#186211=CARTESIAN_POINT('Ctrl Pts',(17.5265483705793,17.4644118186841,8.3660979523529));
#186212=CARTESIAN_POINT('Ctrl Pts',(17.3951035362788,17.5630114445614,8.37712898107205));
#186213=CARTESIAN_POINT('Ctrl Pts',(17.2538230711235,17.6971541617917,8.38949101684688));
#186214=CARTESIAN_POINT('Ctrl Pts',(17.2317792069455,17.7190261773293,8.39143495321358));
#186215=CARTESIAN_POINT('Ctrl Pts',(17.2052685506064,17.7465137095053,8.39378276704108));
#186216=CARTESIAN_POINT('Ctrl Pts',(17.2003398386427,17.7516760290386,8.39421969567358));
#186217=CARTESIAN_POINT('Ctrl Pts',(17.192629870127,17.7598336321366,8.3949037271252));
#186218=CARTESIAN_POINT('Ctrl Pts',(17.1898310723782,17.762812157176,8.39515215187031));
#186219=CARTESIAN_POINT('Ctrl Pts',(17.184600121321,17.7684114241679,8.39561663993207));
#186220=CARTESIAN_POINT('Ctrl Pts',(17.182166009356,17.771030191683,8.39583285027263));
#186221=CARTESIAN_POINT('Ctrl Pts',(17.1766043152108,17.7770442858546,8.39632704935111));
#186222=CARTESIAN_POINT('Ctrl Pts',(17.1734812015795,17.7804436782034,8.39660469720257));
#186223=CARTESIAN_POINT('Ctrl Pts',(17.1638449847441,17.7910014473595,8.39746188811729));
#186224=CARTESIAN_POINT('Ctrl Pts',(17.1573697247597,17.7981944066286,8.3980386390588));
#186225=CARTESIAN_POINT('Ctrl Pts',(17.0888253216945,17.8753942370954,8.40415509099116));
#186226=CARTESIAN_POINT('Ctrl Pts',(17.0314046947335,17.9494072864013,8.40937985767366));
#186227=CARTESIAN_POINT('Ctrl Pts',(16.9052198389649,18.136437404125,8.42175707314412));
#186228=CARTESIAN_POINT('Ctrl Pts',(16.8417777130446,18.2525550238779,8.42880642862429));
#186229=CARTESIAN_POINT('Ctrl Pts',(16.7672717976745,18.4256038862872,8.43927195419713));
#186230=CARTESIAN_POINT('Ctrl Pts',(16.7470574656025,18.478247955487,8.44244770343866));
#186231=CARTESIAN_POINT('Ctrl Pts',(16.7177768299157,18.5646645950144,8.44769447419419));
#186232=CARTESIAN_POINT('Ctrl Pts',(16.7074032722856,18.5979658864742,8.44972401166756));
#186233=CARTESIAN_POINT('Ctrl Pts',(16.6948809049371,18.6419652442051,8.45242171561416));
#186234=CARTESIAN_POINT('Ctrl Pts',(16.6919850793439,18.6524462476225,8.45306550904215));
#186235=CARTESIAN_POINT('Ctrl Pts',(16.687380676545,18.6696257059902,8.45412285921641));
#186236=CARTESIAN_POINT('Ctrl Pts',(16.685623914715,18.6763111251912,8.45453484790281));
#186237=CARTESIAN_POINT('Ctrl Pts',(16.6822909630623,18.689252315848,8.45533339897452));
#186238=CARTESIAN_POINT('Ctrl Pts',(16.6807105628131,18.6955069313001,8.45571982000635));
#186239=CARTESIAN_POINT('Ctrl Pts',(16.6771333681718,18.7099415620988,8.45661274807098));
#186240=CARTESIAN_POINT('Ctrl Pts',(16.675156749043,18.7181264217778,8.45711989992978));
#186241=CARTESIAN_POINT('Ctrl Pts',(16.6699846633705,18.7401173122278,8.45848483941948));
#186242=CARTESIAN_POINT('Ctrl Pts',(16.6668789475786,18.7539438165892,8.45934549332977));
#186243=CARTESIAN_POINT('Ctrl Pts',(16.6325818105057,18.9141381136881,8.46934707087851));
#186244=CARTESIAN_POINT('Ctrl Pts',(16.6168624934387,19.0633573065227,8.47899859422792));
#186245=CARTESIAN_POINT('Ctrl Pts',(16.617139476207,19.3627302310582,8.4987281552706));
#186246=CARTESIAN_POINT('Ctrl Pts',(16.6331712122024,19.5120733058891,8.50874331273543));
#186247=CARTESIAN_POINT('Ctrl Pts',(16.6681544975782,19.6738371178254,8.5190680570008));
#186248=CARTESIAN_POINT('Ctrl Pts',(16.671646380716,19.6891562714579,8.52004014896673));
#186249=CARTESIAN_POINT('Ctrl Pts',(16.6766589553007,19.7100695241367,8.52135811742987));
#186250=CARTESIAN_POINT('Ctrl Pts',(16.6780324478114,19.7156979198373,8.52171191625856));
#186251=CARTESIAN_POINT('Ctrl Pts',(16.6802514660234,19.7246317736394,8.52227197438837));
#186252=CARTESIAN_POINT('Ctrl Pts',(16.6810818949222,19.7279408998413,8.52247908939753));
#186253=CARTESIAN_POINT('Ctrl Pts',(16.6828132675962,19.7347701706098,8.52290581951831));
#186254=CARTESIAN_POINT('Ctrl Pts',(16.6837152750071,19.7382900050455,8.52312536596812));
#186255=CARTESIAN_POINT('Ctrl Pts',(16.6858857791743,19.7466700183093,8.52364716007648));
#186256=CARTESIAN_POINT('Ctrl Pts',(16.687162529565,19.7515280759319,8.52394893195275));
#186257=CARTESIAN_POINT('Ctrl Pts',(16.6915249191881,19.7678899359836,8.52496299930673));
#186258=CARTESIAN_POINT('Ctrl Pts',(16.6946904096531,19.7793724711379,8.52567082640978));
#186259=CARTESIAN_POINT('Ctrl Pts',(16.7120038266166,19.8401679778402,8.5294010897818));
#186260=CARTESIAN_POINT('Ctrl Pts',(16.7278379789767,19.8889605106395,8.53233405544009));
#186261=CARTESIAN_POINT('Ctrl Pts',(16.7454193934539,19.9371103024118,8.53521106676425));
#186262=CARTESIAN_POINT('Origin',(18.734,19.211,0.));
#186263=CARTESIAN_POINT('',(16.7437494103711,19.9377357416701,9.55561790998273));
#186264=CARTESIAN_POINT('',(16.7454193811439,19.9371102686989,9.33206801830578));
#186265=CARTESIAN_POINT('',(16.7454193623258,19.9371102171621,0.));
#186266=CARTESIAN_POINT('',(16.616352496962,19.2128935159974,9.51094372097751));
#186267=CARTESIAN_POINT('Ctrl Pts',(16.616352496962,19.2128935159974,9.51094372097751));
#186268=CARTESIAN_POINT('Ctrl Pts',(16.6150297892913,19.3558822368192,9.51955279572482));
#186269=CARTESIAN_POINT('Ctrl Pts',(16.6379357136472,19.6027931032506,9.5344441920599));
#186270=CARTESIAN_POINT('Ctrl Pts',(16.7071052565872,19.8401886875416,9.54933558839497));
#186271=CARTESIAN_POINT('Ctrl Pts',(16.7437494103711,19.9377357416701,9.55561790998273));
#186272=CARTESIAN_POINT('Ctrl Pts',(16.6170008641642,19.2129128174038,9.51057059174555));
#186273=CARTESIAN_POINT('Ctrl Pts',(16.6168631868029,19.0605392273433,9.50228575561247));
#186274=CARTESIAN_POINT('Ctrl Pts',(16.6331756165184,18.9086044877191,9.49407331105422));
#186275=CARTESIAN_POINT('Ctrl Pts',(16.6710117387555,18.7351851106024,9.48389303380534));
#186276=CARTESIAN_POINT('Ctrl Pts',(16.6768043973513,18.7107335185976,9.48243957060468));
#186277=CARTESIAN_POINT('Ctrl Pts',(16.6862549747941,18.6737862621852,9.48021287530327));
#186278=CARTESIAN_POINT('Ctrl Pts',(16.6895953042397,18.6612112067376,9.47944961775237));
#186279=CARTESIAN_POINT('Ctrl Pts',(16.6960056019571,18.637945435653,9.47802702852224));
#186280=CARTESIAN_POINT('Ctrl Pts',(16.6990443286782,18.6272465342369,9.47736871703937));
#186281=CARTESIAN_POINT('Ctrl Pts',(16.7041234695228,18.6098853584401,9.47629355189756));
#186282=CARTESIAN_POINT('Ctrl Pts',(16.7061127423382,18.6032082513643,9.47587837053529));
#186283=CARTESIAN_POINT('Ctrl Pts',(16.7100017484915,18.5903862345436,9.47507782781616));
#186284=CARTESIAN_POINT('Ctrl Pts',(16.711896599253,18.5842399157133,9.47469263024993));
#186285=CARTESIAN_POINT('Ctrl Pts',(16.7162994341446,18.5701862658294,9.47380849840893));
#186286=CARTESIAN_POINT('Ctrl Pts',(16.7188259343314,18.5622848873713,9.4733089599268));
#186287=CARTESIAN_POINT('Ctrl Pts',(16.7256616973275,18.5413320444977,9.47197766285819));
#186288=CARTESIAN_POINT('Ctrl Pts',(16.7300516812434,18.5283075140467,9.47114325456751));
#186289=CARTESIAN_POINT('Ctrl Pts',(16.7645088008198,18.4292744148387,9.46474530371271));
#186290=CARTESIAN_POINT('Ctrl Pts',(16.7999694901022,18.3452560210027,9.45900206102836));
#186291=CARTESIAN_POINT('Ctrl Pts',(16.8622522444355,18.2207657410432,9.45001095382446));
#186292=CARTESIAN_POINT('Ctrl Pts',(16.8852374914198,18.1784883159323,9.44686823633246));
#186293=CARTESIAN_POINT('Ctrl Pts',(16.9358507399165,18.0925111726021,9.44030887825123));
#186294=CARTESIAN_POINT('Ctrl Pts',(16.9636801260305,18.0489649597478,9.4368912216606));
#186295=CARTESIAN_POINT('Ctrl Pts',(17.0410581348755,17.9371282998117,9.42790784999361));
#186296=CARTESIAN_POINT('Ctrl Pts',(17.0931467175513,17.8707001764926,9.42235623719979));
#186297=CARTESIAN_POINT('Ctrl Pts',(17.1736468430556,17.779789947113,9.41460812106404));
#186298=CARTESIAN_POINT('Ctrl Pts',(17.198958106632,17.7526752887502,9.41227648247279));
#186299=CARTESIAN_POINT('Ctrl Pts',(17.2302643853823,17.7208573297973,9.40952976152539));
#186300=CARTESIAN_POINT('Ctrl Pts',(17.2355872031759,17.7155050750742,9.4090673497681));
#186301=CARTESIAN_POINT('Ctrl Pts',(17.2439050643718,17.7072302065798,9.4083520236153));
#186302=CARTESIAN_POINT('Ctrl Pts',(17.2468802759877,17.7042878722394,9.40809758960079));
#186303=CARTESIAN_POINT('Ctrl Pts',(17.2524054123862,17.6988560991563,9.40762776709647));
#186304=CARTESIAN_POINT('Ctrl Pts',(17.2549528770421,17.6963642988243,9.40741219569709));
#186305=CARTESIAN_POINT('Ctrl Pts',(17.260715228745,17.6907562602201,9.40692692315031));
#186306=CARTESIAN_POINT('Ctrl Pts',(17.2639337075602,17.6876437901032,9.40665751609366));
#186307=CARTESIAN_POINT('Ctrl Pts',(17.2734297528344,17.6785186421983,9.40586734374596));
#186308=CARTESIAN_POINT('Ctrl Pts',(17.2797345928115,17.6725343064488,9.40534872659042));
#186309=CARTESIAN_POINT('Ctrl Pts',(17.3245664470674,17.6305033307233,9.40170171030165));
#186310=CARTESIAN_POINT('Ctrl Pts',(17.3643957203279,17.5958660214916,9.39867246161717));
#186311=CARTESIAN_POINT('Ctrl Pts',(17.4205669785028,17.5505909739008,9.39461311580937));
#186312=CARTESIAN_POINT('Ctrl Pts',(17.4358193874765,17.5386389250701,9.39353122639919));
#186313=CARTESIAN_POINT('Ctrl Pts',(17.60170288466,17.4122869186503,9.38195672191991));
#186314=CARTESIAN_POINT('Ctrl Pts',(17.766848813507,17.3183592594585,9.37203060454308));
#186315=CARTESIAN_POINT('Ctrl Pts',(17.9921022215736,17.2275277199031,9.35827028911597));
#186316=CARTESIAN_POINT('Ctrl Pts',(18.0426651317156,17.2093431889747,9.3551752436795));
#186317=CARTESIAN_POINT('Ctrl Pts',(18.105898312267,17.1892837183624,9.35127299965955));
#186318=CARTESIAN_POINT('Ctrl Pts',(18.1179684008066,17.1855732518881,9.35052677202271));
#186319=CARTESIAN_POINT('Ctrl Pts',(18.1370676250858,17.1798884735445,9.34934354915956));
#186320=CARTESIAN_POINT('Ctrl Pts',(18.1440751386236,17.1778421239354,9.34890891306893));
#186321=CARTESIAN_POINT('Ctrl Pts',(18.15721380775,17.1740789839324,9.34809298391168));
#186322=CARTESIAN_POINT('Ctrl Pts',(18.1633424107606,17.1723535245805,9.34771197864494));
#186323=CARTESIAN_POINT('Ctrl Pts',(18.1770509902638,17.168560642189,9.346858781466));
#186324=CARTESIAN_POINT('Ctrl Pts',(18.1846348513574,17.1665077254628,9.34638612393971));
#186325=CARTESIAN_POINT('Ctrl Pts',(18.2038347157889,17.1614249509809,9.34518778721889));
#186326=CARTESIAN_POINT('Ctrl Pts',(18.2154652744089,17.1584516231797,9.34446029070854));
#186327=CARTESIAN_POINT('Ctrl Pts',(18.2811550344823,17.1422521293461,9.34034192892597));
#186328=CARTESIAN_POINT('Ctrl Pts',(18.3356897791891,17.1310638529534,9.33688613978704));
#186329=CARTESIAN_POINT('Ctrl Pts',(18.4151676168696,17.1179985950006,9.33179366450893));
#186330=CARTESIAN_POINT('Ctrl Pts',(18.4398056387823,17.1143935573068,9.33020744464369));
#186331=CARTESIAN_POINT('Ctrl Pts',(18.6245700875342,17.0906796617505,9.31825943560445));
#186332=CARTESIAN_POINT('Ctrl Pts',(18.7864580297341,17.0885079834089,9.30743879571178));
#186333=CARTESIAN_POINT('Ctrl Pts',(18.9957245827716,17.1096698884429,9.29371319855008));
#186334=CARTESIAN_POINT('Ctrl Pts',(19.0442732601583,17.1162878162427,9.29055236422752));
#186335=CARTESIAN_POINT('Ctrl Pts',(19.1184282446578,17.1290313877083,9.28580100344138));
#186336=CARTESIAN_POINT('Ctrl Pts',(19.1442213675224,17.1339595684642,9.28416283081811));
#186337=CARTESIAN_POINT('Ctrl Pts',(19.1765321006913,17.1407584607714,9.28213458330725));
#186338=CARTESIAN_POINT('Ctrl Pts',(19.1831401500072,17.1421820236199,9.28172103889861));
#186339=CARTESIAN_POINT('Ctrl Pts',(19.1936508829726,17.1444990702068,9.28106539596722));
#186340=CARTESIAN_POINT('Ctrl Pts',(19.1975579811754,17.1453720020882,9.28082214902407));
#186341=CARTESIAN_POINT('Ctrl Pts',(19.2049669237299,17.1470494031167,9.28036181190379));
#186342=CARTESIAN_POINT('Ctrl Pts',(19.208469151896,17.1478516937275,9.28014460674308));
#186343=CARTESIAN_POINT('Ctrl Pts',(19.216530265755,17.1497199458845,9.27964555528487));
#186344=CARTESIAN_POINT('Ctrl Pts',(19.2210876681024,17.1507921164578,9.2793640687497));
#186345=CARTESIAN_POINT('Ctrl Pts',(19.2333014469556,17.1537083132556,9.27861135622915));
#186346=CARTESIAN_POINT('Ctrl Pts',(19.2409512372471,17.1555799780351,9.27814167452741));
#186347=CARTESIAN_POINT('Ctrl Pts',(19.2983968703626,17.1699753505868,9.27462666534343));
#186348=CARTESIAN_POINT('Ctrl Pts',(19.3477370871842,17.1842653962878,9.27167563681548));
#186349=CARTESIAN_POINT('Ctrl Pts',(19.4099920486199,17.2047783855212,9.26798314539287));
#186350=CARTESIAN_POINT('Ctrl Pts',(19.4234265164141,17.2093552992916,9.26718819872463));
#186351=CARTESIAN_POINT('Ctrl Pts',(19.5717313164452,17.261550698438,9.25842355480264));
#186352=CARTESIAN_POINT('Ctrl Pts',(19.7014932310011,17.3225861032539,9.25082984792975));
#186353=CARTESIAN_POINT('Ctrl Pts',(19.9038144242271,17.4441192728222,9.23783195354945));
#186354=CARTESIAN_POINT('Ctrl Pts',(19.9802661958951,17.4971881769649,9.23261193212216));
#186355=CARTESIAN_POINT('Ctrl Pts',(20.0694828619276,17.5682523680661,9.22596822607224));
#186356=CARTESIAN_POINT('Ctrl Pts',(20.0857899748102,17.5816448903583,9.2247298216473));
#186357=CARTESIAN_POINT('Ctrl Pts',(20.1087325361757,17.6010684036486,9.22295148212606));
#186358=CARTESIAN_POINT('Ctrl Pts',(20.1155344106663,17.606901511959,9.22241963578056));
#186359=CARTESIAN_POINT('Ctrl Pts',(20.1272193417023,17.6170516495772,9.22149786041159));
#186360=CARTESIAN_POINT('Ctrl Pts',(20.1321199066549,17.6213484019889,9.22110877554216));
#186361=CARTESIAN_POINT('Ctrl Pts',(20.1414751013927,17.629627639607,9.22036116106304));
#186362=CARTESIAN_POINT('Ctrl Pts',(20.1459328709478,17.633606494861,9.22000278569393));
#186363=CARTESIAN_POINT('Ctrl Pts',(20.1575027846565,17.6440217513706,9.2190670187211));
#186364=CARTESIAN_POINT('Ctrl Pts',(20.1645880749135,17.650487659523,9.21848838232287));
#186365=CARTESIAN_POINT('Ctrl Pts',(20.1887107133792,17.6728039003838,9.21649893120954));
#186366=CARTESIAN_POINT('Ctrl Pts',(20.205530062419,17.6888864339084,9.21507820400915));
#186367=CARTESIAN_POINT('Ctrl Pts',(20.3440123295447,17.8257429593144,9.20309096646443));
#186368=CARTESIAN_POINT('Ctrl Pts',(20.4508344127262,17.9605862841972,9.19185696588243));
#186369=CARTESIAN_POINT('Ctrl Pts',(20.5871011322324,18.1834859995083,9.17459316183655));
#186370=CARTESIAN_POINT('Ctrl Pts',(20.6290565811356,18.2630910549778,9.16866181252265));
#186371=CARTESIAN_POINT('Ctrl Pts',(20.6815899466365,18.3802967761655,9.16045645100884));
#186372=CARTESIAN_POINT('Ctrl Pts',(20.6963915809533,18.4158936163153,9.15803093408932));
#186373=CARTESIAN_POINT('Ctrl Pts',(20.712943609435,18.4589832862587,9.15519024378226));
#186374=CARTESIAN_POINT('Ctrl Pts',(20.7156349591384,18.4661041416202,9.15472387695126));
#186375=CARTESIAN_POINT('Ctrl Pts',(20.7197484392224,18.4771677977887,9.15400421690796));
#186376=CARTESIAN_POINT('Ctrl Pts',(20.7211973375232,18.4811004813538,9.15374936914788));
#186377=CARTESIAN_POINT('Ctrl Pts',(20.7238563932898,18.4883844527164,9.15327916280796));
#186378=CARTESIAN_POINT('Ctrl Pts',(20.7250697590424,18.4917344648692,9.15306361888813));
#186379=CARTESIAN_POINT('Ctrl Pts',(20.7277858647258,18.4992929715216,9.1525788857334));
#186380=CARTESIAN_POINT('Ctrl Pts',(20.7292837361619,18.5035031577345,9.15230998768544));
#186381=CARTESIAN_POINT('Ctrl Pts',(20.7336427672952,18.5158793828259,9.1515226901763));
#186382=CARTESIAN_POINT('Ctrl Pts',(20.7364672462755,18.5240583703047,9.15100641550432));
#186383=CARTESIAN_POINT('Ctrl Pts',(20.7558471715588,18.5813131695926,9.14741889934705));
#186384=CARTESIAN_POINT('Ctrl Pts',(20.7706483470256,18.6309690169995,9.14444316253679));
#186385=CARTESIAN_POINT('Ctrl Pts',(20.7889950504447,18.7019356560429,9.14031552488931));
#186386=CARTESIAN_POINT('Ctrl Pts',(20.7940587001143,18.7228306040054,9.13911531609063));
#186387=CARTESIAN_POINT('Ctrl Pts',(20.8292197080863,18.8782254933424,9.13027766202423));
#186388=CARTESIAN_POINT('Ctrl Pts',(20.8464369297966,19.0153028105548,9.12294747445923));
#186389=CARTESIAN_POINT('Ctrl Pts',(20.8526907767981,19.2438180023166,9.11034417241446));
#186390=CARTESIAN_POINT('Ctrl Pts',(20.8493359483967,19.334607113795,9.10524185800939));
#186391=CARTESIAN_POINT('Ctrl Pts',(20.8380618606554,19.4456202746019,9.09874056226291));
#186392=CARTESIAN_POINT('Ctrl Pts',(20.8356512762426,19.4663132470701,9.09751770070753));
#186393=CARTESIAN_POINT('Ctrl Pts',(20.8317736957737,19.4958051783106,9.09575783048884));
#186394=CARTESIAN_POINT('Ctrl Pts',(20.8305558231179,19.504636075985,9.09522867922539));
#186395=CARTESIAN_POINT('Ctrl Pts',(20.8283522331054,19.5199014318079,9.09431008629121));
#186396=CARTESIAN_POINT('Ctrl Pts',(20.827392540083,19.5263395670572,9.09392147289336));
#186397=CARTESIAN_POINT('Ctrl Pts',(20.8254934472971,19.538688851528,9.09317371420938));
#186398=CARTESIAN_POINT('Ctrl Pts',(20.8245586400775,19.5446006516122,9.09281471812043));
#186399=CARTESIAN_POINT('Ctrl Pts',(20.8220516521553,19.5600306071277,9.09187499391617));
#186400=CARTESIAN_POINT('Ctrl Pts',(20.8204394712529,19.5695420404342,9.09129300025844));
#186401=CARTESIAN_POINT('Ctrl Pts',(20.8146594185818,19.6022829672878,9.0892800458128));
#186402=CARTESIAN_POINT('Ctrl Pts',(20.8101682690658,19.6254529218304,9.08783885528337));
#186403=CARTESIAN_POINT('Ctrl Pts',(20.7711451420421,19.8101853620767,9.07621038718791));
#186404=CARTESIAN_POINT('Ctrl Pts',(20.7182011930178,19.9672468774428,9.0654086352931));
#186405=CARTESIAN_POINT('Ctrl Pts',(20.5930554604647,20.2317049056693,9.04607413444419));
#186406=CARTESIAN_POINT('Ctrl Pts',(20.5282578836148,20.3417391809126,9.0376464110774));
#186407=CARTESIAN_POINT('Ctrl Pts',(20.4469596193446,20.4550265677872,9.02899833398777));
#186408=CARTESIAN_POINT('Ctrl Pts',(20.4398862408848,20.4647084618394,9.02825962761895));
#186409=CARTESIAN_POINT('Ctrl Pts',(20.4297252408377,20.4783714033376,9.02721834065978));
#186410=CARTESIAN_POINT('Ctrl Pts',(20.426705231929,20.4824021257711,9.02691129487356));
#186411=CARTESIAN_POINT('Ctrl Pts',(20.4214803329305,20.4893240378003,9.02638431608451));
#186412=CARTESIAN_POINT('Ctrl Pts',(20.4192823357679,20.4922203827491,9.02616390552331));
#186413=CARTESIAN_POINT('Ctrl Pts',(20.415009655659,20.4978205593769,9.0257379367387));
#186414=CARTESIAN_POINT('Ctrl Pts',(20.412935905607,20.5005250442304,9.02553231331246));
#186415=CARTESIAN_POINT('Ctrl Pts',(20.4073307962305,20.5077985163791,9.02497951222334));
#186416=CARTESIAN_POINT('Ctrl Pts',(20.4037872285638,20.5123581208878,9.02463319020381));
#186417=CARTESIAN_POINT('Ctrl Pts',(20.3906101418841,20.5291709985758,9.02335675283312));
#186418=CARTESIAN_POINT('Ctrl Pts',(20.3808597747519,20.541332611756,9.02243457556222));
#186419=CARTESIAN_POINT('Ctrl Pts',(20.2842999522995,20.6590827224316,9.01350484426809));
#186420=CARTESIAN_POINT('Ctrl Pts',(20.187578319304,20.756151758549,9.0061213883061));
#186421=CARTESIAN_POINT('Ctrl Pts',(19.9630191764834,20.9416295759864,8.99030479204379));
#186422=CARTESIAN_POINT('Ctrl Pts',(19.8334804035951,21.0266823094003,8.98188541975609));
#186423=CARTESIAN_POINT('Ctrl Pts',(19.6768994407564,21.106542681726,8.97164903787487));
#186424=CARTESIAN_POINT('Ctrl Pts',(19.6578075221962,21.1159202153943,8.97040086726002));
#186425=CARTESIAN_POINT('Ctrl Pts',(19.6304507513228,21.1288492789825,8.96861093279639));
#186426=CARTESIAN_POINT('Ctrl Pts',(19.6222991730791,21.1326384628103,8.968077404776));
#186427=CARTESIAN_POINT('Ctrl Pts',(19.6081915297166,21.139087320333,8.9671536403025));
#186428=CARTESIAN_POINT('Ctrl Pts',(19.6022468067036,21.1417716143131,8.9667642579435));
#186429=CARTESIAN_POINT('Ctrl Pts',(19.5908383018242,21.1468596940281,8.966016719406));
#186430=CARTESIAN_POINT('Ctrl Pts',(19.5853765647875,21.1492679314873,8.96565872058304));
#186431=CARTESIAN_POINT('Ctrl Pts',(19.57114234161,21.1554724394587,8.9647253646448));
#186432=CARTESIAN_POINT('Ctrl Pts',(19.5623542716346,21.1592324204027,8.96414877533224));
#186433=CARTESIAN_POINT('Ctrl Pts',(19.5322725792559,21.1718625611146,8.96217375435025));
#186434=CARTESIAN_POINT('Ctrl Pts',(19.5108601721294,21.1804439066081,8.96076560306096));
#186435=CARTESIAN_POINT('Ctrl Pts',(19.3263064582098,21.2509286086192,8.94860481058065));
#186436=CARTESIAN_POINT('Ctrl Pts',(19.1562580037787,21.2927806783011,8.93715751326993));
#186437=CARTESIAN_POINT('Ctrl Pts',(18.8959421557957,21.3236185655257,8.91983712157592));
#186438=CARTESIAN_POINT('Ctrl Pts',(18.8082760677541,21.3285144546901,8.91405462361345));
#186439=CARTESIAN_POINT('Ctrl Pts',(18.6825554902011,21.3277159560012,8.90602654579139));
#186440=CARTESIAN_POINT('Ctrl Pts',(18.6445671356337,21.326451524889,8.90363598349833));
#186441=CARTESIAN_POINT('Ctrl Pts',(18.5990627653466,21.323708788843,8.90083069806408));
#186442=CARTESIAN_POINT('Ctrl Pts',(18.5914970692073,21.3232119691119,8.90036622133922));
#186443=CARTESIAN_POINT('Ctrl Pts',(18.579760167528,21.3223778874392,8.8996488445639));
#186444=CARTESIAN_POINT('Ctrl Pts',(18.5755871066085,21.3220688916743,8.89939440537963));
#186445=CARTESIAN_POINT('Ctrl Pts',(18.5678619271626,21.3214738424368,8.89892457809114));
#186446=CARTESIAN_POINT('Ctrl Pts',(18.5643096452303,21.3211911957582,8.89870900704697));
#186447=CARTESIAN_POINT('Ctrl Pts',(18.5562959081252,21.3205331948837,8.89822374129377));
#186448=CARTESIAN_POINT('Ctrl Pts',(18.5518349327937,21.3201526577566,8.897954340639));
#186449=CARTESIAN_POINT('Ctrl Pts',(18.5387170287883,21.3189917246913,8.89716420447811));
#186450=CARTESIAN_POINT('Ctrl Pts',(18.530063539453,21.3181721515184,8.89664561681286));
#186451=CARTESIAN_POINT('Ctrl Pts',(18.468943507397,21.3120034216941,8.89299994260129));
#186452=CARTESIAN_POINT('Ctrl Pts',(18.4166832720523,21.3047481713275,8.88997192145887));
#186453=CARTESIAN_POINT('Ctrl Pts',(18.3492011147206,21.2927944152816,8.88611580775541));
#186454=CARTESIAN_POINT('Ctrl Pts',(18.3336889852804,21.2898673066634,8.8852331521866));
#186455=CARTESIAN_POINT('Ctrl Pts',(18.2683586240147,21.2767812228372,8.88152638802928));
#186456=CARTESIAN_POINT('Ctrl Pts',(18.2188806346554,21.2650025168272,8.87874487300235));
#186457=CARTESIAN_POINT('Ctrl Pts',(18.0644204639103,21.2222987187503,8.87001963641199));
#186458=CARTESIAN_POINT('Ctrl Pts',(17.9613874627891,21.1850132425348,8.86412865608804));
#186459=CARTESIAN_POINT('Ctrl Pts',(17.8114225751872,21.1171964404653,8.85497760027843));
#186460=CARTESIAN_POINT('Ctrl Pts',(17.7620546699484,21.0925035483122,8.85186623188849));
#186461=CARTESIAN_POINT('Ctrl Pts',(17.6836215478701,21.0493615891663,8.84671641334545));
#186462=CARTESIAN_POINT('Ctrl Pts',(17.6539415372318,21.032082575034,8.84471746757898));
#186463=CARTESIAN_POINT('Ctrl Pts',(17.6154867519729,21.008424275622,8.84205472349388));
#186464=CARTESIAN_POINT('Ctrl Pts',(17.6063211138068,21.0026880966497,8.84141450086276));
#186465=CARTESIAN_POINT('Ctrl Pts',(17.5913800242238,20.9931773724797,8.84036152887099));
#186466=CARTESIAN_POINT('Ctrl Pts',(17.5855782992451,20.9894443178026,8.83995032231926));
#186467=CARTESIAN_POINT('Ctrl Pts',(17.5743824825011,20.9821628664757,8.83915222667252));
#186468=CARTESIAN_POINT('Ctrl Pts',(17.5689861667969,20.978618016848,8.83876547329724));
#186469=CARTESIAN_POINT('Ctrl Pts',(17.5565627272509,20.9703754338939,8.83787023536037));
#186470=CARTESIAN_POINT('Ctrl Pts',(17.5495473896912,20.9656602119338,8.83736109531864));
#186471=CARTESIAN_POINT('Ctrl Pts',(17.5307542220067,20.9528646917018,8.83598732310633));
#186472=CARTESIAN_POINT('Ctrl Pts',(17.5190297750097,20.9447071099665,8.835119766423));
#186473=CARTESIAN_POINT('Ctrl Pts',(17.3924219245189,20.8547014690873,8.82563478892659));
#186474=CARTESIAN_POINT('Ctrl Pts',(17.2859326259487,20.7617010618435,8.81656767221894));
#186475=CARTESIAN_POINT('Ctrl Pts',(17.1234054373051,20.5883208351413,8.80093329491484));
#186476=CARTESIAN_POINT('Ctrl Pts',(17.0622207724101,20.5133754994165,8.79450512456632));
#186477=CARTESIAN_POINT('Ctrl Pts',(16.9686661036172,20.381273955029,8.78394198541052));
#186478=CARTESIAN_POINT('Ctrl Pts',(16.9334397172737,20.3263157397975,8.77974785945581));
#186479=CARTESIAN_POINT('Ctrl Pts',(16.8942250423268,20.2584207346613,8.7748764161203));
#186480=CARTESIAN_POINT('Ctrl Pts',(16.887751058384,20.246966677005,8.7740648272924));
#186481=CARTESIAN_POINT('Ctrl Pts',(16.8788540528302,20.2308773697379,8.77293982866617));
#186482=CARTESIAN_POINT('Ctrl Pts',(16.8763409391769,20.2262926423885,8.772620943944));
#186483=CARTESIAN_POINT('Ctrl Pts',(16.8720920954119,20.2184727949759,8.77207997594959));
#186484=CARTESIAN_POINT('Ctrl Pts',(16.8703477577309,20.2152424002171,8.77185734856318));
#186485=CARTESIAN_POINT('Ctrl Pts',(16.8670223269156,20.2090454239041,8.77143191907515));
#186486=CARTESIAN_POINT('Ctrl Pts',(16.8654398911147,20.206079604765,8.77122902887216));
#186487=CARTESIAN_POINT('Ctrl Pts',(16.8612708338858,20.1982208977377,8.77069327944462));
#186488=CARTESIAN_POINT('Ctrl Pts',(16.8586963034075,20.1933215754845,8.77036118282769));
#186489=CARTESIAN_POINT('Ctrl Pts',(16.8496512051845,20.175943625713,8.76918975715014));
#186490=CARTESIAN_POINT('Ctrl Pts',(16.8432855755135,20.163410400007,8.76835677297196));
#186491=CARTESIAN_POINT('Ctrl Pts',(16.8025847883873,20.0812584720126,8.76296776030849));
#186492=CARTESIAN_POINT('Ctrl Pts',(16.7720027251434,20.0099134727692,8.75861676559915));
#186493=CARTESIAN_POINT('Ctrl Pts',(16.7454192421517,19.937109888044,8.75434672885778));
#186494=CARTESIAN_POINT('',(16.6170000979998,19.2103558486173,9.29097292758594));
#186495=CARTESIAN_POINT('Ctrl Pts',(16.7454193934539,19.9371103024118,8.53521106676425));
#186496=CARTESIAN_POINT('Ctrl Pts',(16.7707333790309,20.0064370983899,8.5393534310353));
#186497=CARTESIAN_POINT('Ctrl Pts',(16.7996695295206,20.074431401749,8.54338075368839));
#186498=CARTESIAN_POINT('Ctrl Pts',(16.9057915083873,20.291498613237,8.55651367139851));
#186499=CARTESIAN_POINT('Ctrl Pts',(16.997098875721,20.432880142472,8.56556714308397));
#186500=CARTESIAN_POINT('Ctrl Pts',(17.1191104677879,20.58007705896,8.57667156062985));
#186501=CARTESIAN_POINT('Ctrl Pts',(17.1343922602669,20.5979012974354,8.57804656005877));
#186502=CARTESIAN_POINT('Ctrl Pts',(17.1563534133947,20.6226702588014,8.58000255688896));
#186503=CARTESIAN_POINT('Ctrl Pts',(17.1627889130972,20.6298295836901,8.58057339999643));
#186504=CARTESIAN_POINT('Ctrl Pts',(17.1733019002434,20.6413657643934,8.58150227841002));
#186505=CARTESIAN_POINT('Ctrl Pts',(17.1773495484935,20.6457697199295,8.58185904757045));
#186506=CARTESIAN_POINT('Ctrl Pts',(17.1858429072387,20.6549324867784,8.58260591348199));
#186507=CARTESIAN_POINT('Ctrl Pts',(17.1902920153215,20.6596880502063,8.58299615365754));
#186508=CARTESIAN_POINT('Ctrl Pts',(17.2008948676105,20.6709169239469,8.58392385193664));
#186509=CARTESIAN_POINT('Ctrl Pts',(17.2070677383426,20.6773719297212,8.5844621338399));
#186510=CARTESIAN_POINT('Ctrl Pts',(17.2278430917356,20.6988234074668,8.58626788715645));
#186511=CARTESIAN_POINT('Ctrl Pts',(17.2426267489851,20.7136419736238,8.58754326790624));
#186512=CARTESIAN_POINT('Ctrl Pts',(17.3232616674467,20.7921050453753,8.59445099681882));
#186513=CARTESIAN_POINT('Ctrl Pts',(17.3929624739339,20.8516371852736,8.60025765400415));
#186514=CARTESIAN_POINT('Ctrl Pts',(17.5419206392686,20.9630141532614,8.61232139834067));
#186515=CARTESIAN_POINT('Ctrl Pts',(17.6212468240622,21.0144371199192,8.61857368373425));
#186516=CARTESIAN_POINT('Ctrl Pts',(17.7685850356702,21.0965167811082,8.6297108964382));
#186517=CARTESIAN_POINT('Ctrl Pts',(17.8352936637507,21.1292095187879,8.63459302604559));
#186518=CARTESIAN_POINT('Ctrl Pts',(17.9424467809842,21.1749036002337,8.64206172980219));
#186519=CARTESIAN_POINT('Ctrl Pts',(17.9817987944551,21.1903099172229,8.64472884379296));
#186520=CARTESIAN_POINT('Ctrl Pts',(18.0286043463597,21.2070364428942,8.64779172992458));
#186521=CARTESIAN_POINT('Ctrl Pts',(18.0356335873533,21.209506659228,8.64824884936479));
#186522=CARTESIAN_POINT('Ctrl Pts',(18.0470291418612,21.2134438203127,8.64898512079277));
#186523=CARTESIAN_POINT('Ctrl Pts',(18.0513873874888,21.2149336904217,8.6492655787132));
#186524=CARTESIAN_POINT('Ctrl Pts',(18.0591363508275,21.2175544673072,8.64976218403288));
#186525=CARTESIAN_POINT('Ctrl Pts',(18.0625251002234,21.2186910207715,8.64997866165255));
#186526=CARTESIAN_POINT('Ctrl Pts',(18.0698013087,21.221110906632,8.65044197371743));
#186527=CARTESIAN_POINT('Ctrl Pts',(18.0736896053987,21.2223915436632,8.65068864872613));
#186528=CARTESIAN_POINT('Ctrl Pts',(18.0843955130379,21.2258832170086,8.6513653919139));
#186529=CARTESIAN_POINT('Ctrl Pts',(18.0912207483391,21.228070946854,8.65179410929906));
#186530=CARTESIAN_POINT('Ctrl Pts',(18.1280704630463,21.2396765514499,8.65409479170168));
#186531=CARTESIAN_POINT('Ctrl Pts',(18.1582927002294,21.2484593241625,8.65593179515854));
#186532=CARTESIAN_POINT('Ctrl Pts',(18.3467774085552,21.298704827258,8.66714516511271));
#186533=CARTESIAN_POINT('Ctrl Pts',(18.5092219756294,21.3223834013349,8.67579050159908));
#186534=CARTESIAN_POINT('Ctrl Pts',(18.7898605182821,21.3305014015687,8.69115899752462));
#186535=CARTESIAN_POINT('Ctrl Pts',(18.9069971212944,21.3241666512854,8.69769646181053));
#186536=CARTESIAN_POINT('Ctrl Pts',(19.037160292131,21.3062296169909,8.7053938810828));
#186537=CARTESIAN_POINT('Ctrl Pts',(19.0512998105927,21.3041349994487,8.7062356112971));
#186538=CARTESIAN_POINT('Ctrl Pts',(19.0737683370982,21.3005736354431,8.70758248036757));
#186539=CARTESIAN_POINT('Ctrl Pts',(19.0821117931145,21.299199865234,8.70808467602384));
#186540=CARTESIAN_POINT('Ctrl Pts',(19.0968115301044,21.2966889716874,8.70897316419808));
#186541=CARTESIAN_POINT('Ctrl Pts',(19.1031712938687,21.2955726773977,8.70935879032419));
#186542=CARTESIAN_POINT('Ctrl Pts',(19.1163141392255,21.2932037550712,8.71015829004696));
#186543=CARTESIAN_POINT('Ctrl Pts',(19.1230963971161,21.2919470369723,8.71057228981612));
#186544=CARTESIAN_POINT('Ctrl Pts',(19.140488597262,21.2886363515486,8.71163765246111));
#186545=CARTESIAN_POINT('Ctrl Pts',(19.1510890764613,21.2865342648327,8.71229054402126));
#186546=CARTESIAN_POINT('Ctrl Pts',(19.1952560094763,21.2774238939222,8.71502598067293));
#186547=CARTESIAN_POINT('Ctrl Pts',(19.2286642503852,21.2696820733236,8.717131843797));
#186548=CARTESIAN_POINT('Ctrl Pts',(19.3152006953957,21.2474006645485,8.72268611991857));
#186549=CARTESIAN_POINT('Ctrl Pts',(19.3679729777837,21.2315938134161,8.72617291489086));
#186550=CARTESIAN_POINT('Ctrl Pts',(19.523531182944,21.1783054790676,8.7367418925451));
#186551=CARTESIAN_POINT('Ctrl Pts',(19.6240874605982,21.1348999929048,8.74397246793019));
#186552=CARTESIAN_POINT('Ctrl Pts',(19.7612298644618,21.0626405847473,8.75421235438756));
#186553=CARTESIAN_POINT('Ctrl Pts',(19.8009293902062,21.0400532841605,8.75722312466314));
#186554=CARTESIAN_POINT('Ctrl Pts',(19.8593541487939,21.0042621778817,8.7616985698565));
#186555=CARTESIAN_POINT('Ctrl Pts',(19.878646074205,20.9920099989053,8.76318389081542));
#186556=CARTESIAN_POINT('Ctrl Pts',(19.8983376726445,20.9790518381292,8.76470519208233));
#186557=CARTESIAN_POINT('Ctrl Pts',(19.8989388408954,20.9786557965923,8.76475164120195));
#186558=CARTESIAN_POINT('Ctrl Pts',(19.9093096320504,20.9718160708575,8.76555302357388));
#186559=CARTESIAN_POINT('Ctrl Pts',(19.9190260227094,20.9652916807653,8.76630515239283));
#186560=CARTESIAN_POINT('Ctrl Pts',(19.9615144178983,20.9362473632967,8.76959831909168));
#186561=CARTESIAN_POINT('Ctrl Pts',(19.9937046455668,20.912885655489,8.77210452662167));
#186562=CARTESIAN_POINT('Ctrl Pts',(20.0310177805011,20.8841668794075,8.77500517654869));
#186563=CARTESIAN_POINT('Ctrl Pts',(20.0367926069563,20.8796743109737,8.77545396810254));
#186564=CARTESIAN_POINT('Ctrl Pts',(20.0461328811133,20.8723299324777,8.77617947322858));
#186565=CARTESIAN_POINT('Ctrl Pts',(20.0497125418777,20.8694964125053,8.77645743264842));
#186566=CARTESIAN_POINT('Ctrl Pts',(20.0560753336055,20.864426309135,8.77695129648943));
#186567=CARTESIAN_POINT('Ctrl Pts',(20.0588619932381,20.8621942487141,8.7771675172768));
#186568=CARTESIAN_POINT('Ctrl Pts',(20.0648524964655,20.8573710427763,8.77763216412739));
#186569=CARTESIAN_POINT('Ctrl Pts',(20.0680544164151,20.8547775982625,8.77788042082209));
#186570=CARTESIAN_POINT('Ctrl Pts',(20.0768991123255,20.8475708346685,8.77856597875068));
#186571=CARTESIAN_POINT('Ctrl Pts',(20.0825257287828,20.8429376474286,8.77900187019559));
#186572=CARTESIAN_POINT('Ctrl Pts',(20.1136733879469,20.817018292085,8.78141429106097));
#186573=CARTESIAN_POINT('Ctrl Pts',(20.1387159212892,20.7951612514057,8.78335171941658));
#186574=CARTESIAN_POINT('Ctrl Pts',(20.2828169990551,20.6632848617021,8.79455868187381));
#186575=CARTESIAN_POINT('Ctrl Pts',(20.389446226444,20.5404641003221,8.80312774843457));
#186576=CARTESIAN_POINT('Ctrl Pts',(20.5468965738085,20.3104089037244,8.81839031467752));
#186577=CARTESIAN_POINT('Ctrl Pts',(20.6046978678858,20.2088868522372,8.82490242911166));
#186578=CARTESIAN_POINT('Ctrl Pts',(20.6598628768075,20.0901730826768,8.83257131253773));
#186579=CARTESIAN_POINT('Ctrl Pts',(20.6657523261035,20.0771559127899,8.8334126748036));
#186580=CARTESIAN_POINT('Ctrl Pts',(20.6749161301474,20.0563431525228,8.83475906508666));
#186581=CARTESIAN_POINT('Ctrl Pts',(20.6782763867676,20.0485856962002,8.83526115321533));
#186582=CARTESIAN_POINT('Ctrl Pts',(20.684120912583,20.0348683847638,8.83614951613709));
#186583=CARTESIAN_POINT('Ctrl Pts',(20.6866245632216,20.0289168678936,8.83653512514127));
#186584=CARTESIAN_POINT('Ctrl Pts',(20.6917467682554,20.0165831306335,8.83733465319021));
#186585=CARTESIAN_POINT('Ctrl Pts',(20.6943614284052,20.0101993851627,8.83774869872205));
#186586=CARTESIAN_POINT('Ctrl Pts',(20.7009932023591,19.9937794097391,8.83881431357548));
#186587=CARTESIAN_POINT('Ctrl Pts',(20.7049646915113,19.9837250743088,8.83946741297881));
#186588=CARTESIAN_POINT('Ctrl Pts',(20.7212224979436,19.9416254777837,8.84220486402173));
#186589=CARTESIAN_POINT('Ctrl Pts',(20.7328050882426,19.9093157221215,8.84431257666857));
#186590=CARTESIAN_POINT('Ctrl Pts',(20.7609359556144,19.824400157788,8.84987289449645));
#186591=CARTESIAN_POINT('Ctrl Pts',(20.7762224790125,19.7714066788445,8.85336398583704));
#186592=CARTESIAN_POINT('Ctrl Pts',(20.8156217323103,19.6116409701314,8.86394121614207));
#186593=CARTESIAN_POINT('Ctrl Pts',(20.8335429627489,19.5035373580111,8.8711757202685));
#186594=CARTESIAN_POINT('Ctrl Pts',(20.8474041199237,19.3442635919094,8.88173661362823));
#186595=CARTESIAN_POINT('Ctrl Pts',(20.8499805205521,19.2938424506443,8.88506354649273));
#186596=CARTESIAN_POINT('Ctrl Pts',(20.8509988449089,19.2272645826091,8.88940321332845));
#186597=CARTESIAN_POINT('Ctrl Pts',(20.8510613222928,19.2111503441033,8.89044940917388));
#186598=CARTESIAN_POINT('Ctrl Pts',(20.8505413610625,19.1421968553651,8.89490447670405));
#186599=CARTESIAN_POINT('Ctrl Pts',(20.8481646395735,19.0893854716826,8.89826254618084));
#186600=CARTESIAN_POINT('Ctrl Pts',(20.8430978029372,19.0280490469424,8.90205894433047));
#186601=CARTESIAN_POINT('Ctrl Pts',(20.842328628064,19.0193884251656,8.9025925639966));
#186602=CARTESIAN_POINT('Ctrl Pts',(20.8410825189931,19.0062750441389,8.90339660857446));
#186603=CARTESIAN_POINT('Ctrl Pts',(20.8406447887768,19.0018187767251,8.90366915550236));
#186604=CARTESIAN_POINT('Ctrl Pts',(20.8398333041824,18.9938185231043,8.90415717641673));
#186605=CARTESIAN_POINT('Ctrl Pts',(20.839464738958,18.9902740783354,8.90437293664061));
#186606=CARTESIAN_POINT('Ctrl Pts',(20.8386439729184,18.9825700255041,8.90484091398196));
#186607=CARTESIAN_POINT('Ctrl Pts',(20.8381883915918,18.9784108356438,8.90509293856372));
#186608=CARTESIAN_POINT('Ctrl Pts',(20.8368728095645,18.9667206488736,8.9057996187306));
#186609=CARTESIAN_POINT('Ctrl Pts',(20.8359846785952,18.9591927930324,8.90625271857221));
#186610=CARTESIAN_POINT('Ctrl Pts',(20.8304053367159,18.9139897748609,8.90896253630085));
#186611=CARTESIAN_POINT('Ctrl Pts',(20.8247414451538,18.8764390597623,8.9111679320323));
#186612=CARTESIAN_POINT('Ctrl Pts',(20.8026836505075,18.752844381319,8.91833491903559));
#186613=CARTESIAN_POINT('Ctrl Pts',(20.7819608713346,18.6676609568276,8.92312829340249));
#186614=CARTESIAN_POINT('Ctrl Pts',(20.7042885988098,18.4171746002083,8.93739582605823));
#186615=CARTESIAN_POINT('Ctrl Pts',(20.6321197415067,18.2574117042414,8.94678989527399));
#186616=CARTESIAN_POINT('Ctrl Pts',(20.5291465987849,18.0886501645176,8.95827704152751));
#186617=CARTESIAN_POINT('Ctrl Pts',(20.5168185540834,18.0691688364069,8.95962758848565));
#186618=CARTESIAN_POINT('Ctrl Pts',(20.4989337854135,18.0419024599577,8.96155461648782));
#186619=CARTESIAN_POINT('Ctrl Pts',(20.4936384184402,18.0339473432233,8.96212135021274));
#186620=CARTESIAN_POINT('Ctrl Pts',(20.4849485019721,18.0210823688148,8.96304535197681));
#186621=CARTESIAN_POINT('Ctrl Pts',(20.481586691658,18.0161504782693,8.9634013803295));
#186622=CARTESIAN_POINT('Ctrl Pts',(20.4745072955408,18.00585855428,8.96414816604074));
#186623=CARTESIAN_POINT('Ctrl Pts',(20.4707857079106,18.0005013616934,8.96453907332771));
#186624=CARTESIAN_POINT('Ctrl Pts',(20.4618756257479,17.987801053287,8.96547106243703));
#186625=CARTESIAN_POINT('Ctrl Pts',(20.4566650238094,17.9804736682464,8.96601298864685));
#186626=CARTESIAN_POINT('Ctrl Pts',(20.4389645798133,17.9559152686154,8.96784371992947));
#186627=CARTESIAN_POINT('Ctrl Pts',(20.4262619453185,17.9388398851153,8.96914073630141));
#186628=CARTESIAN_POINT('Ctrl Pts',(20.3163310565787,17.7956268458123,8.9802292688884));
#186629=CARTESIAN_POINT('Ctrl Pts',(20.2054297812672,17.6806637677722,8.99059332796988));
#186630=CARTESIAN_POINT('Ctrl Pts',(19.9812007735863,17.4953294479985,9.00980967430905));
#186631=CARTESIAN_POINT('Ctrl Pts',(19.8720662794367,17.4210708213553,9.01855491827325));
#186632=CARTESIAN_POINT('Ctrl Pts',(19.7429111980303,17.3498078320537,9.02775812765303));
#186633=CARTESIAN_POINT('Ctrl Pts',(19.729007194783,17.3423376956487,9.02873471550535));
#186634=CARTESIAN_POINT('Ctrl Pts',(19.7098769976273,17.3323337774844,9.03005777381811));
#186635=CARTESIAN_POINT('Ctrl Pts',(19.7047223986525,17.3296651768764,9.03041224398883));
#186636=CARTESIAN_POINT('Ctrl Pts',(19.6965187462765,17.3254607356707,9.03097310171822));
#186637=CARTESIAN_POINT('Ctrl Pts',(19.6934768856401,17.3239110353334,9.03118034924952));
#186638=CARTESIAN_POINT('Ctrl Pts',(19.6871908520463,17.3207276935028,9.03160713364915));
#186639=CARTESIAN_POINT('Ctrl Pts',(19.6839462220329,17.3190950424166,9.03182660278023));
#186640=CARTESIAN_POINT('Ctrl Pts',(19.6762115503046,17.3152279812235,9.03234785992133));
#186641=CARTESIAN_POINT('Ctrl Pts',(19.6717177050944,17.3130011434581,9.03264917479978));
#186642=CARTESIAN_POINT('Ctrl Pts',(19.6565657351984,17.3055598281373,9.03366010467592));
#186643=CARTESIAN_POINT('Ctrl Pts',(19.6458714741732,17.300418880699,9.03436528884837));
#186644=CARTESIAN_POINT('Ctrl Pts',(19.5223241343228,17.242300858796,9.04242297514951));
#186645=CARTESIAN_POINT('Ctrl Pts',(19.4050297579828,17.1992944630783,9.04922979631553));
#186646=CARTESIAN_POINT('Ctrl Pts',(19.1220702337999,17.1230753835632,9.06515897295743));
#186647=CARTESIAN_POINT('Ctrl Pts',(18.9549014802433,17.0988391837974,9.07424240420731));
#186648=CARTESIAN_POINT('Ctrl Pts',(18.7631944423158,17.0940714720116,9.08538062365513));
#186649=CARTESIAN_POINT('Ctrl Pts',(18.7397484958448,17.0938779916243,9.0867537966696));
#186650=CARTESIAN_POINT('Ctrl Pts',(18.7066838299938,17.0941543757055,9.08870762755243));
#186651=CARTESIAN_POINT('Ctrl Pts',(18.6970636066579,17.0943003830393,9.08927816178767));
#186652=CARTESIAN_POINT('Ctrl Pts',(18.6814657282565,17.0946434805853,9.09020667340948));
#186653=CARTESIAN_POINT('Ctrl Pts',(18.6754872567324,17.0948003343914,9.09056338664541));
#186654=CARTESIAN_POINT('Ctrl Pts',(18.6629994987755,17.0951809270853,9.09131024509307));
#186655=CARTESIAN_POINT('Ctrl Pts',(18.656490428226,17.0954093767234,9.09170053421352));
#186656=CARTESIAN_POINT('Ctrl Pts',(18.641053696506,17.0960224976979,9.09262854922548));
#186657=CARTESIAN_POINT('Ctrl Pts',(18.6321272656718,17.0964336631945,9.09316710043475));
#186658=CARTESIAN_POINT('Ctrl Pts',(18.6022753854696,17.0979981476717,9.09497469118979));
#186659=CARTESIAN_POINT('Ctrl Pts',(18.5813650193629,17.0994056461668,9.09625166208203));
#186660=CARTESIAN_POINT('Ctrl Pts',(18.4689977468757,17.1086469529097,9.10317411768674));
#186661=CARTESIAN_POINT('Ctrl Pts',(18.3781139811271,17.1221113341864,9.1089947447229));
#186662=CARTESIAN_POINT('Ctrl Pts',(18.1513559762775,17.1709346404093,9.1240412595165));
#186663=CARTESIAN_POINT('Ctrl Pts',(18.0175919036499,17.2139780693049,9.13342403371388));
#186664=CARTESIAN_POINT('Ctrl Pts',(17.8259582696312,17.2973943028361,9.14705017370816));
#186665=CARTESIAN_POINT('Ctrl Pts',(17.7642184589406,17.3279300828075,9.15146497331408));
#186666=CARTESIAN_POINT('Ctrl Pts',(17.6959109174147,17.3659668614466,9.15629247252829));
#186667=CARTESIAN_POINT('Ctrl Pts',(17.6877812076023,17.3705645972942,9.15686605679635));
#186668=CARTESIAN_POINT('Ctrl Pts',(17.6757366186877,17.3774819836445,9.15771410368726));
#186669=CARTESIAN_POINT('Ctrl Pts',(17.6717984876837,17.3797606249721,9.1579911033273));
#186670=CARTESIAN_POINT('Ctrl Pts',(17.6648889400269,17.383788345756,9.15847657074113));
#186671=CARTESIAN_POINT('Ctrl Pts',(17.6619144263182,17.3855320021261,9.15868538407952));
#186672=CARTESIAN_POINT('Ctrl Pts',(17.6555033720541,17.389311229614,9.15913505463748));
#186673=CARTESIAN_POINT('Ctrl Pts',(17.6520683380182,17.3913492554754,9.15937574898482));
#186674=CARTESIAN_POINT('Ctrl Pts',(17.6449785466941,17.395582843679,9.15987208363725));
#186675=CARTESIAN_POINT('Ctrl Pts',(17.6413246092274,17.3977797518398,9.16012763614554));
#186676=CARTESIAN_POINT('Ctrl Pts',(17.6321211229603,17.4033512164634,9.16077075504814));
#186677=CARTESIAN_POINT('Ctrl Pts',(17.6265803770579,17.4067403276081,9.16115741104872));
#186678=CARTESIAN_POINT('Ctrl Pts',(17.6107923423075,17.4164975304387,9.16225793850135));
#186679=CARTESIAN_POINT('Ctrl Pts',(17.6005836022289,17.4229278988107,9.16296806836283));
#186680=CARTESIAN_POINT('Ctrl Pts',(17.5662421936137,17.4449714547255,9.16535381211929));
#186681=CARTESIAN_POINT('Ctrl Pts',(17.5423717695735,17.4609893041071,9.16700694129817));
#186682=CARTESIAN_POINT('Ctrl Pts',(17.4287621384894,17.5406280153867,9.17488717422829));
#186683=CARTESIAN_POINT('Ctrl Pts',(17.3437410750251,17.6106961488667,9.18082889373141));
#186684=CARTESIAN_POINT('Ctrl Pts',(17.1599907382053,17.7878767883132,9.19469283800449));
#186685=CARTESIAN_POINT('Ctrl Pts',(17.0661011901421,17.8991723322635,9.20262350572933));
#186686=CARTESIAN_POINT('Ctrl Pts',(16.9708166169588,18.0390567821129,9.2124484074637));
#186687=CARTESIAN_POINT('Ctrl Pts',(16.9576268383166,18.0591472015648,9.21385537328414));
#186688=CARTESIAN_POINT('Ctrl Pts',(16.9395871698974,18.0876718799658,9.21584932050586));
#186689=CARTESIAN_POINT('Ctrl Pts',(16.9344487309834,18.0959221123655,9.21642560399533));
#186690=CARTESIAN_POINT('Ctrl Pts',(16.9262311968928,18.1093208552034,9.21736094927235));
#186691=CARTESIAN_POINT('Ctrl Pts',(16.9231168153573,18.1144476419223,9.21771870960385));
#186692=CARTESIAN_POINT('Ctrl Pts',(16.9166737686729,18.1251562702191,9.21846574364963));
#186693=CARTESIAN_POINT('Ctrl Pts',(16.9133489375958,18.1307403348829,9.21885515237451));
#186694=CARTESIAN_POINT('Ctrl Pts',(16.9055544185879,18.1439694567169,9.21977741952153));
#186695=CARTESIAN_POINT('Ctrl Pts',(16.9011069111751,18.151627381089,9.22031107575355));
#186696=CARTESIAN_POINT('Ctrl Pts',(16.8865271959018,18.177098074261,9.22208547440209));
#186697=CARTESIAN_POINT('Ctrl Pts',(16.8766058305006,18.1950296231209,9.22333375552151));
#186698=CARTESIAN_POINT('Ctrl Pts',(16.8254558304671,18.2907305574893,9.22999307239614));
#186699=CARTESIAN_POINT('Ctrl Pts',(16.7888520233515,18.3708615246763,9.23556468886471));
#186700=CARTESIAN_POINT('Ctrl Pts',(16.6888533288183,18.6316407808105,9.25364607310298));
#186701=CARTESIAN_POINT('Ctrl Pts',(16.6448918386729,18.8186948884003,9.26662241364255));
#186702=CARTESIAN_POINT('Ctrl Pts',(16.6241532271636,19.0351570266968,9.28035987111827));
#186703=CARTESIAN_POINT('Ctrl Pts',(16.6221401954149,19.0612586674574,9.28199387235902));
#186704=CARTESIAN_POINT('Ctrl Pts',(16.6202046990117,19.094350894635,9.28403146023798));
#186705=CARTESIAN_POINT('Ctrl Pts',(16.6198320670718,19.1013116106487,9.28445814794421));
#186706=CARTESIAN_POINT('Ctrl Pts',(16.6192953239796,19.1123599163827,9.28513224516597));
#186707=CARTESIAN_POINT('Ctrl Pts',(16.6191086720113,19.1164462886426,9.28538088456156));
#186708=CARTESIAN_POINT('Ctrl Pts',(16.6187836663883,19.1240447502766,9.2858419146969));
#186709=CARTESIAN_POINT('Ctrl Pts',(16.6186422162379,19.1275566041032,9.28605447119874));
#186710=CARTESIAN_POINT('Ctrl Pts',(16.6183781735427,19.1345448679932,9.2864764145905));
#186711=CARTESIAN_POINT('Ctrl Pts',(16.6182554037768,19.1380212103176,9.28668580992454));
#186712=CARTESIAN_POINT('Ctrl Pts',(16.6179937476174,19.145986829088,9.28716449546407));
#186713=CARTESIAN_POINT('Ctrl Pts',(16.617860577756,19.1504762941652,9.28743347133359));
#186714=CARTESIAN_POINT('Ctrl Pts',(16.6175253050956,19.1631387138012,9.28818990071531));
#186715=CARTESIAN_POINT('Ctrl Pts',(16.6173562536601,19.1713125623867,9.28867559512321));
#186716=CARTESIAN_POINT('Ctrl Pts',(16.6170813859026,19.1897759473539,9.28976724649768));
#186717=CARTESIAN_POINT('Ctrl Pts',(16.6170032290323,19.2000657276411,9.29037180813144));
#186718=CARTESIAN_POINT('Ctrl Pts',(16.6170000979998,19.2103558486173,9.29097292758594));
#186719=CARTESIAN_POINT('Ctrl Pts',(16.6170000985829,19.2103539350032,9.29097281579803));
#186720=CARTESIAN_POINT('Ctrl Pts',(16.6169387584115,19.411350951311,9.3027144953519));
#186721=CARTESIAN_POINT('Ctrl Pts',(16.6455016513076,19.6113762936101,9.31315911815543));
#186722=CARTESIAN_POINT('Ctrl Pts',(16.7149256836481,19.8491205389225,9.32683326560889));
#186723=CARTESIAN_POINT('Ctrl Pts',(16.7294513745603,19.8933790755415,9.32943087882338));
#186724=CARTESIAN_POINT('Ctrl Pts',(16.7454193811439,19.9371102686989,9.33206801830577));
#186725=CARTESIAN_POINT('Origin',(18.734,19.211,0.));
#186726=CARTESIAN_POINT('',(16.7454193623258,19.9371102171621,10.3555828633409));
#186727=CARTESIAN_POINT('',(16.74541937607,19.9371102548029,10.1325348912934));
#186728=CARTESIAN_POINT('',(16.7454193623258,19.9371102171621,0.));
#186729=CARTESIAN_POINT('',(16.6146463426453,19.2099228989265,10.3109437268626));
#186730=CARTESIAN_POINT('Ctrl Pts',(16.6170002731508,19.2099245836057,10.3109437563774));
#186731=CARTESIAN_POINT('Ctrl Pts',(16.6169638477094,19.28162950639,10.3152783077146));
#186732=CARTESIAN_POINT('Ctrl Pts',(16.6205747319164,19.353482380977,10.3196128590518));
#186733=CARTESIAN_POINT('Ctrl Pts',(16.6278517403654,19.4250759408207,10.3239474103889));
#186734=CARTESIAN_POINT('Ctrl Pts',(16.6351199717677,19.4965831492434,10.3282767336767));
#186735=CARTESIAN_POINT('Ctrl Pts',(16.646045514733,19.5678311749636,10.3326060569645));
#186736=CARTESIAN_POINT('Ctrl Pts',(16.6605951836038,19.6384125259569,10.3369353802523));
#186737=CARTESIAN_POINT('Ctrl Pts',(16.6751308912189,19.7089261500286,10.341260549302));
#186738=CARTESIAN_POINT('Ctrl Pts',(16.6932837245209,19.7787738865221,10.3455857183516));
#186739=CARTESIAN_POINT('Ctrl Pts',(16.7149688972743,19.8475551085539,10.3499108874013));
#186740=CARTESIAN_POINT('Ctrl Pts',(16.7244481243049,19.877621404382,10.3518015460478));
#186741=CARTESIAN_POINT('Ctrl Pts',(16.7346016565717,19.9074840258511,10.3536922046944));
#186742=CARTESIAN_POINT('Ctrl Pts',(16.7454193623258,19.9371102171621,10.3555828633409));
#186743=CARTESIAN_POINT('Ctrl Pts',(16.7437494103711,19.9377357416701,9.55561790998273));
#186744=CARTESIAN_POINT('Ctrl Pts',(16.9543731788316,20.4984180339644,9.59172752395545));
#186745=CARTESIAN_POINT('Ctrl Pts',(17.9482900406235,21.5302730916103,9.67022907348861));
#186746=CARTESIAN_POINT('Ctrl Pts',(20.2082247613025,21.2341144439156,9.79112255858232));
#186747=CARTESIAN_POINT('Ctrl Pts',(21.2330889849398,19.0664837539622,9.91829836526373));
#186748=CARTESIAN_POINT('Ctrl Pts',(19.9651941758505,17.0314377500589,10.0454741719452));
#186749=CARTESIAN_POINT('Ctrl Pts',(17.5677551269472,16.9960048315866,10.1726499786266));
#186750=CARTESIAN_POINT('Ctrl Pts',(16.6440836776345,18.3853146100795,10.2611398283041));
#186751=CARTESIAN_POINT('Ctrl Pts',(16.6137958787386,19.1485339243465,10.307237742421));
#186752=CARTESIAN_POINT('Ctrl Pts',(16.6141769831468,19.2099225630116,10.3109437209775));
#186753=CARTESIAN_POINT('Ctrl Pts',(16.7454193811439,19.9371102686989,9.33206801830577));
#186754=CARTESIAN_POINT('Ctrl Pts',(16.7596281007385,19.9760233451594,9.33441460898639));
#186755=CARTESIAN_POINT('Ctrl Pts',(16.7749788270604,20.0145188815229,9.33679243678394));
#186756=CARTESIAN_POINT('Ctrl Pts',(16.799600250514,20.0713526206786,9.34040242819754));
#186757=CARTESIAN_POINT('Ctrl Pts',(16.8080196105005,20.0900384055731,9.34160574272052));
#186758=CARTESIAN_POINT('Ctrl Pts',(16.8204636459809,20.1166191537079,9.34334235730709));
#186759=CARTESIAN_POINT('Ctrl Pts',(16.8242688215022,20.1246160309219,9.34386808618027));
#186760=CARTESIAN_POINT('Ctrl Pts',(16.8309532210406,20.1384395906669,9.34478264772074));
#186761=CARTESIAN_POINT('Ctrl Pts',(16.833809326711,20.1442773654905,9.34517067219684));
#186762=CARTESIAN_POINT('Ctrl Pts',(16.8393532075784,20.1554779058867,9.34591865544923));
#186763=CARTESIAN_POINT('Ctrl Pts',(16.8420369875027,20.1608425874493,9.3462784715275));
#186764=CARTESIAN_POINT('Ctrl Pts',(16.8491288389102,20.1748693734016,9.3472233930721));
#186765=CARTESIAN_POINT('Ctrl Pts',(16.8535737882089,20.1835125808802,9.34780979147014));
#186766=CARTESIAN_POINT('Ctrl Pts',(16.8692147876912,20.2134183538443,9.34985337542285));
#186767=CARTESIAN_POINT('Ctrl Pts',(16.8807129028743,20.234520056051,9.35132121027353));
#186768=CARTESIAN_POINT('Ctrl Pts',(16.9644481534212,20.3821548241038,9.36177890161196));
#186769=CARTESIAN_POINT('Ctrl Pts',(17.0492075563428,20.5011077237472,9.3712345550802));
#186770=CARTESIAN_POINT('Ctrl Pts',(17.2361105315342,20.713268522094,9.38989437635894));
#186771=CARTESIAN_POINT('Ctrl Pts',(17.336517670782,20.8070990942191,9.39902731688534));
#186772=CARTESIAN_POINT('Ctrl Pts',(17.4553852073467,20.898304007343,9.40841002993629));
#186773=CARTESIAN_POINT('Ctrl Pts',(17.4655404945254,20.9059516515597,9.40920105765478));
#186774=CARTESIAN_POINT('Ctrl Pts',(17.4811848239039,20.9175135700109,9.410402799992));
#186775=CARTESIAN_POINT('Ctrl Pts',(17.4866245144744,20.9214937389326,9.41081758410069));
#186776=CARTESIAN_POINT('Ctrl Pts',(17.4956182803278,20.9280086693425,9.41149819785481));
#186777=CARTESIAN_POINT('Ctrl Pts',(17.4991613057385,20.9305585055886,9.41176500808274));
#186778=CARTESIAN_POINT('Ctrl Pts',(17.5060249205051,20.9354659428674,9.41227930598831));
#186779=CARTESIAN_POINT('Ctrl Pts',(17.5093444726057,20.9378249546025,9.41252688810126));
#186780=CARTESIAN_POINT('Ctrl Pts',(17.5126805298925,20.940181237487,9.41277452751432));
#186781=CARTESIAN_POINT('Ctrl Pts',(17.5126902162028,20.9401880788803,9.41277524653049));
#186782=CARTESIAN_POINT('Ctrl Pts',(17.5127096231875,20.9402017856938,9.41277668709386));
#186783=CARTESIAN_POINT('Ctrl Pts',(17.5127193439062,20.9402086511444,9.41277740864427));
#186784=CARTESIAN_POINT('Ctrl Pts',(17.5127388197587,20.9402224061058,9.41277885427966));
#186785=CARTESIAN_POINT('Ctrl Pts',(17.5127485751299,20.9402292957833,9.4127795783822));
#186786=CARTESIAN_POINT('Ctrl Pts',(17.5127687274431,20.9402435279888,9.41278107418778));
#186787=CARTESIAN_POINT('Ctrl Pts',(17.5127791240243,20.940250870245,9.41278184586269));
#186788=CARTESIAN_POINT('Ctrl Pts',(17.5128000847218,20.9402656727906,9.4127834016246));
#186789=CARTESIAN_POINT('Ctrl Pts',(17.5128106488415,20.9402731330777,9.41278418571149));
#186790=CARTESIAN_POINT('Ctrl Pts',(17.5128319477846,20.9402881739089,9.41278576653144));
#186791=CARTESIAN_POINT('Ctrl Pts',(17.5128426830051,20.9402957547286,9.41278656329358));
#186792=CARTESIAN_POINT('Ctrl Pts',(17.5128643283085,20.9403110395475,9.41278816977154));
#186793=CARTESIAN_POINT('Ctrl Pts',(17.512875237834,20.9403187431481,9.41278897944558));
#186794=CARTESIAN_POINT('Ctrl Pts',(17.5128972351988,20.940334275951,9.41279061200228));
#186795=CARTESIAN_POINT('Ctrl Pts',(17.5129083234166,20.9403421054155,9.41279143491261));
#186796=CARTESIAN_POINT('Ctrl Pts',(17.5129306815463,20.9403578923176,9.4127930941915));
#186797=CARTESIAN_POINT('Ctrl Pts',(17.5129419520928,20.9403658501981,9.41279393060673));
#186798=CARTESIAN_POINT('Ctrl Pts',(17.5129646793556,20.9403818970764,9.41279561722627));
#186799=CARTESIAN_POINT('Ctrl Pts',(17.5129761358252,20.9403899858945,9.41279646741182));
#186800=CARTESIAN_POINT('Ctrl Pts',(17.5129992393282,20.940406297734,9.41279818189675));
#186801=CARTESIAN_POINT('Ctrl Pts',(17.5130108860964,20.9404145205624,9.41279904617598));
#186802=CARTESIAN_POINT('Ctrl Pts',(17.5130343743115,20.9404311033103,9.4128007891522));
#186803=CARTESIAN_POINT('Ctrl Pts',(17.5130462156395,20.94043946314,9.41280166783989));
#186804=CARTESIAN_POINT('Ctrl Pts',(17.51307009722,20.9404563228699,9.41280343994664));
#186805=CARTESIAN_POINT('Ctrl Pts',(17.5130821374053,20.9404648227167,9.41280433336023));
#186806=CARTESIAN_POINT('Ctrl Pts',(17.513106420893,20.940481965422,9.41280613522834));
#186807=CARTESIAN_POINT('Ctrl Pts',(17.5131186644979,20.9404906084877,9.4128070437048));
#186808=CARTESIAN_POINT('Ctrl Pts',(17.513143359442,20.9405080408711,9.41280887603971));
#186809=CARTESIAN_POINT('Ctrl Pts',(17.513155810855,20.9405168302342,9.41280979990309));
#186810=CARTESIAN_POINT('Ctrl Pts',(17.5131809264171,20.9405345587228,9.41281166338132));
#186811=CARTESIAN_POINT('Ctrl Pts',(17.5131935903392,20.9405434976812,9.41281260297876));
#186812=CARTESIAN_POINT('Ctrl Pts',(17.5132191357901,20.9405615287776,9.41281449828479));
#186813=CARTESIAN_POINT('Ctrl Pts',(17.5132320172368,20.9405706208504,9.41281545398669));
#186814=CARTESIAN_POINT('Ctrl Pts',(17.513258002494,20.9405889615115,9.41281738185281));
#186815=CARTESIAN_POINT('Ctrl Pts',(17.5132711065358,20.9405982102554,9.41281835403357));
#186816=CARTESIAN_POINT('Ctrl Pts',(17.513297542199,20.9406168679175,9.41282031524251));
#186817=CARTESIAN_POINT('Ctrl Pts',(17.5133108738215,20.9406262768286,9.41282130427014));
#186818=CARTESIAN_POINT('Ctrl Pts',(17.5133377700112,20.9406452585875,9.41282329956891));
#186819=CARTESIAN_POINT('Ctrl Pts',(17.5133513346364,20.9406548314683,9.41282430584369));
#186820=CARTESIAN_POINT('Ctrl Pts',(17.5133787024836,20.9406741451311,9.41282633605408));
#186821=CARTESIAN_POINT('Ctrl Pts',(17.5133925054929,20.9406838857544,9.41282735997321));
#186822=CARTESIAN_POINT('Ctrl Pts',(17.513420355744,20.9407035388539,9.41282942588828));
#186823=CARTESIAN_POINT('Ctrl Pts',(17.5134344029478,20.9407134512942,9.41283046788066));
#186824=CARTESIAN_POINT('Ctrl Pts',(17.5134627471682,20.9407334519388,9.41283257035401));
#186825=CARTESIAN_POINT('Ctrl Pts',(17.5134770444489,20.9407435403201,9.4128336308538));
#186826=CARTESIAN_POINT('Ctrl Pts',(17.5135058949749,20.9407638971594,9.41283577079599));
#186827=CARTESIAN_POINT('Ctrl Pts',(17.5135204481435,20.9407741655538,9.41283685023193));
#186828=CARTESIAN_POINT('Ctrl Pts',(17.5135498167024,20.9407948868053,9.41283902850815));
#186829=CARTESIAN_POINT('Ctrl Pts',(17.5135646321264,20.9408053396761,9.41284012735012));
#186830=CARTESIAN_POINT('Ctrl Pts',(17.5135945318045,20.9408264345128,9.4128423449261));
#186831=CARTESIAN_POINT('Ctrl Pts',(17.5136096157503,20.9408370762507,9.41284346363639));
#186832=CARTESIAN_POINT('Ctrl Pts',(17.513640058837,20.9408585532806,9.41284572141851));
#186833=CARTESIAN_POINT('Ctrl Pts',(17.5136554182315,20.9408693887405,9.41284686050826));
#186834=CARTESIAN_POINT('Ctrl Pts',(17.5136864190702,20.9408912580173,9.41284915955498));
#186835=CARTESIAN_POINT('Ctrl Pts',(17.5137020604677,20.9409022917898,9.41285031950756));
#186836=CARTESIAN_POINT('Ctrl Pts',(17.5165618938005,20.9429196206005,9.41306239756386));
#186837=CARTESIAN_POINT('Ctrl Pts',(17.5194109871642,20.9449188691196,9.41327282152059));
#186838=CARTESIAN_POINT('Ctrl Pts',(17.5260570240062,20.9495580669258,9.41376170238612));
#186839=CARTESIAN_POINT('Ctrl Pts',(17.5298576951851,20.9521926073843,9.41403978901974));
#186840=CARTESIAN_POINT('Ctrl Pts',(17.5399926626179,20.9591688851703,9.41477747456173));
#186841=CARTESIAN_POINT('Ctrl Pts',(17.5463420690897,20.963488692114,9.41523562436576));
#186842=CARTESIAN_POINT('Ctrl Pts',(17.591525953381,20.9938711142462,9.41846874397601));
#186843=CARTESIAN_POINT('Ctrl Pts',(17.6311943467449,21.0186771727644,9.42116560175244));
#186844=CARTESIAN_POINT('Ctrl Pts',(17.6796763050525,21.0468040586029,9.42433588769273));
#186845=CARTESIAN_POINT('Ctrl Pts',(17.6877281129654,21.0514048841929,9.42485835628003));
#186846=CARTESIAN_POINT('Ctrl Pts',(17.7985384561741,21.1137599740331,9.43199687768628));
#186847=CARTESIAN_POINT('Ctrl Pts',(17.9059214618201,21.1628896352737,9.43831699960669));
#186848=CARTESIAN_POINT('Ctrl Pts',(18.1043043065165,21.2343175122883,9.44980139837942));
#186849=CARTESIAN_POINT('Ctrl Pts',(18.1937407176716,21.2600115413304,9.45491327822184));
#186850=CARTESIAN_POINT('Ctrl Pts',(18.3325838853385,21.2901748862576,9.46299073782786));
#186851=CARTESIAN_POINT('Ctrl Pts',(18.3809429405163,21.2989303784758,9.46582841130734));
#186852=CARTESIAN_POINT('Ctrl Pts',(18.4416600177764,21.3077536411689,9.46943946885941));
#186853=CARTESIAN_POINT('Ctrl Pts',(18.4537746321943,21.3094070698383,9.47016231597628));
#186854=CARTESIAN_POINT('Ctrl Pts',(18.4730565038001,21.3118687495453,9.47131680140594));
#186855=CARTESIAN_POINT('Ctrl Pts',(18.4802148572275,21.3127454913376,9.47174627272721));
#186856=CARTESIAN_POINT('Ctrl Pts',(18.4937112527438,21.314328549348,9.47255769549362));
#186857=CARTESIAN_POINT('Ctrl Pts',(18.5000482920473,21.31504283833,9.47293939053565));
#186858=CARTESIAN_POINT('Ctrl Pts',(18.5143264170593,21.3165869171924,9.47380101982015));
#186859=CARTESIAN_POINT('Ctrl Pts',(18.5222691317894,21.3174004333495,9.4742814615128));
#186860=CARTESIAN_POINT('Ctrl Pts',(18.5425762963924,21.3193643345392,9.47551277453454));
#186861=CARTESIAN_POINT('Ctrl Pts',(18.5549464838449,21.320450883406,9.47626564132454));
#186862=CARTESIAN_POINT('Ctrl Pts',(18.6291252882684,21.3263092808806,9.48079766067618));
#186863=CARTESIAN_POINT('Ctrl Pts',(18.6911041758201,21.3284727297351,9.48465794720081));
#186864=CARTESIAN_POINT('Ctrl Pts',(18.9003128034564,21.3265867102618,9.49794316495959));
#186865=CARTESIAN_POINT('Ctrl Pts',(19.0469878126794,21.3099035079008,9.50771742881051));
#186866=CARTESIAN_POINT('Ctrl Pts',(19.2612722989046,21.2625587021597,9.52218318720205));
#186867=CARTESIAN_POINT('Ctrl Pts',(19.3309826031314,21.2433686682805,9.52691186885705));
#186868=CARTESIAN_POINT('Ctrl Pts',(19.4316861478351,21.2100164996713,9.53366083424626));
#186869=CARTESIAN_POINT('Ctrl Pts',(19.4635358006561,21.1986143344654,9.5357825793678));
#186870=CARTESIAN_POINT('Ctrl Pts',(19.5019380082488,21.1838187718195,9.53831371588949));
#186871=CARTESIAN_POINT('Ctrl Pts',(19.5087618865754,21.1811489064738,9.53876242815051));
#186872=CARTESIAN_POINT('Ctrl Pts',(19.5194091322563,21.1769192616052,9.53946073766161));
#186873=CARTESIAN_POINT('Ctrl Pts',(19.5232419557631,21.1753836652034,9.53971174804479));
#186874=CARTESIAN_POINT('Ctrl Pts',(19.5303796690615,21.1724997227989,9.54017847255514));
#186875=CARTESIAN_POINT('Ctrl Pts',(19.5336856069989,21.1711542464921,9.54039434929202));
#186876=CARTESIAN_POINT('Ctrl Pts',(19.5412008644859,21.1680734511483,9.54088443992989));
#186877=CARTESIAN_POINT('Ctrl Pts',(19.5454079892703,21.1663329140209,9.5411583342207));
#186878=CARTESIAN_POINT('Ctrl Pts',(19.5582425095303,21.1609745651282,9.54199257027974));
#186879=CARTESIAN_POINT('Ctrl Pts',(19.5668517014783,21.1573130708558,9.54255033142214));
#186880=CARTESIAN_POINT('Ctrl Pts',(19.6398343106918,21.1257005903039,9.5472653374098));
#186881=CARTESIAN_POINT('Ctrl Pts',(19.7028124370688,21.0946185210883,9.55124625427611));
#186882=CARTESIAN_POINT('Ctrl Pts',(19.8992010421097,20.9852315694685,9.56373242246249));
#186883=CARTESIAN_POINT('Ctrl Pts',(20.0256204835678,20.8954320242298,9.57191522153338));
#186884=CARTESIAN_POINT('Ctrl Pts',(20.1997608206408,20.7405068302424,9.58485344076542));
#186885=CARTESIAN_POINT('Ctrl Pts',(20.2554342288704,20.6851376813337,9.58929456876296));
#186886=CARTESIAN_POINT('Ctrl Pts',(20.3207875952805,20.6124868218698,9.5949975322865));
#186887=CARTESIAN_POINT('Ctrl Pts',(20.3334759766611,20.597988373502,9.59612973170588));
#186888=CARTESIAN_POINT('Ctrl Pts',(20.3515639094661,20.5767417817744,9.59778146651719));
#186889=CARTESIAN_POINT('Ctrl Pts',(20.3571230372128,20.5701303169263,9.59829442756405));
#186890=CARTESIAN_POINT('Ctrl Pts',(20.366770155013,20.5585134078847,9.59919405943496));
#186891=CARTESIAN_POINT('Ctrl Pts',(20.3708760028081,20.5535228912506,9.59957999620287));
#186892=CARTESIAN_POINT('Ctrl Pts',(20.3787836918481,20.5438211642618,9.60032927282243));
#186893=CARTESIAN_POINT('Ctrl Pts',(20.3825883054764,20.5391122869457,9.60069249526767));
#186894=CARTESIAN_POINT('Ctrl Pts',(20.3916029334457,20.5278566811168,9.60155967097323));
#186895=CARTESIAN_POINT('Ctrl Pts',(20.3967944075215,20.5212952944819,9.60206436039392));
#186896=CARTESIAN_POINT('Ctrl Pts',(20.4152072233348,20.4977380976677,9.60387352275821));
#186897=CARTESIAN_POINT('Ctrl Pts',(20.4282076401234,20.4805720059056,9.60518668480398));
#186898=CARTESIAN_POINT('Ctrl Pts',(20.5538775553782,20.3092658586791,9.61824486798882));
#186899=CARTESIAN_POINT('Ctrl Pts',(20.6454462374491,20.1407771015906,9.63084302977509));
#186900=CARTESIAN_POINT('Ctrl Pts',(20.7404062532465,19.8906375899434,9.64849732622681));
#186901=CARTESIAN_POINT('Ctrl Pts',(20.763715345848,19.8174903334324,9.65352906561344));
#186902=CARTESIAN_POINT('Ctrl Pts',(20.7918249920106,19.7092735126506,9.66065043991878));
#186903=CARTESIAN_POINT('Ctrl Pts',(20.7998014553974,19.6750957559884,9.66285353592872));
#186904=CARTESIAN_POINT('Ctrl Pts',(20.8084288842392,19.6334792154909,9.66546799988751));
#186905=CARTESIAN_POINT('Ctrl Pts',(20.8098946498099,19.6262171599412,9.66592172557927));
#186906=CARTESIAN_POINT('Ctrl Pts',(20.8121213511723,19.6148785021958,9.6666261033216));
#186907=CARTESIAN_POINT('Ctrl Pts',(20.8129084655181,19.6108071877952,9.66687820808131));
#186908=CARTESIAN_POINT('Ctrl Pts',(20.8143504395285,19.6032292360288,9.66734590698785));
#186909=CARTESIAN_POINT('Ctrl Pts',(20.815008392145,19.599723290952,9.66756167027225));
#186910=CARTESIAN_POINT('Ctrl Pts',(20.8164813800908,19.591763446499,9.66805014862078));
#186911=CARTESIAN_POINT('Ctrl Pts',(20.8172909883079,19.5873085961343,9.66832255253708));
#186912=CARTESIAN_POINT('Ctrl Pts',(20.8196545536143,19.5740616980512,9.66912974932144));
#186913=CARTESIAN_POINT('Ctrl Pts',(20.8211672132267,19.565262253105,9.66966225321033));
#186914=CARTESIAN_POINT('Ctrl Pts',(20.8322368213428,19.4983349740359,9.67368620393002));
#186915=CARTESIAN_POINT('Ctrl Pts',(20.8394203940534,19.439834967184,9.67705377020056));
#186916=CARTESIAN_POINT('Ctrl Pts',(20.8570770517325,19.2208054902046,9.6893566039729));
#186917=CARTESIAN_POINT('Ctrl Pts',(20.8516923482769,19.0595489754792,9.69784431923421));
#186918=CARTESIAN_POINT('Ctrl Pts',(20.8191689273743,18.840237593498,9.71011781427093));
#186919=CARTESIAN_POINT('Ctrl Pts',(20.807647454331,18.7804426573627,9.71353580115989));
#186920=CARTESIAN_POINT('Ctrl Pts',(20.785040255936,18.6853754910086,9.71914553620922));
#186921=CARTESIAN_POINT('Ctrl Pts',(20.775579519628,18.6497513215909,9.72128786260963));
#186922=CARTESIAN_POINT('Ctrl Pts',(20.7620683839582,18.6037515694995,9.72411415973216));
#186923=CARTESIAN_POINT('Ctrl Pts',(20.7588590063686,18.593134299703,9.72477069831319));
#186924=CARTESIAN_POINT('Ctrl Pts',(20.7535000923061,18.5758962091658,9.72584368684579));
#186925=CARTESIAN_POINT('Ctrl Pts',(20.7514010479275,18.5692598204887,9.72625847736569));
#186926=CARTESIAN_POINT('Ctrl Pts',(20.7472988162594,18.5565091499987,9.72705876548025));
#186927=CARTESIAN_POINT('Ctrl Pts',(20.7453004052019,18.5503934038293,9.7274441019859));
#186928=CARTESIAN_POINT('Ctrl Pts',(20.740657039339,18.5363996856014,9.7283292593097));
#186929=CARTESIAN_POINT('Ctrl Pts',(20.7379935272576,18.528528024495,9.72882968907687));
#186930=CARTESIAN_POINT('Ctrl Pts',(20.730785679499,18.5076322246168,9.73016491009954));
#186931=CARTESIAN_POINT('Ctrl Pts',(20.7261603340591,18.4946366378958,9.73100237589546));
#186932=CARTESIAN_POINT('Ctrl Pts',(20.6893635205931,18.3943637260913,9.73752004312335));
#186933=CARTESIAN_POINT('Ctrl Pts',(20.6516026765133,18.309258785791,9.74338782813992));
#186934=CARTESIAN_POINT('Ctrl Pts',(20.5253710009559,18.0688254956185,9.76094443945539));
#186935=CARTESIAN_POINT('Ctrl Pts',(20.4227092916545,17.9218812959764,9.77300970691708));
#186936=CARTESIAN_POINT('Ctrl Pts',(20.2755859673156,17.7595014255634,9.78703159142716));
#186937=CARTESIAN_POINT('Ctrl Pts',(20.2474808402312,17.7302192429143,9.78958854688714));
#186938=CARTESIAN_POINT('Ctrl Pts',(20.2130440612626,17.6963458160479,9.79256190395354));
#186939=CARTESIAN_POINT('Ctrl Pts',(20.2075091221436,17.6909606902144,9.79303508282084));
#186940=CARTESIAN_POINT('Ctrl Pts',(20.198907785184,17.6826832967284,9.79376296659046));
#186941=CARTESIAN_POINT('Ctrl Pts',(20.195862075093,17.6797697629975,9.79401928213883));
#186942=CARTESIAN_POINT('Ctrl Pts',(20.1902268206243,17.6744112032621,9.79449086517782));
#186943=CARTESIAN_POINT('Ctrl Pts',(20.1876398271179,17.671963633726,9.79470632659517));
#186944=CARTESIAN_POINT('Ctrl Pts',(20.1818143231824,17.6664798832497,9.79518921435753));
#186945=CARTESIAN_POINT('Ctrl Pts',(20.1785724426174,17.6634473629906,9.79545635953401));
#186946=CARTESIAN_POINT('Ctrl Pts',(20.1702651323803,17.6557253882091,9.79613696539065));
#186947=CARTESIAN_POINT('Ctrl Pts',(20.165186217024,17.6510504291051,9.79654934360758));
#186948=CARTESIAN_POINT('Ctrl Pts',(20.1356114285308,17.6240939196917,9.79892975153214));
#186949=CARTESIAN_POINT('Ctrl Pts',(20.1106168676723,17.602363379293,9.80085896197606));
#186950=CARTESIAN_POINT('Ctrl Pts',(20.0710799883463,17.569586351999,9.80380386622175));
#186951=CARTESIAN_POINT('Ctrl Pts',(20.0568885109559,17.5581274454272,9.80484044571783));
#186952=CARTESIAN_POINT('Ctrl Pts',(20.0413783741312,17.5459315300434,9.80595355913886));
#186953=CARTESIAN_POINT('Ctrl Pts',(20.0402054192809,17.5450112168902,9.80603761743213));
#186954=CARTESIAN_POINT('Ctrl Pts',(20.0209855025488,17.5299638365166,9.80741302652882));
#186955=CARTESIAN_POINT('Ctrl Pts',(20.0027108115793,17.5161291506381,9.80869251753807));
#186956=CARTESIAN_POINT('Ctrl Pts',(19.9473566218194,17.475620862615,9.81249591811558));
#186957=CARTESIAN_POINT('Ctrl Pts',(19.9096342976774,17.449847173987,9.81499336509444));
#186958=CARTESIAN_POINT('Ctrl Pts',(19.7788703661665,17.3665780558736,9.8234336080593));
#186959=CARTESIAN_POINT('Ctrl Pts',(19.6822226065287,17.3150782202702,9.82932170190214));
#186960=CARTESIAN_POINT('Ctrl Pts',(19.5315380787513,17.2492000250523,9.83846604670764));
#186961=CARTESIAN_POINT('Ctrl Pts',(19.4802031295573,17.2291053577884,9.84157356806095));
#186962=CARTESIAN_POINT('Ctrl Pts',(19.395734245113,17.1997879759382,9.84671758659699));
#186963=CARTESIAN_POINT('Ctrl Pts',(19.3630560511335,17.1893288336569,9.84871469596928));
#186964=CARTESIAN_POINT('Ctrl Pts',(19.319767937637,17.1766249716555,9.85137534020413));
#186965=CARTESIAN_POINT('Ctrl Pts',(19.3093734145566,17.1736607400881,9.8520153468036));
#186966=CARTESIAN_POINT('Ctrl Pts',(19.2923087888241,17.1689353876189,9.85306805391278));
#186967=CARTESIAN_POINT('Ctrl Pts',(19.2856518903108,17.1671270159322,9.85347921313596));
#186968=CARTESIAN_POINT('Ctrl Pts',(19.2727471211575,17.1636890245688,9.85427728154789));
#186969=CARTESIAN_POINT('Ctrl Pts',(19.266500392518,17.162055388447,9.85466405535921));
#186970=CARTESIAN_POINT('Ctrl Pts',(19.2520570036281,17.1583486844274,9.85555943473606));
#186971=CARTESIAN_POINT('Ctrl Pts',(19.2438552437357,17.1562961017398,9.85606869643465));
#186972=CARTESIAN_POINT('Ctrl Pts',(19.2217585237542,17.1509065978905,9.8574430099492));
#186973=CARTESIAN_POINT('Ctrl Pts',(19.2078418939941,17.147661189555,9.85831098986632));
#186974=CARTESIAN_POINT('Ctrl Pts',(19.0798345040287,17.119172721012,9.86631834169499));
#186975=CARTESIAN_POINT('Ctrl Pts',(18.9638883078665,17.1032793287341,9.87375949835684));
#186976=CARTESIAN_POINT('Ctrl Pts',(18.684749178758,17.0883266571225,9.89201886129173));
#186977=CARTESIAN_POINT('Ctrl Pts',(18.521801851443,17.0983855574817,9.90297712302515));
#186978=CARTESIAN_POINT('Ctrl Pts',(18.3296137113565,17.1327272631173,9.91538262512077));
#186979=CARTESIAN_POINT('Ctrl Pts',(18.2977454115203,17.1391824303416,9.91742015081506));
#186980=CARTESIAN_POINT('Ctrl Pts',(18.258975903729,17.1479698205654,9.91986466718118));
#186981=CARTESIAN_POINT('Ctrl Pts',(18.2519234313814,17.1496063940205,9.92030794582583));
#186982=CARTESIAN_POINT('Ctrl Pts',(18.2408808821106,17.1522286612831,9.92099967406839));
#186983=CARTESIAN_POINT('Ctrl Pts',(18.2368851211693,17.1531898320158,9.92124949442663));
#186984=CARTESIAN_POINT('Ctrl Pts',(18.2294217721284,17.1550081298072,9.92171517768832));
#186985=CARTESIAN_POINT('Ctrl Pts',(18.225953592492,17.1558623874812,9.92193119605804));
#186986=CARTESIAN_POINT('Ctrl Pts',(18.2180419452963,17.157832380401,9.92242312320166));
#186987=CARTESIAN_POINT('Ctrl Pts',(18.2135999356597,17.1589537621381,9.9226987028075));
#186988=CARTESIAN_POINT('Ctrl Pts',(18.1999587829063,17.1624446027444,9.92354320179306));
#186989=CARTESIAN_POINT('Ctrl Pts',(18.1907717736573,17.164861603192,9.92410944703244));
#186990=CARTESIAN_POINT('Ctrl Pts',(18.1084454909791,17.187114303175,9.92916368603585));
#186991=CARTESIAN_POINT('Ctrl Pts',(18.0363957230491,17.2108043533015,9.93344589228252));
#186992=CARTESIAN_POINT('Ctrl Pts',(17.9259443271559,17.2538180556921,9.94000667112427));
#186993=CARTESIAN_POINT('Ctrl Pts',(17.8866016881268,17.2705280417435,9.94234269396019));
#186994=CARTESIAN_POINT('Ctrl Pts',(17.7485092341623,17.3341813865009,9.95062116243442));
#186995=CARTESIAN_POINT('Ctrl Pts',(17.652922559694,17.3875661957144,9.95650786140303));
#186996=CARTESIAN_POINT('Ctrl Pts',(17.5160260242026,17.4785849988185,9.96564896340301));
#186997=CARTESIAN_POINT('Ctrl Pts',(17.4713725031269,17.5108548585996,9.96875462608136));
#186998=CARTESIAN_POINT('Ctrl Pts',(17.4010406017053,17.5659820083536,9.97389584213913));
#186999=CARTESIAN_POINT('Ctrl Pts',(17.3745703894922,17.5877884031711,9.9758920639649));
#187000=CARTESIAN_POINT('Ctrl Pts',(17.3404706758821,17.6172993327085,9.97855169331007));
#187001=CARTESIAN_POINT('Ctrl Pts',(17.3323532379288,17.6244338520182,9.97919159547047));
#187002=CARTESIAN_POINT('Ctrl Pts',(17.3191448627516,17.6362233428168,9.98024417455092));
#187003=CARTESIAN_POINT('Ctrl Pts',(17.3140213577778,17.6408416534283,9.98065531092042));
#187004=CARTESIAN_POINT('Ctrl Pts',(17.3041456362576,17.64983146611,9.9814533662518));
#187005=CARTESIAN_POINT('Ctrl Pts',(17.2993906642124,17.6541998378213,9.98184015000184));
#187006=CARTESIAN_POINT('Ctrl Pts',(17.2884551799254,17.664338863289,9.98273559796094));
#187007=CARTESIAN_POINT('Ctrl Pts',(17.2822891391162,17.6701249006464,9.98324491861934));
#187008=CARTESIAN_POINT('Ctrl Pts',(17.2657938264573,17.6857905291081,9.98461949441582));
#187009=CARTESIAN_POINT('Ctrl Pts',(17.2555298120623,17.6957379151518,9.98548767939412));
#187010=CARTESIAN_POINT('Ctrl Pts',(17.1621045915556,17.7881340994369,9.99351084430885));
#187011=CARTESIAN_POINT('Ctrl Pts',(17.085831394973,17.8772328015539,10.0009689933854));
#187012=CARTESIAN_POINT('Ctrl Pts',(16.9216222308105,18.1047806964446,10.0193000846084));
#187013=CARTESIAN_POINT('Ctrl Pts',(16.8416122341248,18.248034232571,10.030315221451));
#187014=CARTESIAN_POINT('Ctrl Pts',(16.766787803809,18.4282095920219,10.0427007555383));
#187015=CARTESIAN_POINT('Ctrl Pts',(16.7553382284952,18.457619293694,10.044677089349));
#187016=CARTESIAN_POINT('Ctrl Pts',(16.7420974934782,18.4940168337103,10.0470584329619));
#187017=CARTESIAN_POINT('Ctrl Pts',(16.7396794444505,18.5007704727776,10.0474975984361));
#187018=CARTESIAN_POINT('Ctrl Pts',(16.735934967577,18.5113987594066,10.0481843418059));
#187019=CARTESIAN_POINT('Ctrl Pts',(16.734585400856,18.5152651144164,10.0484332587459));
#187020=CARTESIAN_POINT('Ctrl Pts',(16.7320789915764,18.5225132172317,10.0488981650053));
#187021=CARTESIAN_POINT('Ctrl Pts',(16.7309195071424,18.5258939400612,10.0491143043344));
#187022=CARTESIAN_POINT('Ctrl Pts',(16.7282860719747,18.5336361149015,10.0496076870388));
#187023=CARTESIAN_POINT('Ctrl Pts',(16.7268177853716,18.5379994412275,10.049884593726));
#187024=CARTESIAN_POINT('Ctrl Pts',(16.722327345533,18.5514891553477,10.0507372239692));
#187025=CARTESIAN_POINT('Ctrl Pts',(16.7193530677122,18.5606315128752,10.0513101980963));
#187026=CARTESIAN_POINT('Ctrl Pts',(16.6905474218074,18.6512686680753,10.0569454327714));
#187027=CARTESIAN_POINT('Ctrl Pts',(16.6696095011782,18.7342474219198,10.0617451522039));
#187028=CARTESIAN_POINT('Ctrl Pts',(16.6294008318276,18.947231259688,10.0736795322587));
#187029=CARTESIAN_POINT('Ctrl Pts',(16.6170990832107,19.0781722139405,10.0806785868332));
#187030=CARTESIAN_POINT('Ctrl Pts',(16.6169313786663,19.3016470690534,10.0930378845873));
#187031=CARTESIAN_POINT('Ctrl Pts',(16.6228899854553,19.3937783351956,10.0982490879101));
#187032=CARTESIAN_POINT('Ctrl Pts',(16.6366195100217,19.4988780731671,10.1044627454843));
#187033=CARTESIAN_POINT('Ctrl Pts',(16.6385368153887,19.5125173847697,10.1052742421342));
#187034=CARTESIAN_POINT('Ctrl Pts',(16.6418231771176,19.5343482615356,10.1065817209942));
#187035=CARTESIAN_POINT('Ctrl Pts',(16.6431076017331,19.5425523070582,10.1070750262759));
#187036=CARTESIAN_POINT('Ctrl Pts',(16.6454726643887,19.5570981838056,10.1079532175542));
#187037=CARTESIAN_POINT('Ctrl Pts',(16.646534009996,19.5634430785184,10.1083374867896));
#187038=CARTESIAN_POINT('Ctrl Pts',(16.6488043602059,19.5766454984752,10.1091396200645));
#187039=CARTESIAN_POINT('Ctrl Pts',(16.6500183105162,19.5835020843766,10.1095576372742));
#187040=CARTESIAN_POINT('Ctrl Pts',(16.6532558815059,19.6012771066016,10.1106450894066));
#187041=CARTESIAN_POINT('Ctrl Pts',(16.6553316014523,19.6121857276935,10.1113161770975));
#187042=CARTESIAN_POINT('Ctrl Pts',(16.6646897605166,19.6593426085278,10.1142336505211));
#187043=CARTESIAN_POINT('Ctrl Pts',(16.6728349140608,19.6954111683336,10.1165074103893));
#187044=CARTESIAN_POINT('Ctrl Pts',(16.6969459037756,19.7905155160465,10.1226194541523));
#187045=CARTESIAN_POINT('Ctrl Pts',(16.7145313850519,19.8491011210258,10.1265064288919));
#187046=CARTESIAN_POINT('Ctrl Pts',(16.7381478917004,19.9169590415021,10.1311462812496));
#187047=CARTESIAN_POINT('Ctrl Pts',(16.7417458056892,19.9270495362942,10.1318398413702));
#187048=CARTESIAN_POINT('Ctrl Pts',(16.74541937607,19.9371102548029,10.1325348912934));
#187049=CARTESIAN_POINT('Origin',(18.734,19.211,0.));
#187050=CARTESIAN_POINT('',(16.745419285258,19.9371100060984,11.1558808557757));
#187051=CARTESIAN_POINT('',(16.7454193623258,19.9371102171621,10.9336112429045));
#187052=CARTESIAN_POINT('',(16.7454193623258,19.9371102171621,0.));
#187053=CARTESIAN_POINT('',(16.6170004031077,19.2096935705332,11.1109437209282));
#187054=CARTESIAN_POINT('Ctrl Pts',(16.745419285258,19.9371100060985,11.1558808557757));
#187055=CARTESIAN_POINT('Ctrl Pts',(16.7234349503207,19.8769020154143,11.1523876679106));
#187056=CARTESIAN_POINT('Ctrl Pts',(16.7041766146871,19.8156728636758,11.148866777791));
#187057=CARTESIAN_POINT('Ctrl Pts',(16.6773854470669,19.7146376045154,11.1430184305134));
#187058=CARTESIAN_POINT('Ctrl Pts',(16.6681681722473,19.6753843801569,11.140737389594));
#187059=CARTESIAN_POINT('Ctrl Pts',(16.6588573166312,19.6299377081226,11.1380746112071));
#187060=CARTESIAN_POINT('Ctrl Pts',(16.6576628084352,19.6239767856912,11.1377249294554));
#187061=CARTESIAN_POINT('Ctrl Pts',(16.6558534143148,19.6147410928009,11.1371824413015));
#187062=CARTESIAN_POINT('Ctrl Pts',(16.6552205500167,19.6114698487589,11.1369901584407));
#187063=CARTESIAN_POINT('Ctrl Pts',(16.649172395059,19.5798065763244,11.1351276415146));
#187064=CARTESIAN_POINT('Ctrl Pts',(16.6443315839102,19.5513090136826,11.1334407179447));
#187065=CARTESIAN_POINT('Ctrl Pts',(16.63853230186,19.5123536407143,11.1311167824628));
#187066=CARTESIAN_POINT('Ctrl Pts',(16.637065784985,19.5019738521413,11.13049584114));
#187067=CARTESIAN_POINT('Ctrl Pts',(16.634862067449,19.4854935228041,11.1295070686686));
#187068=CARTESIAN_POINT('Ctrl Pts',(16.6340742206889,19.4793998399713,11.129140841427));
#187069=CARTESIAN_POINT('Ctrl Pts',(16.63254836061,19.4671797882265,11.128405137446));
#187070=CARTESIAN_POINT('Ctrl Pts',(16.6318105825512,19.4610534513,11.1280356571333));
#187071=CARTESIAN_POINT('Ctrl Pts',(16.6303836083822,19.4487513235021,11.127292384545));
#187072=CARTESIAN_POINT('Ctrl Pts',(16.6296947991948,19.442575550285,11.1269185839524));
#187073=CARTESIAN_POINT('Ctrl Pts',(16.6281826815282,19.4284539820372,11.1260622805929));
#187074=CARTESIAN_POINT('Ctrl Pts',(16.6273771405197,19.4205064157806,11.1255792227055));
#187075=CARTESIAN_POINT('Ctrl Pts',(16.6254321889408,19.4001706885657,11.1243402363105));
#187076=CARTESIAN_POINT('Ctrl Pts',(16.6243569717339,19.3877768258634,11.1235823054178));
#187077=CARTESIAN_POINT('Ctrl Pts',(16.6190952486441,19.320214972957,11.119434868949));
#187078=CARTESIAN_POINT('Ctrl Pts',(16.616963796918,19.264913558275,11.1159819804477));
#187079=CARTESIAN_POINT('Ctrl Pts',(16.6170004651088,19.2095966930235,11.1124693456188));
#187080=CARTESIAN_POINT('Ctrl Pts',(16.7454193623258,19.9371102171621,10.3555828633409));
#187081=CARTESIAN_POINT('Ctrl Pts',(16.7701522519194,20.0048455887312,10.3599055406837));
#187082=CARTESIAN_POINT('Ctrl Pts',(16.7983602447238,20.0713437241127,10.3642282180265));
#187083=CARTESIAN_POINT('Ctrl Pts',(16.8298869170301,20.1362255764207,10.3685508953693));
#187084=CARTESIAN_POINT('Ctrl Pts',(16.8614136510539,20.2011075557432,10.3728735811742));
#187085=CARTESIAN_POINT('Ctrl Pts',(16.8962588589392,20.2643728019858,10.3771962669792));
#187086=CARTESIAN_POINT('Ctrl Pts',(16.9342193458651,20.3256652398822,10.3815189527842));
#187087=CARTESIAN_POINT('Ctrl Pts',(16.972217843787,20.3870190517705,10.3858459670266));
#187088=CARTESIAN_POINT('Ctrl Pts',(17.0133375849194,20.4463956918691,10.390172981269));
#187089=CARTESIAN_POINT('Ctrl Pts',(17.0573316197914,20.5034674629594,10.3944999955115));
#187090=CARTESIAN_POINT('Ctrl Pts',(17.1013502165957,20.5605710973007,10.3988294255321));
#187091=CARTESIAN_POINT('Ctrl Pts',(17.1482459768821,20.6153669278815,10.4031588555527));
#187092=CARTESIAN_POINT('Ctrl Pts',(17.197733021574,20.6675619695014,10.4074882855733));
#187093=CARTESIAN_POINT('Ctrl Pts',(17.2473041635017,20.7198457102697,10.4118250729357));
#187094=CARTESIAN_POINT('Ctrl Pts',(17.2994750180666,20.7695195032584,10.416161860298));
#187095=CARTESIAN_POINT('Ctrl Pts',(17.3539250691498,20.8163293074129,10.4204986476603));
#187096=CARTESIAN_POINT('Ctrl Pts',(17.3811407337521,20.8397261620462,10.42266629577));
#187097=CARTESIAN_POINT('Ctrl Pts',(17.4089253239853,20.862408172781,10.4248339438798));
#187098=CARTESIAN_POINT('Ctrl Pts',(17.4372361998843,20.8843477363386,10.4270015919895));
#187099=CARTESIAN_POINT('Ctrl Pts',(17.494549025663,20.9287624124625,10.4313898009204));
#187100=CARTESIAN_POINT('Ctrl Pts',(17.5542581954977,20.9703158984434,10.4357780098513));
#187101=CARTESIAN_POINT('Ctrl Pts',(17.6160462231312,21.0087397900655,10.4401662187822));
#187102=CARTESIAN_POINT('Ctrl Pts',(17.677742547087,21.0471066542616,10.4445479148834));
#187103=CARTESIAN_POINT('Ctrl Pts',(17.7415111977163,21.0823528921037,10.4489296109847));
#187104=CARTESIAN_POINT('Ctrl Pts',(17.8070029012395,21.1142512653062,10.4533113070859));
#187105=CARTESIAN_POINT('Ctrl Pts',(17.872417646799,21.1461121553816,10.4576878543456));
#187106=CARTESIAN_POINT('Ctrl Pts',(17.9395509916039,21.1746327855722,10.4620644016052));
#187107=CARTESIAN_POINT('Ctrl Pts',(18.0080275301098,21.1996309292982,10.4664409488649));
#187108=CARTESIAN_POINT('Ctrl Pts',(18.0764606417902,21.2246132195648,10.4708147205818));
#187109=CARTESIAN_POINT('Ctrl Pts',(18.1462348050099,21.2460772907211,10.4751884922988));
#187110=CARTESIAN_POINT('Ctrl Pts',(18.2169543269186,21.263888884462,10.4795622640158));
#187111=CARTESIAN_POINT('Ctrl Pts',(18.2876523286393,21.2816950580752,10.4839347047793));
#187112=CARTESIAN_POINT('Ctrl Pts',(18.3592946504356,21.2958508431231,10.4883071455429));
#187113=CARTESIAN_POINT('Ctrl Pts',(18.4314717388384,21.3062722141045,10.4926795863064));
#187114=CARTESIAN_POINT('Ctrl Pts',(18.5036506728174,21.3166938515616,10.4970521388738));
#187115=CARTESIAN_POINT('Ctrl Pts',(18.5763639228389,21.3233808184122,10.5014246914411));
#187116=CARTESIAN_POINT('Ctrl Pts',(18.6491947479435,21.3263007042082,10.5057972440085));
#187117=CARTESIAN_POINT('Ctrl Pts',(18.7221011596255,21.3292236203718,10.5101743345758));
#187118=CARTESIAN_POINT('Ctrl Pts',(18.7951249069976,21.3283716302984,10.5145514251431));
#187119=CARTESIAN_POINT('Ctrl Pts',(18.8678480060379,21.3237644713218,10.5189285157104));
#187120=CARTESIAN_POINT('Ctrl Pts',(18.9406108218616,21.3191547962047,10.5233079967694));
#187121=CARTESIAN_POINT('Ctrl Pts',(19.0130721829179,21.3107859243703,10.5276874778283));
#187122=CARTESIAN_POINT('Ctrl Pts',(19.0848207051465,21.2987293485604,10.5320669588873));
#187123=CARTESIAN_POINT('Ctrl Pts',(19.1566964011491,21.2866514025508,10.536454202547));
#187124=CARTESIAN_POINT('Ctrl Pts',(19.2278562638075,21.2708728040951,10.5408414462067));
#187125=CARTESIAN_POINT('Ctrl Pts',(19.2979011262237,21.2515157484919,10.5452286898664));
#187126=CARTESIAN_POINT('Ctrl Pts',(19.3455248831599,21.2383548159232,10.5482115928013));
#187127=CARTESIAN_POINT('Ctrl Pts',(19.3926335158209,21.2235407241657,10.5511944957361));
#187128=CARTESIAN_POINT('Ctrl Pts',(19.4391069833084,21.2071245307069,10.5541773986709));
#187129=CARTESIAN_POINT('Ctrl Pts',(19.507475042724,21.1829743359732,10.5585656076018));
#187130=CARTESIAN_POINT('Ctrl Pts',(19.5747343896098,21.1552604871605,10.5629538165327));
#187131=CARTESIAN_POINT('Ctrl Pts',(19.6404874892067,21.1241046578564,10.5673420254636));
#187132=CARTESIAN_POINT('Ctrl Pts',(19.7061430003017,21.0929950689686,10.5717237215648));
#187133=CARTESIAN_POINT('Ctrl Pts',(19.7702962696064,21.0584538454433,10.5761054176661));
#187134=CARTESIAN_POINT('Ctrl Pts',(19.8325671704115,21.0206516714811,10.5804871137674));
#187135=CARTESIAN_POINT('Ctrl Pts',(19.8947648979524,20.9828939180816,10.584863661027));
#187136=CARTESIAN_POINT('Ctrl Pts',(19.9550842407134,20.9418830753685,10.5892402082867));
#187137=CARTESIAN_POINT('Ctrl Pts',(20.013168775078,20.8978361642037,10.5936167555463));
#187138=CARTESIAN_POINT('Ctrl Pts',(20.071216473075,20.8538171869499,10.5979905272633));
#187139=CARTESIAN_POINT('Ctrl Pts',(20.1270317913337,20.8067662523015,10.6023642989803));
#187140=CARTESIAN_POINT('Ctrl Pts',(20.1802876588313,20.7569434038516,10.6067380706973));
#187141=CARTESIAN_POINT('Ctrl Pts',(20.2335273203897,20.7071357166618,10.6111105114608));
#187142=CARTESIAN_POINT('Ctrl Pts',(20.2842087253977,20.654558119635,10.6154829522244));
#187143=CARTESIAN_POINT('Ctrl Pts',(20.3320395381811,20.5995095010153,10.6198553929879));
#187144=CARTESIAN_POINT('Ctrl Pts',(20.3798715740037,20.5444594747964,10.6242279455553));
#187145=CARTESIAN_POINT('Ctrl Pts',(20.4248525580104,20.4869386669774,10.6286004981226));
#187146=CARTESIAN_POINT('Ctrl Pts',(20.4667296641662,20.4272799475937,10.63297305069));
#187147=CARTESIAN_POINT('Ctrl Pts',(20.5086502319623,20.3675593121408,10.6373501412573));
#187148=CARTESIAN_POINT('Ctrl Pts',(20.5474602125885,20.3056967307918,10.6417272318247));
#187149=CARTESIAN_POINT('Ctrl Pts',(20.5829499551957,20.2420543454065,10.646104322392));
#187150=CARTESIAN_POINT('Ctrl Pts',(20.6184590800686,20.1783772025526,10.6504838034509));
#187151=CARTESIAN_POINT('Ctrl Pts',(20.6506441436598,20.1129187535676,10.6548632845099));
#187152=CARTESIAN_POINT('Ctrl Pts',(20.6793425856621,20.0460636050083,10.6592427655688));
#187153=CARTESIAN_POINT('Ctrl Pts',(20.7080918954602,19.979089956147,10.6636300092285));
#187154=CARTESIAN_POINT('Ctrl Pts',(20.7333420751798,19.9107151168643,10.6680172528883));
#187155=CARTESIAN_POINT('Ctrl Pts',(20.754979810258,19.8413408653496,10.672404496548));
#187156=CARTESIAN_POINT('Ctrl Pts',(20.7696913851039,19.7941730592069,10.6753873994828));
#187157=CARTESIAN_POINT('Ctrl Pts',(20.7827340876901,19.7465435673451,10.6783703024176));
#187158=CARTESIAN_POINT('Ctrl Pts',(20.794085873422,19.6985809616125,10.6813532053524));
#187159=CARTESIAN_POINT('Ctrl Pts',(20.810785715361,19.6280222007594,10.6857414142833));
#187160=CARTESIAN_POINT('Ctrl Pts',(20.8238889631161,19.5564667533233,10.6901296232142));
#187161=CARTESIAN_POINT('Ctrl Pts',(20.8332827468938,19.4843147427306,10.6945178321451));
#187162=CARTESIAN_POINT('Ctrl Pts',(20.8426625887389,19.4122698176847,10.6988995282463));
#187163=CARTESIAN_POINT('Ctrl Pts',(20.8483438339329,19.3396305615062,10.7032812243476));
#187164=CARTESIAN_POINT('Ctrl Pts',(20.8502642454991,19.266808988722,10.7076629204489));
#187165=CARTESIAN_POINT('Ctrl Pts',(20.8521824004289,19.1940729870813,10.7120394677085));
#187166=CARTESIAN_POINT('Ctrl Pts',(20.8503484880034,19.1211555742339,10.7164160149681));
#187167=CARTESIAN_POINT('Ctrl Pts',(20.8447520630799,19.0484739153125,10.7207925622278));
#187168=CARTESIAN_POINT('Ctrl Pts',(20.8391591873278,18.9758383500428,10.7251663339447));
#187169=CARTESIAN_POINT('Ctrl Pts',(20.8298085704125,18.9034387218193,10.7295401056617));
#187170=CARTESIAN_POINT('Ctrl Pts',(20.8167418305019,18.8316908022767,10.7339138773787));
#187171=CARTESIAN_POINT('Ctrl Pts',(20.8036790668442,18.759964715867,10.7382863181422));
#187172=CARTESIAN_POINT('Ctrl Pts',(20.7869025116119,18.688890418704,10.7426587589058));
#187173=CARTESIAN_POINT('Ctrl Pts',(20.7665052467621,18.6188755013642,10.7470311996693));
#187174=CARTESIAN_POINT('Ctrl Pts',(20.746107460352,18.5488587937354,10.7514037522367));
#187175=CARTESIAN_POINT('Ctrl Pts',(20.7220889173525,18.4799019822769,10.755776304804));
#187176=CARTESIAN_POINT('Ctrl Pts',(20.6945926588479,18.4123978299105,10.7601488573713));
#187177=CARTESIAN_POINT('Ctrl Pts',(20.6670678636891,18.3448236191885,10.7645259479387));
#187178=CARTESIAN_POINT('Ctrl Pts',(20.636058329164,18.278705525327,10.768903038506));
#187179=CARTESIAN_POINT('Ctrl Pts',(20.6017550792379,18.2144158520321,10.7732801290733));
#187180=CARTESIAN_POINT('Ctrl Pts',(20.567433095034,18.1500910677606,10.7776596101322));
#187181=CARTESIAN_POINT('Ctrl Pts',(20.5298140629457,18.0875971057592,10.7820390911912));
#187182=CARTESIAN_POINT('Ctrl Pts',(20.4891333854109,18.0272788337552,10.7864185722501));
#187183=CARTESIAN_POINT('Ctrl Pts',(20.4483806016482,17.9668536480189,10.7908058159098));
#187184=CARTESIAN_POINT('Ctrl Pts',(20.4045556257391,17.9086122391301,10.7951930595695));
#187185=CARTESIAN_POINT('Ctrl Pts',(20.3579349545344,17.8528673616169,10.7995803032293));
#187186=CARTESIAN_POINT('Ctrl Pts',(20.3262373904722,17.8149662164714,10.8025632061641));
#187187=CARTESIAN_POINT('Ctrl Pts',(20.2932482928821,17.7782184270684,10.8055461090989));
#187188=CARTESIAN_POINT('Ctrl Pts',(20.2590638380206,17.7427121229262,10.8085290120338));
#187189=CARTESIAN_POINT('Ctrl Pts',(20.2087743940131,17.6904780796657,10.8129172209647));
#187190=CARTESIAN_POINT('Ctrl Pts',(20.1557001261014,17.6407287153968,10.8173054298956));
#187191=CARTESIAN_POINT('Ctrl Pts',(20.1001163804879,17.5937755149755,10.8216936388264));
#187192=CARTESIAN_POINT('Ctrl Pts',(20.0446151303688,17.5468920008887,10.8260753349277));
#187193=CARTESIAN_POINT('Ctrl Pts',(19.9866121616044,17.5027967211002,10.830457031029));
#187194=CARTESIAN_POINT('Ctrl Pts',(19.926420225514,17.461765022707,10.8348387271302));
#187195=CARTESIAN_POINT('Ctrl Pts',(19.8662990197387,17.4207815398248,10.8392152743899));
#187196=CARTESIAN_POINT('Ctrl Pts',(19.8039943529517,17.3828547573655,10.8435918216495));
#187197=CARTESIAN_POINT('Ctrl Pts',(19.7398513412541,17.3482192616152,10.8479683689092));
#187198=CARTESIAN_POINT('Ctrl Pts',(19.6757490081223,17.3136057311929,10.8523421406261));
#187199=CARTESIAN_POINT('Ctrl Pts',(19.6098110666881,17.2822795746617,10.8567159123431));
#187200=CARTESIAN_POINT('Ctrl Pts',(19.5424096422239,17.2544308470285,10.8610896840601));
#187201=CARTESIAN_POINT('Ctrl Pts',(19.4750287282394,17.2265905938567,10.8654621248236));
#187202=CARTESIAN_POINT('Ctrl Pts',(19.4061856609219,17.202225852836,10.8698345655872));
#187203=CARTESIAN_POINT('Ctrl Pts',(19.3362735429415,17.1814789778195,10.8742070063508));
#187204=CARTESIAN_POINT('Ctrl Pts',(19.2663596373006,17.1607315723031,10.8785795589181));
#187205=CARTESIAN_POINT('Ctrl Pts',(19.1953770897379,17.1436023517757,10.8829521114854));
#187206=CARTESIAN_POINT('Ctrl Pts',(19.1237335771406,17.1301836364424,10.8873246640528));
#187207=CARTESIAN_POINT('Ctrl Pts',(19.0520157102037,17.1167509946602,10.8917017546201));
#187208=CARTESIAN_POINT('Ctrl Pts',(18.9796359837851,17.1070366356522,10.8960788451874));
#187209=CARTESIAN_POINT('Ctrl Pts',(18.9070108440332,17.1010814594286,10.9004559357548));
#187210=CARTESIAN_POINT('Ctrl Pts',(18.8343460409969,17.0951230308623,10.9048354168137));
#187211=CARTESIAN_POINT('Ctrl Pts',(18.7614360402695,17.092927887168,10.9092148978727));
#187212=CARTESIAN_POINT('Ctrl Pts',(18.688698239908,17.0944847625088,10.9135943789316));
#187213=CARTESIAN_POINT('Ctrl Pts',(18.6158315122837,17.0960443974006,10.9179816225913));
#187214=CARTESIAN_POINT('Ctrl Pts',(18.5431380760578,17.1013692966916,10.9223688662511));
#187215=CARTESIAN_POINT('Ctrl Pts',(18.4710305707953,17.110396258381,10.9267561099108));
#187216=CARTESIAN_POINT('Ctrl Pts',(18.4220044154796,17.1165337224938,10.9297390128456));
#187217=CARTESIAN_POINT('Ctrl Pts',(18.373248967218,17.1243814515023,10.9327219157804));
#187218=CARTESIAN_POINT('Ctrl Pts',(18.3248903873722,17.1339062792316,10.9357048187152));
#187219=CARTESIAN_POINT('Ctrl Pts',(18.2537491009803,17.1479184462449,10.9400930276461));
#187220=CARTESIAN_POINT('Ctrl Pts',(18.1831896640502,17.1656171190662,10.944481236577));
#187221=CARTESIAN_POINT('Ctrl Pts',(18.1136230257296,17.1869393759585,10.9488694455079));
#187222=CARTESIAN_POINT('Ctrl Pts',(18.0441596358344,17.2082299870864,10.9532511416092));
#187223=CARTESIAN_POINT('Ctrl Pts',(17.9756865768824,17.2331333660322,10.9576328377104));
#187224=CARTESIAN_POINT('Ctrl Pts',(17.9086046585652,17.2615355785914,10.9620145338117));
#187225=CARTESIAN_POINT('Ctrl Pts',(17.8416015668408,17.2899044162905,10.9663910810714));
#187226=CARTESIAN_POINT('Ctrl Pts',(17.7759868104056,17.3217637331242,10.970767628331));
#187227=CARTESIAN_POINT('Ctrl Pts',(17.7121444440022,17.3569503181747,10.9751441755907));
#187228=CARTESIAN_POINT('Ctrl Pts',(17.6483425654998,17.3921145884043,10.9795179473076));
#187229=CARTESIAN_POINT('Ctrl Pts',(17.5863112682425,17.4306017078622,10.9838917190246));
#187230=CARTESIAN_POINT('Ctrl Pts',(17.5264117827665,17.4722016512549,10.9882654907416));
#187231=CARTESIAN_POINT('Ctrl Pts',(17.466530524905,17.5137889356452,10.9926379315051));
#187232=CARTESIAN_POINT('Ctrl Pts',(17.4087801868836,17.5584868884069,10.9970103722687));
#187233=CARTESIAN_POINT('Ctrl Pts',(17.3534932447844,17.6060420258449,11.0013828130322));
#187234=CARTESIAN_POINT('Ctrl Pts',(17.2982048889917,17.6535983792732,11.0057553655996));
#187235=CARTESIAN_POINT('Ctrl Pts',(17.2453804185809,17.7040117463517,11.0101279181669));
#187236=CARTESIAN_POINT('Ctrl Pts',(17.1953181280009,17.7569893065106,11.0145004707343));
#187237=CARTESIAN_POINT('Ctrl Pts',(17.1452038808876,17.8100218487797,11.0188775613016));
#187238=CARTESIAN_POINT('Ctrl Pts',(17.0978578691722,17.8656235460741,11.0232546518689));
#187239=CARTESIAN_POINT('Ctrl Pts',(17.0535398976922,17.9234663714871,11.0276317424363));
#187240=CARTESIAN_POINT('Ctrl Pts',(17.0091977225231,17.9813407870138,11.0320112234952));
#187241=CARTESIAN_POINT('Ctrl Pts',(16.9678871535191,18.0414583697202,11.0363907045542));
#187242=CARTESIAN_POINT('Ctrl Pts',(16.9298246475457,18.1034620559113,11.0407701856131));
#187243=CARTESIAN_POINT('Ctrl Pts',(16.8916946760359,18.1655756432198,11.0451574292728));
#187244=CARTESIAN_POINT('Ctrl Pts',(16.856824495367,18.2295815860916,11.0495446729326));
#187245=CARTESIAN_POINT('Ctrl Pts',(16.8253843166286,18.29509870991,11.0539319165923));
#187246=CARTESIAN_POINT('Ctrl Pts',(16.804008024655,18.3396440408911,11.0569148195271));
#187247=CARTESIAN_POINT('Ctrl Pts',(16.7842163233974,18.3848874840303,11.0598977224619));
#187248=CARTESIAN_POINT('Ctrl Pts',(16.7660496141036,18.4307050053664,11.0628806253966));
#187249=CARTESIAN_POINT('Ctrl Pts',(16.7358636223545,18.506835871923,11.0678370477141));
#187250=CARTESIAN_POINT('Ctrl Pts',(16.7100671742208,18.5848010792819,11.0727934700315));
#187251=CARTESIAN_POINT('Ctrl Pts',(16.6888585600977,18.6641129085501,11.077749892349));
#187252=CARTESIAN_POINT('Ctrl Pts',(16.6677318984798,18.7431182678595,11.082687162485));
#187253=CARTESIAN_POINT('Ctrl Pts',(16.6511578246458,18.8234596442757,11.087624432621));
#187254=CARTESIAN_POINT('Ctrl Pts',(16.639285644145,18.9046329531839,11.092561702757));
#187255=CARTESIAN_POINT('Ctrl Pts',(16.6274900435731,18.9852826644061,11.0974671256854));
#187256=CARTESIAN_POINT('Ctrl Pts',(16.6203359927514,19.0667533747576,11.1023725486138));
#187257=CARTESIAN_POINT('Ctrl Pts',(16.6179218376292,19.148532322459,11.1072779715423));
#187258=CARTESIAN_POINT('Ctrl Pts',(16.6173204835913,19.1689030517308,11.1084998880042));
#187259=CARTESIAN_POINT('Ctrl Pts',(16.6170129926863,19.1892928268081,11.1097218044662));
#187260=CARTESIAN_POINT('Ctrl Pts',(16.6170004031077,19.2096935705332,11.1109437209282));
#187261=CARTESIAN_POINT('',(16.6170004031077,19.2123064294672,10.8890562790718));
#187262=CARTESIAN_POINT('Ctrl Pts',(16.74541937607,19.9371102548029,10.1325348912934));
#187263=CARTESIAN_POINT('Ctrl Pts',(16.7957300871112,20.0748949844512,10.1420538203509));
#187264=CARTESIAN_POINT('Ctrl Pts',(16.8602294130613,20.2070927770557,10.1518904231319));
#187265=CARTESIAN_POINT('Ctrl Pts',(16.9705620701912,20.3839384574977,10.1654299263584));
#187266=CARTESIAN_POINT('Ctrl Pts',(17.005507726352,20.4348520887237,10.1693725855517));
#187267=CARTESIAN_POINT('Ctrl Pts',(17.0481243237945,20.4914669517243,10.1737463497107));
#187268=CARTESIAN_POINT('Ctrl Pts',(17.0536641593785,20.4987281854847,10.1743070950182));
#187269=CARTESIAN_POINT('Ctrl Pts',(17.0620088147972,20.5095202363625,10.1751398905875));
#187270=CARTESIAN_POINT('Ctrl Pts',(17.0647781206029,20.5130782026633,10.1754143490037));
#187271=CARTESIAN_POINT('Ctrl Pts',(17.0697578835671,20.5194341374356,10.1759044173227));
#187272=CARTESIAN_POINT('Ctrl Pts',(17.071964054018,20.5222353827532,10.1761203241256));
#187273=CARTESIAN_POINT('Ctrl Pts',(17.0767598421284,20.5282931980694,10.1765870517956));
#187274=CARTESIAN_POINT('Ctrl Pts',(17.0793519774033,20.5315477017296,10.1768376885868));
#187275=CARTESIAN_POINT('Ctrl Pts',(17.0866262033125,20.5406256645147,10.1775365670396));
#187276=CARTESIAN_POINT('Ctrl Pts',(17.0913296091945,20.5464320741603,10.1779833076267));
#187277=CARTESIAN_POINT('Ctrl Pts',(17.118952348447,20.5801659161903,10.1805779717675));
#187278=CARTESIAN_POINT('Ctrl Pts',(17.1425543053568,20.6075296900622,10.1826795136911));
#187279=CARTESIAN_POINT('Ctrl Pts',(17.220974678788,20.6938773863978,10.1893509065886));
#187280=CARTESIAN_POINT('Ctrl Pts',(17.2784630051519,20.7503456564029,10.1937780097012));
#187281=CARTESIAN_POINT('Ctrl Pts',(17.4407097909254,20.8924759219074,10.2055350900232));
#187282=CARTESIAN_POINT('Ctrl Pts',(17.5506782810402,20.9715989992329,10.2127865849435));
#187283=CARTESIAN_POINT('Ctrl Pts',(17.721908541426,21.071466675794,10.2239369567949));
#187284=CARTESIAN_POINT('Ctrl Pts',(17.7777672529595,21.100783903157,10.2275505940441));
#187285=CARTESIAN_POINT('Ctrl Pts',(17.8461537344153,21.1328673151038,10.2319867423496));
#187286=CARTESIAN_POINT('Ctrl Pts',(17.8575065567011,21.1380714055328,10.232723519243));
#187287=CARTESIAN_POINT('Ctrl Pts',(17.876211673527,21.14644627516,10.2339382844348));
#187288=CARTESIAN_POINT('Ctrl Pts',(17.8835371877504,21.1496763781902,10.2344142333636));
#187289=CARTESIAN_POINT('Ctrl Pts',(17.8967322475627,21.1554054117174,10.2352719829291));
#187290=CARTESIAN_POINT('Ctrl Pts',(17.9025951264354,21.1579195230476,10.2356532592963));
#187291=CARTESIAN_POINT('Ctrl Pts',(17.9150972022701,21.1632138755813,10.2364666731196));
#187292=CARTESIAN_POINT('Ctrl Pts',(17.9217393813976,21.1659868269677,10.2368990527367));
#187293=CARTESIAN_POINT('Ctrl Pts',(17.9396436270696,21.1733544269303,10.238065215204));
#187294=CARTESIAN_POINT('Ctrl Pts',(17.9509312371049,21.1778859262824,10.2388011221852));
#187295=CARTESIAN_POINT('Ctrl Pts',(18.0072714593683,21.1999423001178,10.2424782716742));
#187296=CARTESIAN_POINT('Ctrl Pts',(18.0528730329247,21.2160165336841,10.2454676607904));
#187297=CARTESIAN_POINT('Ctrl Pts',(18.1854403586944,21.2577011130997,10.2542017476429));
#187298=CARTESIAN_POINT('Ctrl Pts',(18.2735461230385,21.2793041892006,10.2600638156925));
#187299=CARTESIAN_POINT('Ctrl Pts',(18.5213290176749,21.3234400849024,10.2765863247773));
#187300=CARTESIAN_POINT('Ctrl Pts',(18.682610212615,21.3334973897724,10.2874126602705));
#187301=CARTESIAN_POINT('Ctrl Pts',(18.8634556716809,21.3241328638617,10.2987727045214));
#187302=CARTESIAN_POINT('Ctrl Pts',(18.8834208643317,21.322815035384,10.3000154249877));
#187303=CARTESIAN_POINT('Ctrl Pts',(18.909726645604,21.3207037410137,10.301635117501));
#187304=CARTESIAN_POINT('Ctrl Pts',(18.9160858563881,21.3201644014005,10.3020252983786));
#187305=CARTESIAN_POINT('Ctrl Pts',(18.9263462544684,21.3192474424093,10.3026525304847));
#187306=CARTESIAN_POINT('Ctrl Pts',(18.9302489451616,21.3188877370806,10.3028905666247));
#187307=CARTESIAN_POINT('Ctrl Pts',(18.9377547927568,21.318174907649,10.3033472996069));
#187308=CARTESIAN_POINT('Ctrl Pts',(18.9413580460358,21.3178233784252,10.3035660803881));
#187309=CARTESIAN_POINT('Ctrl Pts',(18.9498803941602,21.3169698726508,10.3040824357027));
#187310=CARTESIAN_POINT('Ctrl Pts',(18.9547987005138,21.316459898473,10.3043795612766));
#187311=CARTESIAN_POINT('Ctrl Pts',(18.9711071481925,21.3147111180669,10.3053620474774));
#187312=CARTESIAN_POINT('Ctrl Pts',(18.98248924533,21.3133970548121,10.3060433101046));
#187313=CARTESIAN_POINT('Ctrl Pts',(19.0903407899513,21.3000574687938,10.3124612282572));
#187314=CARTESIAN_POINT('Ctrl Pts',(19.1858975522566,21.2814910665904,10.3178657671543));
#187315=CARTESIAN_POINT('Ctrl Pts',(19.3524153639701,21.2370533582304,10.3272974760259));
#187316=CARTESIAN_POINT('Ctrl Pts',(19.4238995390087,21.2138401417208,10.3313511972611));
#187317=CARTESIAN_POINT('Ctrl Pts',(19.6179294553143,21.1392086601816,10.3426813823989));
#187318=CARTESIAN_POINT('Ctrl Pts',(19.7370824942925,21.0799940189519,10.3500352953538));
#187319=CARTESIAN_POINT('Ctrl Pts',(19.8633132958297,21.0016953116394,10.3587362688878));
#187320=CARTESIAN_POINT('Ctrl Pts',(19.8766349620666,20.9932243244337,10.3596662979032));
#187321=CARTESIAN_POINT('Ctrl Pts',(19.8966275950702,20.9801951051994,10.3610805368106));
#187322=CARTESIAN_POINT('Ctrl Pts',(19.9033694413513,20.9757462571005,10.3615606658));
#187323=CARTESIAN_POINT('Ctrl Pts',(19.9153957552,20.9677110903517,10.3624230058577));
#187324=CARTESIAN_POINT('Ctrl Pts',(19.9206897917394,20.9641392192776,10.3628046691847));
#187325=CARTESIAN_POINT('Ctrl Pts',(19.9318793905945,20.9565157227513,10.3636157769336));
#187326=CARTESIAN_POINT('Ctrl Pts',(19.9377707299438,20.952458067413,10.3640454474057));
#187327=CARTESIAN_POINT('Ctrl Pts',(19.9534592811113,20.9415349406939,10.3651967460016));
#187328=CARTESIAN_POINT('Ctrl Pts',(19.9632189454135,20.9346162259274,10.3659204056326));
#187329=CARTESIAN_POINT('Ctrl Pts',(20.0101715068826,20.9007295216238,10.3694385686195));
#187330=CARTESIAN_POINT('Ctrl Pts',(20.0465361870195,20.8726400974848,10.3722763496522));
#187331=CARTESIAN_POINT('Ctrl Pts',(20.2126103330943,20.7355034668146,10.3857885327702));
#187332=CARTESIAN_POINT('Ctrl Pts',(20.3298229084178,20.6123319588386,10.3970390207031));
#187333=CARTESIAN_POINT('Ctrl Pts',(20.4905160495344,20.396843266539,10.4147482674157));
#187334=CARTESIAN_POINT('Ctrl Pts',(20.5442674237925,20.3130478363557,10.4212274626824));
#187335=CARTESIAN_POINT('Ctrl Pts',(20.5965812906995,20.217267320545,10.4279703788607));
#187336=CARTESIAN_POINT('Ctrl Pts',(20.6011699521907,20.2087270983095,10.4285660453203));
#187337=CARTESIAN_POINT('Ctrl Pts',(20.6078582813773,20.1960713072625,10.4294402446069));
#187338=CARTESIAN_POINT('Ctrl Pts',(20.6100033294292,20.1919800446404,10.42972154322));
#187339=CARTESIAN_POINT('Ctrl Pts',(20.6137849628936,20.1847095452751,10.4302190766529));
#187340=CARTESIAN_POINT('Ctrl Pts',(20.6154269008567,20.1815331538352,10.4304356463494));
#187341=CARTESIAN_POINT('Ctrl Pts',(20.6189274717902,20.1747188977478,10.4308985353165));
#187342=CARTESIAN_POINT('Ctrl Pts',(20.6207836201712,20.1710798191236,10.4311446983954));
#187343=CARTESIAN_POINT('Ctrl Pts',(20.6258495529179,20.1610763529531,10.43181859432));
#187344=CARTESIAN_POINT('Ctrl Pts',(20.6290377800182,20.1547010241123,10.4322449951897));
#187345=CARTESIAN_POINT('Ctrl Pts',(20.6458835129206,20.1205858658636,10.4345109559536));
#187346=CARTESIAN_POINT('Ctrl Pts',(20.6589650341288,20.0925638710295,10.4363167906306));
#187347=CARTESIAN_POINT('Ctrl Pts',(20.6966949899269,20.0068938756825,10.441701271943));
#187348=CARTESIAN_POINT('Ctrl Pts',(20.7194025216674,19.9484256980049,10.4451932067317));
#187349=CARTESIAN_POINT('Ctrl Pts',(20.7825323192419,19.7617003962861,10.4560260400965));
#187350=CARTESIAN_POINT('Ctrl Pts',(20.8133570332004,19.6305600322206,10.4631939275482));
#187351=CARTESIAN_POINT('Ctrl Pts',(20.8370589769717,19.4569598758478,10.4729176038633));
#187352=CARTESIAN_POINT('Ctrl Pts',(20.8414079545718,19.4163893589733,10.4752044795843));
#187353=CARTESIAN_POINT('Ctrl Pts',(20.8483658788832,19.3272364043524,10.480286725375));
#187354=CARTESIAN_POINT('Ctrl Pts',(20.8504777991199,19.2786399537743,10.4830939607998));
#187355=CARTESIAN_POINT('Ctrl Pts',(20.8510278249307,19.2174109296055,10.4866951579177));
#187356=CARTESIAN_POINT('Ctrl Pts',(20.8510284650092,19.204804876958,10.4874399796913));
#187357=CARTESIAN_POINT('Ctrl Pts',(20.8508510753374,19.1848306978137,10.4886258058009));
#187358=CARTESIAN_POINT('Ctrl Pts',(20.8507471539886,19.1774620884726,10.4890644859234));
#187359=CARTESIAN_POINT('Ctrl Pts',(20.8504818440078,19.1637340363762,10.4898841002203));
#187360=CARTESIAN_POINT('Ctrl Pts',(20.8503302598147,19.1573744710327,10.4902647225078));
#187361=CARTESIAN_POINT('Ctrl Pts',(20.8499299453271,19.1432520080514,10.4911120704385));
#187362=CARTESIAN_POINT('Ctrl Pts',(20.8496671537285,19.1354896293758,10.4915792320877));
#187363=CARTESIAN_POINT('Ctrl Pts',(20.8487795583968,19.1129417549045,10.4929404348042));
#187364=CARTESIAN_POINT('Ctrl Pts',(20.8480424372916,19.0981613721878,10.4938379817583));
#187365=CARTESIAN_POINT('Ctrl Pts',(20.8409614218368,18.9809035027416,10.501001623834));
#187366=CARTESIAN_POINT('Ctrl Pts',(20.8273259251446,18.8790180880072,10.5074978158596));
#187367=CARTESIAN_POINT('Ctrl Pts',(20.7748106556447,18.6273664013535,10.5241841356418));
#187368=CARTESIAN_POINT('Ctrl Pts',(20.7268215378695,18.4801136197315,10.534558879243));
#187369=CARTESIAN_POINT('Ctrl Pts',(20.641028217822,18.2902151943768,10.5480316975662));
#187370=CARTESIAN_POINT('Ctrl Pts',(20.6169351578503,18.2418985904145,10.5514635448109));
#187371=CARTESIAN_POINT('Ctrl Pts',(20.5868215894256,18.1868820362228,10.5553326854529));
#187372=CARTESIAN_POINT('Ctrl Pts',(20.5825760385602,18.1792383600413,10.5558693418908));
#187373=CARTESIAN_POINT('Ctrl Pts',(20.5760796170467,18.1677110523727,10.5566770447229));
#187374=CARTESIAN_POINT('Ctrl Pts',(20.5738636116541,18.1638080237369,10.5569502415293));
#187375=CARTESIAN_POINT('Ctrl Pts',(20.5698655446414,18.1568181343681,10.557438956443));
#187376=CARTESIAN_POINT('Ctrl Pts',(20.5680880925522,18.1537287135389,10.5576547644159));
#187377=CARTESIAN_POINT('Ctrl Pts',(20.5642111785997,18.1470293800548,10.5581223073707));
#187378=CARTESIAN_POINT('Ctrl Pts',(20.5621088423131,18.1434211974162,10.5583738527293));
#187379=CARTESIAN_POINT('Ctrl Pts',(20.556179320107,18.1333133958066,10.5590778357925));
#187380=CARTESIAN_POINT('Ctrl Pts',(20.5523280104854,18.1268279003548,10.5595287367539));
#187381=CARTESIAN_POINT('Ctrl Pts',(20.5292167185712,18.0883787182219,10.5621979881362));
#187382=CARTESIAN_POINT('Ctrl Pts',(20.5091476846135,18.05690611673,10.5643667870077));
#187383=CARTESIAN_POINT('Ctrl Pts',(20.4406577061334,17.9555164513515,10.5713561834721));
#187384=CARTESIAN_POINT('Ctrl Pts',(20.388853691367,17.8879803445313,10.5760179379409));
#187385=CARTESIAN_POINT('Ctrl Pts',(20.2162719043821,17.6890418045363,10.5903546240858));
#187386=CARTESIAN_POINT('Ctrl Pts',(20.0828856112584,17.5696628006295,10.5999274915264));
#187387=CARTESIAN_POINT('Ctrl Pts',(19.917373904607,17.4554847428305,10.611614148404));
#187388=CARTESIAN_POINT('Ctrl Pts',(19.8984215783637,17.4428569218332,10.6129485197993));
#187389=CARTESIAN_POINT('Ctrl Pts',(19.8712712802945,17.4253926856173,10.6148564091392));
#187390=CARTESIAN_POINT('Ctrl Pts',(19.8632383315085,17.4203017472716,10.6154204447334));
#187391=CARTESIAN_POINT('Ctrl Pts',(19.85011559208,17.4121085326836,10.6163412486508));
#187392=CARTESIAN_POINT('Ctrl Pts',(19.8450464652129,17.4089732862449,10.6166967945617));
#187393=CARTESIAN_POINT('Ctrl Pts',(19.8343958162144,17.4024479013006,10.6174435507512));
#187394=CARTESIAN_POINT('Ctrl Pts',(19.8288117202931,17.3990621032503,10.617834915302));
#187395=CARTESIAN_POINT('Ctrl Pts',(19.8154676484916,17.391055414418,10.6187698147042));
#187396=CARTESIAN_POINT('Ctrl Pts',(19.807693639502,17.3864582674368,10.6193142079375));
#187397=CARTESIAN_POINT('Ctrl Pts',(19.7812966117848,17.3710755587793,10.6211619885186));
#187398=CARTESIAN_POINT('Ctrl Pts',(19.762539099839,17.3605245451789,10.622473796705));
#187399=CARTESIAN_POINT('Ctrl Pts',(19.5850852396242,17.2642392365245,10.6348767858291));
#187400=CARTESIAN_POINT('Ctrl Pts',(19.416230969203,17.1988472306411,10.6467203448037));
#187401=CARTESIAN_POINT('Ctrl Pts',(19.1251260688293,17.1270139337721,10.6665283006269));
#187402=CARTESIAN_POINT('Ctrl Pts',(19.0068414311021,17.1082537691679,10.6743928266103));
#187403=CARTESIAN_POINT('Ctrl Pts',(18.8781140149752,17.0988895626419,10.6823645329544));
#187404=CARTESIAN_POINT('Ctrl Pts',(18.8686291192085,17.0982637748847,10.6829484216145));
#187405=CARTESIAN_POINT('Ctrl Pts',(18.8545656802276,17.0974310004847,10.6838086845926));
#187406=CARTESIAN_POINT('Ctrl Pts',(18.8499903137156,17.0971749724736,10.6840877015579));
#187407=CARTESIAN_POINT('Ctrl Pts',(18.8418471005566,17.0967458143016,10.6845827226335));
#187408=CARTESIAN_POINT('Ctrl Pts',(18.8382796185922,17.096566855953,10.6847990489774));
#187409=CARTESIAN_POINT('Ctrl Pts',(18.8306073468514,17.0962014507775,10.6852631163605));
#187410=CARTESIAN_POINT('Ctrl Pts',(18.8265024742595,17.0960179253301,10.6855106922892));
#187411=CARTESIAN_POINT('Ctrl Pts',(18.8151671424244,17.0955441961839,10.6861924529052));
#187412=CARTESIAN_POINT('Ctrl Pts',(18.8079356111265,17.0952791082577,10.6866252533551));
#187413=CARTESIAN_POINT('Ctrl Pts',(18.7682606336491,17.0940284023046,10.6889887285462));
#187414=CARTESIAN_POINT('Ctrl Pts',(18.7357972673219,17.0937518882932,10.6908821457287));
#187415=CARTESIAN_POINT('Ctrl Pts',(18.5406086071179,17.0965791991765,10.7020913157596));
#187416=CARTESIAN_POINT('Ctrl Pts',(18.3786765670616,17.1176933614959,10.7106933723548));
#187417=CARTESIAN_POINT('Ctrl Pts',(18.107397307336,17.1854854424246,10.7260011154506));
#187418=CARTESIAN_POINT('Ctrl Pts',(17.9965994894125,17.2231430171881,10.7325235546343));
#187419=CARTESIAN_POINT('Ctrl Pts',(17.8763668409597,17.2754486820515,10.7402047325094));
#187420=CARTESIAN_POINT('Ctrl Pts',(17.8633107589045,17.2812866092623,10.7410469283496));
#187421=CARTESIAN_POINT('Ctrl Pts',(17.8426290491511,17.2907868951309,10.7423944032879));
#187422=CARTESIAN_POINT('Ctrl Pts',(17.8349643491886,17.294363509809,10.7428967349929));
#187423=CARTESIAN_POINT('Ctrl Pts',(17.8214861888465,17.3007515233942,10.7437853816656));
#187424=CARTESIAN_POINT('Ctrl Pts',(17.8156637403704,17.3035437853665,10.7441710294786));
#187425=CARTESIAN_POINT('Ctrl Pts',(17.8097007059104,17.3064370989501,10.7445678198506));
#187426=CARTESIAN_POINT('Ctrl Pts',(17.8095472134244,17.306511597698,10.7445780347475));
#187427=CARTESIAN_POINT('Ctrl Pts',(17.8092663778586,17.3066479453308,10.7445967265874));
#187428=CARTESIAN_POINT('Ctrl Pts',(17.8091390319691,17.306709788437,10.7446052033284));
#187429=CARTESIAN_POINT('Ctrl Pts',(17.8089024434121,17.3068247124945,10.7446209533723));
#187430=CARTESIAN_POINT('Ctrl Pts',(17.8087931994503,17.3068777899074,10.7446282265344));
#187431=CARTESIAN_POINT('Ctrl Pts',(17.8085902492665,17.3069764171358,10.7446417395748));
#187432=CARTESIAN_POINT('Ctrl Pts',(17.808496541362,17.3070219647001,10.7446479793979));
#187433=CARTESIAN_POINT('Ctrl Pts',(17.8083224568012,17.3071065959447,10.7446595722084));
#187434=CARTESIAN_POINT('Ctrl Pts',(17.8082420785269,17.3071456781525,10.7446649251805));
#187435=CARTESIAN_POINT('Ctrl Pts',(17.8080927577167,17.307218293878,10.744674870173));
#187436=CARTESIAN_POINT('Ctrl Pts',(17.8080238136811,17.3072518264625,10.7446794622027));
#187437=CARTESIAN_POINT('Ctrl Pts',(17.8078957346041,17.3073141293953,10.7446879934013));
#187438=CARTESIAN_POINT('Ctrl Pts',(17.8078365979246,17.3073428993172,10.7446919326125));
#187439=CARTESIAN_POINT('Ctrl Pts',(17.8077088154405,17.307405072702,10.744700444858));
#187440=CARTESIAN_POINT('Ctrl Pts',(17.8076401687993,17.3074384777564,10.7447050180124));
#187441=CARTESIAN_POINT('Ctrl Pts',(17.8075052320939,17.3075041501287,10.7447140078214));
#187442=CARTESIAN_POINT('Ctrl Pts',(17.8074389445209,17.3075364159238,10.7447184242929));
#187443=CARTESIAN_POINT('Ctrl Pts',(17.8073086442183,17.3075998486424,10.7447271061314));
#187444=CARTESIAN_POINT('Ctrl Pts',(17.8072446309937,17.3076310155184,10.7447313715156));
#187445=CARTESIAN_POINT('Ctrl Pts',(17.807118796977,17.3076922896677,10.7447397566241));
#187446=CARTESIAN_POINT('Ctrl Pts',(17.8070569756069,17.3077223969539,10.7447438763723));
#187447=CARTESIAN_POINT('Ctrl Pts',(17.8069354460599,17.3077815897174,10.744751975446));
#187448=CARTESIAN_POINT('Ctrl Pts',(17.8068757371987,17.307810675278,10.7447559548034));
#187449=CARTESIAN_POINT('Ctrl Pts',(17.8067583561941,17.3078678611018,10.7447637781518));
#187450=CARTESIAN_POINT('Ctrl Pts',(17.8067006834021,17.3078959614482,10.7447676221733));
#187451=CARTESIAN_POINT('Ctrl Pts',(17.8065873010777,17.307951211945,10.7447751797086));
#187452=CARTESIAN_POINT('Ctrl Pts',(17.8065315908239,17.3079783622302,10.7447788932586));
#187453=CARTESIAN_POINT('Ctrl Pts',(17.806422063013,17.3080317463502,10.7447861945193));
#187454=CARTESIAN_POINT('Ctrl Pts',(17.8063682446217,17.30805798039,10.7447897822746));
#187455=CARTESIAN_POINT('Ctrl Pts',(17.8062624323477,17.3081095646591,10.744796836459));
#187456=CARTESIAN_POINT('Ctrl Pts',(17.8062104376947,17.3081349150761,10.7448003029293));
#187457=CARTESIAN_POINT('Ctrl Pts',(17.806108207636,17.3081847633608,10.7448071188641));
#187458=CARTESIAN_POINT('Ctrl Pts',(17.8060579713042,17.308209261505,10.7448104683809));
#187459=CARTESIAN_POINT('Ctrl Pts',(17.8059591948887,17.3082574354464,10.7448170545809));
#187460=CARTESIAN_POINT('Ctrl Pts',(17.8059106538732,17.308281111535,10.7448202913175));
#187461=CARTESIAN_POINT('Ctrl Pts',(17.8058152075798,17.3083276703955,10.7448266559656));
#187462=CARTESIAN_POINT('Ctrl Pts',(17.8057683012866,17.3083505535107,10.7448297839365));
#187463=CARTESIAN_POINT('Ctrl Pts',(17.80567606627,17.3083955543501,10.7448359349077));
#187464=CARTESIAN_POINT('Ctrl Pts',(17.8056307364209,17.3084176724819,10.7448389579754));
#187465=CARTESIAN_POINT('Ctrl Pts',(17.8055416032693,17.30846116783,10.7448449025198));
#187466=CARTESIAN_POINT('Ctrl Pts',(17.8054977987418,17.3084825455108,10.7448478240708));
#187467=CARTESIAN_POINT('Ctrl Pts',(17.8054116380863,17.3085245977047,10.7448535707732));
#187468=CARTESIAN_POINT('Ctrl Pts',(17.8053692955266,17.3085452654717,10.7448563950126));
#187469=CARTESIAN_POINT('Ctrl Pts',(17.8052860248987,17.3085859140224,10.7448619493331));
#187470=CARTESIAN_POINT('Ctrl Pts',(17.8052450968604,17.3086058946768,10.7448646794059));
#187471=CARTESIAN_POINT('Ctrl Pts',(17.805164605607,17.3086451929093,10.7448700486875));
#187472=CARTESIAN_POINT('Ctrl Pts',(17.8051250422739,17.3086645104378,10.7448726878984));
#187473=CARTESIAN_POINT('Ctrl Pts',(17.7985011501907,17.311899004069,10.7453145718262));
#187474=CARTESIAN_POINT('Ctrl Pts',(17.7919336235539,17.3151483098601,10.7457550069991));
#187475=CARTESIAN_POINT('Ctrl Pts',(17.7737986951425,17.3242381258899,10.7469776667063));
#187476=CARTESIAN_POINT('Ctrl Pts',(17.7622679932774,17.3301507740256,10.747762415341));
#187477=CARTESIAN_POINT('Ctrl Pts',(17.7366952585574,17.3435617439011,10.7495195293927));
#187478=CARTESIAN_POINT('Ctrl Pts',(17.7226821651151,17.3511132822686,10.7504937426596));
#187479=CARTESIAN_POINT('Ctrl Pts',(17.6796445474024,17.3749360815964,10.7535215780836));
#187480=CARTESIAN_POINT('Ctrl Pts',(17.6509185467627,17.3917335253399,10.7555935546413));
#187481=CARTESIAN_POINT('Ctrl Pts',(17.5398316012297,17.4602549366746,10.7638101234837));
#187482=CARTESIAN_POINT('Ctrl Pts',(17.460686968916,17.5169466884081,10.7701220025741));
#187483=CARTESIAN_POINT('Ctrl Pts',(17.2630943013048,17.6801745733501,10.7869860853912));
#187484=CARTESIAN_POINT('Ctrl Pts',(17.1522643756485,17.7949814291251,10.7976554552696));
#187485=CARTESIAN_POINT('Ctrl Pts',(17.0465207438521,17.9325978306237,10.8084633883669));
#187486=CARTESIAN_POINT('Ctrl Pts',(17.0378225548171,17.9441612386155,10.8093575252665));
#187487=CARTESIAN_POINT('Ctrl Pts',(17.0259221726123,17.9603239779325,10.8105869635517));
#187488=CARTESIAN_POINT('Ctrl Pts',(17.0226188805738,17.9648479056299,10.8109289005769));
#187489=CARTESIAN_POINT('Ctrl Pts',(17.0173544802148,17.972118025886,10.811474849864));
#187490=CARTESIAN_POINT('Ctrl Pts',(17.0153819412441,17.9748558519041,10.8116796437401));
#187491=CARTESIAN_POINT('Ctrl Pts',(17.0112833764433,17.980573312696,10.8121056275169));
#187492=CARTESIAN_POINT('Ctrl Pts',(17.0091585262205,17.9835537533395,10.8123267317868));
#187493=CARTESIAN_POINT('Ctrl Pts',(17.0040506283553,17.9907578482032,10.8128589034139));
#187494=CARTESIAN_POINT('Ctrl Pts',(17.00107527965,17.9949869851174,10.8131694435653));
#187495=CARTESIAN_POINT('Ctrl Pts',(16.9907892868477,18.009721837901,10.8142450855552));
#187496=CARTESIAN_POINT('Ctrl Pts',(16.9835582754486,18.0202831569854,10.8150049481536));
#187497=CARTESIAN_POINT('Ctrl Pts',(16.9419209234204,18.0822960722414,10.8194062547253));
#187498=CARTESIAN_POINT('Ctrl Pts',(16.909685385747,18.1351758513538,10.8229192027546));
#187499=CARTESIAN_POINT('Ctrl Pts',(16.7964878859874,18.3406270456282,10.8359751612939));
#187500=CARTESIAN_POINT('Ctrl Pts',(16.7319777455018,18.5014830941564,10.8450643141511));
#187501=CARTESIAN_POINT('Ctrl Pts',(16.6773854536263,18.7073623694484,10.8569814755598));
#187502=CARTESIAN_POINT('Ctrl Pts',(16.6681681803629,18.7466155845529,10.8592625159251));
#187503=CARTESIAN_POINT('Ctrl Pts',(16.65885732692,18.7920622410054,10.8619252933743));
#187504=CARTESIAN_POINT('Ctrl Pts',(16.6576628198152,18.7980231571865,10.8622749747557));
#187505=CARTESIAN_POINT('Ctrl Pts',(16.6558534174598,18.8072588906171,10.8628174652843));
#187506=CARTESIAN_POINT('Ctrl Pts',(16.6552205441102,18.8105301815036,10.8630097508983));
#187507=CARTESIAN_POINT('Ctrl Pts',(16.6491723848835,18.8421934826621,10.8648722695303));
#187508=CARTESIAN_POINT('Ctrl Pts',(16.6443315775463,18.8706910269824,10.8665591920273));
#187509=CARTESIAN_POINT('Ctrl Pts',(16.6385322992379,18.909646377655,10.8688831261859));
#187510=CARTESIAN_POINT('Ctrl Pts',(16.6370657829911,18.9200261623686,10.8695040672793));
#187511=CARTESIAN_POINT('Ctrl Pts',(16.634862066262,18.9365064863082,10.8704928394284));
#187512=CARTESIAN_POINT('Ctrl Pts',(16.6340742197246,18.9426001676087,10.8708590665784));
#187513=CARTESIAN_POINT('Ctrl Pts',(16.6325483600515,18.9548202163897,10.8715947703817));
#187514=CARTESIAN_POINT('Ctrl Pts',(16.6318105821765,18.9609465518859,10.8719642506085));
#187515=CARTESIAN_POINT('Ctrl Pts',(16.6303836082957,18.9732486772884,10.8727075230525));
#187516=CARTESIAN_POINT('Ctrl Pts',(16.6296947992168,18.9794244495415,10.873081323587));
#187517=CARTESIAN_POINT('Ctrl Pts',(16.6281826817362,18.9935460159799,10.873937626837));
#187518=CARTESIAN_POINT('Ctrl Pts',(16.6273771408042,19.0014935813907,10.8744206846731));
#187519=CARTESIAN_POINT('Ctrl Pts',(16.6254321893437,19.0218293069931,10.8756596709703));
#187520=CARTESIAN_POINT('Ctrl Pts',(16.6243569721749,19.0342231689276,10.8764176018163));
#187521=CARTESIAN_POINT('Ctrl Pts',(16.6190952486465,19.1017850249937,10.8805650384811));
#187522=CARTESIAN_POINT('Ctrl Pts',(16.6169637967665,19.1570864436259,10.8840179272398));
#187523=CARTESIAN_POINT('Ctrl Pts',(16.6170004651127,19.2124033128222,10.8875305623383));
#187524=CARTESIAN_POINT('Ctrl Pts',(16.7454193623258,19.9371102171621,10.9336112429045));
#187525=CARTESIAN_POINT('Ctrl Pts',(16.7173390128125,19.8602072373921,10.9286590653809));
#187526=CARTESIAN_POINT('Ctrl Pts',(16.6936915503228,19.781585811724,10.9237068878573));
#187527=CARTESIAN_POINT('Ctrl Pts',(16.6746638706561,19.7017379202578,10.9187547103338));
#187528=CARTESIAN_POINT('Ctrl Pts',(16.6556455622465,19.6219293544019,10.9138049717901));
#187529=CARTESIAN_POINT('Ctrl Pts',(16.6412426570166,19.5408957414284,10.9088552332465));
#187530=CARTESIAN_POINT('Ctrl Pts',(16.6315940722725,19.4591497835104,10.9039054947028));
#187531=CARTESIAN_POINT('Ctrl Pts',(16.6219454875284,19.3774038255923,10.8989557561591));
#187532=CARTESIAN_POINT('Ctrl Pts',(16.6170514009658,19.2949457511214,10.8940060176155));
#187533=CARTESIAN_POINT('Ctrl Pts',(16.6170004031077,19.2123064294672,10.8890562790718));
#187534=CARTESIAN_POINT('Origin',(18.734,19.211,0.));
#187535=CARTESIAN_POINT('',(16.7454193623241,19.9371102171575,11.9535387334123));
#187536=CARTESIAN_POINT('',(16.7460270442576,19.936878801227,11.7337477294316));
#187537=CARTESIAN_POINT('',(16.7454193623258,19.9371102171621,0.));
#187538=CARTESIAN_POINT('Ctrl Pts',(16.7454193623241,19.9371102171575,11.9535387334123));
#187539=CARTESIAN_POINT('Ctrl Pts',(16.7451290268508,19.9363150823599,11.9534866359792));
#187540=CARTESIAN_POINT('Ctrl Pts',(16.7448391668873,19.9355197696119,11.9534345643187));
#187541=CARTESIAN_POINT('Ctrl Pts',(16.7420974952995,19.9279831713629,11.9529414752215));
#187542=CARTESIAN_POINT('Ctrl Pts',(16.7396794458117,19.921229531058,11.9525023096659));
#187543=CARTESIAN_POINT('Ctrl Pts',(16.7359349682283,19.9106012424581,11.951815566168));
#187544=CARTESIAN_POINT('Ctrl Pts',(16.7345854012506,19.9067348867221,11.9515666491811));
#187545=CARTESIAN_POINT('Ctrl Pts',(16.7320789914907,19.8994867825225,11.9511017428328));
#187546=CARTESIAN_POINT('Ctrl Pts',(16.7309195068312,19.8961060590327,11.9508856034616));
#187547=CARTESIAN_POINT('Ctrl Pts',(16.7282860711328,19.8883638826122,11.9503922206569));
#187548=CARTESIAN_POINT('Ctrl Pts',(16.7268177842271,19.8840005553657,11.9501153139117));
#187549=CARTESIAN_POINT('Ctrl Pts',(16.722327343384,19.8705108381309,11.9492626834733));
#187550=CARTESIAN_POINT('Ctrl Pts',(16.7193530648855,19.8613684784025,11.9486897092102));
#187551=CARTESIAN_POINT('Ctrl Pts',(16.6905473891357,19.7707312275937,11.9430544686176));
#187552=CARTESIAN_POINT('Ctrl Pts',(16.6696094506914,19.6877523770249,11.9382547439852));
#187553=CARTESIAN_POINT('Ctrl Pts',(16.6294008130744,19.474768539116,11.9263203647501));
#187554=CARTESIAN_POINT('Ctrl Pts',(16.6170990834764,19.3438276878587,11.9193213153926));
#187555=CARTESIAN_POINT('Ctrl Pts',(16.616931378433,19.1203529379548,11.9069620233889));
#187556=CARTESIAN_POINT('Ctrl Pts',(16.6228899847845,19.0282216733242,11.9017508201384));
#187557=CARTESIAN_POINT('Ctrl Pts',(16.6366195088672,18.9231219351655,11.8955371625626));
#187558=CARTESIAN_POINT('Ctrl Pts',(16.6385368144155,18.9094826219187,11.894725665816));
#187559=CARTESIAN_POINT('Ctrl Pts',(16.6418231765306,18.8876517422287,11.893418186782));
#187560=CARTESIAN_POINT('Ctrl Pts',(16.6431076013345,18.8794476954235,11.8929248814234));
#187561=CARTESIAN_POINT('Ctrl Pts',(16.6454726643803,18.864901816223,11.8920466899971));
#187562=CARTESIAN_POINT('Ctrl Pts',(16.6465340101855,18.8585569203376,11.8916624206906));
#187563=CARTESIAN_POINT('Ctrl Pts',(16.6488043608628,18.8453544977507,11.8908602872554));
#187564=CARTESIAN_POINT('Ctrl Pts',(16.650018311446,18.838497910394,11.8904422699565));
#187565=CARTESIAN_POINT('Ctrl Pts',(16.6532558832587,18.8207228839739,11.8893548175654));
#187566=CARTESIAN_POINT('Ctrl Pts',(16.6553316037841,18.8098142601474,11.8886837297044));
#187567=CARTESIAN_POINT('Ctrl Pts',(16.6646897663983,18.7626573631951,11.8857662552718));
#187568=CARTESIAN_POINT('Ctrl Pts',(16.6728349235718,18.7265887901512,11.8834924945459));
#187569=CARTESIAN_POINT('Ctrl Pts',(16.6969459261816,18.6314844021895,11.8773804480956));
#187570=CARTESIAN_POINT('Ctrl Pts',(16.7145314183952,18.5728987707211,11.8734934714816));
#187571=CARTESIAN_POINT('Ctrl Pts',(16.786380717627,18.3664523620685,11.8593774937429));
#187572=CARTESIAN_POINT('Ctrl Pts',(16.8545581904161,18.2239974661177,11.8488054422961));
#187573=CARTESIAN_POINT('Ctrl Pts',(16.9705615847297,18.0380622514951,11.8345700363483));
#187574=CARTESIAN_POINT('Ctrl Pts',(17.0055074497953,17.9871482818579,11.8306273509307));
#187575=CARTESIAN_POINT('Ctrl Pts',(17.0481242922943,17.9305330896517,11.8262535613372));
#187576=CARTESIAN_POINT('Ctrl Pts',(17.0536641360199,17.9232718448985,11.8256928151803));
#187577=CARTESIAN_POINT('Ctrl Pts',(17.0620088016684,17.912479780531,11.8248600185695));
#187578=CARTESIAN_POINT('Ctrl Pts',(17.0647781094392,17.908921811637,11.824585559953));
#187579=CARTESIAN_POINT('Ctrl Pts',(17.0697578748995,17.9025658735866,11.8240954913808));
#187580=CARTESIAN_POINT('Ctrl Pts',(17.0719640458661,17.8997646275772,11.8238795845244));
#187581=CARTESIAN_POINT('Ctrl Pts',(17.0767598339052,17.8937068122788,11.8234128568554));
#187582=CARTESIAN_POINT('Ctrl Pts',(17.0793519685854,17.8904523093223,11.823162220118));
#187583=CARTESIAN_POINT('Ctrl Pts',(17.0866261898216,17.8813743522364,11.822463342103));
#187584=CARTESIAN_POINT('Ctrl Pts',(17.0913295915774,17.8755679475459,11.8220166018962));
#187585=CARTESIAN_POINT('Ctrl Pts',(17.1189522482874,17.8418342052015,11.8194219454171));
#187586=CARTESIAN_POINT('Ctrl Pts',(17.1425541219988,17.8144705220699,11.8173204104481));
#187587=CARTESIAN_POINT('Ctrl Pts',(17.2209740847264,17.7281232449019,11.8106490502104));
#187588=CARTESIAN_POINT('Ctrl Pts',(17.2784620503688,17.6716552706437,11.8062219711733));
#187589=CARTESIAN_POINT('Ctrl Pts',(17.4407086333482,17.5295249399828,11.7944648949924));
#187590=CARTESIAN_POINT('Ctrl Pts',(17.5506773655383,17.4504015889066,11.7872133827168));
#187591=CARTESIAN_POINT('Ctrl Pts',(17.7219080787525,17.3505335687752,11.776062980708));
#187592=CARTESIAN_POINT('Ctrl Pts',(17.7777669708736,17.3212162325674,11.772449331803));
#187593=CARTESIAN_POINT('Ctrl Pts',(17.8461536571563,17.2891327204718,11.7680131702154));
#187594=CARTESIAN_POINT('Ctrl Pts',(17.8575064954522,17.2839286222097,11.7672763922841));
#187595=CARTESIAN_POINT('Ctrl Pts',(17.8762116340555,17.2755537423078,11.7660616256793));
#187596=CARTESIAN_POINT('Ctrl Pts',(17.883537153945,17.2723236366138,11.765585676383));
#187597=CARTESIAN_POINT('Ctrl Pts',(17.8967322209495,17.2665945997368,11.7647279263509));
#187598=CARTESIAN_POINT('Ctrl Pts',(17.9025951013253,17.2640804876699,11.7643466498865));
#187599=CARTESIAN_POINT('Ctrl Pts',(17.9150971771305,17.2587861349701,11.7635332360662));
#187600=CARTESIAN_POINT('Ctrl Pts',(17.921739354713,17.2560131841253,11.7631008565504));
#187601=CARTESIAN_POINT('Ctrl Pts',(17.9396435883359,17.2486455888189,11.7619346948704));
#187602=CARTESIAN_POINT('Ctrl Pts',(17.9509311878002,17.2441140934168,11.7611987885809));
#187603=CARTESIAN_POINT('Ctrl Pts',(18.0072712518788,17.2220577795327,11.7575216494345));
#187604=CARTESIAN_POINT('Ctrl Pts',(18.052872674146,17.205983592002,11.7545322703025));
#187605=CARTESIAN_POINT('Ctrl Pts',(18.185439394958,17.1642991658036,11.7457982236481));
#187606=CARTESIAN_POINT('Ctrl Pts',(18.2735446935313,17.1426961494182,11.7399361871599));
#187607=CARTESIAN_POINT('Ctrl Pts',(18.521323084779,17.0985608225958,11.7234139787401));
#187608=CARTESIAN_POINT('Ctrl Pts',(18.6826001408388,17.088503163016,11.7125879234403));
#187609=CARTESIAN_POINT('Ctrl Pts',(18.8634453702092,17.097866469298,11.7012278450611));
#187610=CARTESIAN_POINT('Ctrl Pts',(18.8834143387194,17.0991844671051,11.6999848858957));
#187611=CARTESIAN_POINT('Ctrl Pts',(18.9097243575146,17.101296066981,11.6983649308391));
#187612=CARTESIAN_POINT('Ctrl Pts',(18.9160840370131,17.1018354401103,11.6979747208991));
#187613=CARTESIAN_POINT('Ctrl Pts',(18.926345008534,17.1027524437223,11.6973474534102));
#187614=CARTESIAN_POINT('Ctrl Pts',(18.9302478042486,17.1031121565025,11.6971094107527));
#187615=CARTESIAN_POINT('Ctrl Pts',(18.9377537164033,17.1038249883426,11.6966526736526));
#187616=CARTESIAN_POINT('Ctrl Pts',(18.9413569292791,17.1041765117315,11.6964338952279));
#187617=CARTESIAN_POINT('Ctrl Pts',(18.9498789862241,17.1050299836163,11.6959175573198));
#187618=CARTESIAN_POINT('Ctrl Pts',(18.9547970419502,17.1055399281874,11.6956204467097));
#187619=CARTESIAN_POINT('Ctrl Pts',(18.9711038049876,17.1072885129879,11.6946380612876));
#187620=CARTESIAN_POINT('Ctrl Pts',(18.9824844704968,17.1086023887075,11.6939568833196));
#187621=CARTESIAN_POINT('Ctrl Pts',(19.1109324947416,17.1244890590825,11.6863133149267));
#187622=CARTESIAN_POINT('Ctrl Pts',(19.2266129258574,17.1487327291917,11.6798419021154));
#187623=CARTESIAN_POINT('Ctrl Pts',(19.5086719421455,17.2329516115556,11.6638230600567));
#187624=CARTESIAN_POINT('Ctrl Pts',(19.6706728924389,17.304319827775,11.6543458740009));
#187625=CARTESIAN_POINT('Ctrl Pts',(19.8416151672737,17.4067263706571,11.6427658792243));
#187626=CARTESIAN_POINT('Ctrl Pts',(19.8610904185327,17.4188276264973,11.641422579047));
#187627=CARTESIAN_POINT('Ctrl Pts',(19.8883814409061,17.4364061254231,11.6395041256385));
#187628=CARTESIAN_POINT('Ctrl Pts',(19.8963630560191,17.441623823978,11.6389386005849));
#187629=CARTESIAN_POINT('Ctrl Pts',(19.9092796865872,17.4501927308181,11.638016031709));
#187630=CARTESIAN_POINT('Ctrl Pts',(19.9142363246372,17.453511223992,11.637660219825));
#187631=CARTESIAN_POINT('Ctrl Pts',(19.9245865375435,17.4605042732831,11.6369134495187));
#187632=CARTESIAN_POINT('Ctrl Pts',(19.9299772703034,17.4641829059483,11.6365223392293));
#187633=CARTESIAN_POINT('Ctrl Pts',(19.9427688964197,17.472998872286,11.6355890554431));
#187634=CARTESIAN_POINT('Ctrl Pts',(19.9501541300167,17.4781586070825,11.635046031337));
#187635=CARTESIAN_POINT('Ctrl Pts',(19.9749601424897,17.4957261561287,11.6332077271044));
#187636=CARTESIAN_POINT('Ctrl Pts',(19.9922253197168,17.5083504685743,11.6319041429512));
#187637=CARTESIAN_POINT('Ctrl Pts',(20.0854145658999,17.5786820065511,11.6247326934401));
#187638=CARTESIAN_POINT('Ctrl Pts',(20.1575544480654,17.6412000611845,11.6186752640702));
#187639=CARTESIAN_POINT('Ctrl Pts',(20.3463173134782,17.8285292930982,11.601393168069));
#187640=CARTESIAN_POINT('Ctrl Pts',(20.4524301921778,17.9628866480319,11.5898824037791));
#187641=CARTESIAN_POINT('Ctrl Pts',(20.5603509505221,18.1397979273546,11.5766576666444));
#187642=CARTESIAN_POINT('Ctrl Pts',(20.57861949941,18.1715718157039,11.5743529639277));
#187643=CARTESIAN_POINT('Ctrl Pts',(20.5994487038554,18.2100799178343,11.5716570035792));
#187644=CARTESIAN_POINT('Ctrl Pts',(20.602810589737,18.21637099349,11.5712196051305));
#187645=CARTESIAN_POINT('Ctrl Pts',(20.6082459609496,18.226667020723,11.5705088550857));
#187646=CARTESIAN_POINT('Ctrl Pts',(20.6103385276089,18.2306617589275,11.5702343378718));
#187647=CARTESIAN_POINT('Ctrl Pts',(20.6140628232737,18.2378270990376,11.5697442062462));
#187648=CARTESIAN_POINT('Ctrl Pts',(20.6156993150121,18.2409951530477,11.5695282946073));
#187649=CARTESIAN_POINT('Ctrl Pts',(20.6192276530486,18.2478681290267,11.5690616039283));
#187650=CARTESIAN_POINT('Ctrl Pts',(20.6211165800761,18.2515744851269,11.5688110087091));
#187651=CARTESIAN_POINT('Ctrl Pts',(20.626366437074,18.2619509741536,11.5681123636846));
#187652=CARTESIAN_POINT('Ctrl Pts',(20.6297030491524,18.2686334371222,11.5676658133312));
#187653=CARTESIAN_POINT('Ctrl Pts',(20.6489484254469,18.3076933513134,11.5650744951055));
#187654=CARTESIAN_POINT('Ctrl Pts',(20.6640639132924,18.3404576321502,11.5629759692517));
#187655=CARTESIAN_POINT('Ctrl Pts',(20.7101041284028,18.4473563975019,11.5563185937797));
#187656=CARTESIAN_POINT('Ctrl Pts',(20.7376520855221,18.5228725301513,11.5519018029582));
#187657=CARTESIAN_POINT('Ctrl Pts',(20.814350346623,18.7772073608206,11.5374210755901));
#187658=CARTESIAN_POINT('Ctrl Pts',(20.8443233527318,18.9608741795873,11.5275076728548));
#187659=CARTESIAN_POINT('Ctrl Pts',(20.850683492793,19.1682208228441,11.5154430554136));
#187660=CARTESIAN_POINT('Ctrl Pts',(20.8510150821734,19.1903565020096,11.514145375606));
#187661=CARTESIAN_POINT('Ctrl Pts',(20.8509935059029,19.2209564225428,11.5123365701689));
#187662=CARTESIAN_POINT('Ctrl Pts',(20.8509367816855,19.229419923203,11.5118347054949));
#187663=CARTESIAN_POINT('Ctrl Pts',(20.8507521095536,19.2439615597,11.5109696283486));
#187664=CARTESIAN_POINT('Ctrl Pts',(20.8506487283448,19.2500399452842,11.5106071882997));
#187665=CARTESIAN_POINT('Ctrl Pts',(20.8503817373643,19.262564760712,11.5098585984424));
#187666=CARTESIAN_POINT('Ctrl Pts',(20.8502148518894,19.2690110507754,11.5094723497967));
#187667=CARTESIAN_POINT('Ctrl Pts',(20.8497582249999,19.2840015033914,11.5085718683574));
#187668=CARTESIAN_POINT('Ctrl Pts',(20.8494461760307,19.2925448288995,11.508056941505));
#187669=CARTESIAN_POINT('Ctrl Pts',(20.8482832880671,19.3198476914612,11.506405690706));
#187670=CARTESIAN_POINT('Ctrl Pts',(20.8472346028292,19.3385974916544,11.5052631939268));
#187671=CARTESIAN_POINT('Ctrl Pts',(20.8407644072337,19.4319796143988,11.4995290342648));
#187672=CARTESIAN_POINT('Ctrl Pts',(20.8316385705084,19.5062940176621,11.4948225831321));
#187673=CARTESIAN_POINT('Ctrl Pts',(20.7996299614578,19.687139086067,11.483024051358));
#187674=CARTESIAN_POINT('Ctrl Pts',(20.7724244874635,19.7926852207526,11.4758315175729));
#187675=CARTESIAN_POINT('Ctrl Pts',(20.6984130390039,20.0092325456473,11.4607128992608));
#187676=CARTESIAN_POINT('Ctrl Pts',(20.6500047460643,20.1193095677476,11.4528146158638));
#187677=CARTESIAN_POINT('Ctrl Pts',(20.5879671131522,20.2330496086128,11.4448124904301));
#187678=CARTESIAN_POINT('Ctrl Pts',(20.5833565701869,20.241368741364,11.4442282413917));
#187679=CARTESIAN_POINT('Ctrl Pts',(20.5764411833575,20.2536507062563,11.443367551538));
#187680=CARTESIAN_POINT('Ctrl Pts',(20.5741793569393,20.257637446586,11.443088464346));
#187681=CARTESIAN_POINT('Ctrl Pts',(20.5701318464466,20.2647179898275,11.4425933662205));
#187682=CARTESIAN_POINT('Ctrl Pts',(20.568351266249,20.2678146442444,11.4423770326644));
#187683=CARTESIAN_POINT('Ctrl Pts',(20.564505999401,20.2744630521267,11.4419130028762));
#187684=CARTESIAN_POINT('Ctrl Pts',(20.5624388157592,20.2780132964338,11.4416654714748));
#187685=CARTESIAN_POINT('Ctrl Pts',(20.5567036949756,20.2877973596427,11.4409839591826));
#187686=CARTESIAN_POINT('Ctrl Pts',(20.5530140856026,20.2940185008691,11.440551360865));
#187687=CARTESIAN_POINT('Ctrl Pts',(20.5326181655577,20.3280102918894,11.4381910441826));
#187688=CARTESIAN_POINT('Ctrl Pts',(20.5153067554257,20.3554150470175,11.436300466029));
#187689=CARTESIAN_POINT('Ctrl Pts',(20.4072947045071,20.5180096149243,11.4250911199681));
#187690=CARTESIAN_POINT('Ctrl Pts',(20.3018689459553,20.6427779714588,11.416486910597));
#187691=CARTESIAN_POINT('Ctrl Pts',(20.09793873662,20.8342779509002,11.4011722330067));
#187692=CARTESIAN_POINT('Ctrl Pts',(20.006231539933,20.9071078444334,11.3946449646661));
#187693=CARTESIAN_POINT('Ctrl Pts',(19.8971257895582,20.9799066663237,11.386960711716));
#187694=CARTESIAN_POINT('Ctrl Pts',(19.8851829588666,20.9877020506805,11.3861208407895));
#187695=CARTESIAN_POINT('Ctrl Pts',(19.8660430767335,20.9999211319645,11.3847763911939));
#187696=CARTESIAN_POINT('Ctrl Pts',(19.8588966067553,21.0044235319427,11.384274739009));
#187697=CARTESIAN_POINT('Ctrl Pts',(19.8462410710984,21.0122913348911,11.3833868836638));
#187698=CARTESIAN_POINT('Ctrl Pts',(19.840743166652,21.0156745510025,11.3830013438486));
#187699=CARTESIAN_POINT('Ctrl Pts',(19.8293356543442,21.0226225973459,11.3822016999385));
#187700=CARTESIAN_POINT('Ctrl Pts',(19.8234239229801,21.0261837772457,11.3817874680774));
#187701=CARTESIAN_POINT('Ctrl Pts',(19.8081959275306,21.0352558129019,11.3807208267198));
#187702=CARTESIAN_POINT('Ctrl Pts',(19.7988547052325,21.040724190024,11.3800668814504));
#187703=CARTESIAN_POINT('Ctrl Pts',(19.7596174765505,21.0632915349395,11.3773212180823));
#187704=CARTESIAN_POINT('Ctrl Pts',(19.7293497752228,21.0797305168827,11.3752059633401));
#187705=CARTESIAN_POINT('Ctrl Pts',(19.6493784143508,21.1206703889558,11.369620985308));
#187706=CARTESIAN_POINT('Ctrl Pts',(19.5990925190084,21.1439699263036,11.3661123489404));
#187707=CARTESIAN_POINT('Ctrl Pts',(19.4467384063022,21.2074254863261,11.3555014376942));
#187708=CARTESIAN_POINT('Ctrl Pts',(19.3424074793955,21.2416520229834,11.3482509136916));
#187709=CARTESIAN_POINT('Ctrl Pts',(19.1747107431891,21.2825768883695,11.3368488670876));
#187710=CARTESIAN_POINT('Ctrl Pts',(19.1128778844095,21.2947727674556,11.3326994998946));
#187711=CARTESIAN_POINT('Ctrl Pts',(19.0438800960324,21.3052085363039,11.3281829746019));
#187712=CARTESIAN_POINT('Ctrl Pts',(19.0371642199998,21.30619128596,11.3277445549054));
#187713=CARTESIAN_POINT('Ctrl Pts',(19.024295039637,21.3080112903441,11.3269068594373));
#187714=CARTESIAN_POINT('Ctrl Pts',(19.0181425530176,21.3088538015726,11.3265074312346));
#187715=CARTESIAN_POINT('Ctrl Pts',(18.9688108796419,21.3153881967183,11.3233136428653));
#187716=CARTESIAN_POINT('Ctrl Pts',(18.9254656145631,21.3197738974488,11.320561820466));
#187717=CARTESIAN_POINT('Ctrl Pts',(18.8745136451574,21.3233450067153,11.3174139063159));
#187718=CARTESIAN_POINT('Ctrl Pts',(18.8670117286538,21.3238306595101,11.3169526273957));
#187719=CARTESIAN_POINT('Ctrl Pts',(18.8548894646491,21.3245505994799,11.3162109846748));
#187720=CARTESIAN_POINT('Ctrl Pts',(18.8502707344577,21.3248097162401,11.3159292844753));
#187721=CARTESIAN_POINT('Ctrl Pts',(18.8420797806199,21.3252423113772,11.3154313066971));
#187722=CARTESIAN_POINT('Ctrl Pts',(18.838507932476,21.3254218791267,11.3152146920184));
#187723=CARTESIAN_POINT('Ctrl Pts',(18.8308592081091,21.3257869746991,11.314752000603));
#187724=CARTESIAN_POINT('Ctrl Pts',(18.8267822566414,21.3259697652809,11.3145060785246));
#187725=CARTESIAN_POINT('Ctrl Pts',(18.815601521543,21.3264386628916,11.3138335222304));
#187726=CARTESIAN_POINT('Ctrl Pts',(18.8084967102127,21.3267007794601,11.3134082111764));
#187727=CARTESIAN_POINT('Ctrl Pts',(18.7707404119018,21.3279032875953,11.3111583671086));
#187728=CARTESIAN_POINT('Ctrl Pts',(18.7400708072438,21.328213440811,11.309366993464));
#187729=CARTESIAN_POINT('Ctrl Pts',(18.647516376947,21.3271380201154,11.3040413601126));
#187730=CARTESIAN_POINT('Ctrl Pts',(18.5856858241574,21.323705269713,11.3005915993964));
#187731=CARTESIAN_POINT('Ctrl Pts',(18.3776128451735,21.3029717840945,11.2890938563863));
#187732=CARTESIAN_POINT('Ctrl Pts',(18.2330600690706,21.27313910069,11.2812648274557));
#187733=CARTESIAN_POINT('Ctrl Pts',(18.0216914871102,21.2059606560408,11.2688802993139));
#187734=CARTESIAN_POINT('Ctrl Pts',(17.9518634479933,21.1796320398422,11.2646305106726));
#187735=CARTESIAN_POINT('Ctrl Pts',(17.8715560718002,21.1444041776926,11.2594850483937));
#187736=CARTESIAN_POINT('Ctrl Pts',(17.8595869076564,21.1390204812067,11.2587112955402));
#187737=CARTESIAN_POINT('Ctrl Pts',(17.8402224192874,21.1300929809537,11.2574479303016));
#187738=CARTESIAN_POINT('Ctrl Pts',(17.8327961548068,21.1266168353431,11.2569606475912));
#187739=CARTESIAN_POINT('Ctrl Pts',(17.8196096840524,21.120350756607,11.256090354038));
#187740=CARTESIAN_POINT('Ctrl Pts',(17.813841553171,21.1175776650832,11.2557079311689));
#187741=CARTESIAN_POINT('Ctrl Pts',(17.8080207710294,21.1147466934437,11.2553202426781));
#187742=CARTESIAN_POINT('Ctrl Pts',(17.8079554093732,21.1147149002549,11.2553158890908));
#187743=CARTESIAN_POINT('Ctrl Pts',(17.8078339885017,21.1146558310345,11.255307801109));
#187744=CARTESIAN_POINT('Ctrl Pts',(17.8077779250923,21.1146285540619,11.2553040664948));
#187745=CARTESIAN_POINT('Ctrl Pts',(17.8076538533986,21.1145681817042,11.2552958011998));
#187746=CARTESIAN_POINT('Ctrl Pts',(17.8075858444125,21.114535084533,11.2552912703936));
#187747=CARTESIAN_POINT('Ctrl Pts',(17.807452159529,21.1144700167466,11.2552823637298));
#187748=CARTESIAN_POINT('Ctrl Pts',(17.8073864863653,21.1144380477662,11.2552779880711));
#187749=CARTESIAN_POINT('Ctrl Pts',(17.8072573926156,21.1143751980715,11.2552693863875));
#187750=CARTESIAN_POINT('Ctrl Pts',(17.8071939715084,21.1143443173864,11.2552651603432));
#187751=CARTESIAN_POINT('Ctrl Pts',(17.8070693003332,21.1142836054189,11.2552568525009));
#187752=CARTESIAN_POINT('Ctrl Pts',(17.8070080496665,21.1142537741084,11.2552527706773));
#187753=CARTESIAN_POINT('Ctrl Pts',(17.8068876406461,21.1141951233289,11.2552447460723));
#187754=CARTESIAN_POINT('Ctrl Pts',(17.8068284817233,21.114166303828,11.2552408032664));
#187755=CARTESIAN_POINT('Ctrl Pts',(17.8067121810781,21.1141096408034,11.2552330517305));
#187756=CARTESIAN_POINT('Ctrl Pts',(17.8066550384826,21.1140817970828,11.2552292429547));
#187757=CARTESIAN_POINT('Ctrl Pts',(17.8065426972086,21.1140270505878,11.2552217546312));
#187758=CARTESIAN_POINT('Ctrl Pts',(17.806487497978,21.1140001477569,11.2552180750583));
#187759=CARTESIAN_POINT('Ctrl Pts',(17.806378973743,21.1139472497063,11.2552108405295));
#187760=CARTESIAN_POINT('Ctrl Pts',(17.8063256479171,21.113921254284,11.2552072855296));
#187761=CARTESIAN_POINT('Ctrl Pts',(17.806220803362,21.1138701389139,11.2552002957034));
#187762=CARTESIAN_POINT('Ctrl Pts',(17.8061692836892,21.1138450186903,11.2551968608243));
#187763=CARTESIAN_POINT('Ctrl Pts',(17.8060679863102,21.1137956225081,11.2551901069273));
#187764=CARTESIAN_POINT('Ctrl Pts',(17.8060182078432,21.1137713463502,11.2551867878681));
#187765=CARTESIAN_POINT('Ctrl Pts',(17.8059203308769,21.1137236085736,11.2551802615048));
#187766=CARTESIAN_POINT('Ctrl Pts',(17.8058722313404,21.1137001466089,11.2551770541403));
#187767=CARTESIAN_POINT('Ctrl Pts',(17.8057776524382,21.1136540085261,11.255170747205));
#187768=CARTESIAN_POINT('Ctrl Pts',(17.8057311719284,21.1136313319989,11.255167647566));
#187769=CARTESIAN_POINT('Ctrl Pts',(17.8056397731782,21.1135867369853,11.2551615522446));
#187770=CARTESIAN_POINT('Ctrl Pts',(17.8055948538635,21.1135648181136,11.2551585564981));
#187771=CARTESIAN_POINT('Ctrl Pts',(17.8055065277404,21.1135217145418,11.2551526656655));
#187772=CARTESIAN_POINT('Ctrl Pts',(17.8054631194813,21.1135005292644,11.2551497704899));
#187773=CARTESIAN_POINT('Ctrl Pts',(17.8053777363302,21.1134588546397,11.2551440755411));
#187774=CARTESIAN_POINT('Ctrl Pts',(17.8053357757297,21.1134383723897,11.2551412767281));
#187775=CARTESIAN_POINT('Ctrl Pts',(17.805253255661,21.1133980884444,11.2551357723743));
#187776=CARTESIAN_POINT('Ctrl Pts',(17.805212696102,21.1133782868176,11.2551330668337));
#187777=CARTESIAN_POINT('Ctrl Pts',(17.8051329288425,21.1133393403973,11.2551277457562));
#187778=CARTESIAN_POINT('Ctrl Pts',(17.805093720955,21.1133201956176,11.2551251302126));
#187779=CARTESIAN_POINT('Ctrl Pts',(17.79846621008,21.1100838012974,11.2546829975794));
#187780=CARTESIAN_POINT('Ctrl Pts',(17.791894730149,21.1068323804713,11.2542422885588));
#187781=CARTESIAN_POINT('Ctrl Pts',(17.7737379027954,21.0977310738973,11.2530181240525));
#187782=CARTESIAN_POINT('Ctrl Pts',(17.7621894045932,21.0918087609933,11.2522321343146));
#187783=CARTESIAN_POINT('Ctrl Pts',(17.7365723286292,21.0783728613398,11.2504718796223));
#187784=CARTESIAN_POINT('Ctrl Pts',(17.7225328455187,21.0708057792333,11.2494957571305));
#187785=CARTESIAN_POINT('Ctrl Pts',(17.6793927687354,21.0469209289685,11.2464604104779));
#187786=CARTESIAN_POINT('Ctrl Pts',(17.6505924926393,21.0300739535338,11.2443827273179));
#187787=CARTESIAN_POINT('Ctrl Pts',(17.539088083641,20.9612610312077,11.2361333383974));
#187788=CARTESIAN_POINT('Ctrl Pts',(17.459630917763,20.9042831492104,11.2297928851541));
#187789=CARTESIAN_POINT('Ctrl Pts',(17.2624186334956,20.7410991442357,11.2129477485755));
#187790=CARTESIAN_POINT('Ctrl Pts',(17.1521409148208,20.6267976799242,11.2023305703547));
#187791=CARTESIAN_POINT('Ctrl Pts',(17.0467431035819,20.489696998505,11.1915593608907));
#187792=CARTESIAN_POINT('Ctrl Pts',(17.0379707577474,20.4780385490817,11.1906576667491));
#187793=CARTESIAN_POINT('Ctrl Pts',(17.0259863703975,20.4617637812291,11.1894195867916));
#187794=CARTESIAN_POINT('Ctrl Pts',(17.0226713707513,20.457224265418,11.1890764455044));
#187795=CARTESIAN_POINT('Ctrl Pts',(17.0173930949866,20.4499354887966,11.1885290657091));
#187796=CARTESIAN_POINT('Ctrl Pts',(17.0154182778975,20.4471946758364,11.1883240381722));
#187797=CARTESIAN_POINT('Ctrl Pts',(17.0113191227705,20.4414767251303,11.1878979983809));
#187798=CARTESIAN_POINT('Ctrl Pts',(17.0091959336214,20.438498801897,11.1876770699764));
#187799=CARTESIAN_POINT('Ctrl Pts',(17.0040988612963,20.4313104611357,11.1871460343829));
#187800=CARTESIAN_POINT('Ctrl Pts',(17.0011325936524,20.4270946198962,11.1868364487473));
#187801=CARTESIAN_POINT('Ctrl Pts',(16.9909116500558,20.4124546577151,11.1857676402282));
#187802=CARTESIAN_POINT('Ctrl Pts',(16.9837352337982,20.4019758839497,11.1850135678328));
#187803=CARTESIAN_POINT('Ctrl Pts',(16.9426473012017,20.3408070180423,11.1806708939601));
#187804=CARTESIAN_POINT('Ctrl Pts',(16.9108415162874,20.2887304468159,11.1772070877362));
#187805=CARTESIAN_POINT('Ctrl Pts',(16.828339396904,20.1395141436943,11.1677104439598));
#187806=CARTESIAN_POINT('Ctrl Pts',(16.7829144564847,20.0397971661308,11.1618386287765));
#187807=CARTESIAN_POINT('Ctrl Pts',(16.745419285258,19.9371100060985,11.1558808557757));
#187808=CARTESIAN_POINT('',(16.6169841362445,19.2120754279768,11.689056243827));
#187809=CARTESIAN_POINT('Ctrl Pts',(16.6170002731508,19.2120754164278,11.6890562436246));
#187810=CARTESIAN_POINT('Ctrl Pts',(16.6169638390757,19.1403535001558,11.6847206650338));
#187811=CARTESIAN_POINT('Ctrl Pts',(16.6205764456709,19.0684835617616,11.6803850864429));
#187812=CARTESIAN_POINT('Ctrl Pts',(16.6278569147558,18.9968731579697,11.6760495078521));
#187813=CARTESIAN_POINT('Ctrl Pts',(16.6351262827892,18.9253719436775,11.6717205400277));
#187814=CARTESIAN_POINT('Ctrl Pts',(16.6460523594264,18.8541299663727,11.6673915722033));
#187815=CARTESIAN_POINT('Ctrl Pts',(16.660601956967,18.7835546173521,11.663062604379));
#187816=CARTESIAN_POINT('Ctrl Pts',(16.6751392352658,18.7130390249528,11.6587373019207));
#187817=CARTESIAN_POINT('Ctrl Pts',(16.6932938534713,18.6431894242013,11.6544119994624));
#187818=CARTESIAN_POINT('Ctrl Pts',(16.7149810087479,18.5744064774415,11.6500866970042));
#187819=CARTESIAN_POINT('Ctrl Pts',(16.7366573538935,18.5056578160759,11.6457635505265));
#187820=CARTESIAN_POINT('Ctrl Pts',(16.7618625956119,18.4379752252655,11.6414404040489));
#187821=CARTESIAN_POINT('Ctrl Pts',(16.7904616388557,18.3717457841867,11.6371172575712));
#187822=CARTESIAN_POINT('Ctrl Pts',(16.8190563851715,18.3055262939003,11.6327947606345));
#187823=CARTESIAN_POINT('Ctrl Pts',(16.8510437238671,18.2407599735886,11.6284722636978));
#187824=CARTESIAN_POINT('Ctrl Pts',(16.8862405216007,18.1778137099316,11.6241497667611));
#187825=CARTESIAN_POINT('Ctrl Pts',(16.9214689659605,18.1148108491688,11.6198233833218));
#187826=CARTESIAN_POINT('Ctrl Pts',(16.9599123931251,18.0536317475416,11.6154969998825));
#187827=CARTESIAN_POINT('Ctrl Pts',(17.001342278154,17.994617568802,11.6111706164432));
#187828=CARTESIAN_POINT('Ctrl Pts',(17.042789639319,17.9355784964421,11.6068424080298));
#187829=CARTESIAN_POINT('Ctrl Pts',(17.0872256618387,17.8787065557693,11.6025141996164));
#187830=CARTESIAN_POINT('Ctrl Pts',(17.134380883397,17.8243105315903,11.5981859912031));
#187831=CARTESIAN_POINT('Ctrl Pts',(17.1816225942449,17.7698147374743,11.5938498442485));
#187832=CARTESIAN_POINT('Ctrl Pts',(17.231593123781,17.7178042891481,11.5895136972939));
#187833=CARTESIAN_POINT('Ctrl Pts',(17.283985843864,17.6685513146282,11.5851775503393));
#187834=CARTESIAN_POINT('Ctrl Pts',(17.333038486034,17.6224382567243,11.5811178362297));
#187835=CARTESIAN_POINT('Ctrl Pts',(17.3842137273592,17.5787421229118,11.5770581221201));
#187836=CARTESIAN_POINT('Ctrl Pts',(17.4372361998845,17.5376522636613,11.5729984080105));
#187837=CARTESIAN_POINT('Ctrl Pts',(17.494549025663,17.4932375875375,11.5686101990796));
#187838=CARTESIAN_POINT('Ctrl Pts',(17.5542581954977,17.4516841015565,11.5642219901487));
#187839=CARTESIAN_POINT('Ctrl Pts',(17.6160462231312,17.4132602099345,11.5598337812178));
#187840=CARTESIAN_POINT('Ctrl Pts',(17.677742547087,17.3748933457384,11.5554520851166));
#187841=CARTESIAN_POINT('Ctrl Pts',(17.7415111977163,17.3396471078963,11.5510703890153));
#187842=CARTESIAN_POINT('Ctrl Pts',(17.8070029012394,17.3077487346939,11.5466886929141));
#187843=CARTESIAN_POINT('Ctrl Pts',(17.872417646799,17.2758878446184,11.5423121456544));
#187844=CARTESIAN_POINT('Ctrl Pts',(17.9395509916038,17.2473672144278,11.5379355983948));
#187845=CARTESIAN_POINT('Ctrl Pts',(18.0080275301098,17.2223690707018,11.5335590511351));
#187846=CARTESIAN_POINT('Ctrl Pts',(18.0764606417902,17.1973867804352,11.5291852794182));
#187847=CARTESIAN_POINT('Ctrl Pts',(18.1462348050098,17.1759227092789,11.5248115077012));
#187848=CARTESIAN_POINT('Ctrl Pts',(18.2169543269185,17.158111115538,11.5204377359842));
#187849=CARTESIAN_POINT('Ctrl Pts',(18.2876523286392,17.1403049419248,11.5160652952207));
#187850=CARTESIAN_POINT('Ctrl Pts',(18.3592946504355,17.1261491568769,11.5116928544571));
#187851=CARTESIAN_POINT('Ctrl Pts',(18.4314717388384,17.1157277858955,11.5073204136936));
#187852=CARTESIAN_POINT('Ctrl Pts',(18.5036506728172,17.1053061484385,11.5029478611262));
#187853=CARTESIAN_POINT('Ctrl Pts',(18.5763639228386,17.0986191815878,11.4985753085589));
#187854=CARTESIAN_POINT('Ctrl Pts',(18.6491947479431,17.0956992957918,11.4942027559916));
#187855=CARTESIAN_POINT('Ctrl Pts',(18.722101159625,17.0927763796282,11.4898256654242));
#187856=CARTESIAN_POINT('Ctrl Pts',(18.7951249069972,17.0936283697016,11.4854485748569));
#187857=CARTESIAN_POINT('Ctrl Pts',(18.8678480060374,17.0982355286782,11.4810714842896));
#187858=CARTESIAN_POINT('Ctrl Pts',(18.9406108218611,17.1028452037952,11.4766920032306));
#187859=CARTESIAN_POINT('Ctrl Pts',(19.0130721829172,17.1112140756296,11.4723125221717));
#187860=CARTESIAN_POINT('Ctrl Pts',(19.0848207051458,17.1232706514395,11.4679330411128));
#187861=CARTESIAN_POINT('Ctrl Pts',(19.1566964011484,17.135348597449,11.4635457974531));
#187862=CARTESIAN_POINT('Ctrl Pts',(19.2278562638068,17.1511271959047,11.4591585537933));
#187863=CARTESIAN_POINT('Ctrl Pts',(19.297901126223,17.1704842515079,11.4547713101336));
#187864=CARTESIAN_POINT('Ctrl Pts',(19.3455248831594,17.1836451840766,11.4517884071988));
#187865=CARTESIAN_POINT('Ctrl Pts',(19.3926335158207,17.1984592758342,11.448805504264));
#187866=CARTESIAN_POINT('Ctrl Pts',(19.4391069833084,17.2148754692931,11.4458226013291));
#187867=CARTESIAN_POINT('Ctrl Pts',(19.5074750427239,17.2390256640267,11.4414343923982));
#187868=CARTESIAN_POINT('Ctrl Pts',(19.5747343896097,17.2667395128394,11.4370461834673));
#187869=CARTESIAN_POINT('Ctrl Pts',(19.6404874892065,17.2978953421435,11.4326579745364));
#187870=CARTESIAN_POINT('Ctrl Pts',(19.7061430003017,17.3290049310313,11.4282762784352));
#187871=CARTESIAN_POINT('Ctrl Pts',(19.7702962696066,17.3635461545568,11.4238945823339));
#187872=CARTESIAN_POINT('Ctrl Pts',(19.8325671704118,17.4013483285191,11.4195128862326));
#187873=CARTESIAN_POINT('Ctrl Pts',(19.8947648979526,17.4391060819186,11.415136338973));
#187874=CARTESIAN_POINT('Ctrl Pts',(19.9550842407136,17.4801169246317,11.4107597917133));
#187875=CARTESIAN_POINT('Ctrl Pts',(20.0131687750781,17.5241638357964,11.4063832444537));
#187876=CARTESIAN_POINT('Ctrl Pts',(20.0712164730752,17.5681828130502,11.4020094727367));
#187877=CARTESIAN_POINT('Ctrl Pts',(20.1270317913338,17.6152337476986,11.3976357010197));
#187878=CARTESIAN_POINT('Ctrl Pts',(20.1802876588314,17.6650565961485,11.3932619293028));
#187879=CARTESIAN_POINT('Ctrl Pts',(20.2335273203896,17.7148642833382,11.3888894885392));
#187880=CARTESIAN_POINT('Ctrl Pts',(20.2842087253976,17.7674418803648,11.3845170477756));
#187881=CARTESIAN_POINT('Ctrl Pts',(20.3320395381809,17.8224904989844,11.3801446070121));
#187882=CARTESIAN_POINT('Ctrl Pts',(20.3798715740033,17.8775405252032,11.3757720544448));
#187883=CARTESIAN_POINT('Ctrl Pts',(20.42485255801,17.935061333022,11.3713995018774));
#187884=CARTESIAN_POINT('Ctrl Pts',(20.4667296641656,17.9947200524055,11.3670269493101));
#187885=CARTESIAN_POINT('Ctrl Pts',(20.5086502319617,18.0544406878584,11.3626498587428));
#187886=CARTESIAN_POINT('Ctrl Pts',(20.5474602125879,18.1163032692072,11.3582727681754));
#187887=CARTESIAN_POINT('Ctrl Pts',(20.5829499551952,18.1799456545924,11.3538956776081));
#187888=CARTESIAN_POINT('Ctrl Pts',(20.618459080068,18.2436227974464,11.3495161965492));
#187889=CARTESIAN_POINT('Ctrl Pts',(20.6506441436593,18.3090812464314,11.3451367154902));
#187890=CARTESIAN_POINT('Ctrl Pts',(20.6793425856617,18.3759363949906,11.3407572344313));
#187891=CARTESIAN_POINT('Ctrl Pts',(20.7080918954598,18.442910043852,11.3363699907715));
#187892=CARTESIAN_POINT('Ctrl Pts',(20.7333420751794,18.5112848831346,11.3319827471118));
#187893=CARTESIAN_POINT('Ctrl Pts',(20.7549798102576,18.5806591346493,11.3275955034521));
#187894=CARTESIAN_POINT('Ctrl Pts',(20.7696913851037,18.6278269407924,11.3246126005173));
#187895=CARTESIAN_POINT('Ctrl Pts',(20.78273408769,18.6754564326547,11.3216296975824));
#187896=CARTESIAN_POINT('Ctrl Pts',(20.7940858734221,18.7234190383877,11.3186467946476));
#187897=CARTESIAN_POINT('Ctrl Pts',(20.8107857153611,18.7939777992408,11.3142585857167));
#187898=CARTESIAN_POINT('Ctrl Pts',(20.8238889631162,18.865533246677,11.3098703767858));
#187899=CARTESIAN_POINT('Ctrl Pts',(20.8332827468939,18.9376852572697,11.3054821678549));
#187900=CARTESIAN_POINT('Ctrl Pts',(20.8426625887389,19.0097301823156,11.3011004717537));
#187901=CARTESIAN_POINT('Ctrl Pts',(20.8483438339329,19.0823694384942,11.2967187756524));
#187902=CARTESIAN_POINT('Ctrl Pts',(20.8502642454991,19.1551910112784,11.2923370795511));
#187903=CARTESIAN_POINT('Ctrl Pts',(20.8521824004289,19.2279270129192,11.2879605322915));
#187904=CARTESIAN_POINT('Ctrl Pts',(20.8503484880034,19.3008444257667,11.2835839850318));
#187905=CARTESIAN_POINT('Ctrl Pts',(20.8447520630799,19.3735260846882,11.2792074377722));
#187906=CARTESIAN_POINT('Ctrl Pts',(20.8391591873277,19.4461616499579,11.2748336660552));
#187907=CARTESIAN_POINT('Ctrl Pts',(20.8298085704124,19.5185612781815,11.2704598943383));
#187908=CARTESIAN_POINT('Ctrl Pts',(20.8167418305018,19.5903091977241,11.2660861226213));
#187909=CARTESIAN_POINT('Ctrl Pts',(20.803679066844,19.6620352841338,11.2617136818577));
#187910=CARTESIAN_POINT('Ctrl Pts',(20.7869025116117,19.7331095812968,11.2573412410942));
#187911=CARTESIAN_POINT('Ctrl Pts',(20.7665052467619,19.8031244986364,11.2529688003306));
#187912=CARTESIAN_POINT('Ctrl Pts',(20.7461074603517,19.8731412062653,11.2485962477633));
#187913=CARTESIAN_POINT('Ctrl Pts',(20.7220889173522,19.9420980177239,11.244223695196));
#187914=CARTESIAN_POINT('Ctrl Pts',(20.6945926588476,20.0096021700903,11.2398511426286));
#187915=CARTESIAN_POINT('Ctrl Pts',(20.6670678636887,20.0771763808123,11.2354740520613));
#187916=CARTESIAN_POINT('Ctrl Pts',(20.6360583291635,20.1432944746739,11.231096961494));
#187917=CARTESIAN_POINT('Ctrl Pts',(20.6017550792375,20.2075841479687,11.2267198709267));
#187918=CARTESIAN_POINT('Ctrl Pts',(20.5674330950335,20.2719089322403,11.2223403898677));
#187919=CARTESIAN_POINT('Ctrl Pts',(20.5298140629451,20.3344028942418,11.2179609088088));
#187920=CARTESIAN_POINT('Ctrl Pts',(20.4891333854102,20.3947211662459,11.2135814277498));
#187921=CARTESIAN_POINT('Ctrl Pts',(20.4483806016475,20.4551463519821,11.2091941840901));
#187922=CARTESIAN_POINT('Ctrl Pts',(20.4045556257383,20.513387760871,11.2048069404304));
#187923=CARTESIAN_POINT('Ctrl Pts',(20.3579349545335,20.5691326383842,11.2004196967707));
#187924=CARTESIAN_POINT('Ctrl Pts',(20.3262373904715,20.6070337835293,11.1974367938359));
#187925=CARTESIAN_POINT('Ctrl Pts',(20.2932482928816,20.643781572932,11.194453890901));
#187926=CARTESIAN_POINT('Ctrl Pts',(20.2590638380205,20.6792878770739,11.1914709879662));
#187927=CARTESIAN_POINT('Ctrl Pts',(20.208774394013,20.7315219203344,11.1870827790353));
#187928=CARTESIAN_POINT('Ctrl Pts',(20.1557001261013,20.7812712846033,11.1826945701045));
#187929=CARTESIAN_POINT('Ctrl Pts',(20.1001163804878,20.8282244850246,11.1783063611736));
#187930=CARTESIAN_POINT('Ctrl Pts',(20.0446151303686,20.8751079991115,11.1739246650723));
#187931=CARTESIAN_POINT('Ctrl Pts',(19.9866121616041,20.9192032789,11.169542968971));
#187932=CARTESIAN_POINT('Ctrl Pts',(19.9264202255136,20.9602349772932,11.1651612728697));
#187933=CARTESIAN_POINT('Ctrl Pts',(19.8662990197384,21.0012184601753,11.1607847256101));
#187934=CARTESIAN_POINT('Ctrl Pts',(19.8039943529514,21.0391452426346,11.1564081783505));
#187935=CARTESIAN_POINT('Ctrl Pts',(19.7398513412539,21.0737807383849,11.1520316310908));
#187936=CARTESIAN_POINT('Ctrl Pts',(19.6757490081222,21.1083942688071,11.1476578593739));
#187937=CARTESIAN_POINT('Ctrl Pts',(19.609811066688,21.1397204253384,11.1432840876569));
#187938=CARTESIAN_POINT('Ctrl Pts',(19.5424096422239,21.1675691529715,11.1389103159399));
#187939=CARTESIAN_POINT('Ctrl Pts',(19.4750287282396,21.1954094061432,11.1345378751764));
#187940=CARTESIAN_POINT('Ctrl Pts',(19.4061856609221,21.2197741471639,11.1301654344128));
#187941=CARTESIAN_POINT('Ctrl Pts',(19.3362735429419,21.2405210221804,11.1257929936493));
#187942=CARTESIAN_POINT('Ctrl Pts',(19.2663596373011,21.2612684276968,11.1214204410819));
#187943=CARTESIAN_POINT('Ctrl Pts',(19.1953770897385,21.2783976482242,11.1170478885146));
#187944=CARTESIAN_POINT('Ctrl Pts',(19.1237335771413,21.2918163635575,11.1126753359473));
#187945=CARTESIAN_POINT('Ctrl Pts',(19.0520157102043,21.3052490053397,11.1082982453799));
#187946=CARTESIAN_POINT('Ctrl Pts',(18.9796359837857,21.3149633643477,11.1039211548126));
#187947=CARTESIAN_POINT('Ctrl Pts',(18.9070108440337,21.3209185405713,11.0995440642453));
#187948=CARTESIAN_POINT('Ctrl Pts',(18.8343460409976,21.3268769691377,11.0951645831863));
#187949=CARTESIAN_POINT('Ctrl Pts',(18.7614360402703,21.329072112832,11.0907851021274));
#187950=CARTESIAN_POINT('Ctrl Pts',(18.6886982399089,21.3275152374913,11.0864056210685));
#187951=CARTESIAN_POINT('Ctrl Pts',(18.6158315122846,21.3259556025994,11.0820183774087));
#187952=CARTESIAN_POINT('Ctrl Pts',(18.5431380760587,21.3206307033085,11.077631133749));
#187953=CARTESIAN_POINT('Ctrl Pts',(18.4710305707961,21.3116037416191,11.0732438900893));
#187954=CARTESIAN_POINT('Ctrl Pts',(18.42200441548,21.3054662775062,11.0702609871545));
#187955=CARTESIAN_POINT('Ctrl Pts',(18.3732489672181,21.2976185484977,11.0672780842196));
#187956=CARTESIAN_POINT('Ctrl Pts',(18.324890387372,21.2880937207684,11.0642951812848));
#187957=CARTESIAN_POINT('Ctrl Pts',(18.2537491009801,21.2740815537551,11.0599069723539));
#187958=CARTESIAN_POINT('Ctrl Pts',(18.1831896640501,21.2563828809338,11.055518763423));
#187959=CARTESIAN_POINT('Ctrl Pts',(18.1136230257294,21.2350606240414,11.0511305544921));
#187960=CARTESIAN_POINT('Ctrl Pts',(18.0441596358343,21.2137700129135,11.0467488583908));
#187961=CARTESIAN_POINT('Ctrl Pts',(17.9756865768824,21.1888666339678,11.0423671622896));
#187962=CARTESIAN_POINT('Ctrl Pts',(17.9086046585653,21.1604644214086,11.0379854661883));
#187963=CARTESIAN_POINT('Ctrl Pts',(17.8416015668409,21.1320955837095,11.0336089189286));
#187964=CARTESIAN_POINT('Ctrl Pts',(17.7759868104058,21.1002362668759,11.029232371669));
#187965=CARTESIAN_POINT('Ctrl Pts',(17.7121444440024,21.0650496818254,11.0248558244094));
#187966=CARTESIAN_POINT('Ctrl Pts',(17.6483425654999,21.0298854115958,11.0204820526924));
#187967=CARTESIAN_POINT('Ctrl Pts',(17.5863112682425,20.9913982921379,11.0161082809754));
#187968=CARTESIAN_POINT('Ctrl Pts',(17.5264117827665,20.9497983487451,11.0117345092584));
#187969=CARTESIAN_POINT('Ctrl Pts',(17.4665305249049,20.9082110643548,11.0073620684949));
#187970=CARTESIAN_POINT('Ctrl Pts',(17.4087801868834,20.863513111593,11.0029896277313));
#187971=CARTESIAN_POINT('Ctrl Pts',(17.3534932447841,20.8159579741549,10.9986171869678));
#187972=CARTESIAN_POINT('Ctrl Pts',(17.2982048889917,20.7684016207268,10.9942446344004));
#187973=CARTESIAN_POINT('Ctrl Pts',(17.245380418581,20.7179882536485,10.9898720818331));
#187974=CARTESIAN_POINT('Ctrl Pts',(17.1953181280013,20.6650106934898,10.9854995292658));
#187975=CARTESIAN_POINT('Ctrl Pts',(17.145203880888,20.6119781512208,10.9811224386984));
#187976=CARTESIAN_POINT('Ctrl Pts',(17.0978578691726,20.5563764539264,10.9767453481311));
#187977=CARTESIAN_POINT('Ctrl Pts',(17.0535398976926,20.4985336285134,10.9723682575638));
#187978=CARTESIAN_POINT('Ctrl Pts',(17.0091977225236,20.4406592129868,10.9679887765048));
#187979=CARTESIAN_POINT('Ctrl Pts',(16.9678871535196,20.3805416302804,10.9636092954459));
#187980=CARTESIAN_POINT('Ctrl Pts',(16.9298246475462,20.3185379440895,10.9592298143869));
#187981=CARTESIAN_POINT('Ctrl Pts',(16.8916946760364,20.256424356781,10.9548425707272));
#187982=CARTESIAN_POINT('Ctrl Pts',(16.8568244953674,20.1924184139091,10.9504553270675));
#187983=CARTESIAN_POINT('Ctrl Pts',(16.8253843166289,20.1269012900908,10.9460680834078));
#187984=CARTESIAN_POINT('Ctrl Pts',(16.8040080246552,20.0823559591094,10.943085180473));
#187985=CARTESIAN_POINT('Ctrl Pts',(16.7842163233974,20.0371125159699,10.9401022775382));
#187986=CARTESIAN_POINT('Ctrl Pts',(16.7660496141036,19.9912949946335,10.9371193746033));
#187987=CARTESIAN_POINT('Ctrl Pts',(16.7589277812078,19.9733333084868,10.9359499973704));
#187988=CARTESIAN_POINT('Ctrl Pts',(16.7520500861352,19.9552696214365,10.9347806201374));
#187989=CARTESIAN_POINT('Ctrl Pts',(16.7454193623258,19.9371102171621,10.9336112429045));
#187990=CARTESIAN_POINT('Ctrl Pts',(16.7460270442577,19.9368788012273,11.7337477294316));
#187991=CARTESIAN_POINT('Ctrl Pts',(16.6804602657827,19.7626326020608,11.7225565578517));
#187992=CARTESIAN_POINT('Ctrl Pts',(16.623583940577,19.5201104597515,11.7076594077154));
#187993=CARTESIAN_POINT('Ctrl Pts',(16.613796038846,19.2734660709366,11.692762257579));
#187994=CARTESIAN_POINT('Ctrl Pts',(16.6141771432254,19.2120774369074,11.6890562790225));
#187995=CARTESIAN_POINT('Origin',(18.734,19.211,0.));
#187996=CARTESIAN_POINT('',(16.745419226499,19.9371098451765,12.7565300941239));
#187997=CARTESIAN_POINT('',(16.7454193728684,19.937110246035,12.5316746173356));
#187998=CARTESIAN_POINT('',(16.7454193623258,19.9371102171621,0.));
#187999=CARTESIAN_POINT('',(16.6170000980014,19.2116441567485,12.7090269805744));
#188000=CARTESIAN_POINT('Ctrl Pts',(16.745419226499,19.9371098451765,12.7565300941239));
#188001=CARTESIAN_POINT('Ctrl Pts',(16.7109718279897,19.8427695262457,12.7499960896148));
#188002=CARTESIAN_POINT('Ctrl Pts',(16.6832543081821,19.7460230012717,12.7433224418381));
#188003=CARTESIAN_POINT('Ctrl Pts',(16.6461765008723,19.5701016041718,12.7314741686189));
#188004=CARTESIAN_POINT('Ctrl Pts',(16.6342037280546,19.4917464784093,12.7262975863649));
#188005=CARTESIAN_POINT('Ctrl Pts',(16.6241532252603,19.386842951453,12.7196400353508));
#188006=CARTESIAN_POINT('Ctrl Pts',(16.6221401933133,19.3607413040614,12.718006033714));
#188007=CARTESIAN_POINT('Ctrl Pts',(16.6202046974363,19.3276490764454,12.7159684458409));
#188008=CARTESIAN_POINT('Ctrl Pts',(16.6198320659138,19.3206883666375,12.7155417585203));
#188009=CARTESIAN_POINT('Ctrl Pts',(16.6192953232568,19.3096400680818,12.7148676617419));
#188010=CARTESIAN_POINT('Ctrl Pts',(16.6191086713618,19.3055536967893,12.7146190224069));
#188011=CARTESIAN_POINT('Ctrl Pts',(16.6187836658417,19.2979552364133,12.7141579923509));
#188012=CARTESIAN_POINT('Ctrl Pts',(16.6186422157249,19.2944433828792,12.713945435868));
#188013=CARTESIAN_POINT('Ctrl Pts',(16.6183781730345,19.2874551180024,12.713523492419));
#188014=CARTESIAN_POINT('Ctrl Pts',(16.6182554032475,19.2839787743982,12.7133140970092));
#188015=CARTESIAN_POINT('Ctrl Pts',(16.6179937470186,19.2760131516113,12.7128354112316));
#188016=CARTESIAN_POINT('Ctrl Pts',(16.6178605771198,19.271523683795,12.7125664352002));
#188017=CARTESIAN_POINT('Ctrl Pts',(16.6175253046709,19.258861266542,12.7118100059682));
#188018=CARTESIAN_POINT('Ctrl Pts',(16.6173562534074,19.2506874230827,12.7113243118677));
#188019=CARTESIAN_POINT('Ctrl Pts',(16.6170813858816,19.2322240481652,12.7102326610896));
#188020=CARTESIAN_POINT('Ctrl Pts',(16.6170032290586,19.2219342728014,12.7096280997442));
#188021=CARTESIAN_POINT('Ctrl Pts',(16.6170000980014,19.2116441567485,12.7090269805744));
#188022=CARTESIAN_POINT('Ctrl Pts',(16.6170000985846,19.211646070454,12.7090270923677));
#188023=CARTESIAN_POINT('Ctrl Pts',(16.6169387604032,19.0106572727102,12.6972858928636));
#188024=CARTESIAN_POINT('Ctrl Pts',(16.6454993147949,18.8106400257173,12.6868416498719));
#188025=CARTESIAN_POINT('Ctrl Pts',(16.7265384440085,18.5331076467323,12.670879152307));
#188026=CARTESIAN_POINT('Ctrl Pts',(16.756460397437,18.4502276826733,12.6659226579821));
#188027=CARTESIAN_POINT('Ctrl Pts',(16.7995990705701,18.3506500116555,12.659597648559));
#188028=CARTESIAN_POINT('Ctrl Pts',(16.8080187647746,18.33196342723,12.6583942839193));
#188029=CARTESIAN_POINT('Ctrl Pts',(16.8204632172919,18.305381750612,12.6566576096086));
#188030=CARTESIAN_POINT('Ctrl Pts',(16.8242684544766,18.2973847348022,12.6561318718541));
#188031=CARTESIAN_POINT('Ctrl Pts',(16.8309529273847,18.2835610117046,12.6552172998102));
#188032=CARTESIAN_POINT('Ctrl Pts',(16.8338090432712,18.2777232114141,12.6548292737635));
#188033=CARTESIAN_POINT('Ctrl Pts',(16.8393529180669,18.266522675095,12.6540812910053));
#188034=CARTESIAN_POINT('Ctrl Pts',(16.8420366812202,18.2611580228387,12.6537214770087));
#188035=CARTESIAN_POINT('Ctrl Pts',(16.8491284285195,18.2471314310087,12.652776568871));
#188036=CARTESIAN_POINT('Ctrl Pts',(16.8535732884557,18.2384883872946,12.6521901818696));
#188037=CARTESIAN_POINT('Ctrl Pts',(16.8692136681454,18.2085837554897,12.6501466771834));
#188038=CARTESIAN_POINT('Ctrl Pts',(16.8807112218679,18.1874830138528,12.6486789112992));
#188039=CARTESIAN_POINT('Ctrl Pts',(16.9645641503801,18.0396400157092,12.6382064943479));
#188040=CARTESIAN_POINT('Ctrl Pts',(17.0494840526099,17.9205041437133,12.6287343676895));
#188041=CARTESIAN_POINT('Ctrl Pts',(17.2364708926923,17.708392449996,12.6100727414369));
#188042=CARTESIAN_POINT('Ctrl Pts',(17.336731979102,17.6147323021957,12.6009553692923));
#188043=CARTESIAN_POINT('Ctrl Pts',(17.4554189558392,17.5236704857472,12.5915872424048));
#188044=CARTESIAN_POINT('Ctrl Pts',(17.4655673061445,17.5160283500168,12.5907967765417));
#188045=CARTESIAN_POINT('Ctrl Pts',(17.4812019684215,17.5044738568522,12.5895957983659));
#188046=CARTESIAN_POINT('Ctrl Pts',(17.4866390061365,17.5004957062644,12.5891812225684));
#188047=CARTESIAN_POINT('Ctrl Pts',(17.4956289991096,17.4939836033656,12.5885009017715));
#188048=CARTESIAN_POINT('Ctrl Pts',(17.4991709183665,17.4914345949975,12.5882341773707));
#188049=CARTESIAN_POINT('Ctrl Pts',(17.5060326408267,17.4865285618955,12.5877200253526));
#188050=CARTESIAN_POINT('Ctrl Pts',(17.5093514085005,17.4841701288151,12.5874725034557));
#188051=CARTESIAN_POINT('Ctrl Pts',(17.5126866850503,17.4818144151458,12.5872249234406));
#188052=CARTESIAN_POINT('Ctrl Pts',(17.5126963787218,17.481807568605,12.5872242038822));
#188053=CARTESIAN_POINT('Ctrl Pts',(17.5127158007082,17.4817938512999,12.5872227622137));
#188054=CARTESIAN_POINT('Ctrl Pts',(17.5127255285653,17.4817869808599,12.5872220401377));
#188055=CARTESIAN_POINT('Ctrl Pts',(17.5127450188822,17.4817732157876,12.5872205934371));
#188056=CARTESIAN_POINT('Ctrl Pts',(17.5127547816535,17.4817663209362,12.5872198687896));
#188057=CARTESIAN_POINT('Ctrl Pts',(17.5127749744187,17.481752060271,12.5872183699903));
#188058=CARTESIAN_POINT('Ctrl Pts',(17.5127854044269,17.4817446944647,12.5872175958389));
#188059=CARTESIAN_POINT('Ctrl Pts',(17.5128064327553,17.4817298442729,12.5872160350666));
#188060=CARTESIAN_POINT('Ctrl Pts',(17.5128170307833,17.4817223600985,12.5872152484677));
#188061=CARTESIAN_POINT('Ctrl Pts',(17.5128383984912,17.4817072708259,12.5872136625536));
#188062=CARTESIAN_POINT('Ctrl Pts',(17.5128491683808,17.4816996655845,12.5872128632233));
#188063=CARTESIAN_POINT('Ctrl Pts',(17.5128708834199,17.4816843316445,12.5872112515796));
#188064=CARTESIAN_POINT('Ctrl Pts',(17.5128818286274,17.4816766029099,12.5872104392624));
#188065=CARTESIAN_POINT('Ctrl Pts',(17.5129038985387,17.4816610190072,12.5872088013319));
#188066=CARTESIAN_POINT('Ctrl Pts',(17.5129150226881,17.4816531642355,12.5872079757601));
#188067=CARTESIAN_POINT('Ctrl Pts',(17.51293745395,17.4816373258262,12.5872063110645));
#188068=CARTESIAN_POINT('Ctrl Pts',(17.5129487614422,17.4816293419258,12.5872054719128));
#188069=CARTESIAN_POINT('Ctrl Pts',(17.5129715632085,17.4816132425786,12.5872037797753));
#188070=CARTESIAN_POINT('Ctrl Pts',(17.5129830576609,17.4816051270115,12.5872029267766));
#188071=CARTESIAN_POINT('Ctrl Pts',(17.51300623779,17.4815887612113,12.5872012066167));
#188072=CARTESIAN_POINT('Ctrl Pts',(17.5130179232493,17.4815805111373,12.587200339472));
#188073=CARTESIAN_POINT('Ctrl Pts',(17.5130414893778,17.4815638735268,12.5871985907259));
#188074=CARTESIAN_POINT('Ctrl Pts',(17.5130533703946,17.4815554857508,12.587197709099));
#188075=CARTESIAN_POINT('Ctrl Pts',(17.513077332228,17.4815385695139,12.5871959310493));
#188076=CARTESIAN_POINT('Ctrl Pts',(17.5130894127562,17.4815300412627,12.5871950346484));
#188077=CARTESIAN_POINT('Ctrl Pts',(17.5131137781087,17.4815128409201,12.5871932267183));
#188078=CARTESIAN_POINT('Ctrl Pts',(17.5131260629415,17.4815041688291,12.5871923151891));
#188079=CARTESIAN_POINT('Ctrl Pts',(17.5131508412232,17.4814866777767,12.5871904766836));
#188080=CARTESIAN_POINT('Ctrl Pts',(17.5131633349751,17.4814778586081,12.5871895496854));
#188081=CARTESIAN_POINT('Ctrl Pts',(17.5131885363069,17.4814600697418,12.5871876798568));
#188082=CARTESIAN_POINT('Ctrl Pts',(17.5132012433539,17.4814511004273,12.5871867370666));
#188083=CARTESIAN_POINT('Ctrl Pts',(17.5132268759753,17.481433007973,12.5871848353069));
#188084=CARTESIAN_POINT('Ctrl Pts',(17.5132398017299,17.4814238847134,12.5871838763248));
#188085=CARTESIAN_POINT('Ctrl Pts',(17.5132658766755,17.4814054809262,12.587181941819));
#188086=CARTESIAN_POINT('Ctrl Pts',(17.5132790258933,17.4813962003872,12.587180966294));
#188087=CARTESIAN_POINT('Ctrl Pts',(17.5161295888974,17.4793843605113,12.5869694903282));
#188088=CARTESIAN_POINT('Ctrl Pts',(17.5189718855124,17.4773888145413,12.5867594811754));
#188089=CARTESIAN_POINT('Ctrl Pts',(17.5255910720128,17.4727658298507,12.5862723713935));
#188090=CARTESIAN_POINT('Ctrl Pts',(17.5293716209543,17.4701437058654,12.5859956347871));
#188091=CARTESIAN_POINT('Ctrl Pts',(17.5410660208189,17.4620890068941,12.5851440493046));
#188092=CARTESIAN_POINT('Ctrl Pts',(17.549008422291,17.4566978284536,12.5845719401235));
#188093=CARTESIAN_POINT('Ctrl Pts',(17.6515087940936,17.3881359171802,12.5772648276371));
#188094=CARTESIAN_POINT('Ctrl Pts',(17.7509851461404,17.3326204316007,12.5709971427924));
#188095=CARTESIAN_POINT('Ctrl Pts',(17.9581449953138,17.2379989222324,12.5585849310954));
#188096=CARTESIAN_POINT('Ctrl Pts',(18.0654897152336,17.199091093247,12.5524565708601));
#188097=CARTESIAN_POINT('Ctrl Pts',(18.2285727248127,17.1544820277548,12.5430552207825));
#188098=CARTESIAN_POINT('Ctrl Pts',(18.2822455064783,17.1420292090627,12.5399492838202));
#188099=CARTESIAN_POINT('Ctrl Pts',(18.3700241107728,17.1252419459907,12.5348076541231));
#188100=CARTESIAN_POINT('Ctrl Pts',(18.4038581131141,17.119619774897,12.5328113012355));
#188101=CARTESIAN_POINT('Ctrl Pts',(18.4485134975469,17.1133100189139,12.5301515219491));
#188102=CARTESIAN_POINT('Ctrl Pts',(18.4592258646563,17.1118799539278,12.5295116042883));
#188103=CARTESIAN_POINT('Ctrl Pts',(18.4767925395974,17.1096716338146,12.528459006155));
#188104=CARTESIAN_POINT('Ctrl Pts',(18.4836406159394,17.1088447352054,12.5280478663419));
#188105=CARTESIAN_POINT('Ctrl Pts',(18.4969066602564,17.1073086156269,12.5272498089319));
#188106=CARTESIAN_POINT('Ctrl Pts',(18.5033240794254,17.1065952597776,12.5268630265715));
#188107=CARTESIAN_POINT('Ctrl Pts',(18.5181525792627,17.1050155776359,12.5259675885405));
#188108=CARTESIAN_POINT('Ctrl Pts',(18.526565745182,17.1041702672102,12.5254582764669));
#188109=CARTESIAN_POINT('Ctrl Pts',(18.54921315962,17.1020317432914,12.5240837390301));
#188110=CARTESIAN_POINT('Ctrl Pts',(18.563455623542,17.1008322616166,12.523215584082));
#188111=CARTESIAN_POINT('Ctrl Pts',(18.6944563158825,17.091134448096,12.5151947707832));
#188112=CARTESIAN_POINT('Ctrl Pts',(18.8117001618678,17.0921917270833,12.5077391494698));
#188113=CARTESIAN_POINT('Ctrl Pts',(19.0909641228782,17.1179234122904,12.4894190486677));
#188114=CARTESIAN_POINT('Ctrl Pts',(19.2514009456122,17.1517065704701,12.4784127146827));
#188115=CARTESIAN_POINT('Ctrl Pts',(19.4364131370526,17.2136743690216,12.466024206083));
#188116=CARTESIAN_POINT('Ctrl Pts',(19.466243901464,17.2244167497298,12.4640385147701));
#188117=CARTESIAN_POINT('Ctrl Pts',(19.5025262506239,17.2384108369186,12.4616474974234));
#188118=CARTESIAN_POINT('Ctrl Pts',(19.5092155104863,17.241030071317,12.4612076935512));
#188119=CARTESIAN_POINT('Ctrl Pts',(19.5196990585668,17.2451966584612,12.4605201762969));
#188120=CARTESIAN_POINT('Ctrl Pts',(19.523502335295,17.2467210352245,12.4602711189686));
#188121=CARTESIAN_POINT('Ctrl Pts',(19.530614520113,17.2495956363273,12.4598060927066));
#188122=CARTESIAN_POINT('Ctrl Pts',(19.5339243974569,17.2509431819302,12.4595899729136));
#188123=CARTESIAN_POINT('Ctrl Pts',(19.5414871061499,17.2540445240389,12.4590968198226));
#188124=CARTESIAN_POINT('Ctrl Pts',(19.545737635987,17.2558038019854,12.4588201220291));
#188125=CARTESIAN_POINT('Ctrl Pts',(19.5588366369341,17.2612755070236,12.4579687748242));
#188126=CARTESIAN_POINT('Ctrl Pts',(19.5676657700213,17.2650343096884,12.4573968628904));
#188127=CARTESIAN_POINT('Ctrl Pts',(19.6520261986637,17.3016283824231,12.4519480306099));
#188128=CARTESIAN_POINT('Ctrl Pts',(19.7256155647243,17.3387890425237,12.4473145497081));
#188129=CARTESIAN_POINT('Ctrl Pts',(19.9204061040629,17.4518702878759,12.434893169299));
#188130=CARTESIAN_POINT('Ctrl Pts',(20.0363750951913,17.5359127117115,12.4272971835306));
#188131=CARTESIAN_POINT('Ctrl Pts',(20.2010418772366,17.6827573998835,12.4150448484645));
#188132=CARTESIAN_POINT('Ctrl Pts',(20.2561837109088,17.7376730856162,12.4106413581722));
#188133=CARTESIAN_POINT('Ctrl Pts',(20.3209966749389,17.8097512020768,12.4049837749805));
#188134=CARTESIAN_POINT('Ctrl Pts',(20.3336224808072,17.8241818709403,12.4038569177371));
#188135=CARTESIAN_POINT('Ctrl Pts',(20.3516384812304,17.8453466504768,12.4022115767129));
#188136=CARTESIAN_POINT('Ctrl Pts',(20.3571865105103,17.8519455949942,12.4016995951999));
#188137=CARTESIAN_POINT('Ctrl Pts',(20.3668207842451,17.8635479542822,12.4008011007121));
#188138=CARTESIAN_POINT('Ctrl Pts',(20.3709247486381,17.8685365573542,12.400415316153));
#188139=CARTESIAN_POINT('Ctrl Pts',(20.3788333443386,17.8782400911947,12.399665907595));
#188140=CARTESIAN_POINT('Ctrl Pts',(20.3826406981208,17.8829527295762,12.3993023989869));
#188141=CARTESIAN_POINT('Ctrl Pts',(20.3916688730864,17.8942262120945,12.3984338560035));
#188142=CARTESIAN_POINT('Ctrl Pts',(20.3968710193114,17.9008018198436,12.3979280801225));
#188143=CARTESIAN_POINT('Ctrl Pts',(20.4153602060731,17.9244599831696,12.3961111953677));
#188144=CARTESIAN_POINT('Ctrl Pts',(20.42842383789,17.9417147048461,12.3947913005092));
#188145=CARTESIAN_POINT('Ctrl Pts',(20.5535656086143,18.1123799843618,12.3817826321626));
#188146=CARTESIAN_POINT('Ctrl Pts',(20.6447543120481,18.2799933909853,12.3692503567173));
#188147=CARTESIAN_POINT('Ctrl Pts',(20.7398679353733,18.529708054316,12.3516166715367));
#188148=CARTESIAN_POINT('Ctrl Pts',(20.763408153841,18.6034071612342,12.3465444579389));
#188149=CARTESIAN_POINT('Ctrl Pts',(20.7917370738072,18.7123518968674,12.3393736389055));
#188150=CARTESIAN_POINT('Ctrl Pts',(20.7997559561205,18.7466892608215,12.3371599363058));
#188151=CARTESIAN_POINT('Ctrl Pts',(20.8084200500398,18.7884772292334,12.3345346319601));
#188152=CARTESIAN_POINT('Ctrl Pts',(20.8098879861357,18.7957493424596,12.3340802687922));
#188153=CARTESIAN_POINT('Ctrl Pts',(20.8121172312758,18.8071002767284,12.333375119713));
#188154=CARTESIAN_POINT('Ctrl Pts',(20.8129048118116,18.8111737908877,12.3331228760275));
#188155=CARTESIAN_POINT('Ctrl Pts',(20.814347221162,18.818753696663,12.3326550522728));
#188156=CARTESIAN_POINT('Ctrl Pts',(20.815005157165,18.8222593934293,12.3324393022404));
#188157=CARTESIAN_POINT('Ctrl Pts',(20.8164775991352,18.8302159122948,12.331951023367));
#188158=CARTESIAN_POINT('Ctrl Pts',(20.8172866964435,18.8346676819031,12.3316788046212));
#188159=CARTESIAN_POINT('Ctrl Pts',(20.8193431868608,18.8461926830013,12.3309765214122));
#188160=CARTESIAN_POINT('Ctrl Pts',(20.8205688797905,18.8532697961615,12.3305476600726));
#188161=CARTESIAN_POINT('Ctrl Pts',(20.8279613566092,18.8972847517752,12.3278944811131));
#188162=CARTESIAN_POINT('Ctrl Pts',(20.833183542551,18.9343770429387,12.3257200014894));
#188163=CARTESIAN_POINT('Ctrl Pts',(20.8565548960087,19.1397148363527,12.3139241909942));
#188164=CARTESIAN_POINT('Ctrl Pts',(20.8554669831909,19.3095411506274,12.3050166702248));
#188165=CARTESIAN_POINT('Ctrl Pts',(20.8221149301088,19.5724334827263,12.2904420727788));
#188166=CARTESIAN_POINT('Ctrl Pts',(20.803633726641,19.6664901328602,12.2850742117915));
#188167=CARTESIAN_POINT('Ctrl Pts',(20.7733042873709,19.7796707885036,12.278251486055));
#188168=CARTESIAN_POINT('Ctrl Pts',(20.7674421653872,19.8002888532445,12.276993800894));
#188169=CARTESIAN_POINT('Ctrl Pts',(20.7586707222561,19.8294486834147,12.2751925776329));
#188170=CARTESIAN_POINT('Ctrl Pts',(20.7560181930505,19.8380667673546,12.2746574199199));
#188171=CARTESIAN_POINT('Ctrl Pts',(20.7513506443056,19.8528940639882,12.2737317254693));
#188172=CARTESIAN_POINT('Ctrl Pts',(20.7493617991531,19.8591114321674,12.2733420524814));
#188173=CARTESIAN_POINT('Ctrl Pts',(20.7455011060697,19.8709908042675,12.2725945775596));
#188174=CARTESIAN_POINT('Ctrl Pts',(20.7436340245679,19.8766543003732,12.2722369359772));
#188175=CARTESIAN_POINT('Ctrl Pts',(20.7387220829723,19.8913448602326,12.2713058751967));
#188176=CARTESIAN_POINT('Ctrl Pts',(20.7356401979983,19.9003593198896,12.2707312357628));
#188177=CARTESIAN_POINT('Ctrl Pts',(20.7249522999965,19.9309452158217,12.2687700074478));
#188178=CARTESIAN_POINT('Ctrl Pts',(20.7170577833659,19.9524134730854,12.2673738818407));
#188179=CARTESIAN_POINT('Ctrl Pts',(20.6450122292029,20.1389450934458,12.255067323928));
#188180=CARTESIAN_POINT('Ctrl Pts',(20.5607424089589,20.2954528318668,12.2434385931731));
#188181=CARTESIAN_POINT('Ctrl Pts',(20.4274581620335,20.4824791282448,12.2282659895484));
#188182=CARTESIAN_POINT('Ctrl Pts',(20.3953206283761,20.5241922149986,12.2247947652309));
#188183=CARTESIAN_POINT('Ctrl Pts',(20.3176601832236,20.6175719432667,12.2168801295183));
#188184=CARTESIAN_POINT('Ctrl Pts',(20.2711010346898,20.6683080114399,12.212469773892));
#188185=CARTESIAN_POINT('Ctrl Pts',(20.2159399040907,20.7228264833275,12.2076863885666));
#188186=CARTESIAN_POINT('Ctrl Pts',(20.2096935108621,20.7289241954265,12.2071507375361));
#188187=CARTESIAN_POINT('Ctrl Pts',(20.2002227526364,20.7380558062979,12.2063478490094));
#188188=CARTESIAN_POINT('Ctrl Pts',(20.1970263842658,20.7411184253721,12.2060784464144));
#188189=CARTESIAN_POINT('Ctrl Pts',(20.1912657085946,20.7466034963174,12.2055957683517));
#188190=CARTESIAN_POINT('Ctrl Pts',(20.1887049480794,20.7490295699078,12.2053822146375));
#188191=CARTESIAN_POINT('Ctrl Pts',(20.1830738246341,20.754337871076,12.2049148182156));
#188192=CARTESIAN_POINT('Ctrl Pts',(20.1800009316714,20.7572173326706,12.2046611874514));
#188193=CARTESIAN_POINT('Ctrl Pts',(20.1714356858358,20.7651955512158,12.2039581134963));
#188194=CARTESIAN_POINT('Ctrl Pts',(20.1659247580008,20.7702743997007,12.2035101659433));
#188195=CARTESIAN_POINT('Ctrl Pts',(20.1366555825276,20.7969627129844,12.2011535421934));
#188196=CARTESIAN_POINT('Ctrl Pts',(20.1124334934574,20.8180599756423,12.1992809939189));
#188197=CARTESIAN_POINT('Ctrl Pts',(20.0728030321974,20.8510222149184,12.196321899611));
#188198=CARTESIAN_POINT('Ctrl Pts',(20.0576960547959,20.8632394564732,12.1952173029466));
#188199=CARTESIAN_POINT('Ctrl Pts',(20.0412884782937,20.8761390079734,12.1940399061242));
#188200=CARTESIAN_POINT('Ctrl Pts',(20.0401534162749,20.8770295119004,12.1939585680488));
#188201=CARTESIAN_POINT('Ctrl Pts',(20.0209795414295,20.8920405851875,12.1925864693753));
#188202=CARTESIAN_POINT('Ctrl Pts',(20.0027131474509,20.9058689599033,12.1913075600736));
#188203=CARTESIAN_POINT('Ctrl Pts',(19.9473641170615,20.9463740112137,12.1875044861132));
#188204=CARTESIAN_POINT('Ctrl Pts',(19.9096382839208,20.9721502778281,12.1850068003114));
#188205=CARTESIAN_POINT('Ctrl Pts',(19.7788706621966,21.055421779044,12.1765663179));
#188206=CARTESIAN_POINT('Ctrl Pts',(19.6822228710713,21.1069216499718,12.1706782218446));
#188207=CARTESIAN_POINT('Ctrl Pts',(19.5315382636709,21.1727999012095,12.161533872076));
#188208=CARTESIAN_POINT('Ctrl Pts',(19.4802032684083,21.1928945913558,12.1584263479471));
#188209=CARTESIAN_POINT('Ctrl Pts',(19.3957343138344,21.2222120018684,12.1532823251587));
#188210=CARTESIAN_POINT('Ctrl Pts',(19.3630560968352,21.2326711525379,12.1512852143881));
#188211=CARTESIAN_POINT('Ctrl Pts',(19.319767956074,21.2453750230576,12.1486245684813));
#188212=CARTESIAN_POINT('Ctrl Pts',(19.3093734290834,21.248339255831,12.1479845616418));
#188213=CARTESIAN_POINT('Ctrl Pts',(19.2923087977329,21.2530646099514,12.1469318541869));
#188214=CARTESIAN_POINT('Ctrl Pts',(19.2856518975241,21.2548729821268,12.1465206948594));
#188215=CARTESIAN_POINT('Ctrl Pts',(19.2727471256471,21.2583109742531,12.1457226262795));
#188216=CARTESIAN_POINT('Ctrl Pts',(19.2665003959816,21.2599446106562,12.1453358524049));
#188217=CARTESIAN_POINT('Ctrl Pts',(19.2520570055273,21.2636513150955,12.1444404729316));
#188218=CARTESIAN_POINT('Ctrl Pts',(19.2438552450985,21.2657038979243,12.1439312112001));
#188219=CARTESIAN_POINT('Ctrl Pts',(19.221758525465,21.2710934016981,12.1425568977084));
#188220=CARTESIAN_POINT('Ctrl Pts',(19.2078418965947,21.2743388098415,12.141688917848));
#188221=CARTESIAN_POINT('Ctrl Pts',(19.0798347076321,21.3028272338778,12.133681578609));
#188222=CARTESIAN_POINT('Ctrl Pts',(18.9638887178433,21.3187206151964,12.1262404356165));
#188223=CARTESIAN_POINT('Ctrl Pts',(18.6847502786384,21.3336733314719,12.1079811189833));
#188224=CARTESIAN_POINT('Ctrl Pts',(18.521803430621,21.3236145640143,12.0970228908445));
#188225=CARTESIAN_POINT('Ctrl Pts',(18.3296151316165,21.2892730227673,12.0846173735738));
#188226=CARTESIAN_POINT('Ctrl Pts',(18.2977462306467,21.2828177517052,12.0825798088158));
#188227=CARTESIAN_POINT('Ctrl Pts',(18.2589760858404,21.2740302215162,12.080135252125));
#188228=CARTESIAN_POINT('Ctrl Pts',(18.2519235718755,21.272393638985,12.0796919708425));
#188229=CARTESIAN_POINT('Ctrl Pts',(18.240880971458,21.2697713601372,12.0790002393744));
#188230=CARTESIAN_POINT('Ctrl Pts',(18.2368852009058,21.2688101872662,12.0787504184084));
#188231=CARTESIAN_POINT('Ctrl Pts',(18.2294218428266,21.2669918875424,12.0782847345719));
#188232=CARTESIAN_POINT('Ctrl Pts',(18.2259536637447,21.266137630132,12.0780687162314));
#188233=CARTESIAN_POINT('Ctrl Pts',(18.2180420293894,21.2641676407031,12.0775767898743));
#188234=CARTESIAN_POINT('Ctrl Pts',(18.2136000320197,21.2630462622705,12.0773012110212));
#188235=CARTESIAN_POINT('Ctrl Pts',(18.1999589566366,21.2595554422334,12.0764567167957));
#188236=CARTESIAN_POINT('Ctrl Pts',(18.1907720122815,21.2571384598475,12.075890475519));
#188237=CARTESIAN_POINT('Ctrl Pts',(18.1084484488737,21.2348865079895,12.0708364030099));
#188238=CARTESIAN_POINT('Ctrl Pts',(18.0364012526074,21.2111974708642,12.0665543442511));
#188239=CARTESIAN_POINT('Ctrl Pts',(17.9259496547316,21.1681842046639,12.0599935529638));
#188240=CARTESIAN_POINT('Ctrl Pts',(17.8866044167707,21.1514732111642,12.0576573773012));
#188241=CARTESIAN_POINT('Ctrl Pts',(17.7485094048649,21.0878187045986,12.0493787556857));
#188242=CARTESIAN_POINT('Ctrl Pts',(17.6529227037613,21.0344338912099,12.0434920554354));
#188243=CARTESIAN_POINT('Ctrl Pts',(17.516026117633,20.9434150677657,12.0343509506364));
#188244=CARTESIAN_POINT('Ctrl Pts',(17.4713725721059,20.9111451935431,12.0312452864231));
#188245=CARTESIAN_POINT('Ctrl Pts',(17.4010406358429,20.856018019602,12.0261040679831));
#188246=CARTESIAN_POINT('Ctrl Pts',(17.3745704123617,20.8342116162799,12.0241078453512));
#188247=CARTESIAN_POINT('Ctrl Pts',(17.3404706856775,20.8047006758762,12.0214482150112));
#188248=CARTESIAN_POINT('Ctrl Pts',(17.3323532455072,20.7975661546967,12.0208083126805));
#188249=CARTESIAN_POINT('Ctrl Pts',(17.3191448670055,20.7857766610118,12.0197557333397));
#188250=CARTESIAN_POINT('Ctrl Pts',(17.3140213609048,20.7811583494063,12.019344596881));
#188251=CARTESIAN_POINT('Ctrl Pts',(17.3041456373962,20.7721685349377,12.0185465413904));
#188252=CARTESIAN_POINT('Ctrl Pts',(17.2993906644874,20.767800162437,12.0181597575704));
#188253=CARTESIAN_POINT('Ctrl Pts',(17.288455178468,20.7576611353554,12.0172643094692));
#188254=CARTESIAN_POINT('Ctrl Pts',(17.2822891367916,20.7518750971701,12.0167549887386));
#188255=CARTESIAN_POINT('Ctrl Pts',(17.2657938223441,20.7362094669447,12.0153804127899));
#188256=CARTESIAN_POINT('Ctrl Pts',(17.2555298070371,20.7262620799574,12.0145122277316));
#188257=CARTESIAN_POINT('Ctrl Pts',(17.1621046131226,20.6338659212449,12.0064890650655));
#188258=CARTESIAN_POINT('Ctrl Pts',(17.0858314394438,20.5447672500487,11.9990309185508));
#188259=CARTESIAN_POINT('Ctrl Pts',(16.9216222700977,20.3172193719957,11.9806998283651));
#188260=CARTESIAN_POINT('Ctrl Pts',(16.8416122554602,20.1739658140329,11.9696846896713));
#188261=CARTESIAN_POINT('Ctrl Pts',(16.7671124243987,19.9945720871467,11.9573528861249));
#188262=CARTESIAN_POINT('Ctrl Pts',(16.7559529381101,19.9659582685393,11.9554288650358));
#188263=CARTESIAN_POINT('Ctrl Pts',(16.7454193623241,19.9371102171575,11.9535387334123));
#188264=CARTESIAN_POINT('',(16.6163526568764,19.2091064841458,12.4890562790225));
#188265=CARTESIAN_POINT('Ctrl Pts',(16.6163526568764,19.2091064841458,12.4890562790225));
#188266=CARTESIAN_POINT('Ctrl Pts',(16.6150299493055,19.0661177741218,12.4804472042752));
#188267=CARTESIAN_POINT('Ctrl Pts',(16.6934796238476,18.2204816490939,12.4294461939675));
#188268=CARTESIAN_POINT('Ctrl Pts',(17.8308508880792,16.8763369760823,12.336053248099));
#188269=CARTESIAN_POINT('Ctrl Pts',(20.2082246499765,17.1878857088602,12.2088774414178));
#188270=CARTESIAN_POINT('Ctrl Pts',(21.2330887962208,19.3555162351247,12.0817016347362));
#188271=CARTESIAN_POINT('Ctrl Pts',(19.9651940828767,21.3905620853514,11.9545258280549));
#188272=CARTESIAN_POINT('Ctrl Pts',(17.7787241911337,21.4228769879768,11.8385411929533));
#188273=CARTESIAN_POINT('Ctrl Pts',(16.9288259197432,20.4226737419889,11.7649484934122));
#188274=CARTESIAN_POINT('Ctrl Pts',(16.7460270442577,19.9368788012273,11.7337477294316));
#188275=CARTESIAN_POINT('Ctrl Pts',(16.6170008641598,19.2090871874988,12.489429316251));
#188276=CARTESIAN_POINT('Ctrl Pts',(16.6168618955398,19.3628902644884,12.4977918761832));
#188277=CARTESIAN_POINT('Ctrl Pts',(16.633483105635,19.5162417805676,12.5060812887087));
#188278=CARTESIAN_POINT('Ctrl Pts',(16.6718147732515,19.6902443673696,12.5163103612939));
#188279=CARTESIAN_POINT('Ctrl Pts',(16.6774689198822,19.7139541935533,12.5177213153689));
#188280=CARTESIAN_POINT('Ctrl Pts',(16.6866974527108,19.7498908469243,12.519888695236));
#188281=CARTESIAN_POINT('Ctrl Pts',(16.6899750038319,19.7621922256845,12.5206357860504));
#188282=CARTESIAN_POINT('Ctrl Pts',(16.6962720542647,19.7849976098997,12.5220308421496));
#188283=CARTESIAN_POINT('Ctrl Pts',(16.6992623441283,19.7955092830765,12.5226778527903));
#188284=CARTESIAN_POINT('Ctrl Pts',(16.7042800303639,19.8126425797401,12.5237391489304));
#188285=CARTESIAN_POINT('Ctrl Pts',(16.7062587868906,19.819278324291,12.5241518434894));
#188286=CARTESIAN_POINT('Ctrl Pts',(16.7101425344424,19.8320728766593,12.5249508170893));
#188287=CARTESIAN_POINT('Ctrl Pts',(16.7120431741991,19.8382329329575,12.5253369497411));
#188288=CARTESIAN_POINT('Ctrl Pts',(16.716482554786,19.8523912812155,12.5262278480922));
#188289=CARTESIAN_POINT('Ctrl Pts',(16.7190407627863,19.8603833125067,12.5267332492526));
#188290=CARTESIAN_POINT('Ctrl Pts',(16.7260160948594,19.8817366625947,12.5280904273584));
#188291=CARTESIAN_POINT('Ctrl Pts',(16.7305189854825,19.8950693263921,12.528945019885));
#188292=CARTESIAN_POINT('Ctrl Pts',(16.7385075449603,19.9179671007584,12.5304253836614));
#188293=CARTESIAN_POINT('Ctrl Pts',(16.7419293246322,19.9275521350618,12.5310489251602));
#188294=CARTESIAN_POINT('Ctrl Pts',(16.7454193728684,19.937110246035,12.5316746173356));
#188295=CARTESIAN_POINT('Origin',(18.734,19.211,0.));
#188296=CARTESIAN_POINT('',(16.7454193601307,19.9371102111504,13.5571444941232));
#188297=CARTESIAN_POINT('',(16.7454193976962,19.9371103140301,13.3344632337298));
#188298=CARTESIAN_POINT('',(16.7454193623258,19.9371102171621,0.));
#188299=CARTESIAN_POINT('Ctrl Pts',(16.7454193601307,19.9371102111504,13.5571444941232));
#188300=CARTESIAN_POINT('Ctrl Pts',(16.7397540738622,19.9215948273702,13.556205238638));
#188301=CARTESIAN_POINT('Ctrl Pts',(16.7342701797465,19.9060126210941,13.5552608618068));
#188302=CARTESIAN_POINT('Ctrl Pts',(16.7177768414227,19.8573354415282,13.5523054355895));
#188303=CARTESIAN_POINT('Ctrl Pts',(16.7074032797185,19.8240341387795,13.550275897431));
#188304=CARTESIAN_POINT('Ctrl Pts',(16.6948809080674,19.7800347670629,13.5475781926283));
#188305=CARTESIAN_POINT('Ctrl Pts',(16.6919850817183,19.7695537611094,13.5469343990448));
#188306=CARTESIAN_POINT('Ctrl Pts',(16.6873806778076,19.7523742988017,13.5458770486284));
#188307=CARTESIAN_POINT('Ctrl Pts',(16.6856239155965,19.7456888782045,13.5454650598561));
#188308=CARTESIAN_POINT('Ctrl Pts',(16.6822909632723,19.7327476849927,13.5446665086269));
#188309=CARTESIAN_POINT('Ctrl Pts',(16.6807105627297,19.7264930683827,13.5442800875236));
#188310=CARTESIAN_POINT('Ctrl Pts',(16.6771333674884,19.7120584351188,13.5433871593065));
#188311=CARTESIAN_POINT('Ctrl Pts',(16.675156748058,19.7038735741306,13.5428800073666));
#188312=CARTESIAN_POINT('Ctrl Pts',(16.6699846617209,19.6818826805959,13.5415150676855));
#188313=CARTESIAN_POINT('Ctrl Pts',(16.666878945586,19.6680561744549,13.5406544136644));
#188314=CARTESIAN_POINT('Ctrl Pts',(16.6325818101217,19.5078618808092,13.530652836331));
#188315=CARTESIAN_POINT('Ctrl Pts',(16.6168624938294,19.3586426934898,13.5210013133909));
#188316=CARTESIAN_POINT('Ctrl Pts',(16.6171394758123,19.0592697728877,13.5012717527447));
#188317=CARTESIAN_POINT('Ctrl Pts',(16.6331712117549,18.9099266964476,13.4912565952426));
#188318=CARTESIAN_POINT('Ctrl Pts',(16.6681544973136,18.7481628833701,13.4809318509259));
#188319=CARTESIAN_POINT('Ctrl Pts',(16.6716463803462,18.7328437301509,13.4799597589874));
#188320=CARTESIAN_POINT('Ctrl Pts',(16.6766589549459,18.711930477319,13.4786417905151));
#188321=CARTESIAN_POINT('Ctrl Pts',(16.6780324475907,18.706302081055,13.4782879916511));
#188322=CARTESIAN_POINT('Ctrl Pts',(16.6802514660739,18.6973682261554,13.4777279334526));
#188323=CARTESIAN_POINT('Ctrl Pts',(16.681081895107,18.6940590994209,13.4775208184102));
#188324=CARTESIAN_POINT('Ctrl Pts',(16.6828132681113,18.6872298273676,13.4770940882093));
#188325=CARTESIAN_POINT('Ctrl Pts',(16.6837152757193,18.6837099921797,13.4768745417128));
#188326=CARTESIAN_POINT('Ctrl Pts',(16.6858857804549,18.6753299767811,13.4763527474719));
#188327=CARTESIAN_POINT('Ctrl Pts',(16.6871625312223,18.6704719177788,13.4760509755103));
#188328=CARTESIAN_POINT('Ctrl Pts',(16.6915249225735,18.654110051492,13.4750369077715));
#188329=CARTESIAN_POINT('Ctrl Pts',(16.6946904144626,18.6426275115,13.4743290803725));
#188330=CARTESIAN_POINT('Ctrl Pts',(16.7322349721505,18.5107910104225,13.4662399156346));
#188331=CARTESIAN_POINT('Ctrl Pts',(16.7771312058472,18.3936693979983,13.4594083292007));
#188332=CARTESIAN_POINT('Ctrl Pts',(16.9057920733551,18.1305005211885,13.4434861810867));
#188333=CARTESIAN_POINT('Ctrl Pts',(16.9970991709072,17.9891195178236,13.4344327380553));
#188334=CARTESIAN_POINT('Ctrl Pts',(17.1191104020009,17.841923018109,13.4233283528523));
#188335=CARTESIAN_POINT('Ctrl Pts',(17.1343922138713,17.8240987555528,13.4219533516413));
#188336=CARTESIAN_POINT('Ctrl Pts',(17.156353391162,17.7993297660029,13.4199973526351));
#188337=CARTESIAN_POINT('Ctrl Pts',(17.1627888949226,17.7921704363942,13.4194265091625));
#188338=CARTESIAN_POINT('Ctrl Pts',(17.1733018874588,17.7806342495479,13.4184976302671));
#188339=CARTESIAN_POINT('Ctrl Pts',(17.1773495369906,17.7762302925425,13.418140860992));
#188340=CARTESIAN_POINT('Ctrl Pts',(17.1858428974053,17.767067523762,13.4173939949306));
#188341=CARTESIAN_POINT('Ctrl Pts',(17.1902920058684,17.7623119598642,13.4170037547204));
#188342=CARTESIAN_POINT('Ctrl Pts',(17.2008948571889,17.751083087009,13.4160760565232));
#188343=CARTESIAN_POINT('Ctrl Pts',(17.2070677265501,17.7446280825699,13.4155377747377));
#188344=CARTESIAN_POINT('Ctrl Pts',(17.2278430665602,17.7231766182588,13.4137320225775));
#188345=CARTESIAN_POINT('Ctrl Pts',(17.242626711455,17.7083580638623,13.4124566428821));
#188346=CARTESIAN_POINT('Ctrl Pts',(17.323261505804,17.6298951076832,13.405548924508));
#188347=CARTESIAN_POINT('Ctrl Pts',(17.3929621875943,17.5703630572841,13.3997422774234));
#188348=CARTESIAN_POINT('Ctrl Pts',(17.5419202795196,17.4589860863717,13.3876785377884));
#188349=CARTESIAN_POINT('Ctrl Pts',(17.6212465352811,17.4075630532717,13.3814262462463));
#188350=CARTESIAN_POINT('Ctrl Pts',(17.7685848998751,17.3254832848588,13.3702890212522));
#188351=CARTESIAN_POINT('Ctrl Pts',(17.835293607746,17.2927905039487,13.3654068856028));
#188352=CARTESIAN_POINT('Ctrl Pts',(17.9424467989667,17.24709639275,13.3579381768206));
#188353=CARTESIAN_POINT('Ctrl Pts',(17.9817988025074,17.2316900799468,13.355271063532));
#188354=CARTESIAN_POINT('Ctrl Pts',(18.0286043446051,17.2149635577244,13.3522081780424));
#188355=CARTESIAN_POINT('Ctrl Pts',(18.0356335859481,17.2124933412616,13.3517510585795));
#188356=CARTESIAN_POINT('Ctrl Pts',(18.0470291413366,17.2085561798659,13.3510147870947));
#188357=CARTESIAN_POINT('Ctrl Pts',(18.0513873874959,17.2070663095746,13.3507343291401));
#188358=CARTESIAN_POINT('Ctrl Pts',(18.0591363519902,17.2044455323006,13.3502377237466));
#188359=CARTESIAN_POINT('Ctrl Pts',(18.0625251020079,17.2033089786305,13.3500212460875));
#188360=CARTESIAN_POINT('Ctrl Pts',(18.0698013120878,17.2008890922465,13.3495579339211));
#188361=CARTESIAN_POINT('Ctrl Pts',(18.073689609769,17.1996084549,13.3493112588506));
#188362=CARTESIAN_POINT('Ctrl Pts',(18.0843955207839,17.1961167804851,13.3486345154514));
#188363=CARTESIAN_POINT('Ctrl Pts',(18.0912207584813,17.1939290499052,13.3482057979176));
#188364=CARTESIAN_POINT('Ctrl Pts',(18.1280704969853,17.1823234380661,13.3459051140435));
#188365=CARTESIAN_POINT('Ctrl Pts',(18.1582927558532,17.1735406597748,13.3440681093112));
#188366=CARTESIAN_POINT('Ctrl Pts',(18.3467775002746,17.1232951547105,13.3328547375767));
#188367=CARTESIAN_POINT('Ctrl Pts',(18.5092220814565,17.0996165863916,13.3242094004181));
#188368=CARTESIAN_POINT('Ctrl Pts',(18.7898605950997,17.0914986028029,13.3088409057954));
#188369=CARTESIAN_POINT('Ctrl Pts',(18.9069971553275,17.0978333538537,13.3023034437241));
#188370=CARTESIAN_POINT('Ctrl Pts',(19.0371602854161,17.115770382029,13.2946060268684));
#188371=CARTESIAN_POINT('Ctrl Pts',(19.0512998051299,17.1178649997146,13.2937642965802));
#188372=CARTESIAN_POINT('Ctrl Pts',(19.0737683340558,17.1214263640575,13.2924174273655));
#188373=CARTESIAN_POINT('Ctrl Pts',(19.0821117912416,17.122800134449,13.291915231639));
#188374=CARTESIAN_POINT('Ctrl Pts',(19.0968115305499,17.1253110283864,13.2910267433246));
#188375=CARTESIAN_POINT('Ctrl Pts',(19.103171295463,17.126427322881,13.2906411171286));
#188376=CARTESIAN_POINT('Ctrl Pts',(19.1163141434507,17.1287962456996,13.2898416172451));
#188377=CARTESIAN_POINT('Ctrl Pts',(19.1230964028221,17.1300529640896,13.289427617385));
#188378=CARTESIAN_POINT('Ctrl Pts',(19.1404886073149,17.1333636504031,13.2883622544716));
#188379=CARTESIAN_POINT('Ctrl Pts',(19.1510890893745,17.135465737747,13.2877093627331));
#188380=CARTESIAN_POINT('Ctrl Pts',(19.1952560392294,17.1445761124812,13.2849739250263));
#188381=CARTESIAN_POINT('Ctrl Pts',(19.2286642939744,17.1523179369113,13.2828680610068));
#188382=CARTESIAN_POINT('Ctrl Pts',(19.315200780115,17.1745993588527,13.2773137821463));
#188383=CARTESIAN_POINT('Ctrl Pts',(19.3679730893346,17.1904062207996,13.2738269852899));
#188384=CARTESIAN_POINT('Ctrl Pts',(19.5235313423195,17.243694583468,13.263258003926));
#188385=CARTESIAN_POINT('Ctrl Pts',(19.6240876398678,17.2871000885754,13.2560274267358));
#188386=CARTESIAN_POINT('Ctrl Pts',(19.7612323084613,17.3593607083982,13.2457873707386));
#188387=CARTESIAN_POINT('Ctrl Pts',(19.800934003124,17.3819493431767,13.2427764331929));
#188388=CARTESIAN_POINT('Ctrl Pts',(19.8593556375535,17.4177388334853,13.2383012221881));
#188389=CARTESIAN_POINT('Ctrl Pts',(19.8786424606454,17.4299877563269,13.236816294639));
#188390=CARTESIAN_POINT('Ctrl Pts',(19.8983086694723,17.4429290721572,13.2352969564636));
#188391=CARTESIAN_POINT('Ctrl Pts',(19.8988894558718,17.4433116679426,13.2352520823547));
#188392=CARTESIAN_POINT('Ctrl Pts',(19.9087269765776,17.4497991349456,13.2344919136997));
#188393=CARTESIAN_POINT('Ctrl Pts',(19.9179359409109,17.4559764525475,13.2337791349056));
#188394=CARTESIAN_POINT('Ctrl Pts',(19.9604241808332,17.4849639322779,13.2304864497088));
#188395=CARTESIAN_POINT('Ctrl Pts',(19.9930980326395,17.5086517954744,13.2279425500857));
#188396=CARTESIAN_POINT('Ctrl Pts',(20.0309009368652,17.5377424102635,13.2250038123527));
#188397=CARTESIAN_POINT('Ctrl Pts',(20.0367014690806,17.5422543969451,13.2245530206632));
#188398=CARTESIAN_POINT('Ctrl Pts',(20.0460750153494,17.5496243394705,13.2238249282495));
#188399=CARTESIAN_POINT('Ctrl Pts',(20.0496624084111,17.5524637901735,13.2235463673584));
#188400=CARTESIAN_POINT('Ctrl Pts',(20.0560336517982,17.5575403611265,13.2230518458929));
#188401=CARTESIAN_POINT('Ctrl Pts',(20.0588210678533,17.5597729130448,13.222835565615));
#188402=CARTESIAN_POINT('Ctrl Pts',(20.0648072698867,17.5645924155432,13.2223712508755));
#188403=CARTESIAN_POINT('Ctrl Pts',(20.0680041593003,17.567181631879,13.222123383351));
#188404=CARTESIAN_POINT('Ctrl Pts',(20.0768208083879,17.5743650486191,13.2214399969953));
#188405=CARTESIAN_POINT('Ctrl Pts',(20.0824245796626,17.5789789082391,13.2210058733151));
#188406=CARTESIAN_POINT('Ctrl Pts',(20.1132087318636,17.6045918099911,13.2186215980315));
#188407=CARTESIAN_POINT('Ctrl Pts',(20.137923880987,17.62614606254,13.2167094816335));
#188408=CARTESIAN_POINT('Ctrl Pts',(20.2820626923086,17.7578697444379,13.2055013599741));
#188409=CARTESIAN_POINT('Ctrl Pts',(20.388992178696,17.8809254619845,13.1969133998443));
#188410=CARTESIAN_POINT('Ctrl Pts',(20.5467660705564,18.1113624518841,13.1816242300727));
#188411=CARTESIAN_POINT('Ctrl Pts',(20.604640064079,18.2129899499217,13.1751054354326));
#188412=CARTESIAN_POINT('Ctrl Pts',(20.6598598036079,18.3318201577148,13.1674290318761));
#188413=CARTESIAN_POINT('Ctrl Pts',(20.6657499953327,18.3448388609165,13.166587570704));
#188414=CARTESIAN_POINT('Ctrl Pts',(20.6749147243179,18.3656536147415,13.1652410516712));
#188415=CARTESIAN_POINT('Ctrl Pts',(20.6782751894718,18.3734115195486,13.1647389345883));
#188416=CARTESIAN_POINT('Ctrl Pts',(20.6841199576659,18.38712935428,13.1638505378828));
#188417=CARTESIAN_POINT('Ctrl Pts',(20.6866236468956,18.3930809439042,13.1634649242111));
#188418=CARTESIAN_POINT('Ctrl Pts',(20.6917458204163,18.4054145676137,13.1626654036184));
#188419=CARTESIAN_POINT('Ctrl Pts',(20.6943604129559,18.4117981257568,13.1622513702947));
#188420=CARTESIAN_POINT('Ctrl Pts',(20.7009917938761,18.4282170635601,13.1611858229549));
#188421=CARTESIAN_POINT('Ctrl Pts',(20.7049629687823,18.4382705443305,13.1605327792316));
#188422=CARTESIAN_POINT('Ctrl Pts',(20.7212176994973,18.480361843897,13.1577958686475));
#188423=CARTESIAN_POINT('Ctrl Pts',(20.7327978776588,18.5126640291441,13.1556886523177));
#188424=CARTESIAN_POINT('Ctrl Pts',(20.7609219089828,18.5975550055894,13.1501299561792));
#188425=CARTESIAN_POINT('Ctrl Pts',(20.776204957309,18.6505311988173,13.1466400181981));
#188426=CARTESIAN_POINT('Ctrl Pts',(20.8156027094488,18.8102641856276,13.1360650030276));
#188427=CARTESIAN_POINT('Ctrl Pts',(20.8335268487071,18.9183524663537,13.1288315532572));
#188428=CARTESIAN_POINT('Ctrl Pts',(20.8472922902954,19.0764177004891,13.1183507058952));
#188429=CARTESIAN_POINT('Ctrl Pts',(20.8498521887972,19.1256391944558,13.1151025285415));
#188430=CARTESIAN_POINT('Ctrl Pts',(20.8509790979049,19.1917260410636,13.110792261341));
#188431=CARTESIAN_POINT('Ctrl Pts',(20.8510654217678,19.2085489412297,13.1096995107603));
#188432=CARTESIAN_POINT('Ctrl Pts',(20.8505891738575,19.2787017795715,13.1051655061558));
#188433=CARTESIAN_POINT('Ctrl Pts',(20.8482119577541,19.3320045265726,13.1017752562434));
#188434=CARTESIAN_POINT('Ctrl Pts',(20.8431062578115,19.3938546332154,13.0979469027155));
#188435=CARTESIAN_POINT('Ctrl Pts',(20.8423352440206,19.4025398873771,13.0974117488231));
#188436=CARTESIAN_POINT('Ctrl Pts',(20.8410865885957,19.4156831826243,13.0966058557712));
#188437=CARTESIAN_POINT('Ctrl Pts',(20.8406484209221,19.4201447550645,13.0963329802714));
#188438=CARTESIAN_POINT('Ctrl Pts',(20.8398364828793,19.4281506590888,13.0958446087146));
#188439=CARTESIAN_POINT('Ctrl Pts',(20.839467933502,19.4316954529372,13.0956288245853));
#188440=CARTESIAN_POINT('Ctrl Pts',(20.8386476757942,19.4393957802578,13.0951610679864));
#188441=CARTESIAN_POINT('Ctrl Pts',(20.8381926128612,19.4435508983845,13.0949092865756));
#188442=CARTESIAN_POINT('Ctrl Pts',(20.8368798386515,19.4552182478057,13.0942039755402));
#188443=CARTESIAN_POINT('Ctrl Pts',(20.8359941744184,19.4627273584427,13.0937519920002));
#188444=CARTESIAN_POINT('Ctrl Pts',(20.8304597778886,19.5075835447496,13.0910628711354));
#188445=CARTESIAN_POINT('Ctrl Pts',(20.8248557288286,19.5448084995763,13.0888761484958));
#188446=CARTESIAN_POINT('Ctrl Pts',(20.8031483977735,19.6668031566322,13.0818001900211));
#188447=CARTESIAN_POINT('Ctrl Pts',(20.7828560319212,19.7507433865722,13.0770743318795));
#188448=CARTESIAN_POINT('Ctrl Pts',(20.7056113723781,20.0019489289599,13.0627720153405));
#188449=CARTESIAN_POINT('Ctrl Pts',(20.6328342005034,20.1635091290785,13.0532865757092));
#188450=CARTESIAN_POINT('Ctrl Pts',(20.5289143588762,20.3337183705636,13.0416973717006));
#188451=CARTESIAN_POINT('Ctrl Pts',(20.5166570633827,20.353080482869,13.0403548178549));
#188452=CARTESIAN_POINT('Ctrl Pts',(20.4988587372857,20.380210642994,13.0384372474192));
#188453=CARTESIAN_POINT('Ctrl Pts',(20.4935755239224,20.3881464910359,13.0378718467758));
#188454=CARTESIAN_POINT('Ctrl Pts',(20.4849001172674,20.4009888048519,13.0369494253568));
#188455=CARTESIAN_POINT('Ctrl Pts',(20.4815404356815,20.4059171522982,13.0365936357227));
#188456=CARTESIAN_POINT('Ctrl Pts',(20.474460957284,20.4162083858102,13.0358468668041));
#188457=CARTESIAN_POINT('Ctrl Pts',(20.4707371026215,20.4215683921011,13.0354557354522));
#188458=CARTESIAN_POINT('Ctrl Pts',(20.4618130245185,20.4342875176059,13.0345223175787));
#188459=CARTESIAN_POINT('Ctrl Pts',(20.4565905150963,20.4416307780169,13.0339791798033));
#188460=CARTESIAN_POINT('Ctrl Pts',(20.4388081802749,20.4662991574739,13.032140090187));
#188461=CARTESIAN_POINT('Ctrl Pts',(20.4260329179353,20.4834666825315,13.030835824671));
#188462=CARTESIAN_POINT('Ctrl Pts',(20.3548584525755,20.5761442727884,13.0236579371424));
#188463=CARTESIAN_POINT('Ctrl Pts',(20.2916709156374,20.6478222122537,13.0175943698583));
#188464=CARTESIAN_POINT('Ctrl Pts',(20.102757300723,20.8349629094854,13.0003131591558));
#188465=CARTESIAN_POINT('Ctrl Pts',(19.9676031346825,20.9398644550541,12.9888106745707));
#188466=CARTESIAN_POINT('Ctrl Pts',(19.7898897515995,21.0462463434158,12.9755928202219));
#188467=CARTESIAN_POINT('Ctrl Pts',(19.7579566110554,21.0642526920185,12.9732875602183));
#188468=CARTESIAN_POINT('Ctrl Pts',(19.7192673661779,21.0847630859846,12.9705910311118));
#188469=CARTESIAN_POINT('Ctrl Pts',(19.7129478892879,21.0880724329709,12.970153599355));
#188470=CARTESIAN_POINT('Ctrl Pts',(19.7026060929287,21.0934217312935,12.9694428061299));
#188471=CARTESIAN_POINT('Ctrl Pts',(19.6985938287514,21.0954808526779,12.9691682788126));
#188472=CARTESIAN_POINT('Ctrl Pts',(19.6913974003784,21.0991451036556,12.9686781363137));
#188473=CARTESIAN_POINT('Ctrl Pts',(19.6882157445421,21.1007550180335,12.9684622238485));
#188474=CARTESIAN_POINT('Ctrl Pts',(19.6813135643646,21.1042256374955,12.9679955395396));
#188475=CARTESIAN_POINT('Ctrl Pts',(19.6775916307304,21.1060834120953,12.9677449514729));
#188476=CARTESIAN_POINT('Ctrl Pts',(19.6671721546053,21.1112459070399,12.9670463465847));
#188477=CARTESIAN_POINT('Ctrl Pts',(19.6604624883982,21.1145262117225,12.9665998289362));
#188478=CARTESIAN_POINT('Ctrl Pts',(19.6212515661908,21.1334396926026,12.9640090852071));
#188479=CARTESIAN_POINT('Ctrl Pts',(19.588370332991,21.1482767993219,12.9619110771972));
#188480=CARTESIAN_POINT('Ctrl Pts',(19.4811302382674,21.1934051110076,12.9552561063467));
#188481=CARTESIAN_POINT('Ctrl Pts',(19.4054192438977,21.2203112827015,12.9508410842745));
#188482=CARTESIAN_POINT('Ctrl Pts',(19.1504389061178,21.2948981213496,12.9363592389987));
#188483=CARTESIAN_POINT('Ctrl Pts',(18.9664766600931,21.3233449790301,12.9264433370417));
#188484=CARTESIAN_POINT('Ctrl Pts',(18.7590375426672,21.3279676331766,12.9143759547045));
#188485=CARTESIAN_POINT('Ctrl Pts',(18.7369050173621,21.3281136825569,12.9130785724825));
#188486=CARTESIAN_POINT('Ctrl Pts',(18.7063123096548,21.327835849226,12.9112701164498));
#188487=CARTESIAN_POINT('Ctrl Pts',(18.6978503855179,21.3277082517385,12.9107682988479));
#188488=CARTESIAN_POINT('Ctrl Pts',(18.6833118226015,21.327401820025,12.9099032813667));
#188489=CARTESIAN_POINT('Ctrl Pts',(18.677234728488,21.3272475417346,12.9095408536662));
#188490=CARTESIAN_POINT('Ctrl Pts',(18.6647126903276,21.3268756704825,12.9087922693));
#188491=CARTESIAN_POINT('Ctrl Pts',(18.6582679135756,21.326654800264,12.9084060137079));
#188492=CARTESIAN_POINT('Ctrl Pts',(18.6432809836845,21.3260726130555,12.9075054817577));
#188493=CARTESIAN_POINT('Ctrl Pts',(18.6347398547215,21.3256889886289,12.9069905111009));
#188494=CARTESIAN_POINT('Ctrl Pts',(18.6074430812867,21.3242972187698,12.9053389791064));
#188495=CARTESIAN_POINT('Ctrl Pts',(18.5886988360557,21.3230912207108,12.9041962419787));
#188496=CARTESIAN_POINT('Ctrl Pts',(18.4953416648932,21.315836041475,12.8984600578295));
#188497=CARTESIAN_POINT('Ctrl Pts',(18.4210779900157,21.3060823963527,12.8937517313576));
#188498=CARTESIAN_POINT('Ctrl Pts',(18.2404624928557,21.2725431882532,12.8819499532233));
#188499=CARTESIAN_POINT('Ctrl Pts',(18.1351316684906,21.2444435891157,12.8747560833273));
#188500=CARTESIAN_POINT('Ctrl Pts',(17.919239853413,21.1686132225083,12.8596390929953));
#188501=CARTESIAN_POINT('Ctrl Pts',(17.8096130647179,21.1192974322654,12.8517437931516));
#188502=CARTESIAN_POINT('Ctrl Pts',(17.6964404430413,21.0563318112895,12.8437448065828));
#188503=CARTESIAN_POINT('Ctrl Pts',(17.6881662590596,21.0516550795968,12.8431609863434));
#188504=CARTESIAN_POINT('Ctrl Pts',(17.6759498212068,21.0446411361393,12.842300804376));
#188505=CARTESIAN_POINT('Ctrl Pts',(17.6719833410133,21.042346666782,12.842021800709));
#188506=CARTESIAN_POINT('Ctrl Pts',(17.6650378145969,21.0382987699757,12.8415337911044));
#188507=CARTESIAN_POINT('Ctrl Pts',(17.6620555855149,21.0365509090266,12.841324430124));
#188508=CARTESIAN_POINT('Ctrl Pts',(17.655652694039,21.0327771247632,12.840875320619));
#188509=CARTESIAN_POINT('Ctrl Pts',(17.6522334625651,21.0307488737924,12.8406357265764));
#188510=CARTESIAN_POINT('Ctrl Pts',(17.6451818483515,21.0265390344637,12.8401420488052));
#188511=CARTESIAN_POINT('Ctrl Pts',(17.6415502575272,21.0243561464567,12.8398880499292));
#188512=CARTESIAN_POINT('Ctrl Pts',(17.6324230693109,21.0188325770657,12.8392502371787));
#188513=CARTESIAN_POINT('Ctrl Pts',(17.626936053064,21.0154777030106,12.8388673115854));
#188514=CARTESIAN_POINT('Ctrl Pts',(17.6113420138901,21.0058452863295,12.8377802467602));
#188515=CARTESIAN_POINT('Ctrl Pts',(17.6012723391928,20.999507370897,12.8370797383748));
#188516=CARTESIAN_POINT('Ctrl Pts',(17.5675330353624,20.977872387555,12.8347356573142));
#188517=CARTESIAN_POINT('Ctrl Pts',(17.5441146720641,20.962187103051,12.8331137030966));
#188518=CARTESIAN_POINT('Ctrl Pts',(17.3582698101486,20.8322608824912,12.8202242556187));
#188519=CARTESIAN_POINT('Ctrl Pts',(17.2123307147047,20.6961460411557,12.8099003662596));
#188520=CARTESIAN_POINT('Ctrl Pts',(17.0418418322238,20.4851913693457,12.7947367000877));
#188521=CARTESIAN_POINT('Ctrl Pts',(16.9991350587083,20.426403193772,12.7905946435565));
#188522=CARTESIAN_POINT('Ctrl Pts',(16.9524297804521,20.3546198335921,12.7855690505901));
#188523=CARTESIAN_POINT('Ctrl Pts',(16.9454249621493,20.3436332564456,12.7848007971853));
#188524=CARTESIAN_POINT('Ctrl Pts',(16.9341931541268,20.3256528977271,12.7835446515976));
#188525=CARTESIAN_POINT('Ctrl Pts',(16.9299043899144,20.3186979695176,12.7830590448306));
#188526=CARTESIAN_POINT('Ctrl Pts',(16.9223301086203,20.306254364451,12.782190624843));
#188527=CARTESIAN_POINT('Ctrl Pts',(16.9190289863932,20.300775268833,12.78180839016));
#188528=CARTESIAN_POINT('Ctrl Pts',(16.9121165385757,20.289183684089,12.7809999942452));
#188529=CARTESIAN_POINT('Ctrl Pts',(16.9085110338063,20.2830678318283,12.7805736269709));
#188530=CARTESIAN_POINT('Ctrl Pts',(16.8990353467703,20.2668082566338,12.7794404277033));
#188531=CARTESIAN_POINT('Ctrl Pts',(16.8932185809274,20.2566338326202,12.7787316746851));
#188532=CARTESIAN_POINT('Ctrl Pts',(16.8663619662945,20.2087387856,12.7753964933996));
#188533=CARTESIAN_POINT('Ctrl Pts',(16.8463964369092,20.1704304918226,12.7727320466668));
#188534=CARTESIAN_POINT('Ctrl Pts',(16.7969731233895,20.0680778629996,12.7656162602273));
#188535=CARTESIAN_POINT('Ctrl Pts',(16.7695455578597,20.0031840886229,12.7611063920367));
#188536=CARTESIAN_POINT('Ctrl Pts',(16.745419226499,19.9371098451765,12.7565300941239));
#188537=CARTESIAN_POINT('Ctrl Pts',(16.7454193728684,19.937110246035,12.5316746173356));
#188538=CARTESIAN_POINT('Ctrl Pts',(16.7951534513481,20.0733157678728,12.5405908905923));
#188539=CARTESIAN_POINT('Ctrl Pts',(16.8587496331707,20.2040517459169,12.5499845536731));
#188540=CARTESIAN_POINT('Ctrl Pts',(16.9704453902929,20.384042994092,12.5639575310776));
#188541=CARTESIAN_POINT('Ctrl Pts',(17.0083507021618,20.4391243166459,12.5683870471575));
#188542=CARTESIAN_POINT('Ctrl Pts',(17.0853815792362,20.5404358702716,12.5767428575914));
#188543=CARTESIAN_POINT('Ctrl Pts',(17.1240118117388,20.5869656543858,12.5806727923772));
#188544=CARTESIAN_POINT('Ctrl Pts',(17.1848101369709,20.6541244327597,12.5864164111745));
#188545=CARTESIAN_POINT('Ctrl Pts',(17.2055133917509,20.6760345611683,12.588302358832));
#188546=CARTESIAN_POINT('Ctrl Pts',(17.2314460061007,20.70233047705,12.590572768724));
#188547=CARTESIAN_POINT('Ctrl Pts',(17.2362366505817,20.707141720686,12.5909884674441));
#188548=CARTESIAN_POINT('Ctrl Pts',(17.2440063551608,20.7148701142812,12.5916565586287));
#188549=CARTESIAN_POINT('Ctrl Pts',(17.2469709863386,20.7178016111985,12.5919100570225));
#188550=CARTESIAN_POINT('Ctrl Pts',(17.2524865596783,20.7232234076128,12.592379018702));
#188551=CARTESIAN_POINT('Ctrl Pts',(17.2550351084239,20.7257159991752,12.5925946593841));
#188552=CARTESIAN_POINT('Ctrl Pts',(17.2608129353265,20.7313384807468,12.593081184203));
#188553=CARTESIAN_POINT('Ctrl Pts',(17.2640458887809,20.7344645172529,12.5933517675464));
#188554=CARTESIAN_POINT('Ctrl Pts',(17.2736234849937,20.7436665014956,12.5941486019655));
#188555=CARTESIAN_POINT('Ctrl Pts',(17.279996102778,20.7497133726914,12.5946726503172));
#188556=CARTESIAN_POINT('Ctrl Pts',(17.3265472395098,20.793337530867,12.5984580705629));
#188557=CARTESIAN_POINT('Ctrl Pts',(17.3681429756252,20.8293791371839,12.6016115533307));
#188558=CARTESIAN_POINT('Ctrl Pts',(17.4341018510134,20.8821738108328,12.6063563622713));
#188559=CARTESIAN_POINT('Ctrl Pts',(17.457486914923,20.9001037707016,12.6079923190341));
#188560=CARTESIAN_POINT('Ctrl Pts',(17.5992267863209,21.004154141963,12.6176841330977));
#188561=CARTESIAN_POINT('Ctrl Pts',(17.7258770430646,21.0782979248174,12.6254620917527));
#188562=CARTESIAN_POINT('Ctrl Pts',(17.9081626770306,21.1610197036013,12.6366045313939));
#188563=CARTESIAN_POINT('Ctrl Pts',(17.9579868512715,21.1813774040388,12.6396414866404));
#188564=CARTESIAN_POINT('Ctrl Pts',(18.0400744225546,21.2113209118695,12.6446710844814));
#188565=CARTESIAN_POINT('Ctrl Pts',(18.0718868047725,21.2220749338643,12.6466262603229));
#188566=CARTESIAN_POINT('Ctrl Pts',(18.1142573081268,21.2352837702599,12.6492437388411));
#188567=CARTESIAN_POINT('Ctrl Pts',(18.1245987111298,21.2384209847085,12.6498836208925));
#188568=CARTESIAN_POINT('Ctrl Pts',(18.141579338128,21.2434306477105,12.650936175322));
#188569=CARTESIAN_POINT('Ctrl Pts',(18.14820457672,21.2453500924617,12.6513473072914));
#188570=CARTESIAN_POINT('Ctrl Pts',(18.161049705212,21.2490035948981,12.6521453601056));
#188571=CARTESIAN_POINT('Ctrl Pts',(18.1672683877396,21.2507416432841,12.6525321457706));
#188572=CARTESIAN_POINT('Ctrl Pts',(18.1816489827792,21.2546900096582,12.6534276069409));
#188573=CARTESIAN_POINT('Ctrl Pts',(18.1898163403436,21.2568799190382,12.6539369389564));
#188574=CARTESIAN_POINT('Ctrl Pts',(18.2118246926749,21.2626398964955,12.6553115652768));
#188575=CARTESIAN_POINT('Ctrl Pts',(18.2256889025591,21.2661187627386,12.6561797897569));
#188576=CARTESIAN_POINT('Ctrl Pts',(18.3535020627039,21.2968177226203,12.6642060517678));
#188577=CARTESIAN_POINT('Ctrl Pts',(18.4694728363121,21.3146710214679,12.6716675300691));
#188578=CARTESIAN_POINT('Ctrl Pts',(18.7496195305198,21.3342630297295,12.69001330445));
#188579=CARTESIAN_POINT('Ctrl Pts',(18.9136997210596,21.3267027436058,12.7010402575659));
#188580=CARTESIAN_POINT('Ctrl Pts',(19.1062175737581,21.2952568099131,12.7134218699726));
#188581=CARTESIAN_POINT('Ctrl Pts',(19.1370520153354,21.289514298128,12.7153857117907));
#188582=CARTESIAN_POINT('Ctrl Pts',(19.1747568655624,21.2816215596416,12.7177541337578));
#188583=CARTESIAN_POINT('Ctrl Pts',(19.1817570641724,21.2801191054776,12.7181924416916));
#188584=CARTESIAN_POINT('Ctrl Pts',(19.1927461194891,21.277702141699,12.7188781454743));
#188585=CARTESIAN_POINT('Ctrl Pts',(19.1967401009818,21.2768115461601,12.7191268737939));
#188586=CARTESIAN_POINT('Ctrl Pts',(19.2042181176983,21.2751212898615,12.7195916193548));
#188587=CARTESIAN_POINT('Ctrl Pts',(19.2077026699488,21.2743243947982,12.7198077854625));
#188588=CARTESIAN_POINT('Ctrl Pts',(19.2156751146127,21.272479886332,12.7203014790328));
#188589=CARTESIAN_POINT('Ctrl Pts',(19.2201616077601,21.2714264436882,12.720578668207));
#188590=CARTESIAN_POINT('Ctrl Pts',(19.2319008280872,21.2686295599241,12.7213023690986));
#188591=CARTESIAN_POINT('Ctrl Pts',(19.2391479157896,21.2668624047758,12.72174755272));
#188592=CARTESIAN_POINT('Ctrl Pts',(19.2875407330671,21.2547907899921,12.7247105966769));
#188593=CARTESIAN_POINT('Ctrl Pts',(19.3283811712733,21.2432892767676,12.7271643235586));
#188594=CARTESIAN_POINT('Ctrl Pts',(19.3779669887142,21.2277019668476,12.7301163733928));
#188595=CARTESIAN_POINT('Ctrl Pts',(19.3870632233857,21.224774748226,12.7306567747096));
#188596=CARTESIAN_POINT('Ctrl Pts',(19.4096895645133,21.2173240335051,12.7319988559527));
#188597=CARTESIAN_POINT('Ctrl Pts',(19.4231944651367,21.2127251353947,12.7327979870546));
#188598=CARTESIAN_POINT('Ctrl Pts',(19.5716113515952,21.1605038266174,12.7415693435315));
#188599=CARTESIAN_POINT('Ctrl Pts',(19.7014134825564,21.0994578283077,12.7491651043511));
#188600=CARTESIAN_POINT('Ctrl Pts',(19.9037846689524,20.9779011817902,12.7621659333495));
#188601=CARTESIAN_POINT('Ctrl Pts',(19.980248981247,20.9248251189157,12.7673867183288));
#188602=CARTESIAN_POINT('Ctrl Pts',(20.0694784653254,20.8537512284259,12.7740313484491));
#188603=CARTESIAN_POINT('Ctrl Pts',(20.0857869476221,20.8403576435688,12.77526985305));
#188604=CARTESIAN_POINT('Ctrl Pts',(20.1087310760519,20.8209328447991,12.7770483114854));
#188605=CARTESIAN_POINT('Ctrl Pts',(20.115533178869,20.8150995505733,12.7775801750663));
#188606=CARTESIAN_POINT('Ctrl Pts',(20.1272183777149,20.8049491932252,12.7785019707523));
#188607=CARTESIAN_POINT('Ctrl Pts',(20.1321189842717,20.8006524094719,12.7788910586014));
#188608=CARTESIAN_POINT('Ctrl Pts',(20.1414741740665,20.7923731854999,12.7796386720994));
#188609=CARTESIAN_POINT('Ctrl Pts',(20.1459318977554,20.7883943760029,12.7799970434757));
#188610=CARTESIAN_POINT('Ctrl Pts',(20.1575015097735,20.7779794046365,12.7809327851854));
#188611=CARTESIAN_POINT('Ctrl Pts',(20.1645865470585,20.7715137389722,12.7815114001816));
#188612=CARTESIAN_POINT('Ctrl Pts',(20.1887074057308,20.7491991958307,12.7835007012245));
#188613=CARTESIAN_POINT('Ctrl Pts',(20.2055252726324,20.7331181644514,12.7849212977454));
#188614=CARTESIAN_POINT('Ctrl Pts',(20.3440308911561,20.5962396930944,12.7969104829135));
#188615=CARTESIAN_POINT('Ctrl Pts',(20.4508717111137,20.4613671797419,12.8081468609156));
#188616=CARTESIAN_POINT('Ctrl Pts',(20.5871336332421,20.2384532413753,12.8254112865684));
#188617=CARTESIAN_POINT('Ctrl Pts',(20.6290755032049,20.1588687930003,12.8313409597301));
#188618=CARTESIAN_POINT('Ctrl Pts',(20.6815952813217,20.0416904362553,12.8395443291328));
#188619=CARTESIAN_POINT('Ctrl Pts',(20.6963944125211,20.0060991021721,12.8419694562089));
#188620=CARTESIAN_POINT('Ctrl Pts',(20.712944117017,19.9630153746079,12.8448097518762));
#188621=CARTESIAN_POINT('Ctrl Pts',(20.7156353429459,19.9558948338867,12.8452760977527));
#188622=CARTESIAN_POINT('Ctrl Pts',(20.7197486755566,19.9448315622699,12.8459957324565));
#188623=CARTESIAN_POINT('Ctrl Pts',(20.7211975471602,19.9408989474726,12.8462505756605));
#188624=CARTESIAN_POINT('Ctrl Pts',(20.7238565774959,19.9336150400623,12.8467207777181));
#188625=CARTESIAN_POINT('Ctrl Pts',(20.7250699440785,19.9302650229383,12.8469363218853));
#188626=CARTESIAN_POINT('Ctrl Pts',(20.7277860805794,19.9227064243602,12.8474210607724));
#188627=CARTESIAN_POINT('Ctrl Pts',(20.7292839814788,19.9184961510029,12.8476899642741));
#188628=CARTESIAN_POINT('Ctrl Pts',(20.7336431805049,19.9061194338257,12.8484772926983));
#188629=CARTESIAN_POINT('Ctrl Pts',(20.7364677935121,19.897940039864,12.848993592581));
#188630=CARTESIAN_POINT('Ctrl Pts',(20.7558510235146,19.8406752894476,12.8525817279561));
#188631=CARTESIAN_POINT('Ctrl Pts',(20.7706546720376,19.7910096722866,12.8555580212388));
#188632=CARTESIAN_POINT('Ctrl Pts',(20.7889977551949,19.720052572512,12.8596850524636));
#188633=CARTESIAN_POINT('Ctrl Pts',(20.794056626284,19.6991772580519,12.8608841341525));
#188634=CARTESIAN_POINT('Ctrl Pts',(20.8292168714097,19.5437954003393,12.8697211243266));
#188635=CARTESIAN_POINT('Ctrl Pts',(20.8464361376554,19.4067109023162,12.8770516832755));
#188636=CARTESIAN_POINT('Ctrl Pts',(20.8526909257654,19.178186584094,12.8896554780303));
#188637=CARTESIAN_POINT('Ctrl Pts',(20.8493361875485,19.0873956436999,12.8947578895238));
#188638=CARTESIAN_POINT('Ctrl Pts',(20.838061943456,18.9763804482943,12.9012593026213));
#188639=CARTESIAN_POINT('Ctrl Pts',(20.8356513394552,18.9556872552153,12.90248217698));
#188640=CARTESIAN_POINT('Ctrl Pts',(20.8317737292689,18.9261950672429,12.9042420623618));
#188641=CARTESIAN_POINT('Ctrl Pts',(20.8305558525056,18.917364132717,12.9047712157949));
#188642=CARTESIAN_POINT('Ctrl Pts',(20.8283522576459,18.9020987344584,12.9056898112319));
#188643=CARTESIAN_POINT('Ctrl Pts',(20.8273925642964,18.8956605935684,12.9060784249497));
#188644=CARTESIAN_POINT('Ctrl Pts',(20.8254934730554,18.8833113130543,12.9068261833565));
#188645=CARTESIAN_POINT('Ctrl Pts',(20.8245586678411,18.8773995225478,12.907185178844));
#188646=CARTESIAN_POINT('Ctrl Pts',(20.8220516906762,18.8619696246711,12.9081248994816));
#188647=CARTESIAN_POINT('Ctrl Pts',(20.8204395191019,18.8524582393242,12.9087068901558));
#188648=CARTESIAN_POINT('Ctrl Pts',(20.8146595297657,18.8197176411792,12.9107198241736));
#188649=CARTESIAN_POINT('Ctrl Pts',(20.8101684429913,18.7965479657116,12.9121609969831));
#188650=CARTESIAN_POINT('Ctrl Pts',(20.7711441855071,18.6118096603558,12.9237898296514));
#188651=CARTESIAN_POINT('Ctrl Pts',(20.7181976114173,18.4547423596878,12.9345920158262));
#188652=CARTESIAN_POINT('Ctrl Pts',(20.5930494831104,18.1902849276127,12.9539265501128));
#188653=CARTESIAN_POINT('Ctrl Pts',(20.5282543893181,18.0802559244732,12.9623538704573));
#188654=CARTESIAN_POINT('Ctrl Pts',(20.4469595082992,17.9669732798619,12.9710015854889));
#188655=CARTESIAN_POINT('Ctrl Pts',(20.4398861629441,17.9572914326574,12.9717402882779));
#188656=CARTESIAN_POINT('Ctrl Pts',(20.4297252028044,17.9436285458154,12.9727815710676));
#188657=CARTESIAN_POINT('Ctrl Pts',(20.4267051999686,17.9395978317186,12.9730886162176));
#188658=CARTESIAN_POINT('Ctrl Pts',(20.4214803084455,17.9326759298843,12.9736155942289));
#188659=CARTESIAN_POINT('Ctrl Pts',(20.4192823126398,17.9297795868355,12.9738360046449));
#188660=CARTESIAN_POINT('Ctrl Pts',(20.4150096327264,17.9241794106607,12.9742619733937));
#188661=CARTESIAN_POINT('Ctrl Pts',(20.4129358814965,17.9214749243734,12.9744675969283));
#188662=CARTESIAN_POINT('Ctrl Pts',(20.4073307637021,17.9142014415955,12.9750203988233));
#188663=CARTESIAN_POINT('Ctrl Pts',(20.403787188729,17.9096418279478,12.9753667215354));
#188664=CARTESIAN_POINT('Ctrl Pts',(20.3906100440894,17.8928288775598,12.9766431644192));
#188665=CARTESIAN_POINT('Ctrl Pts',(20.3808596249719,17.8806672018744,12.9775653464204));
#188666=CARTESIAN_POINT('Ctrl Pts',(20.2843015067537,17.7629192057729,12.9864949173469));
#188667=CARTESIAN_POINT('Ctrl Pts',(20.1875820394311,17.6658519887214,12.9938782343677));
#188668=CARTESIAN_POINT('Ctrl Pts',(19.9630236887574,17.4803733886287,13.0096948238436));
#188669=CARTESIAN_POINT('Ctrl Pts',(19.8334828130662,17.3953189210896,13.018114330301));
#188670=CARTESIAN_POINT('Ctrl Pts',(19.6768994534707,17.3154573245388,13.0283508688474));
#188671=CARTESIAN_POINT('Ctrl Pts',(19.6578075301877,17.3060797884219,13.0295990397689));
#188672=CARTESIAN_POINT('Ctrl Pts',(19.6304507546339,17.2931507225657,13.0313889745371));
#188673=CARTESIAN_POINT('Ctrl Pts',(19.6222991765023,17.2893615387726,13.0319225025498));
#188674=CARTESIAN_POINT('Ctrl Pts',(19.6081915341316,17.2829126816721,13.0328462669579));
#188675=CARTESIAN_POINT('Ctrl Pts',(19.6022468120009,17.2802283880722,13.033235649259));
#188676=CARTESIAN_POINT('Ctrl Pts',(19.5908383093738,17.2751403093181,13.0339831876487));
#188677=CARTESIAN_POINT('Ctrl Pts',(19.5853765737099,17.2727320724365,13.0343411863817));
#188678=CARTESIAN_POINT('Ctrl Pts',(19.5711423553406,17.266527566471,13.0352745420045));
#188679=CARTESIAN_POINT('Ctrl Pts',(19.5623542888184,17.2627675869218,13.0358511310905));
#188680=CARTESIAN_POINT('Ctrl Pts',(19.5322726147958,17.2501374535425,13.0378261508669));
#188681=CARTESIAN_POINT('Ctrl Pts',(19.5108602227467,17.241556113546,13.0392343011635));
#188682=CARTESIAN_POINT('Ctrl Pts',(19.3263063261939,17.17107133474,13.0513951056558));
#188683=CARTESIAN_POINT('Ctrl Pts',(19.156257656654,17.129219233369,13.0628424179537));
#188684=CARTESIAN_POINT('Ctrl Pts',(18.8959417329819,17.098381408126,13.0801628140937));
#188685=CARTESIAN_POINT('Ctrl Pts',(18.8082757903396,17.0934855416282,13.0859453020997));
#188686=CARTESIAN_POINT('Ctrl Pts',(18.6825553971514,17.0942840469478,13.0939733679116));
#188687=CARTESIAN_POINT('Ctrl Pts',(18.644567080935,17.0955484781117,13.0963639277373));
#188688=CARTESIAN_POINT('Ctrl Pts',(18.5990627520819,17.0982912120156,13.0991692106039));
#188689=CARTESIAN_POINT('Ctrl Pts',(18.591497059115,17.0987880315803,13.0996336871323));
#188690=CARTESIAN_POINT('Ctrl Pts',(18.5797601617785,17.0996221129831,13.1003510636406));
#188691=CARTESIAN_POINT('Ctrl Pts',(18.575587102031,17.0999311086715,13.100605502753));
#188692=CARTESIAN_POINT('Ctrl Pts',(18.5678619244165,17.1005261577805,13.1010753299295));
#188693=CARTESIAN_POINT('Ctrl Pts',(18.5643096431425,17.1008088044108,13.1012909009335));
#188694=CARTESIAN_POINT('Ctrl Pts',(18.5562959071319,17.1014668052009,13.1017761666201));
#188695=CARTESIAN_POINT('Ctrl Pts',(18.5518349322367,17.1018473422924,13.1020455672483));
#188696=CARTESIAN_POINT('Ctrl Pts',(18.5387170283978,17.1030082753438,13.1028357033986));
#188697=CARTESIAN_POINT('Ctrl Pts',(18.5300635387925,17.1038278485444,13.1033542910794));
#188698=CARTESIAN_POINT('Ctrl Pts',(18.4689434379666,17.1099965853368,13.1069999693863));
#188699=CARTESIAN_POINT('Ctrl Pts',(18.4166831346991,17.1172518477538,13.1100279943347));
#188700=CARTESIAN_POINT('Ctrl Pts',(18.3491993977167,17.1292058904386,13.1138841981394));
#188701=CARTESIAN_POINT('Ctrl Pts',(18.3336857616449,17.1321333024201,13.114766939039));
#188702=CARTESIAN_POINT('Ctrl Pts',(18.268355443228,17.145219532284,13.1184736985784));
#188703=CARTESIAN_POINT('Ctrl Pts',(18.2188789771997,17.1569979372192,13.1212551283587));
#188704=CARTESIAN_POINT('Ctrl Pts',(18.0644203227247,17.1997013293051,13.1299802793178));
#188705=CARTESIAN_POINT('Ctrl Pts',(17.961387342354,17.2369868056763,13.1358712586438));
#188706=CARTESIAN_POINT('Ctrl Pts',(17.8114224953119,17.304803598809,13.145022312314));
#188707=CARTESIAN_POINT('Ctrl Pts',(17.762054610024,17.329496483267,13.1481336795467));
#188708=CARTESIAN_POINT('Ctrl Pts',(17.6836215171005,17.3726384286187,13.1532834962776));
#188709=CARTESIAN_POINT('Ctrl Pts',(17.6539415161595,17.3899174376698,13.1552824414187));
#188710=CARTESIAN_POINT('Ctrl Pts',(17.6154867425232,17.4135757302737,13.1579451847157));
#188711=CARTESIAN_POINT('Ctrl Pts',(17.6063211065328,17.4193119079438,13.1585854071978));
#188712=CARTESIAN_POINT('Ctrl Pts',(17.5913800203159,17.4288226300313,13.1596383789554));
#188713=CARTESIAN_POINT('Ctrl Pts',(17.5855782965406,17.4325556839493,13.1600495854226));
#188714=CARTESIAN_POINT('Ctrl Pts',(17.5743824820032,17.4398371338546,13.1608476809128));
#188715=CARTESIAN_POINT('Ctrl Pts',(17.5689861673034,17.4433819828225,13.1612344342161));
#188716=CARTESIAN_POINT('Ctrl Pts',(17.5565627299155,17.4516245643296,13.1621296719968));
#188717=CARTESIAN_POINT('Ctrl Pts',(17.5495473935053,17.4563397854982,13.1626388119543));
#188718=CARTESIAN_POINT('Ctrl Pts',(17.5307542285844,17.4691353037707,13.164012583961));
#188719=CARTESIAN_POINT('Ctrl Pts',(17.5190297831873,17.4772928843191,13.1648801405224));
#188720=CARTESIAN_POINT('Ctrl Pts',(17.3924219185643,17.5672985341675,13.1743651190266));
#188721=CARTESIAN_POINT('Ctrl Pts',(17.2859326065109,17.6602989546083,13.1834322370289));
#188722=CARTESIAN_POINT('Ctrl Pts',(17.1234053906142,17.8336792176033,13.1990666174563));
#188723=CARTESIAN_POINT('Ctrl Pts',(17.062220711904,17.9086245762899,13.2054947896265));
#188724=CARTESIAN_POINT('Ctrl Pts',(16.968666055254,18.0407261198294,13.2160579281447));
#188725=CARTESIAN_POINT('Ctrl Pts',(16.9334396892371,18.0956843074626,13.2202520518305));
#188726=CARTESIAN_POINT('Ctrl Pts',(16.8942250343322,18.1635792794386,13.225123492732));
#188727=CARTESIAN_POINT('Ctrl Pts',(16.8877510527217,18.1750333331444,13.2259350812737));
#188728=CARTESIAN_POINT('Ctrl Pts',(16.8788540500822,18.1911226352675,13.2270600795359));
#188729=CARTESIAN_POINT('Ctrl Pts',(16.8763409370769,18.1957073614607,13.2273789641767));
#188730=CARTESIAN_POINT('Ctrl Pts',(16.8720920943216,18.2035272070418,13.2279199320434));
#188731=CARTESIAN_POINT('Ctrl Pts',(16.8703477570075,18.2067576011281,13.2281425593833));
#188732=CARTESIAN_POINT('Ctrl Pts',(16.867022326838,18.212954576243,13.2285679887888));
#188733=CARTESIAN_POINT('Ctrl Pts',(16.865439891317,18.215920394857,13.2287708789558));
#188734=CARTESIAN_POINT('Ctrl Pts',(16.8612708347414,18.2237791006438,13.229306628299));
#188735=CARTESIAN_POINT('Ctrl Pts',(16.8586963046326,18.2286784221811,13.2296387248677));
#188736=CARTESIAN_POINT('Ctrl Pts',(16.8496512072843,18.2460563702032,13.2308101504289));
#188737=CARTESIAN_POINT('Ctrl Pts',(16.8432855781046,18.2585895948662,13.2316431345393));
#188738=CARTESIAN_POINT('Ctrl Pts',(16.7641645776927,18.418290257541,13.242119199025));
#188739=CARTESIAN_POINT('Ctrl Pts',(16.70863132133,18.5733961322497,13.2508474035975));
#188740=CARTESIAN_POINT('Ctrl Pts',(16.6409703157188,18.8655650534694,13.2671776861255));
#188741=CARTESIAN_POINT('Ctrl Pts',(16.6231411421165,19.0003664244169,13.2746743969852));
#188742=CARTESIAN_POINT('Ctrl Pts',(16.6177334382085,19.152784649311,13.2835989613812));
#188743=CARTESIAN_POINT('Ctrl Pts',(16.6173369766561,19.1696380758585,13.2845914629408));
#188744=CARTESIAN_POINT('Ctrl Pts',(16.6170471058789,19.1946775550146,13.286075152639));
#188745=CARTESIAN_POINT('Ctrl Pts',(16.6169998255318,19.2028614149966,13.2865615231206));
#188746=CARTESIAN_POINT('Ctrl Pts',(16.6170001372642,19.2174435235817,13.2874307960698));
#188747=CARTESIAN_POINT('Ctrl Pts',(16.6170292805232,19.2238417019445,13.2878131157006));
#188748=CARTESIAN_POINT('Ctrl Pts',(16.6171518843233,19.2373316694133,13.2886211592693));
#188749=CARTESIAN_POINT('Ctrl Pts',(16.6172519794773,19.2444233057235,13.2890470865517));
#188750=CARTESIAN_POINT('Ctrl Pts',(16.6176113756265,19.2631994775609,13.2901778764416));
#188751=CARTESIAN_POINT('Ctrl Pts',(16.6179318027065,19.2748824753308,13.2908846455564));
#188752=CARTESIAN_POINT('Ctrl Pts',(16.6198779960648,19.3293736722594,13.2941962897627));
#188753=CARTESIAN_POINT('Ctrl Pts',(16.6227060715008,19.3721263554048,13.2968385334104));
#188754=CARTESIAN_POINT('Ctrl Pts',(16.6340979511182,19.4899338765473,13.3042463177318));
#188755=CARTESIAN_POINT('Ctrl Pts',(16.6453836996307,19.5646562235029,13.309090131725));
#188756=CARTESIAN_POINT('Ctrl Pts',(16.6815642385049,19.7400858193889,13.3207652590004));
#188757=CARTESIAN_POINT('Ctrl Pts',(16.7099064195447,19.8398517871678,13.3276519356594));
#188758=CARTESIAN_POINT('Ctrl Pts',(16.7454193976962,19.9371103140301,13.3344632337298));
#188759=CARTESIAN_POINT('Origin',(18.734,19.211,0.));
#188760=CARTESIAN_POINT('',(16.7430900140495,19.9379407811485,14.3554399645868));
#188761=CARTESIAN_POINT('',(16.7454193878426,19.9371102870445,14.1348940376456));
#188762=CARTESIAN_POINT('',(16.7454193623258,19.9371102171621,0.));
#188763=CARTESIAN_POINT('',(16.6201365181454,19.2114595403695,14.3110918013087));
#188764=CARTESIAN_POINT('Ctrl Pts',(16.6203928462353,19.2114685807018,14.3109441064946));
#188765=CARTESIAN_POINT('Ctrl Pts',(16.6199115541233,19.4590066736441,14.325776059192));
#188766=CARTESIAN_POINT('Ctrl Pts',(16.6606018319505,19.7063940375655,14.3406080118894));
#188767=CARTESIAN_POINT('Ctrl Pts',(16.7430900140495,19.9379407811485,14.3554399645868));
#188768=CARTESIAN_POINT('Ctrl Pts',(16.6170000287543,19.2113489207865,14.3128990289819));
#188769=CARTESIAN_POINT('Ctrl Pts',(16.6169985638862,19.2024611564085,14.3123784634678));
#188770=CARTESIAN_POINT('Ctrl Pts',(16.6170530690492,19.1935735507239,14.3118562095885));
#188771=CARTESIAN_POINT('Ctrl Pts',(16.6172707415281,19.176062414464,14.3108237389372));
#188772=CARTESIAN_POINT('Ctrl Pts',(16.6174306466518,19.1674390346876,14.3103136339808));
#188773=CARTESIAN_POINT('Ctrl Pts',(16.6177963852388,19.1526059883968,14.30943324476));
#188774=CARTESIAN_POINT('Ctrl Pts',(16.617976868931,19.1463957645254,14.3090637552432));
#188775=CARTESIAN_POINT('Ctrl Pts',(16.6183911392897,19.1340179091227,14.3083254924661));
#188776=CARTESIAN_POINT('Ctrl Pts',(16.6186245665655,19.1278503264735,14.3079567340467));
#188777=CARTESIAN_POINT('Ctrl Pts',(16.6191442765127,19.1155429556841,14.3072190479821));
#188778=CARTESIAN_POINT('Ctrl Pts',(16.6194303342871,19.1094032181427,14.3068501309369));
#188779=CARTESIAN_POINT('Ctrl Pts',(16.6202771219087,19.0927853661848,14.3058491121201));
#188780=CARTESIAN_POINT('Ctrl Pts',(16.6208890191119,19.0823101353717,14.3052154108766));
#188781=CARTESIAN_POINT('Ctrl Pts',(16.6234852744379,19.0428994846476,14.3028208456677));
#188782=CARTESIAN_POINT('Ctrl Pts',(16.6259862442916,19.0140023736038,14.3010438784631));
#188783=CARTESIAN_POINT('Ctrl Pts',(16.6533446372121,18.7590033753178,14.2851680809543));
#188784=CARTESIAN_POINT('Ctrl Pts',(16.7139033612549,18.5382508517552,14.2698309810564));
#188785=CARTESIAN_POINT('Ctrl Pts',(16.8323264863085,18.2789845503511,14.251309568682));
#188786=CARTESIAN_POINT('Ctrl Pts',(16.858423151156,18.2275226793277,14.2476192267588));
#188787=CARTESIAN_POINT('Ctrl Pts',(16.892613336978,18.1664253358584,14.2432746839185));
#188788=CARTESIAN_POINT('Ctrl Pts',(16.8987294823071,18.1557165237836,14.2425146347496));
#188789=CARTESIAN_POINT('Ctrl Pts',(16.9075039228619,18.1406603206734,14.2414487404887));
#188790=CARTESIAN_POINT('Ctrl Pts',(16.9100847347766,18.136268379794,14.2411381445089));
#188791=CARTESIAN_POINT('Ctrl Pts',(16.9145399633951,18.1287488880544,14.240606992286));
#188792=CARTESIAN_POINT('Ctrl Pts',(16.9164066454085,18.1256167993642,14.2403859386258));
#188793=CARTESIAN_POINT('Ctrl Pts',(16.9200260111282,18.1195794212297,14.239960220242));
#188794=CARTESIAN_POINT('Ctrl Pts',(16.9217775888977,18.1166735198579,14.23975548322));
#188795=CARTESIAN_POINT('Ctrl Pts',(16.9264891216629,18.1088993304523,14.2392081669173));
#188796=CARTESIAN_POINT('Ctrl Pts',(16.9294617805855,18.1040387190568,14.2388664129858));
#188797=CARTESIAN_POINT('Ctrl Pts',(16.9403739741107,18.0863569031671,14.2376245782977));
#188798=CARTESIAN_POINT('Ctrl Pts',(16.948431034944,18.0736082838159,14.2367318891418));
#188799=CARTESIAN_POINT('Ctrl Pts',(17.041094420383,17.9303995724018,14.2267216463254));
#188800=CARTESIAN_POINT('Ctrl Pts',(17.1397034617471,17.8095366123898,14.2184157408545));
#188801=CARTESIAN_POINT('Ctrl Pts',(17.3440926802485,17.6088174435505,14.2028364393363));
#188802=CARTESIAN_POINT('Ctrl Pts',(17.4458049400079,17.5259542609323,14.1956400440395));
#188803=CARTESIAN_POINT('Ctrl Pts',(17.5686447156221,17.4435369253067,14.1870590286926));
#188804=CARTESIAN_POINT('Ctrl Pts',(17.5828913248143,17.4342255481382,14.1860657803944));
#188805=CARTESIAN_POINT('Ctrl Pts',(17.6055781914815,17.4197851274794,14.1844863127889));
#188806=CARTESIAN_POINT('Ctrl Pts',(17.6139449052986,17.4145415180481,14.1839042903245));
#188807=CARTESIAN_POINT('Ctrl Pts',(17.6282406453183,17.4057207434189,14.1829104659138));
#188808=CARTESIAN_POINT('Ctrl Pts',(17.634151148038,17.4021137554247,14.1824997600373));
#188809=CARTESIAN_POINT('Ctrl Pts',(17.6458191978139,17.3950714519545,14.1816892866909));
#188810=CARTESIAN_POINT('Ctrl Pts',(17.6515755820502,17.3916343611884,14.1812895902028));
#188811=CARTESIAN_POINT('Ctrl Pts',(17.6627560757811,17.3850304208536,14.1805135085188));
#188812=CARTESIAN_POINT('Ctrl Pts',(17.6681781487294,17.3818602488658,14.1801372496098));
#188813=CARTESIAN_POINT('Ctrl Pts',(17.6809345058232,17.3744778522702,14.1792522492826));
#188814=CARTESIAN_POINT('Ctrl Pts',(17.6882800451251,17.3702853814724,14.1787428005507));
#188815=CARTESIAN_POINT('Ctrl Pts',(17.7081126415037,17.3591229434267,14.1773676551297));
#188816=CARTESIAN_POINT('Ctrl Pts',(17.7206453590406,17.3522353939029,14.1764990248226));
#188817=CARTESIAN_POINT('Ctrl Pts',(17.8361885670301,17.2902526914411,14.1684928198603));
#188818=CARTESIAN_POINT('Ctrl Pts',(17.9435076071107,17.2436541817485,14.1610536420035));
#188819=CARTESIAN_POINT('Ctrl Pts',(18.2081745450131,17.1538992397477,14.1427987640214));
#188820=CARTESIAN_POINT('Ctrl Pts',(18.3677477054533,17.1195853421646,14.1318430299218));
#188821=CARTESIAN_POINT('Ctrl Pts',(18.5620752498504,17.1007415976985,14.1194365949179));
#188822=CARTESIAN_POINT('Ctrl Pts',(18.5945457282129,17.0983473025879,14.1173963057822));
#188823=CARTESIAN_POINT('Ctrl Pts',(18.6342938831879,17.0963368716928,14.1149489412328));
#188824=CARTESIAN_POINT('Ctrl Pts',(18.6415292356707,17.0960081283399,14.1145054801349));
#188825=CARTESIAN_POINT('Ctrl Pts',(18.6528732572232,17.0955510295723,14.1138135308002));
#188826=CARTESIAN_POINT('Ctrl Pts',(18.6569807760099,17.0953975007868,14.1135636703893));
#188827=CARTESIAN_POINT('Ctrl Pts',(18.6646584272161,17.0951329191159,14.1130979523566));
#188828=CARTESIAN_POINT('Ctrl Pts',(18.6682283542751,17.095018939467,14.1128819390276));
#188829=CARTESIAN_POINT('Ctrl Pts',(18.6763769916468,17.0947794140561,14.1123900749896));
#188830=CARTESIAN_POINT('Ctrl Pts',(18.6809558226973,17.0946596928605,14.1121145531211));
#188831=CARTESIAN_POINT('Ctrl Pts',(18.6950269312929,17.0943374754427,14.1112704070589));
#188832=CARTESIAN_POINT('Ctrl Pts',(18.7045203619703,17.0941839707978,14.1107044537608));
#188833=CARTESIAN_POINT('Ctrl Pts',(18.8345138804642,17.0929567271269,14.1029998535792));
#188834=CARTESIAN_POINT('Ctrl Pts',(18.9549089011955,17.1021097502756,14.0963869136496));
#188835=CARTESIAN_POINT('Ctrl Pts',(19.1811224308796,17.138905726983,14.0839139817551));
#188836=CARTESIAN_POINT('Ctrl Pts',(19.2868566443039,17.1645783150994,14.0780602696622));
#188837=CARTESIAN_POINT('Ctrl Pts',(19.4610751541079,17.2213729371848,14.0678643344856));
#188838=CARTESIAN_POINT('Ctrl Pts',(19.5307231228407,17.248225250884,14.0636328979163));
#188839=CARTESIAN_POINT('Ctrl Pts',(19.6159165864917,17.2863536376601,14.058182703268));
#188840=CARTESIAN_POINT('Ctrl Pts',(19.6329259778691,17.2942390502606,14.0570805330923));
#188841=CARTESIAN_POINT('Ctrl Pts',(19.6575305587605,17.3060450671416,14.0554647718549));
#188842=CARTESIAN_POINT('Ctrl Pts',(19.6652105839661,17.3097875357469,14.0549573550628));
#188843=CARTESIAN_POINT('Ctrl Pts',(19.6786465125811,17.3164357921098,14.0540641444558));
#188844=CARTESIAN_POINT('Ctrl Pts',(19.6844122209899,17.319321597014,14.0536790528554));
#188845=CARTESIAN_POINT('Ctrl Pts',(19.6955899894651,17.3249802041417,14.0529289624324));
#188846=CARTESIAN_POINT('Ctrl Pts',(19.7010034675988,17.3277500774828,14.0525640694502));
#188847=CARTESIAN_POINT('Ctrl Pts',(19.7139285741416,17.33443379228,14.051688941553));
#188848=CARTESIAN_POINT('Ctrl Pts',(19.7214287510232,17.3383694435991,14.0511779392764));
#188849=CARTESIAN_POINT('Ctrl Pts',(19.7484816468011,17.3527729227139,14.0493230878162));
#188850=CARTESIAN_POINT('Ctrl Pts',(19.7678926558135,17.3635025575156,14.0479699664171));
#188851=CARTESIAN_POINT('Ctrl Pts',(19.9475541077115,17.4665303970982,14.0352324439307));
#188852=CARTESIAN_POINT('Ctrl Pts',(20.09520280444,17.5791337745752,14.0230552601043));
#188853=CARTESIAN_POINT('Ctrl Pts',(20.2430067593528,17.726028210977,14.0092964186109));
#188854=CARTESIAN_POINT('Ctrl Pts',(20.2594180403768,17.7428915441871,14.0077449890224));
#188855=CARTESIAN_POINT('Ctrl Pts',(20.3186161132586,17.8057847687891,14.002068793576));
#188856=CARTESIAN_POINT('Ctrl Pts',(20.3596315623533,17.8534429292961,13.9979771299646));
#188857=CARTESIAN_POINT('Ctrl Pts',(20.4176043013201,17.9272069492926,13.9920244113195));
#188858=CARTESIAN_POINT('Ctrl Pts',(20.4362049778471,17.9519739922684,13.9900855535907));
#188859=CARTESIAN_POINT('Ctrl Pts',(20.4584130420785,17.9829366799419,13.9877430012044));
#188860=CARTESIAN_POINT('Ctrl Pts',(20.4625402568024,17.9887527084451,13.9873064269833));
#188861=CARTESIAN_POINT('Ctrl Pts',(20.4689857649277,17.9979336004706,13.9866228252507));
#188862=CARTESIAN_POINT('Ctrl Pts',(20.4713237969757,18.0012844469532,13.9863744785173));
#188863=CARTESIAN_POINT('Ctrl Pts',(20.4756896475821,18.0075803075503,13.9859100563487));
#188864=CARTESIAN_POINT('Ctrl Pts',(20.4777196827694,18.0105236558754,13.9856938343639));
#188865=CARTESIAN_POINT('Ctrl Pts',(20.4823546752132,18.0172804947185,13.9851995041577));
#188866=CARTESIAN_POINT('Ctrl Pts',(20.4849546131678,18.0210973690328,13.9849217374955));
#188867=CARTESIAN_POINT('Ctrl Pts',(20.4929700073907,18.0329476352,13.984063814347));
#188868=CARTESIAN_POINT('Ctrl Pts',(20.4983429117096,18.0410098465938,13.9834864568677));
#188869=CARTESIAN_POINT('Ctrl Pts',(20.560432242084,18.1355772482507,13.9767841755339));
#188870=CARTESIAN_POINT('Ctrl Pts',(20.6107983341497,18.2261027392679,13.9710449622374));
#188871=CARTESIAN_POINT('Ctrl Pts',(20.7059003031116,18.4310640248381,13.9586949344838));
#188872=CARTESIAN_POINT('Ctrl Pts',(20.7477123368832,18.5464300677828,13.9521325232381));
#188873=CARTESIAN_POINT('Ctrl Pts',(20.7991936628308,18.7391955852769,13.9410475846764));
#188874=CARTESIAN_POINT('Ctrl Pts',(20.8149923820532,18.8146502137216,13.9366836593196));
#188875=CARTESIAN_POINT('Ctrl Pts',(20.8295288347898,18.9096500032595,13.9310737748004));
#188876=CARTESIAN_POINT('Ctrl Pts',(20.8321591821473,18.9285448192748,13.9299525556339));
#188877=CARTESIAN_POINT('Ctrl Pts',(20.8356047515968,18.9560088431102,13.9283139653334));
#188878=CARTESIAN_POINT('Ctrl Pts',(20.836623680787,18.9645518803336,13.9278030208232));
#188879=CARTESIAN_POINT('Ctrl Pts',(20.8383161024586,18.9795168826797,13.9269057291601));
#188880=CARTESIAN_POINT('Ctrl Pts',(20.8390123460334,18.9859361995075,13.9265201044591));
#188881=CARTESIAN_POINT('Ctrl Pts',(20.8403054332555,18.9983895876167,13.9257705509034));
#188882=CARTESIAN_POINT('Ctrl Pts',(20.8409057423918,19.0044232416205,13.9254067352932));
#188883=CARTESIAN_POINT('Ctrl Pts',(20.8422761811924,19.0188251717179,13.924536727758));
#188884=CARTESIAN_POINT('Ctrl Pts',(20.8430224155299,19.0271955701967,13.9240297885932));
#188885=CARTESIAN_POINT('Ctrl Pts',(20.845521892138,19.0572542583132,13.9222045787106));
#188886=CARTESIAN_POINT('Ctrl Pts',(20.8469905259941,19.0789642636854,13.9208774168238));
#188887=CARTESIAN_POINT('Ctrl Pts',(20.857969374078,19.2893818195942,13.9079241119828));
#188888=CARTESIAN_POINT('Ctrl Pts',(20.8425067367764,19.4785067094947,13.8954650998613));
#188889=CARTESIAN_POINT('Ctrl Pts',(20.7855313284336,19.7391928083066,13.877854066994));
#188890=CARTESIAN_POINT('Ctrl Pts',(20.7646863535259,19.8143929180065,13.8727364499377));
#188891=CARTESIAN_POINT('Ctrl Pts',(20.7284012258231,19.9218505807795,13.8655102442454));
#188892=CARTESIAN_POINT('Ctrl Pts',(20.7162220169946,19.9551377662244,13.863284714015));
#188893=CARTESIAN_POINT('Ctrl Pts',(20.7004845905697,19.9950169387015,13.8606473277932));
#188894=CARTESIAN_POINT('Ctrl Pts',(20.6977207776428,20.0019139753075,13.8601922581269));
#188895=CARTESIAN_POINT('Ctrl Pts',(20.6933562019639,20.012641757818,13.8594862543055));
#188896=CARTESIAN_POINT('Ctrl Pts',(20.6917804172114,20.0164825092571,13.8592338567537));
#188897=CARTESIAN_POINT('Ctrl Pts',(20.6888298080599,20.0236143874385,13.8587658944919));
#188898=CARTESIAN_POINT('Ctrl Pts',(20.6874579778568,20.0269066430468,13.8585501589048));
#188899=CARTESIAN_POINT('Ctrl Pts',(20.684328277839,20.0343644696377,13.8580620998532));
#188900=CARTESIAN_POINT('Ctrl Pts',(20.6825653844702,20.0385278753707,13.8577900853234));
#188901=CARTESIAN_POINT('Ctrl Pts',(20.6772936931835,20.050867719686,13.8569851103267));
#188902=CARTESIAN_POINT('Ctrl Pts',(20.6737466217189,20.0590278381891,13.8564544202059));
#188903=CARTESIAN_POINT('Ctrl Pts',(20.6466785540926,20.1202400547811,13.8524840061117));
#188904=CARTESIAN_POINT('Ctrl Pts',(20.6210342341746,20.1723323084205,13.8491644717245));
#188905=CARTESIAN_POINT('Ctrl Pts',(20.5140205871321,20.3688811535557,13.8366262103916));
#188906=CARTESIAN_POINT('Ctrl Pts',(20.4179382785717,20.5046462005304,13.8278931294995));
#188907=CARTESIAN_POINT('Ctrl Pts',(20.2679994187407,20.6711129833437,13.8154666920476));
#188908=CARTESIAN_POINT('Ctrl Pts',(20.2272348983442,20.7127765934001,13.8121887185459));
#188909=CARTESIAN_POINT('Ctrl Pts',(20.1587942861343,20.7771819914443,13.8067884297344));
#188910=CARTESIAN_POINT('Ctrl Pts',(20.132168447394,20.8009967169374,13.8047108534042));
#188911=CARTESIAN_POINT('Ctrl Pts',(20.096596634695,20.831228288282,13.801958322797));
#188912=CARTESIAN_POINT('Ctrl Pts',(20.0881842859716,20.838265868815,13.8013090214884));
#188913=CARTESIAN_POINT('Ctrl Pts',(20.0743656429183,20.8496448705529,13.8002449150705));
#188914=CARTESIAN_POINT('Ctrl Pts',(20.0689919691202,20.854025717733,13.7998317172679));
#188915=CARTESIAN_POINT('Ctrl Pts',(20.0585828277422,20.8624269135181,13.7990324359482));
#188916=CARTESIAN_POINT('Ctrl Pts',(20.0535503280914,20.8664508293669,13.7986465023825));
#188917=CARTESIAN_POINT('Ctrl Pts',(20.0419374411635,20.8756497323686,13.7977570202314));
#188918=CARTESIAN_POINT('Ctrl Pts',(20.0353446031063,20.8808087621923,13.7972528427217));
#188919=CARTESIAN_POINT('Ctrl Pts',(20.0176419186016,20.8944929551246,13.7959010805419));
#188920=CARTESIAN_POINT('Ctrl Pts',(20.0064779339125,20.9029471026187,13.7950507154075));
#188921=CARTESIAN_POINT('Ctrl Pts',(19.9137396982092,20.9717379365629,13.7880029520564));
#188922=CARTESIAN_POINT('Ctrl Pts',(19.8280200849992,21.0262406666247,13.7815808505949));
#188923=CARTESIAN_POINT('Ctrl Pts',(19.588607694157,21.1553316030364,13.763925480567));
#188924=CARTESIAN_POINT('Ctrl Pts',(19.4292598333498,21.2178357167485,13.7524187033296));
#188925=CARTESIAN_POINT('Ctrl Pts',(19.2256143959061,21.2705116569355,13.7389665919713));
#188926=CARTESIAN_POINT('Ctrl Pts',(19.186806933324,21.2793905174442,13.7364598506713));
#188927=CARTESIAN_POINT('Ctrl Pts',(19.1402365375917,21.2886717436491,13.7335370918876));
#188928=CARTESIAN_POINT('Ctrl Pts',(19.1326953608763,21.2901320333729,13.7330664618871));
#188929=CARTESIAN_POINT('Ctrl Pts',(19.1210127556731,21.2923283779349,13.7323416542064));
#188930=CARTESIAN_POINT('Ctrl Pts',(19.1168768911561,21.2930931719736,13.7320858869709));
#188931=CARTESIAN_POINT('Ctrl Pts',(19.1092342581803,21.2944828866384,13.7316148208808));
#188932=CARTESIAN_POINT('Ctrl Pts',(19.1057282191044,21.2951112779483,13.7313993313013));
#188933=CARTESIAN_POINT('Ctrl Pts',(19.0978383904203,21.2965048376505,13.7309157662693));
#188934=CARTESIAN_POINT('Ctrl Pts',(19.0934537780306,21.2972650321804,13.7306479756776));
#188935=CARTESIAN_POINT('Ctrl Pts',(19.0822268559301,21.2991750872931,13.7299646219927));
#188936=CARTESIAN_POINT('Ctrl Pts',(19.0753811703667,21.3003051567227,13.7295501563365));
#188937=CARTESIAN_POINT('Ctrl Pts',(19.03532608813,21.3067152286986,13.7271373403389));
#188938=CARTESIAN_POINT('Ctrl Pts',(19.0019982179598,21.3112373608545,13.7251790415031));
#188939=CARTESIAN_POINT('Ctrl Pts',(18.9504867708261,21.3169804649612,13.7222086286926));
#188940=CARTESIAN_POINT('Ctrl Pts',(18.9323730921317,21.3187638367739,13.7211747773869));
#188941=CARTESIAN_POINT('Ctrl Pts',(18.8831230489343,21.3229721916632,13.7183874391959));
#188942=CARTESIAN_POINT('Ctrl Pts',(18.851951820444,21.3249422220241,13.7166488560521));
#188943=CARTESIAN_POINT('Ctrl Pts',(18.7822823959153,21.3277994377446,13.7127986426394));
#188944=CARTESIAN_POINT('Ctrl Pts',(18.7437805997319,21.3283274470049,13.7106950363509));
#188945=CARTESIAN_POINT('Ctrl Pts',(18.5960098968152,21.3263229053128,13.7026493474654));
#188946=CARTESIAN_POINT('Ctrl Pts',(18.4870146434121,21.3163811067843,13.6967644158466));
#188947=CARTESIAN_POINT('Ctrl Pts',(18.3250242819036,21.2888489864065,13.6876274224407));
#188948=CARTESIAN_POINT('Ctrl Pts',(18.2711535722023,21.2775164140463,13.6845241144869));
#188949=CARTESIAN_POINT('Ctrl Pts',(18.1845502059323,21.2557416764417,13.6793864490267));
#188950=CARTESIAN_POINT('Ctrl Pts',(18.1515216253027,21.2465791182312,13.6773913518622));
#188951=CARTESIAN_POINT('Ctrl Pts',(18.1083928318406,21.2334790274151,13.6747330085138));
#188952=CARTESIAN_POINT('Ctrl Pts',(18.0980786987662,21.2302597250657,13.6740932386801));
#188953=CARTESIAN_POINT('Ctrl Pts',(18.0812217051616,21.2248562685439,13.6730408217615));
#188954=CARTESIAN_POINT('Ctrl Pts',(18.0746639951562,21.2227188182128,13.6726297142945));
#188955=CARTESIAN_POINT('Ctrl Pts',(18.0619874559928,21.218518327695,13.6718316753803));
#188956=CARTESIAN_POINT('Ctrl Pts',(18.0558673834029,21.216459261169,13.6714448789351));
#188957=CARTESIAN_POINT('Ctrl Pts',(18.0417538801784,21.2116388552162,13.6705493437505));
#188958=CARTESIAN_POINT('Ctrl Pts',(18.0337674245437,21.208857566604,13.6700399481599));
#188959=CARTESIAN_POINT('Ctrl Pts',(18.0123241717683,21.201245567273,13.6686650391726));
#188960=CARTESIAN_POINT('Ctrl Pts',(17.9988994734865,21.1963263256404,13.6677965937267));
#188961=CARTESIAN_POINT('Ctrl Pts',(17.8756712562893,21.1497503246915,13.6597526880633));
#188962=CARTESIAN_POINT('Ctrl Pts',(17.7694802719312,21.0991670550833,13.6522722366108));
#188963=CARTESIAN_POINT('Ctrl Pts',(17.5265488643155,20.9575885417094,13.6339019961134));
#188964=CARTESIAN_POINT('Ctrl Pts',(17.395103842211,20.8589888241786,13.6228709531511));
#188965=CARTESIAN_POINT('Ctrl Pts',(17.2538231742291,20.7248459402256,13.6105089000861));
#188966=CARTESIAN_POINT('Ctrl Pts',(17.2317792671371,20.7029738844986,13.6085649599625));
#188967=CARTESIAN_POINT('Ctrl Pts',(17.2052685660834,20.6754863066757,13.6062171421838));
#188968=CARTESIAN_POINT('Ctrl Pts',(17.2003398505197,20.6703239834686,13.6057802132333));
#188969=CARTESIAN_POINT('Ctrl Pts',(17.1926298773146,20.6621663755025,13.6050961813666));
#188970=CARTESIAN_POINT('Ctrl Pts',(17.1898310784468,20.6591878492994,13.6048477565224));
#188971=CARTESIAN_POINT('Ctrl Pts',(17.1846001258868,20.6535885807373,13.6043832683274));
#188972=CARTESIAN_POINT('Ctrl Pts',(17.182166013534,20.650969812821,13.6041670579525));
#188973=CARTESIAN_POINT('Ctrl Pts',(17.1766043192418,20.6449557185223,13.603672858861));
#188974=CARTESIAN_POINT('Ctrl Pts',(17.1734812058476,20.6415563264513,13.6033952110307));
#188975=CARTESIAN_POINT('Ctrl Pts',(17.1638449923011,20.6309985609655,13.6025380204084));
#188976=CARTESIAN_POINT('Ctrl Pts',(17.157369735324,20.6238056051295,13.6019612697349));
#188977=CARTESIAN_POINT('Ctrl Pts',(17.088826019706,20.5466065504134,13.5958448791517));
#188978=CARTESIAN_POINT('Ctrl Pts',(17.0314059727664,20.4725943617997,13.590620166515));
#188979=CARTESIAN_POINT('Ctrl Pts',(16.9052208604029,20.285564457032,13.5782429474349));
#188980=CARTESIAN_POINT('Ctrl Pts',(16.8417781633985,20.1694460029513,13.5711935411569));
#188981=CARTESIAN_POINT('Ctrl Pts',(16.7738052630997,20.011570871112,13.561645681534));
#188982=CARTESIAN_POINT('Ctrl Pts',(16.7590846198133,19.9745349304647,13.5594100760382));
#188983=CARTESIAN_POINT('Ctrl Pts',(16.7454193601307,19.9371102111504,13.5571444941232));
#188984=CARTESIAN_POINT('',(16.61700079985,19.2129106874016,14.0892703927652));
#188985=CARTESIAN_POINT('Ctrl Pts',(16.7454193976962,19.9371103140301,13.3344632337298));
#188986=CARTESIAN_POINT('Ctrl Pts',(16.7539003396954,19.9603368629759,13.3360898566401));
#188987=CARTESIAN_POINT('Ctrl Pts',(16.7627902574051,19.9834204390165,13.3377116742357));
#188988=CARTESIAN_POINT('Ctrl Pts',(16.778326429023,20.0217439766485,13.3404079852639));
#188989=CARTESIAN_POINT('Ctrl Pts',(16.784748055774,20.0370640352716,13.3414868640114));
#188990=CARTESIAN_POINT('Ctrl Pts',(16.8125073017994,20.1011625175549,13.3460009933274));
#188991=CARTESIAN_POINT('Ctrl Pts',(16.8355026337222,20.1492069485804,13.3493852239665));
#188992=CARTESIAN_POINT('Ctrl Pts',(16.8643428899819,20.2040494547763,13.3532075480442));
#188993=CARTESIAN_POINT('Ctrl Pts',(16.8684462585545,20.2117368147759,13.3537423635551));
#188994=CARTESIAN_POINT('Ctrl Pts',(16.8747318906361,20.2233394608875,13.3545478489336));
#188995=CARTESIAN_POINT('Ctrl Pts',(16.8768792570309,20.2272734048751,13.3548206519788));
#188996=CARTESIAN_POINT('Ctrl Pts',(16.8807565588196,20.2343232375642,13.3553089461363));
#188997=CARTESIAN_POINT('Ctrl Pts',(16.8824818758396,20.2374415898167,13.3555247249163));
#188998=CARTESIAN_POINT('Ctrl Pts',(16.8862483451277,20.2442087403399,13.3559925298717));
#188999=CARTESIAN_POINT('Ctrl Pts',(16.8882924274702,20.2478558417629,13.3562443646639));
#189000=CARTESIAN_POINT('Ctrl Pts',(16.8940655501242,20.2580852168319,13.356949976287));
#189001=CARTESIAN_POINT('Ctrl Pts',(16.8978191314054,20.2646536683704,13.3574022049147));
#189002=CARTESIAN_POINT('Ctrl Pts',(16.9204919322803,20.3038400331006,13.3600958525835));
#189003=CARTESIAN_POINT('Ctrl Pts',(16.9402459327431,20.3359700403961,13.362286659183));
#189004=CARTESIAN_POINT('Ctrl Pts',(17.0081356023194,20.4400536240746,13.3693824521066));
#189005=CARTESIAN_POINT('Ctrl Pts',(17.0598276439886,20.5095877029336,13.3741230124526));
#189006=CARTESIAN_POINT('Ctrl Pts',(17.2291757262982,20.7104037404113,13.3884176297891));
#189007=CARTESIAN_POINT('Ctrl Pts',(17.3590578137782,20.8303316478873,13.3978831090112));
#189008=CARTESIAN_POINT('Ctrl Pts',(17.5209471765395,20.9461421760145,13.4094500382727));
#189009=CARTESIAN_POINT('Ctrl Pts',(17.5398248834471,20.959187991588,13.41079438881));
#189010=CARTESIAN_POINT('Ctrl Pts',(17.5668447396273,20.9772187254177,13.4127140848378));
#189011=CARTESIAN_POINT('Ctrl Pts',(17.5748146844975,20.9824596771105,13.4132797849239));
#189012=CARTESIAN_POINT('Ctrl Pts',(17.5878261075909,20.9908904448638,13.4142025612198));
#189013=CARTESIAN_POINT('Ctrl Pts',(17.5928461856283,20.9941131647152,13.41455840437));
#189014=CARTESIAN_POINT('Ctrl Pts',(17.6033862398915,21.0008167816447,13.4153051765537));
#189015=CARTESIAN_POINT('Ctrl Pts',(17.6089088165838,21.0042934544916,13.4156962571728));
#189016=CARTESIAN_POINT('Ctrl Pts',(17.6220913789668,21.0125075176604,13.4166293522862));
#189017=CARTESIAN_POINT('Ctrl Pts',(17.6297656489515,21.0172216397112,13.417172216483));
#189018=CARTESIAN_POINT('Ctrl Pts',(17.6557515302608,21.0329566432197,13.4190094166166));
#189019=CARTESIAN_POINT('Ctrl Pts',(17.6741994219889,21.0437488792938,13.4203120430282));
#189020=CARTESIAN_POINT('Ctrl Pts',(17.7757271191681,21.1010983274128,13.4274744492781));
#189021=CARTESIAN_POINT('Ctrl Pts',(17.8617021116538,21.1422821558589,13.4335232583251));
#189022=CARTESIAN_POINT('Ctrl Pts',(18.1086038735818,21.2406961341987,13.4507947346567));
#189023=CARTESIAN_POINT('Ctrl Pts',(18.2741028532549,21.2844700802679,13.4623042692789));
#189024=CARTESIAN_POINT('Ctrl Pts',(18.4794996868301,21.3129686798259,13.4755392979049));
#189025=CARTESIAN_POINT('Ctrl Pts',(18.5160720245392,21.3170746698919,13.4778537146383));
#189026=CARTESIAN_POINT('Ctrl Pts',(18.5598511791715,21.3208370076898,13.4805595869314));
#189027=CARTESIAN_POINT('Ctrl Pts',(18.5669703010171,21.3214125411374,13.4809975646307));
#189028=CARTESIAN_POINT('Ctrl Pts',(18.5785918386382,21.3222928895063,13.481709065548));
#189029=CARTESIAN_POINT('Ctrl Pts',(18.5830924898715,21.3226193516248,13.4819837584081));
#189030=CARTESIAN_POINT('Ctrl Pts',(18.5911516294114,21.323178036803,13.4824740790997));
#189031=CARTESIAN_POINT('Ctrl Pts',(18.5947096792151,21.3234156606301,13.482690005137));
#189032=CARTESIAN_POINT('Ctrl Pts',(18.6024176376,21.323910875824,13.4831565852709));
#189033=CARTESIAN_POINT('Ctrl Pts',(18.6065676965805,21.3241652315894,13.4834070563076));
#189034=CARTESIAN_POINT('Ctrl Pts',(18.6181652274313,21.3248417508475,13.4841050047214));
#189035=CARTESIAN_POINT('Ctrl Pts',(18.6256143055934,21.3252367859744,13.4845509874819));
#189036=CARTESIAN_POINT('Ctrl Pts',(18.6689407199082,21.327304859428,13.4871323597342));
#189037=CARTESIAN_POINT('Ctrl Pts',(18.70485620256,21.3281041430899,13.4892219208716));
#189038=CARTESIAN_POINT('Ctrl Pts',(18.8205018060836,21.3277339357359,13.4958377530007));
#189039=CARTESIAN_POINT('Ctrl Pts',(18.9001551293929,21.3229752779491,13.5002239971355));
#189040=CARTESIAN_POINT('Ctrl Pts',(19.1643169283449,21.2921518103999,13.5147242045843));
#189041=CARTESIAN_POINT('Ctrl Pts',(19.3456008833673,21.2462650732379,13.5246808646911));
#189042=CARTESIAN_POINT('Ctrl Pts',(19.5390202448045,21.1690902638659,13.5367933152873));
#189043=CARTESIAN_POINT('Ctrl Pts',(19.559368046502,21.1606006283222,13.5380857808929));
#189044=CARTESIAN_POINT('Ctrl Pts',(19.5873252689255,21.1484200319878,13.5398884609172));
#189045=CARTESIAN_POINT('Ctrl Pts',(19.595051174637,21.1449987762264,13.540389497355));
#189046=CARTESIAN_POINT('Ctrl Pts',(19.6082967122084,21.1390381664547,13.5412535248257));
#189047=CARTESIAN_POINT('Ctrl Pts',(19.6138263130478,21.1365211164693,13.5416157477331));
#189048=CARTESIAN_POINT('Ctrl Pts',(19.6252042152479,21.131282701779,13.5423642418551));
#189049=CARTESIAN_POINT('Ctrl Pts',(19.6310510612237,21.1285583433513,13.5427506134777));
#189050=CARTESIAN_POINT('Ctrl Pts',(19.6446293086184,21.1221558191953,13.5436519873502));
#189051=CARTESIAN_POINT('Ctrl Pts',(19.6523509886666,21.1184574074432,13.544167687902));
#189052=CARTESIAN_POINT('Ctrl Pts',(19.6769987187309,21.1064676604585,13.5458239102111));
#189053=CARTESIAN_POINT('Ctrl Pts',(19.6938361957013,21.0979972646336,13.5469706571928));
#189054=CARTESIAN_POINT('Ctrl Pts',(19.7774009929147,21.0545506816856,13.5527406683659));
#189055=CARTESIAN_POINT('Ctrl Pts',(19.8423340491591,21.0162584893286,13.5574803416403));
#189056=CARTESIAN_POINT('Ctrl Pts',(19.9960270681439,20.9142012426487,13.5693363514648));
#189057=CARTESIAN_POINT('Ctrl Pts',(20.0821575241264,20.8468712088598,13.5765525170721));
#189058=CARTESIAN_POINT('Ctrl Pts',(20.173810868615,20.7630503084306,13.5847573911428));
#189059=CARTESIAN_POINT('Ctrl Pts',(20.1848080757816,20.7527754143141,13.5857510360998));
#189060=CARTESIAN_POINT('Ctrl Pts',(20.270733525578,20.6707602058841,13.5935832201779));
#189061=CARTESIAN_POINT('Ctrl Pts',(20.3404157484905,20.5937086994145,13.600357954239));
#189062=CARTESIAN_POINT('Ctrl Pts',(20.410126095196,20.5042069294113,13.6073671091355));
#189063=CARTESIAN_POINT('Ctrl Pts',(20.4160265005179,20.4965231265975,13.6079623404633));
#189064=CARTESIAN_POINT('Ctrl Pts',(20.4246614949996,20.485116963178,13.6088360253738));
#189065=CARTESIAN_POINT('Ctrl Pts',(20.4274368862186,20.4814258498077,13.6091172401474));
#189066=CARTESIAN_POINT('Ctrl Pts',(20.432339644543,20.4748608452034,13.6096146808992));
#189067=CARTESIAN_POINT('Ctrl Pts',(20.4344718292198,20.4719906197009,13.6098312412901));
#189068=CARTESIAN_POINT('Ctrl Pts',(20.4390250091338,20.4658288381279,13.610294171884));
#189069=CARTESIAN_POINT('Ctrl Pts',(20.4414437432643,20.4625356802768,13.6105403855738));
#189070=CARTESIAN_POINT('Ctrl Pts',(20.4480580359774,20.4534753163946,13.6112145628692));
#189071=CARTESIAN_POINT('Ctrl Pts',(20.4522340542121,20.4476938185299,13.6116411926444));
#189072=CARTESIAN_POINT('Ctrl Pts',(20.4743895766033,20.4166916907396,13.6139105560617));
#189073=CARTESIAN_POINT('Ctrl Pts',(20.4918441937073,20.3910984493655,13.6157194443718));
#189074=CARTESIAN_POINT('Ctrl Pts',(20.5978762550671,20.2280505292606,13.6269060181742));
#189075=CARTESIAN_POINT('Ctrl Pts',(20.6708484891867,20.0810900805629,13.6355484850038));
#189076=CARTESIAN_POINT('Ctrl Pts',(20.7660124005701,19.8163750923714,13.6509436360795));
#189077=CARTESIAN_POINT('Ctrl Pts',(20.7965275074375,19.70245531893,13.657513959608));
#189078=CARTESIAN_POINT('Ctrl Pts',(20.8199515684283,19.5725239763471,13.6652483632143));
#189079=CARTESIAN_POINT('Ctrl Pts',(20.8223461988445,19.5584243372723,13.6660905416018));
#189080=CARTESIAN_POINT('Ctrl Pts',(20.8259293856213,19.5359492025367,13.667437993831));
#189081=CARTESIAN_POINT('Ctrl Pts',(20.827210943084,19.5275888236214,13.6679403204371));
#189082=CARTESIAN_POINT('Ctrl Pts',(20.8293825031154,19.5128325088085,13.6688289611689));
#189083=CARTESIAN_POINT('Ctrl Pts',(20.8302934111599,19.5064397242033,13.6692146081685));
#189084=CARTESIAN_POINT('Ctrl Pts',(20.8321167014959,19.4932106891604,13.6700140735056));
#189085=CARTESIAN_POINT('Ctrl Pts',(20.8330249520295,19.4863739551574,13.6704280176326));
#189086=CARTESIAN_POINT('Ctrl Pts',(20.8352700575238,19.4688174645755,13.6714930735985));
#189087=CARTESIAN_POINT('Ctrl Pts',(20.8365582846678,19.4580917895982,13.6721457124233));
#189088=CARTESIAN_POINT('Ctrl Pts',(20.8415887317162,19.4133168067981,13.6748787015432));
#189089=CARTESIAN_POINT('Ctrl Pts',(20.8445861876299,19.3791906109529,13.6769823177131));
#189090=CARTESIAN_POINT('Ctrl Pts',(20.8502353962861,19.2901259962246,13.6825292568718));
#189091=CARTESIAN_POINT('Ctrl Pts',(20.8515764341003,19.2351330748311,13.6860108355322));
#189092=CARTESIAN_POINT('Ctrl Pts',(20.8491826577452,19.070863536987,13.6965697907205));
#189093=CARTESIAN_POINT('Ctrl Pts',(20.8391284433405,18.9618681622872,13.7037955929223));
#189094=CARTESIAN_POINT('Ctrl Pts',(20.8142500506204,18.8163915763883,13.7135450818054));
#189095=CARTESIAN_POINT('Ctrl Pts',(20.8067700065764,18.7788186944954,13.7160714495894));
#189096=CARTESIAN_POINT('Ctrl Pts',(20.7910541040252,18.7097243646693,13.7207138084502));
#189097=CARTESIAN_POINT('Ctrl Pts',(20.7831020828263,18.6781495066885,13.7228338721764));
#189098=CARTESIAN_POINT('Ctrl Pts',(20.7732481429362,18.6425147320147,13.7252166317415));
#189099=CARTESIAN_POINT('Ctrl Pts',(20.7720582439457,18.6382635133447,13.7255007316984));
#189100=CARTESIAN_POINT('Ctrl Pts',(20.7585621250297,18.5906198369151,13.7286826153294));
#189101=CARTESIAN_POINT('Ctrl Pts',(20.7448844327948,18.5476239352467,13.7315352640544));
#189102=CARTESIAN_POINT('Ctrl Pts',(20.7273100167727,18.4979348895437,13.7347840761101));
#189103=CARTESIAN_POINT('Ctrl Pts',(20.7247391459878,18.4907886898145,13.7352501353234));
#189104=CARTESIAN_POINT('Ctrl Pts',(20.7205496049323,18.4793369480718,13.7359949171625));
#189105=CARTESIAN_POINT('Ctrl Pts',(20.7189552890664,18.475022652698,13.7362750290916));
#189106=CARTESIAN_POINT('Ctrl Pts',(20.7160942986645,18.4673575976407,13.7367718040655));
#189107=CARTESIAN_POINT('Ctrl Pts',(20.7148331664703,18.4640048201577,13.7369887931799));
#189108=CARTESIAN_POINT('Ctrl Pts',(20.7121279558111,18.4568679196462,13.7374500241156));
#189109=CARTESIAN_POINT('Ctrl Pts',(20.7106815297367,18.4530847443078,13.7376941229961));
#189110=CARTESIAN_POINT('Ctrl Pts',(20.7067163363,18.4428022119732,13.7383565631728));
#189111=CARTESIAN_POINT('Ctrl Pts',(20.7041762872266,18.4363110395993,13.7387736470407));
#189112=CARTESIAN_POINT('Ctrl Pts',(20.6909685359419,18.4030433674154,13.7409061351704));
#189113=CARTESIAN_POINT('Ctrl Pts',(20.6797862932525,18.3764727937712,13.7425923472838));
#189114=CARTESIAN_POINT('Ctrl Pts',(20.6451739145466,18.2987105960817,13.7475001041646));
#189115=CARTESIAN_POINT('Ctrl Pts',(20.620239819818,18.2482134616489,13.7506519864536));
#189116=CARTESIAN_POINT('Ctrl Pts',(20.5266220544944,18.0762515956244,13.7614589364468));
#189117=CARTESIAN_POINT('Ctrl Pts',(20.447977809262,17.9606282432826,13.7688802422141));
#189118=CARTESIAN_POINT('Ctrl Pts',(20.3015038893652,17.7853316556721,13.7815347066276));
#189119=CARTESIAN_POINT('Ctrl Pts',(20.240240275257,17.7207529912661,13.7865673865744));
#189120=CARTESIAN_POINT('Ctrl Pts',(20.1650751246328,17.65090373097,13.792583393331));
#189121=CARTESIAN_POINT('Ctrl Pts',(20.1549576889409,17.6416830740437,13.7933899720032));
#189122=CARTESIAN_POINT('Ctrl Pts',(20.1385787850756,17.6270441986982,13.794691034061));
#189123=CARTESIAN_POINT('Ctrl Pts',(20.132373610447,17.621563374464,13.7951828827188));
#189124=CARTESIAN_POINT('Ctrl Pts',(20.1212928442631,17.6118912167137,13.7960593990968));
#189125=CARTESIAN_POINT('Ctrl Pts',(20.1164299827331,17.6076854089232,13.7964434581492));
#189126=CARTESIAN_POINT('Ctrl Pts',(20.1062519413445,17.5989633202575,13.7972460828253));
#189127=CARTESIAN_POINT('Ctrl Pts',(20.1009334569397,17.5944510307923,13.7976648062452));
#189128=CARTESIAN_POINT('Ctrl Pts',(20.0870500383865,17.5827896140155,13.7987561329551));
#189129=CARTESIAN_POINT('Ctrl Pts',(20.0784507993602,17.5756818327794,13.7994304111367));
#189130=CARTESIAN_POINT('Ctrl Pts',(20.0407323987774,17.5450039299075,13.8023810371507));
#189131=CARTESIAN_POINT('Ctrl Pts',(20.0110481228621,17.5221423155561,13.8046855355722));
#189132=CARTESIAN_POINT('Ctrl Pts',(19.9304354458203,17.4633985409742,13.8109017915333));
#189133=CARTESIAN_POINT('Ctrl Pts',(19.878506296171,17.4289582442609,13.8148643232619));
#189134=CARTESIAN_POINT('Ctrl Pts',(19.7241741389192,17.3361331764053,13.8265040618338));
#189135=CARTESIAN_POINT('Ctrl Pts',(19.6183212974585,17.2839444868769,13.8343344223526));
#189136=CARTESIAN_POINT('Ctrl Pts',(19.4168669268243,17.2047307756767,13.848593214044));
#189137=CARTESIAN_POINT('Ctrl Pts',(19.3226236843964,17.1750849185475,13.8550208566877));
#189138=CARTESIAN_POINT('Ctrl Pts',(19.2172178562941,17.1498635442951,13.86171714985));
#189139=CARTESIAN_POINT('Ctrl Pts',(19.2077737958847,17.1476722547751,13.8623128189293));
#189140=CARTESIAN_POINT('Ctrl Pts',(19.1938078561854,17.1445327066358,13.8631870213125));
#189141=CARTESIAN_POINT('Ctrl Pts',(19.1892975468645,17.1435342847083,13.8634683204302));
#189142=CARTESIAN_POINT('Ctrl Pts',(19.1812903074939,17.1417892407711,13.863965854421));
#189143=CARTESIAN_POINT('Ctrl Pts',(19.1777947212744,17.1410367077324,13.8641824241736));
#189144=CARTESIAN_POINT('Ctrl Pts',(19.170301431827,17.13944339968,13.8646453128906));
#189145=CARTESIAN_POINT('Ctrl Pts',(19.1663032078698,17.1386053404677,13.8648914756652));
#189146=CARTESIAN_POINT('Ctrl Pts',(19.1553220451363,17.136336764372,13.8655653698979));
#189147=CARTESIAN_POINT('Ctrl Pts',(19.1483341941905,17.1349299178979,13.8659917693912));
#189148=CARTESIAN_POINT('Ctrl Pts',(19.1109978553072,17.1276091073585,13.8682577097136));
#189149=CARTESIAN_POINT('Ctrl Pts',(19.0805279392286,17.1223249154687,13.8700635260463));
#189150=CARTESIAN_POINT('Ctrl Pts',(18.9879673209267,17.1083542481792,13.8754479324895));
#189151=CARTESIAN_POINT('Ctrl Pts',(18.9255935183328,17.1017556732976,13.8789398135878));
#189152=CARTESIAN_POINT('Ctrl Pts',(18.7042738212957,17.0882428403205,13.8911259296222));
#189153=CARTESIAN_POINT('Ctrl Pts',(18.5449519477682,17.0964686433019,13.8995686527687));
#189154=CARTESIAN_POINT('Ctrl Pts',(18.3259805325961,17.1327392627767,13.9120550465058));
#189155=CARTESIAN_POINT('Ctrl Pts',(18.2644032900513,17.1457819947166,13.9156608522928));
#189156=CARTESIAN_POINT('Ctrl Pts',(18.1914221174167,17.1646730608851,13.9200881445245));
#189157=CARTESIAN_POINT('Ctrl Pts',(18.1793703310514,17.1679066049849,13.9208242970885));
#189158=CARTESIAN_POINT('Ctrl Pts',(18.1596372602922,17.1733885336909,13.922038240547));
#189159=CARTESIAN_POINT('Ctrl Pts',(18.1519387870102,17.1755742985697,13.9225139968257));
#189160=CARTESIAN_POINT('Ctrl Pts',(18.138126582831,17.1795806535486,13.923371535924));
#189161=CARTESIAN_POINT('Ctrl Pts',(18.1320083092197,17.1813853337935,13.9237527955555));
#189162=CARTESIAN_POINT('Ctrl Pts',(18.1190018681884,17.185285771294,13.9245663209507));
#189163=CARTESIAN_POINT('Ctrl Pts',(18.112116062618,17.1873890677935,13.9249988296368));
#189164=CARTESIAN_POINT('Ctrl Pts',(18.0936177046689,17.193142796919,13.9261657008433));
#189165=CARTESIAN_POINT('Ctrl Pts',(18.0820258177424,17.1968582889558,13.9269021919542));
#189166=CARTESIAN_POINT('Ctrl Pts',(18.0251375826535,17.2156349563827,13.9305431139578));
#189167=CARTESIAN_POINT('Ctrl Pts',(17.9803305235137,17.2321242264999,13.93349440139));
#189168=CARTESIAN_POINT('Ctrl Pts',(17.7806194787107,17.3133859656406,13.9470404614779));
#189169=CARTESIAN_POINT('Ctrl Pts',(17.6332142049446,17.394925243404,13.9581913930841));
#189170=CARTESIAN_POINT('Ctrl Pts',(17.416849188789,17.5507107443981,13.9757536987232));
#189171=CARTESIAN_POINT('Ctrl Pts',(17.3408135752584,17.613976866279,13.9821893792898));
#189172=CARTESIAN_POINT('Ctrl Pts',(17.2624671936725,17.6890360758549,13.9888929470817));
#189173=CARTESIAN_POINT('Ctrl Pts',(17.2555127444208,17.6957909616849,13.989488618792));
#189174=CARTESIAN_POINT('Ctrl Pts',(17.2453133466887,17.7058347640599,13.9903628242852));
#189175=CARTESIAN_POINT('Ctrl Pts',(17.242032481042,17.7090867992664,13.9906441239097));
#189176=CARTESIAN_POINT('Ctrl Pts',(17.2362310019053,17.7148750675029,13.9911416584608));
#189177=CARTESIAN_POINT('Ctrl Pts',(17.2337061455294,17.7174069710225,13.9913582282698));
#189178=CARTESIAN_POINT('Ctrl Pts',(17.2283104530683,17.7228452110206,13.9918211167355));
#189179=CARTESIAN_POINT('Ctrl Pts',(17.2254416186569,17.7257534553381,13.9920672792045));
#189180=CARTESIAN_POINT('Ctrl Pts',(17.219571729999,17.7317385330182,13.9925710976025));
#189181=CARTESIAN_POINT('Ctrl Pts',(17.2165715894308,17.7348162403675,13.9928286828565));
#189182=CARTESIAN_POINT('Ctrl Pts',(17.2028282053979,17.7490011216773,13.9940091496748));
#189183=CARTESIAN_POINT('Ctrl Pts',(17.1921970803482,17.7602169104497,13.994923679733));
#189184=CARTESIAN_POINT('Ctrl Pts',(17.1270839219106,17.8304352159113,14.0005412505477));
#189185=CARTESIAN_POINT('Ctrl Pts',(17.0758674163161,17.8923880458916,14.0050328575433));
#189186=CARTESIAN_POINT('Ctrl Pts',(16.9870844287355,18.0131623280466,14.0132735216999));
#189187=CARTESIAN_POINT('Ctrl Pts',(16.9486652663682,18.0712152024473,14.017036525318));
#189188=CARTESIAN_POINT('Ctrl Pts',(16.8366942178351,18.2600025000754,14.0289657726126));
#189189=CARTESIAN_POINT('Ctrl Pts',(16.7741390012416,18.3966891816244,14.037197792598));
#189190=CARTESIAN_POINT('Ctrl Pts',(16.7220478750628,18.5522600454468,14.0468105579356));
#189191=CARTESIAN_POINT('Ctrl Pts',(16.7176849722239,18.5657377471158,14.0476448800404));
#189192=CARTESIAN_POINT('Ctrl Pts',(16.7109454564795,18.5872931858504,14.0489821065602));
#189193=CARTESIAN_POINT('Ctrl Pts',(16.7084811540861,18.5953432142828,14.04948213411));
#189194=CARTESIAN_POINT('Ctrl Pts',(16.7042134851124,18.6095872305298,14.0503681000156));
#189195=CARTESIAN_POINT('Ctrl Pts',(16.7023902813161,18.6157751980733,14.0507533841226));
#189196=CARTESIAN_POINT('Ctrl Pts',(16.6986719539506,18.6286113546009,14.0515534710001));
#189197=CARTESIAN_POINT('Ctrl Pts',(16.6967810570501,18.6352606787376,14.0519684063414));
#189198=CARTESIAN_POINT('Ctrl Pts',(16.6919990650989,18.6523950626001,14.0530389220398));
#189199=CARTESIAN_POINT('Ctrl Pts',(16.6891561701449,18.6628932596528,14.0536960597197));
#189200=CARTESIAN_POINT('Ctrl Pts',(16.6831808523557,18.6856525316541,14.055123505956));
#189201=CARTESIAN_POINT('Ctrl Pts',(16.6800772339591,18.6979206698156,14.0558947188747));
#189202=CARTESIAN_POINT('Ctrl Pts',(16.6713661332148,18.7337005525461,14.0581493256177));
#189203=CARTESIAN_POINT('Ctrl Pts',(16.6660512434075,18.7572808182923,14.0596419400709));
#189204=CARTESIAN_POINT('Ctrl Pts',(16.631655751107,18.9230670248615,14.0701853398582));
#189205=CARTESIAN_POINT('Ctrl Pts',(16.6168699503979,19.0678169686808,14.0796830582003));
#189206=CARTESIAN_POINT('Ctrl Pts',(16.6170008616904,19.2129100775731,14.0892704606451));
#189207=CARTESIAN_POINT('Ctrl Pts',(16.6170008622342,19.2129106802283,14.0892705004671));
#189208=CARTESIAN_POINT('Ctrl Pts',(16.6171115220818,19.3355197900838,14.0973722145855));
#189209=CARTESIAN_POINT('Ctrl Pts',(16.627873578249,19.4579019708157,14.1054939081815));
#189210=CARTESIAN_POINT('Ctrl Pts',(16.6513555158085,19.5910511198309,14.1139585279377));
#189211=CARTESIAN_POINT('Ctrl Pts',(16.6536481259094,19.6034066737466,14.1147402688335));
#189212=CARTESIAN_POINT('Ctrl Pts',(16.6573287572654,19.6223030987319,14.1159293748916));
#189213=CARTESIAN_POINT('Ctrl Pts',(16.6586379331589,19.6288588082238,14.1163407108087));
#189214=CARTESIAN_POINT('Ctrl Pts',(16.6608486766564,19.6396623911444,14.1170164748051));
#189215=CARTESIAN_POINT('Ctrl Pts',(16.661732288431,19.6439138337036,14.1172818639948));
#189216=CARTESIAN_POINT('Ctrl Pts',(16.6634789761593,19.6521900187716,14.1177974009758));
#189217=CARTESIAN_POINT('Ctrl Pts',(16.6643407213195,19.6562150195898,14.1180476216642));
#189218=CARTESIAN_POINT('Ctrl Pts',(16.665971986405,19.6637271660026,14.1185136530072));
#189219=CARTESIAN_POINT('Ctrl Pts',(16.6667385816777,19.6672148401818,14.1187296215364));
#189220=CARTESIAN_POINT('Ctrl Pts',(16.6685067296659,19.6751631716213,14.119220920855));
#189221=CARTESIAN_POINT('Ctrl Pts',(16.6695139067983,19.6796225256659,14.1194959257347));
#189222=CARTESIAN_POINT('Ctrl Pts',(16.6726472977642,19.6932896848048,14.1203369169667));
#189223=CARTESIAN_POINT('Ctrl Pts',(16.6748207595118,19.7024866896663,14.1209002613306));
#189224=CARTESIAN_POINT('Ctrl Pts',(16.6956478218852,19.7880524097973,14.1261199400262));
#189225=CARTESIAN_POINT('Ctrl Pts',(16.7184739237694,19.8633153988605,14.1305523033505));
#189226=CARTESIAN_POINT('Ctrl Pts',(16.7454193878426,19.9371102870445,14.1348940376456));
#189227=CARTESIAN_POINT('Origin',(18.734,19.211,0.));
#189228=CARTESIAN_POINT('',(16.7454193623258,19.9371102171621,15.155594536163));
#189229=CARTESIAN_POINT('',(16.7454193857226,19.9371102812384,14.9318514580964));
#189230=CARTESIAN_POINT('',(16.7454193623258,19.9371102171621,0.));
#189231=CARTESIAN_POINT('',(16.6156459487826,19.212740575031,15.1109429532718));
#189232=CARTESIAN_POINT('Ctrl Pts',(16.6170007251258,19.2127521935258,15.1109437209775));
#189233=CARTESIAN_POINT('Ctrl Pts',(16.6170993834537,19.3319511321298,15.1181312937192));
#189234=CARTESIAN_POINT('Ctrl Pts',(16.6272689227094,19.4507453566806,15.1253188664609));
#189235=CARTESIAN_POINT('Ctrl Pts',(16.6472858251195,19.5678094062,15.1325064392026));
#189236=CARTESIAN_POINT('Ctrl Pts',(16.659503668485,19.6392625307373,15.1368935634507));
#189237=CARTESIAN_POINT('Ctrl Pts',(16.675419638095,19.7102268266389,15.1412806876989));
#189238=CARTESIAN_POINT('Ctrl Pts',(16.6949811994265,19.7802901992024,15.145667811947));
#189239=CARTESIAN_POINT('Ctrl Pts',(16.7097351486035,19.833134214077,15.148976720019));
#189240=CARTESIAN_POINT('Ctrl Pts',(16.7265618764294,19.8854656727906,15.152285628091));
#189241=CARTESIAN_POINT('Ctrl Pts',(16.7454193623258,19.9371102171621,15.155594536163));
#189242=CARTESIAN_POINT('Ctrl Pts',(16.7430900140495,19.9379407811485,14.3554399645868));
#189243=CARTESIAN_POINT('Ctrl Pts',(16.7690653364714,20.0108542721151,14.3601105094292));
#189244=CARTESIAN_POINT('Ctrl Pts',(17.0725680194683,20.7297352289216,14.407172989832));
#189245=CARTESIAN_POINT('Ctrl Pts',(18.453125516026,21.6984565773648,14.4966274057954));
#189246=CARTESIAN_POINT('Ctrl Pts',(20.6735253020556,20.7935840586525,14.6238032124768));
#189247=CARTESIAN_POINT('Ctrl Pts',(21.114531003966,18.4367888923735,14.7509790191583));
#189248=CARTESIAN_POINT('Ctrl Pts',(19.3715472621554,16.7902843643798,14.8781548258396));
#189249=CARTESIAN_POINT('Ctrl Pts',(17.1752233264884,17.3321744887536,14.9981428038775));
#189250=CARTESIAN_POINT('Ctrl Pts',(16.6208559023486,18.6285361102004,15.0757388463549));
#189251=CARTESIAN_POINT('Ctrl Pts',(16.6156459487826,19.212740575031,15.1109429532718));
#189252=CARTESIAN_POINT('Ctrl Pts',(16.7454193878426,19.9371102870445,14.1348940376456));
#189253=CARTESIAN_POINT('Ctrl Pts',(16.7604972143715,19.9784035644483,14.1373235343638));
#189254=CARTESIAN_POINT('Ctrl Pts',(16.7768648728234,20.0192371694941,14.1397244633557));
#189255=CARTESIAN_POINT('Ctrl Pts',(16.8230771657304,20.124862769637,14.1459966983079));
#189256=CARTESIAN_POINT('Ctrl Pts',(16.8549327852444,20.1886898818392,14.1498507198238));
#189257=CARTESIAN_POINT('Ctrl Pts',(16.9337290706316,20.3284343335731,14.1586405514275));
#189258=CARTESIAN_POINT('Ctrl Pts',(16.9823674089659,20.4032314873514,14.1635988479836));
#189259=CARTESIAN_POINT('Ctrl Pts',(17.0559411465615,20.5021126425508,14.1706897807959));
#189260=CARTESIAN_POINT('Ctrl Pts',(17.0769686928333,20.5289910565066,14.1726760533279));
#189261=CARTESIAN_POINT('Ctrl Pts',(17.1055473282265,20.5637562066665,14.1753299197156));
#189262=CARTESIAN_POINT('Ctrl Pts',(17.1125235035304,20.5721103642186,14.1759743089135));
#189263=CARTESIAN_POINT('Ctrl Pts',(17.1240365248426,20.5856833893665,14.1770323897217));
#189264=CARTESIAN_POINT('Ctrl Pts',(17.1285351250224,20.5909345440311,14.1774445090444));
#189265=CARTESIAN_POINT('Ctrl Pts',(17.1372798274166,20.6010414733071,14.1782431375107));
#189266=CARTESIAN_POINT('Ctrl Pts',(17.1415225602354,20.6059000714965,14.1786295043654));
#189267=CARTESIAN_POINT('Ctrl Pts',(17.1513511886196,20.6170521146089,14.1795220529518));
#189268=CARTESIAN_POINT('Ctrl Pts',(17.1569525081977,20.6233317650491,14.1800288777588));
#189269=CARTESIAN_POINT('Ctrl Pts',(17.1720744996244,20.640082931504,14.1813923661629));
#189270=CARTESIAN_POINT('Ctrl Pts',(17.1816628618323,20.6504925105874,14.1822518865271));
#189271=CARTESIAN_POINT('Ctrl Pts',(17.2658131808938,20.7400315153285,14.1897533493696));
#189272=CARTESIAN_POINT('Ctrl Pts',(17.3462525661143,20.8133921541756,14.1966548188598));
#189273=CARTESIAN_POINT('Ctrl Pts',(17.5089838418746,20.9403256574057,14.2100930077399));
#189274=CARTESIAN_POINT('Ctrl Pts',(17.590073873907,20.9950020741772,14.2165775281884));
#189275=CARTESIAN_POINT('Ctrl Pts',(17.7368998283904,21.0798634730265,14.2277552108006));
#189276=CARTESIAN_POINT('Ctrl Pts',(17.8009525811308,21.11265280255,14.2324604630758));
#189277=CARTESIAN_POINT('Ctrl Pts',(17.89726551958,21.1559159188901,14.239177042908));
#189278=CARTESIAN_POINT('Ctrl Pts',(17.9283039878583,21.1689777206307,14.2412890188647));
#189279=CARTESIAN_POINT('Ctrl Pts',(17.966423615382,21.1839593447083,14.2438082347667));
#189280=CARTESIAN_POINT('Ctrl Pts',(17.9732182939624,21.1865893503975,14.2442544297581));
#189281=CARTESIAN_POINT('Ctrl Pts',(17.9839067656961,21.19066319947,14.244951711349));
#189282=CARTESIAN_POINT('Ctrl Pts',(17.987791385608,21.1921307246054,14.2452041790916));
#189283=CARTESIAN_POINT('Ctrl Pts',(17.9950204383038,21.1948374247086,14.2456722045895));
#189284=CARTESIAN_POINT('Ctrl Pts',(17.9983636520336,21.1960795661886,14.2458879336391));
#189285=CARTESIAN_POINT('Ctrl Pts',(18.0059506888618,21.1988766630714,14.2463758926936));
#189286=CARTESIAN_POINT('Ctrl Pts',(18.0101963513963,21.200426476694,14.246647814292));
#189287=CARTESIAN_POINT('Ctrl Pts',(18.0228078148333,21.2049843805099,14.2474522596417));
#189288=CARTESIAN_POINT('Ctrl Pts',(18.0311877564427,21.2079534272303,14.2479825174769));
#189289=CARTESIAN_POINT('Ctrl Pts',(18.0942142684581,21.2298380896441,14.2519404117078));
#189290=CARTESIAN_POINT('Ctrl Pts',(18.1496018238592,21.2465620977439,14.2552487130249));
#189291=CARTESIAN_POINT('Ctrl Pts',(18.3636351368334,21.30172952605,14.2676340742042));
#189292=CARTESIAN_POINT('Ctrl Pts',(18.525845624908,21.3240542411295,14.2762395421047));
#189293=CARTESIAN_POINT('Ctrl Pts',(18.7490765715584,21.3287984505572,14.288607272365));
#189294=CARTESIAN_POINT('Ctrl Pts',(18.8091576894109,21.3275179188448,14.291982319262));
#189295=CARTESIAN_POINT('Ctrl Pts',(18.8932438317346,21.3221408546444,14.2968207419258));
#189296=CARTESIAN_POINT('Ctrl Pts',(18.9173586424913,21.3201832179767,14.2982215052839));
#189297=CARTESIAN_POINT('Ctrl Pts',(18.959416452345,21.3160422629032,14.3006905156906));
#189298=CARTESIAN_POINT('Ctrl Pts',(18.9773751301975,21.3140416119535,14.3017530881889));
#189299=CARTESIAN_POINT('Ctrl Pts',(19.0037769080168,21.3107576748974,14.3033283026308));
#189300=CARTESIAN_POINT('Ctrl Pts',(19.0122416728109,21.3096527682407,14.3038353223592));
#189301=CARTESIAN_POINT('Ctrl Pts',(19.0270866000763,21.3076236674702,14.3047280746367));
#189302=CARTESIAN_POINT('Ctrl Pts',(19.0334696937367,21.3067214650938,14.305113107244));
#189303=CARTESIAN_POINT('Ctrl Pts',(19.0458676887262,21.3049113036467,14.3058632622771));
#189304=CARTESIAN_POINT('Ctrl Pts',(19.0518829990925,21.304006545737,14.3062282797058));
#189305=CARTESIAN_POINT('Ctrl Pts',(19.0662722041711,21.3017788152655,14.3071039973782));
#189306=CARTESIAN_POINT('Ctrl Pts',(19.0746421661294,21.3004314497996,14.3076154673089));
#189307=CARTESIAN_POINT('Ctrl Pts',(19.104927350662,21.2953694428493,14.3094737956557));
#189308=CARTESIAN_POINT('Ctrl Pts',(19.1267912246479,21.2913600814466,14.3108299716777));
#189309=CARTESIAN_POINT('Ctrl Pts',(19.3294001659426,21.2508982346035,14.3235375821658));
#189310=CARTESIAN_POINT('Ctrl Pts',(19.5046886100218,21.1913277891537,14.3356764651532));
#189311=CARTESIAN_POINT('Ctrl Pts',(19.7426167457967,21.074044525038,14.3531918001493));
#189312=CARTESIAN_POINT('Ctrl Pts',(19.8131208857484,21.0341134080646,14.358512757353));
#189313=CARTESIAN_POINT('Ctrl Pts',(19.9116319769776,20.9705981750519,14.3659859985934));
#189314=CARTESIAN_POINT('Ctrl Pts',(19.9415882031334,20.9501762149821,14.3682635995435));
#189315=CARTESIAN_POINT('Ctrl Pts',(19.9770768281583,20.924623336678,14.3709540966073));
#189316=CARTESIAN_POINT('Ctrl Pts',(19.9831233942394,20.9202207846012,14.3714122236791));
#189317=CARTESIAN_POINT('Ctrl Pts',(19.9924983189658,20.9133185085879,14.3721219254567));
#189318=CARTESIAN_POINT('Ctrl Pts',(19.9958427830626,20.9108409087447,14.3723749879964));
#189319=CARTESIAN_POINT('Ctrl Pts',(20.0020387222181,20.9062225553543,14.3728435521985));
#189320=CARTESIAN_POINT('Ctrl Pts',(20.0048920692146,20.9040844816232,14.3730592286806));
#189321=CARTESIAN_POINT('Ctrl Pts',(20.0113396124558,20.8992277165988,14.3735463528807));
#189322=CARTESIAN_POINT('Ctrl Pts',(20.0149305281977,20.8965047586509,14.3738174966156));
#189323=CARTESIAN_POINT('Ctrl Pts',(20.0257640163184,20.8882352084294,14.3746351309585));
#189324=CARTESIAN_POINT('Ctrl Pts',(20.0329795673664,20.8826531663523,14.3751791886612));
#189325=CARTESIAN_POINT('Ctrl Pts',(20.0884676587009,20.8391506455105,14.3793609384994));
#189326=CARTESIAN_POINT('Ctrl Pts',(20.1351111125707,20.7991896299486,14.3828640790201));
#189327=CARTESIAN_POINT('Ctrl Pts',(20.2872053214426,20.6569610465483,14.3945009486614));
#189328=CARTESIAN_POINT('Ctrl Pts',(20.3837334068908,20.545778771863,14.402287180207));
#189329=CARTESIAN_POINT('Ctrl Pts',(20.5211937784511,20.3495214445373,14.4154842682804));
#189330=CARTESIAN_POINT('Ctrl Pts',(20.5693504592298,20.2701404504339,14.4206926457152));
#189331=CARTESIAN_POINT('Ctrl Pts',(20.6218690633925,20.1691667601624,14.4273222593103));
#189332=CARTESIAN_POINT('Ctrl Pts',(20.631313697697,20.1503262617893,14.4285591337442));
#189333=CARTESIAN_POINT('Ctrl Pts',(20.6443687918004,20.1232830094818,14.43033565602));
#189334=CARTESIAN_POINT('Ctrl Pts',(20.648211075904,20.1151931006188,14.4308672380318));
#189335=CARTESIAN_POINT('Ctrl Pts',(20.6547602396822,20.1011750215481,14.431788700917));
#189336=CARTESIAN_POINT('Ctrl Pts',(20.6574913121641,20.0952582416335,14.4321777391962));
#189337=CARTESIAN_POINT('Ctrl Pts',(20.6626744793243,20.0838914409243,14.4329253664322));
#189338=CARTESIAN_POINT('Ctrl Pts',(20.665130903714,20.078443454306,14.4332838016399));
#189339=CARTESIAN_POINT('Ctrl Pts',(20.6714720421519,20.064219313838,14.4342199512762));
#189340=CARTESIAN_POINT('Ctrl Pts',(20.6753201696147,20.0554270873963,14.4347989125022));
#189341=CARTESIAN_POINT('Ctrl Pts',(20.6883060531377,20.025198898276,14.4367906465426));
#189342=CARTESIAN_POINT('Ctrl Pts',(20.6971493465552,20.003638991163,14.4382133624897));
#189343=CARTESIAN_POINT('Ctrl Pts',(20.7678866049364,19.8227320909607,14.4501731186814));
#189344=CARTESIAN_POINT('Ctrl Pts',(20.8106148721748,19.6566005100543,14.4613734082948));
#189345=CARTESIAN_POINT('Ctrl Pts',(20.8446793431816,19.3977183482818,14.4786282361314));
#189346=CARTESIAN_POINT('Ctrl Pts',(20.8507199811218,19.3075895787221,14.484583226353));
#189347=CARTESIAN_POINT('Ctrl Pts',(20.8511062726947,19.1787193877652,14.4928166728075));
#189348=CARTESIAN_POINT('Ctrl Pts',(20.8501648825973,19.1400942021931,14.4952476772599));
#189349=CARTESIAN_POINT('Ctrl Pts',(20.8477729843692,19.0939069184367,14.4980939209036));
#189350=CARTESIAN_POINT('Ctrl Pts',(20.8473379908568,19.0863021265278,14.4985605813137));
#189351=CARTESIAN_POINT('Ctrl Pts',(20.8465999732367,19.0745158377066,14.4992805959177));
#189352=CARTESIAN_POINT('Ctrl Pts',(20.8463255634644,19.0703327041752,14.4995355070597));
#189353=CARTESIAN_POINT('Ctrl Pts',(20.8457949434644,19.0625957841527,14.5000057723232));
#189354=CARTESIAN_POINT('Ctrl Pts',(20.8455421895321,19.059041858863,14.5002213121567));
#189355=CARTESIAN_POINT('Ctrl Pts',(20.8449522950971,19.051033238101,14.5007059632867));
#189356=CARTESIAN_POINT('Ctrl Pts',(20.8446100266102,19.0465789748788,14.5009747838381));
#189357=CARTESIAN_POINT('Ctrl Pts',(20.843563909036,19.0335066808487,14.5017616442111));
#189358=CARTESIAN_POINT('Ctrl Pts',(20.8428213482075,19.0248917202775,14.5022775627819));
#189359=CARTESIAN_POINT('Ctrl Pts',(20.8372752150151,18.964849217182,14.5058563574091));
#189360=CARTESIAN_POINT('Ctrl Pts',(20.8306432958255,18.9136035268714,14.5088242564961));
#189361=CARTESIAN_POINT('Ctrl Pts',(20.8185587170377,18.8411644650598,14.5129602940516));
#189362=CARTESIAN_POINT('Ctrl Pts',(20.8146434144928,18.8197374352134,14.5141762363956));
#189363=CARTESIAN_POINT('Ctrl Pts',(20.8014003898098,18.7530964554045,14.517944796383));
#189364=CARTESIAN_POINT('Ctrl Pts',(20.7909238744259,18.7081238241341,14.5204691490588));
#189365=CARTESIAN_POINT('Ctrl Pts',(20.750705117285,18.5578936011013,14.5289363664688));
#189366=CARTESIAN_POINT('Ctrl Pts',(20.7142828992118,18.4546097208712,14.5348247083245));
#189367=CARTESIAN_POINT('Ctrl Pts',(20.6477506747621,18.3042005970275,14.5439696297338));
#189368=CARTESIAN_POINT('Ctrl Pts',(20.6234958178143,18.2546884862718,14.5470774815972));
#189369=CARTESIAN_POINT('Ctrl Pts',(20.5810528677671,18.1759821691211,14.5522219984525));
#189370=CARTESIAN_POINT('Ctrl Pts',(20.5640366496115,18.1461845836009,14.5542192656255));
#189371=CARTESIAN_POINT('Ctrl Pts',(20.5407177317513,18.1075613395594,14.5568800902988));
#189372=CARTESIAN_POINT('Ctrl Pts',(20.5350601991422,18.0983509124228,14.5575201154625));
#189373=CARTESIAN_POINT('Ctrl Pts',(20.5256770208314,18.0833342521811,14.5585728453291));
#189374=CARTESIAN_POINT('Ctrl Pts',(20.5219930462904,18.0775021171327,14.5589840086147));
#189375=CARTESIAN_POINT('Ctrl Pts',(20.5148057898733,18.0662461272976,14.559782079353));
#189376=CARTESIAN_POINT('Ctrl Pts',(20.5113060651028,18.0608200837132,14.5601688513989));
#189377=CARTESIAN_POINT('Ctrl Pts',(20.5031665841553,18.0483263239681,14.5610642185907));
#189378=CARTESIAN_POINT('Ctrl Pts',(20.4985092253758,18.0412702578144,14.5615734698135));
#189379=CARTESIAN_POINT('Ctrl Pts',(20.4858668762618,18.0223639607299,14.5629477367285));
#189380=CARTESIAN_POINT('Ctrl Pts',(20.4778040713471,18.0105665236953,14.5638156802129));
#189381=CARTESIAN_POINT('Ctrl Pts',(20.4027425004075,17.9030891019998,14.5718202668842));
#189382=CARTESIAN_POINT('Ctrl Pts',(20.3280628690436,17.8130414095241,14.5792584531675));
#189383=CARTESIAN_POINT('Ctrl Pts',(20.1325800434948,17.6134714021885,14.5975057709115));
#189384=CARTESIAN_POINT('Ctrl Pts',(20.0058105106286,17.5108171169729,14.6084546176039));
#189385=CARTESIAN_POINT('Ctrl Pts',(19.8409605862959,17.4061746413851,14.6208636027602));
#189386=CARTESIAN_POINT('Ctrl Pts',(19.812975107256,17.3893059244252,14.6229114311541));
#189387=CARTESIAN_POINT('Ctrl Pts',(19.7783138858032,17.3694924436913,14.6253665638587));
#189388=CARTESIAN_POINT('Ctrl Pts',(19.7720005558519,17.3659264454829,14.625810521068));
#189389=CARTESIAN_POINT('Ctrl Pts',(19.7620781584199,17.3603889631995,14.6265030714428));
#189390=CARTESIAN_POINT('Ctrl Pts',(19.7584815252342,17.3583954781264,14.6267530406308));
#189391=CARTESIAN_POINT('Ctrl Pts',(19.7517502412579,17.3546901653239,14.6272188530325));
#189392=CARTESIAN_POINT('Ctrl Pts',(19.7486171013658,17.3529758091606,14.6274348526086));
#189393=CARTESIAN_POINT('Ctrl Pts',(19.7414581821826,17.3490821805475,14.6279265451391));
#189394=CARTESIAN_POINT('Ctrl Pts',(19.7374296714904,17.3469080359281,14.6282019101421));
#189395=CARTESIAN_POINT('Ctrl Pts',(19.7250361550998,17.340271204371,14.6290450983701));
#189396=CARTESIAN_POINT('Ctrl Pts',(19.7166480648367,17.3358515590098,14.6296102594921));
#189397=CARTESIAN_POINT('Ctrl Pts',(19.6008140049927,17.2758098669582,14.6373429789495));
#189398=CARTESIAN_POINT('Ctrl Pts',(19.4888054223823,17.2294337726252,14.6439804904632));
#189399=CARTESIAN_POINT('Ctrl Pts',(19.2028074076327,17.1388164595042,14.6603064442245));
#189400=CARTESIAN_POINT('Ctrl Pts',(19.0260361577631,17.1066157992238,14.6699251213358));
#189401=CARTESIAN_POINT('Ctrl Pts',(18.8258763569788,17.095885544681,14.6815960719128));
#189402=CARTESIAN_POINT('Ctrl Pts',(18.8044107246304,17.0950622164254,14.6828564264813));
#189403=CARTESIAN_POINT('Ctrl Pts',(18.7739144023739,17.0943570711024,14.6846608155752));
#189404=CARTESIAN_POINT('Ctrl Pts',(18.7648908279094,17.0942061505949,14.6851964289294));
#189405=CARTESIAN_POINT('Ctrl Pts',(18.7493378522245,17.0940454940435,14.6861226633269));
#189406=CARTESIAN_POINT('Ctrl Pts',(18.7428088153607,17.0940082585661,14.6865124179165));
#189407=CARTESIAN_POINT('Ctrl Pts',(18.7303180253619,17.0939948074078,14.687259876628));
#189408=CARTESIAN_POINT('Ctrl Pts',(18.724356331665,17.0940135709149,14.6876174195645));
#189409=CARTESIAN_POINT('Ctrl Pts',(18.7088771923133,17.0941276762297,14.6885478454648));
#189410=CARTESIAN_POINT('Ctrl Pts',(18.6993602465038,17.0942620205937,14.6891219453611));
#189411=CARTESIAN_POINT('Ctrl Pts',(18.6670303135265,17.094936489238,14.691079358234));
#189412=CARTESIAN_POINT('Ctrl Pts',(18.6442259007512,17.0957812719165,14.692472157627));
#189413=CARTESIAN_POINT('Ctrl Pts',(18.4439242815153,17.1064462841869,14.704816458693));
#189414=CARTESIAN_POINT('Ctrl Pts',(18.2683373918396,17.1382182293484,14.7164925055961));
#189415=CARTESIAN_POINT('Ctrl Pts',(18.0173335117221,17.2171654974175,14.7338754502794));
#189416=CARTESIAN_POINT('Ctrl Pts',(17.9374624467102,17.2477076936566,14.7395017557208));
#189417=CARTESIAN_POINT('Ctrl Pts',(17.825572944194,17.2984494866377,14.7473429539149));
#189418=CARTESIAN_POINT('Ctrl Pts',(17.7919077578619,17.3148059732196,14.7496960767993));
#189419=CARTESIAN_POINT('Ctrl Pts',(17.7519919166439,17.3355250989737,14.7524633809533));
#189420=CARTESIAN_POINT('Ctrl Pts',(17.7453107263425,17.3390385943472,14.7529257947244));
#189421=CARTESIAN_POINT('Ctrl Pts',(17.734961658416,17.3445518113027,14.7536406786902));
#189422=CARTESIAN_POINT('Ctrl Pts',(17.7312807435796,17.3465267385811,14.7538946712706));
#189423=CARTESIAN_POINT('Ctrl Pts',(17.7244699981977,17.3502069221203,14.7543640863437));
#189424=CARTESIAN_POINT('Ctrl Pts',(17.7213386561767,17.3519091721371,14.7545796891481));
#189425=CARTESIAN_POINT('Ctrl Pts',(17.7142752507894,17.3557720990114,14.755065546715));
#189426=CARTESIAN_POINT('Ctrl Pts',(17.7103457591595,17.3579373661908,14.7553355042486));
#189427=CARTESIAN_POINT('Ctrl Pts',(17.6987856733985,17.3643553108406,14.7561287911656));
#189428=CARTESIAN_POINT('Ctrl Pts',(17.6911743767624,17.3686428045925,14.7566499469768));
#189429=CARTESIAN_POINT('Ctrl Pts',(17.6369037670882,17.3996578786581,14.7603592321784));
#189430=CARTESIAN_POINT('Ctrl Pts',(17.5912470071207,17.4281099125443,14.7634443325496));
#189431=CARTESIAN_POINT('Ctrl Pts',(17.4071720816061,17.5528004539388,14.7759434097013));
#189432=CARTESIAN_POINT('Ctrl Pts',(17.2794066307537,17.6636590734693,14.7848132797346));
#189433=CARTESIAN_POINT('Ctrl Pts',(17.1115465609669,17.8486733009475,14.7986576607972));
#189434=CARTESIAN_POINT('Ctrl Pts',(17.0604711570531,17.9119278994138,14.8032487695533));
#189435=CARTESIAN_POINT('Ctrl Pts',(17.0017259928095,17.9939128590848,14.8091326233095));
#189436=CARTESIAN_POINT('Ctrl Pts',(16.9905152033967,18.0100274481658,14.8102859094099));
#189437=CARTESIAN_POINT('Ctrl Pts',(16.9746597466664,18.0335083332383,14.8119628576744));
#189438=CARTESIAN_POINT('Ctrl Pts',(16.9698336794029,18.0407513332138,14.8124796571692));
#189439=CARTESIAN_POINT('Ctrl Pts',(16.961496440917,18.0534327083962,14.8133837577837));
#189440=CARTESIAN_POINT('Ctrl Pts',(16.9579652719052,18.0588578452648,14.8137703026835));
#189441=CARTESIAN_POINT('Ctrl Pts',(16.9511894775922,18.0693730569864,14.8145191098314));
#189442=CARTESIAN_POINT('Ctrl Pts',(16.9479416282309,18.0744609873468,14.8148812468836));
#189443=CARTESIAN_POINT('Ctrl Pts',(16.9402801642771,18.086577025803,14.815743214593));
#189444=CARTESIAN_POINT('Ctrl Pts',(16.9358860542763,18.0936172951517,14.8162437611199));
#189445=CARTESIAN_POINT('Ctrl Pts',(16.9204544005099,18.1186687376452,14.8180238582751));
#189446=CARTESIAN_POINT('Ctrl Pts',(16.9096454481286,18.1368186156605,14.8193117390215));
#189447=CARTESIAN_POINT('Ctrl Pts',(16.8022349837243,18.3234758268036,14.8325423902071));
#189448=CARTESIAN_POINT('Ctrl Pts',(16.7290069388184,18.504327211604,14.8453728746243));
#189449=CARTESIAN_POINT('Ctrl Pts',(16.663179753398,18.7649447008822,14.8631017335751));
#189450=CARTESIAN_POINT('Ctrl Pts',(16.6487382172893,18.8382445131747,14.8679934987469));
#189451=CARTESIAN_POINT('Ctrl Pts',(16.6333272063734,18.9463232578167,14.8749433520185));
#189452=CARTESIAN_POINT('Ctrl Pts',(16.6292914351499,18.9806043872408,14.8771093030452));
#189453=CARTESIAN_POINT('Ctrl Pts',(16.6254128237953,19.0223111974838,14.8796857602423));
#189454=CARTESIAN_POINT('Ctrl Pts',(16.6247685437036,19.0296549937335,14.8801372244748));
#189455=CARTESIAN_POINT('Ctrl Pts',(16.6238224662587,19.0411267981678,14.8808388654566));
#189456=CARTESIAN_POINT('Ctrl Pts',(16.6234943983557,19.0452524971157,14.881090477006));
#189457=CARTESIAN_POINT('Ctrl Pts',(16.6229060238798,19.0529368627564,14.8815577348391));
#189458=CARTESIAN_POINT('Ctrl Pts',(16.6226426178651,19.0564951893061,14.881773547323));
#189459=CARTESIAN_POINT('Ctrl Pts',(16.6220645668631,19.0645816660428,14.8822627434926));
#189460=CARTESIAN_POINT('Ctrl Pts',(16.621755488347,19.0691101619884,14.8825358122539));
#189461=CARTESIAN_POINT('Ctrl Pts',(16.6209918952302,19.0808538743417,14.8832417451086));
#189462=CARTESIAN_POINT('Ctrl Pts',(16.6205597666355,19.0880705558767,14.8836733851893));
#189463=CARTESIAN_POINT('Ctrl Pts',(16.6180743366903,19.1334751338754,14.8863762693513));
#189464=CARTESIAN_POINT('Ctrl Pts',(16.6170190193779,19.1717131811661,14.8885955101876));
#189465=CARTESIAN_POINT('Ctrl Pts',(16.6169207098274,19.3720991911078,14.9000236634872));
#189466=CARTESIAN_POINT('Ctrl Pts',(16.6354677287759,19.5337233103895,14.9085853062952));
#189467=CARTESIAN_POINT('Ctrl Pts',(16.6916958528464,19.7749057138282,14.9221735840905));
#189468=CARTESIAN_POINT('Ctrl Pts',(16.7161208846119,19.8568711869279,14.9269355617778));
#189469=CARTESIAN_POINT('Ctrl Pts',(16.7454193857226,19.9371102812384,14.9318514580964));
#189470=CARTESIAN_POINT('Origin',(18.734,19.211,0.));
#189471=CARTESIAN_POINT('',(16.7454193622843,19.9371102170485,15.9575278583994));
#189472=CARTESIAN_POINT('',(16.7454193680152,19.9371102327436,15.7328935264317));
#189473=CARTESIAN_POINT('',(16.7454193623258,19.9371102171621,0.));
#189474=CARTESIAN_POINT('',(16.6170004656572,19.2095958660383,15.9109437209775));
#189475=CARTESIAN_POINT('Ctrl Pts',(16.7454193622843,19.9371102170485,15.9575278583994));
#189476=CARTESIAN_POINT('Ctrl Pts',(16.7400022625306,19.9222745358669,15.9565690136276));
#189477=CARTESIAN_POINT('Ctrl Pts',(16.7347514139459,19.9073788646741,15.9556046485865));
#189478=CARTESIAN_POINT('Ctrl Pts',(16.6996561822292,19.8041504797119,15.9489091241404));
#189479=CARTESIAN_POINT('Ctrl Pts',(16.6755129666081,19.714000406954,15.9429927030363));
#189480=CARTESIAN_POINT('Ctrl Pts',(16.6304401550311,19.4865778873416,15.9279421192691));
#189481=CARTESIAN_POINT('Ctrl Pts',(16.6169140878316,19.348289387691,15.9186652721273));
#189482=CARTESIAN_POINT('Ctrl Pts',(16.6170004105495,19.2096815667617,15.9096291409546));
#189483=CARTESIAN_POINT('Ctrl Pts',(16.7454193623258,19.9371102171621,15.155594536163));
#189484=CARTESIAN_POINT('Ctrl Pts',(16.7703664680976,20.005432257441,15.1599719849976));
#189485=CARTESIAN_POINT('Ctrl Pts',(16.7988694131869,20.0725513229361,15.1643494338322));
#189486=CARTESIAN_POINT('Ctrl Pts',(16.8307866970858,20.1380750366667,15.1687268826668));
#189487=CARTESIAN_POINT('Ctrl Pts',(16.8626811573905,20.2035518953247,15.1731012012503));
#189488=CARTESIAN_POINT('Ctrl Pts',(16.8979849019958,20.2674352332271,15.1774755198337));
#189489=CARTESIAN_POINT('Ctrl Pts',(16.9365083970907,20.3293527786304,15.1818498384171));
#189490=CARTESIAN_POINT('Ctrl Pts',(16.9750170528872,20.3912464733181,15.1862224720076));
#189491=CARTESIAN_POINT('Ctrl Pts',(17.0167427428274,20.451175469324,15.190595105598));
#189492=CARTESIAN_POINT('Ctrl Pts',(17.0614509054573,20.5087937148656,15.1949677391885));
#189493=CARTESIAN_POINT('Ctrl Pts',(17.1061565945774,20.566408772638,15.19934013086));
#189494=CARTESIAN_POINT('Ctrl Pts',(17.1538441318443,20.6217129536265,15.2037125225315));
#189495=CARTESIAN_POINT('Ctrl Pts',(17.2042377275192,20.6743920833784,15.2080849142029));
#189496=CARTESIAN_POINT('Ctrl Pts',(17.2546810076,20.7271231509058,15.2124616167334));
#189497=CARTESIAN_POINT('Ctrl Pts',(17.3078353415552,20.7772236475919,15.2168383192638));
#189498=CARTESIAN_POINT('Ctrl Pts',(17.3633875557035,20.8244157949951,15.2212150217942));
#189499=CARTESIAN_POINT('Ctrl Pts',(17.4189660791044,20.8716302923646,15.2255937971092));
#189500=CARTESIAN_POINT('Ctrl Pts',(17.4769443612593,20.9159334030165,15.2299725724242));
#189501=CARTESIAN_POINT('Ctrl Pts',(17.5369777396172,20.9570889748658,15.2343513477392));
#189502=CARTESIAN_POINT('Ctrl Pts',(17.5971222844656,20.9983207563274,15.2387382314282));
#189503=CARTESIAN_POINT('Ctrl Pts',(17.6593291169464,21.0363931003563,15.2431251151172));
#189504=CARTESIAN_POINT('Ctrl Pts',(17.7232266628523,21.0711145827371,15.2475119988062));
#189505=CARTESIAN_POINT('Ctrl Pts',(17.782315602858,21.1032231020898,15.2515687478321));
#189506=CARTESIAN_POINT('Ctrl Pts',(17.8428498211749,21.1324665095571,15.255625496858));
#189507=CARTESIAN_POINT('Ctrl Pts',(17.9045214391031,21.1587305555473,15.2596822458839));
#189508=CARTESIAN_POINT('Ctrl Pts',(17.9712319856141,21.1871405262996,15.2640704548148));
#189509=CARTESIAN_POINT('Ctrl Pts',(18.0395340178846,21.2121746938963,15.2684586637457));
#189510=CARTESIAN_POINT('Ctrl Pts',(18.1090523123261,21.2336540454737,15.2728468726766));
#189511=CARTESIAN_POINT('Ctrl Pts',(18.1784674300924,21.2551015181321,15.2772285687779));
#189512=CARTESIAN_POINT('Ctrl Pts',(18.2490947695204,21.2730045070021,15.2816102648792));
#189513=CARTESIAN_POINT('Ctrl Pts',(18.3205388114184,21.2872318862633,15.2859919609805));
#189514=CARTESIAN_POINT('Ctrl Pts',(18.3918989008814,21.3014425472217,15.2903685082401));
#189515=CARTESIAN_POINT('Ctrl Pts',(18.464073315643,21.3119860848153,15.2947450554998));
#189516=CARTESIAN_POINT('Ctrl Pts',(18.5366526876881,21.31878154426,15.2991216027594));
#189517=CARTESIAN_POINT('Ctrl Pts',(18.6091860309503,21.3255726941232,15.3034953744764));
#189518=CARTESIAN_POINT('Ctrl Pts',(18.6821233428399,21.3286204372107,15.3078691461934));
#189519=CARTESIAN_POINT('Ctrl Pts',(18.7550478100785,21.3278953657871,15.3122429179104));
#189520=CARTESIAN_POINT('Ctrl Pts',(18.8279500861569,21.3271705150052,15.3166153586739));
#189521=CARTESIAN_POINT('Ctrl Pts',(18.90083904328,21.322675133798,15.3209877994375));
#189522=CARTESIAN_POINT('Ctrl Pts',(18.9732972139369,21.3144319203155,15.325360240201));
#189523=CARTESIAN_POINT('Ctrl Pts',(19.0457572373572,21.306188496053,15.3297327927684));
#189524=CARTESIAN_POINT('Ctrl Pts',(19.1177859733815,21.2941971057617,15.3341053453358));
#189525=CARTESIAN_POINT('Ctrl Pts',(19.1889721056855,21.2785321963752,15.3384778979031));
#189526=CARTESIAN_POINT('Ctrl Pts',(19.2602321176427,21.2628510293548,15.3428549884705));
#189527=CARTESIAN_POINT('Ctrl Pts',(19.3306473077957,21.2434888351841,15.3472320790378));
#189528=CARTESIAN_POINT('Ctrl Pts',(19.3998183959355,21.2205708157798,15.3516091696051));
#189529=CARTESIAN_POINT('Ctrl Pts',(19.4690272609739,21.1976402799945,15.3559886506641));
#189530=CARTESIAN_POINT('Ctrl Pts',(19.5369902214647,21.1711502278382,15.360368131723));
#189531=CARTESIAN_POINT('Ctrl Pts',(19.603327519791,21.1412742456278,15.364747612782));
#189532=CARTESIAN_POINT('Ctrl Pts',(19.6697824005332,21.1113453084395,15.3691348564417));
#189533=CARTESIAN_POINT('Ctrl Pts',(19.734605435542,21.0780186771204,15.3735221001015));
#189534=CARTESIAN_POINT('Ctrl Pts',(19.7974415556905,21.0415138780218,15.3779093437612));
#189535=CARTESIAN_POINT('Ctrl Pts',(19.8401640625163,21.0166941322295,15.3808922466959));
#189536=CARTESIAN_POINT('Ctrl Pts',(19.8819686426657,20.9904061565714,15.3838751496307));
#189537=CARTESIAN_POINT('Ctrl Pts',(19.9227521494642,20.9627298099719,15.3868580525654));
#189538=CARTESIAN_POINT('Ctrl Pts',(19.982749592452,20.9220145758598,15.3912462614963));
#189539=CARTESIAN_POINT('Ctrl Pts',(20.0407699602752,20.878133895861,15.3956344704272));
#189540=CARTESIAN_POINT('Ctrl Pts',(20.096459630033,20.8313063773652,15.4000226793581));
#189541=CARTESIAN_POINT('Ctrl Pts',(20.1520666470873,20.7845483586711,15.4044043754594));
#189542=CARTESIAN_POINT('Ctrl Pts',(20.2053494667963,20.7348524915495,15.4087860715606));
#189543=CARTESIAN_POINT('Ctrl Pts',(20.2559837460592,20.6824803691289,15.4131677676619));
#189544=CARTESIAN_POINT('Ctrl Pts',(20.3065585260143,20.63016978812,15.4175443149215));
#189545=CARTESIAN_POINT('Ctrl Pts',(20.3544906143938,20.5751895440799,15.4219208621811));
#189546=CARTESIAN_POINT('Ctrl Pts',(20.3994903578933,20.5178400314363,15.4262974094408));
#189547=CARTESIAN_POINT('Ctrl Pts',(20.4444615632094,20.4605268890201,15.4306711811577));
#189548=CARTESIAN_POINT('Ctrl Pts',(20.4865038163905,20.4008478378294,15.4350449528747));
#189549=CARTESIAN_POINT('Ctrl Pts',(20.5253667770626,20.3391374340196,15.4394187245917));
#189550=CARTESIAN_POINT('Ctrl Pts',(20.5642179116052,20.277445808893,15.4437911653552));
#189551=CARTESIAN_POINT('Ctrl Pts',(20.5998914174618,20.2137244662945,15.4481636061187));
#189552=CARTESIAN_POINT('Ctrl Pts',(20.6321804129385,20.1483367164134,15.4525360468823));
#189553=CARTESIAN_POINT('Ctrl Pts',(20.6644702340484,20.0829472945602,15.4569085994496));
#189554=CARTESIAN_POINT('Ctrl Pts',(20.693375161169,20.0158918142288,15.461281152017));
#189555=CARTESIAN_POINT('Ctrl Pts',(20.718735154665,19.9475564240687,15.4656537045843));
#189556=CARTESIAN_POINT('Ctrl Pts',(20.7441214677188,19.8791501128632,15.4700307951516));
#189557=CARTESIAN_POINT('Ctrl Pts',(20.7659553334551,19.8094616929188,15.4744078857189));
#189558=CARTESIAN_POINT('Ctrl Pts',(20.7841259040681,19.7388946651266,15.4787849762862));
#189559=CARTESIAN_POINT('Ctrl Pts',(20.802306398304,19.6682890980615,15.4831644573452));
#189560=CARTESIAN_POINT('Ctrl Pts',(20.8168195180766,19.5968044408521,15.4875439384041));
#189561=CARTESIAN_POINT('Ctrl Pts',(20.8276056664122,19.5248539685374,15.491923419463));
#189562=CARTESIAN_POINT('Ctrl Pts',(20.8384109331233,19.4527759644936,15.4963106631227));
#189563=CARTESIAN_POINT('Ctrl Pts',(20.8454759896221,19.3802309770758,15.5006979067825));
#189564=CARTESIAN_POINT('Ctrl Pts',(20.8487932306453,19.307636388679,15.5050851504422));
#189565=CARTESIAN_POINT('Ctrl Pts',(20.8510486348925,19.2582790637657,15.5080680533771));
#189566=CARTESIAN_POINT('Ctrl Pts',(20.8515726338748,19.2088988449428,15.511050956312));
#189567=CARTESIAN_POINT('Ctrl Pts',(20.8503765449711,19.1596256883619,15.5140338592469));
#189568=CARTESIAN_POINT('Ctrl Pts',(20.8486169543561,19.0871389496107,15.5184220681777));
#189569=CARTESIAN_POINT('Ctrl Pts',(20.8431255714046,19.0146012223731,15.5228102771086));
#189570=CARTESIAN_POINT('Ctrl Pts',(20.8338948009669,18.9424281755803,15.5271984860395));
#189571=CARTESIAN_POINT('Ctrl Pts',(20.824677730523,18.8703622455555,15.5315801821408));
#189572=CARTESIAN_POINT('Ctrl Pts',(20.8117323505351,18.798660396053,15.5359618782421));
#189573=CARTESIAN_POINT('Ctrl Pts',(20.7951030586573,18.7277369436907,15.5403435743433));
#189574=CARTESIAN_POINT('Ctrl Pts',(20.7784933075209,18.6568968320293,15.544720121603));
#189575=CARTESIAN_POINT('Ctrl Pts',(20.7582083534313,18.5868337678033,15.5490966688626));
#189576=CARTESIAN_POINT('Ctrl Pts',(20.7343439967237,18.5179539014095,15.5534732161222));
#189577=CARTESIAN_POINT('Ctrl Pts',(20.7104947744443,18.4491177176259,15.5578469878392));
#189578=CARTESIAN_POINT('Ctrl Pts',(20.6830708110599,18.3814636975244,15.5622207595562));
#189579=CARTESIAN_POINT('Ctrl Pts',(20.6522179108564,18.3153834266441,15.5665945312732));
#189580=CARTESIAN_POINT('Ctrl Pts',(20.6213743992941,18.2493232642122,15.5709669720367));
#189581=CARTESIAN_POINT('Ctrl Pts',(20.5871042264083,18.1848363370636,15.5753394128002));
#189582=CARTESIAN_POINT('Ctrl Pts',(20.5496008974362,18.1222932528781,15.5797118535638));
#189583=CARTESIAN_POINT('Ctrl Pts',(20.5120966094998,18.0597485694589,15.5840844061311));
#189584=CARTESIAN_POINT('Ctrl Pts',(20.4713592511259,17.9991482403587,15.5884569586985));
#189585=CARTESIAN_POINT('Ctrl Pts',(20.4276268858002,17.940835848524,15.5928295112658));
#189586=CARTESIAN_POINT('Ctrl Pts',(20.3838491333762,17.8824629378895,15.5972066018331));
#189587=CARTESIAN_POINT('Ctrl Pts',(20.3370704580454,17.8263830921189,15.6015836924005));
#189588=CARTESIAN_POINT('Ctrl Pts',(20.2875701403869,17.7729079240542,15.6059607829678));
#189589=CARTESIAN_POINT('Ctrl Pts',(20.2380427887678,17.7194035512154,15.6103402640267));
#189590=CARTESIAN_POINT('Ctrl Pts',(20.1857911812167,17.6685070251039,15.6147197450856));
#189591=CARTESIAN_POINT('Ctrl Pts',(20.1311305579275,17.6204921552834,15.6190992261446));
#189592=CARTESIAN_POINT('Ctrl Pts',(20.0763730490505,17.5723921794284,15.6234864698043));
#189593=CARTESIAN_POINT('Ctrl Pts',(20.0191983762086,17.5271843592176,15.627873713464));
#189594=CARTESIAN_POINT('Ctrl Pts',(19.9599533753588,17.4851010106479,15.6322609571237));
#189595=CARTESIAN_POINT('Ctrl Pts',(19.9196724836152,17.4564883887621,15.6352438600586));
#189596=CARTESIAN_POINT('Ctrl Pts',(19.8784351648856,17.4293192126642,15.6382267629934));
#189597=CARTESIAN_POINT('Ctrl Pts',(19.8363568176098,17.4036543090296,15.6412096659283));
#189598=CARTESIAN_POINT('Ctrl Pts',(19.7744545085684,17.3658981494092,15.6455978748592));
#189599=CARTESIAN_POINT('Ctrl Pts',(19.7104893778663,17.3312522374743,15.6499860837901));
#189600=CARTESIAN_POINT('Ctrl Pts',(19.6448068261832,17.2999479532524,15.654374292721));
#189601=CARTESIAN_POINT('Ctrl Pts',(19.5792217582972,17.2686901297788,15.6587559888222));
#189602=CARTESIAN_POINT('Ctrl Pts',(19.5119247612702,17.2407642944952,15.6631376849235));
#189603=CARTESIAN_POINT('Ctrl Pts',(19.4432882414192,17.2163573777279,15.6675193810248));
#189604=CARTESIAN_POINT('Ctrl Pts',(19.3747323749412,17.1919791410302,15.6718959282844));
#189605=CARTESIAN_POINT('Ctrl Pts',(19.3048405647331,17.1711117694416,15.6762724755441));
#189606=CARTESIAN_POINT('Ctrl Pts',(19.2340061739085,17.1538945515474,15.6806490228037));
#189607=CARTESIAN_POINT('Ctrl Pts',(19.163216705225,17.1366882525625,15.6850227945207));
#189608=CARTESIAN_POINT('Ctrl Pts',(19.0914863095569,17.1231276279116,15.6893965662377));
#189609=CARTESIAN_POINT('Ctrl Pts',(19.0192231694674,17.1133020370895,15.6937703379547));
#189610=CARTESIAN_POINT('Ctrl Pts',(18.9469820192941,17.1034794362276,15.6981427787182));
#189611=CARTESIAN_POINT('Ctrl Pts',(18.8742089242417,17.0973896776779,15.7025152194818));
#189612=CARTESIAN_POINT('Ctrl Pts',(18.8013202474334,17.0950706570668,15.7068876602453));
#189613=CARTESIAN_POINT('Ctrl Pts',(18.7284297068536,17.0927515771582,15.7112602128127));
#189614=CARTESIAN_POINT('Ctrl Pts',(18.6554240608475,17.0942034399582,15.71563276538));
#189615=CARTESIAN_POINT('Ctrl Pts',(18.5827210675495,17.0994120466822,15.7200053179474));
#189616=CARTESIAN_POINT('Ctrl Pts',(18.5099426203428,17.1046260590948,15.7243824085147));
#189617=CARTESIAN_POINT('Ctrl Pts',(18.4374679351488,17.1136045652851,15.7287594990821));
#189618=CARTESIAN_POINT('Ctrl Pts',(18.3657101983343,17.1262814046042,15.7331365896494));
#189619=CARTESIAN_POINT('Ctrl Pts',(18.2939132719564,17.1389651672158,15.7375160707084));
#189620=CARTESIAN_POINT('Ctrl Pts',(18.2228345439091,17.1553511759151,15.7418955517673));
#189621=CARTESIAN_POINT('Ctrl Pts',(18.1528748782421,17.1753225715104,15.7462750328263));
#189622=CARTESIAN_POINT('Ctrl Pts',(18.0827912095374,17.1953293662704,15.750662276486));
#189623=CARTESIAN_POINT('Ctrl Pts',(18.0138310210268,17.2189340823966,15.7550495201457));
#189624=CARTESIAN_POINT('Ctrl Pts',(17.9463773894242,17.2459708339799,15.7594367638054));
#189625=CARTESIAN_POINT('Ctrl Pts',(17.900515419752,17.2643532198009,15.7624196667402));
#189626=CARTESIAN_POINT('Ctrl Pts',(17.8553494637698,17.2843211191871,15.7654025696749));
#189627=CARTESIAN_POINT('Ctrl Pts',(17.8109931300722,17.3058104246385,15.7683854726097));
#189628=CARTESIAN_POINT('Ctrl Pts',(17.7457396290594,17.3374237771892,15.7727736815406));
#189629=CARTESIAN_POINT('Ctrl Pts',(17.6819847879022,17.3724551543895,15.7771618904715));
#189630=CARTESIAN_POINT('Ctrl Pts',(17.6201101194241,17.4107393705492,15.7815500994024));
#189631=CARTESIAN_POINT('Ctrl Pts',(17.558327283213,17.4489667665845,15.7859317955037));
#189632=CARTESIAN_POINT('Ctrl Pts',(17.4984194869966,17.4904371661199,15.790313491605));
#189633=CARTESIAN_POINT('Ctrl Pts',(17.4407454860727,17.5349386162175,15.7946951877062));
#189634=CARTESIAN_POINT('Ctrl Pts',(17.3831392566899,17.5793877735698,15.7990717349659));
#189635=CARTESIAN_POINT('Ctrl Pts',(17.3277619882545,17.626860612876,15.8034482822255));
#189636=CARTESIAN_POINT('Ctrl Pts',(17.2749437204164,17.6771017722784,15.8078248294852));
#189637=CARTESIAN_POINT('Ctrl Pts',(17.2221589491561,17.7273110694676,15.8121986012021));
#189638=CARTESIAN_POINT('Ctrl Pts',(17.1719303071395,17.7802848717172,15.8165723729191));
#189639=CARTESIAN_POINT('Ctrl Pts',(17.12455387304,17.8357283306876,15.8209461446361));
#189640=CARTESIAN_POINT('Ctrl Pts',(17.0771918557485,17.8911549180272,15.8253185853996));
#189641=CARTESIAN_POINT('Ctrl Pts',(17.0326806364324,17.9490493035727,15.8296910261632));
#189642=CARTESIAN_POINT('Ctrl Pts',(16.9912774487782,18.0090819040121,15.8340634669268));
#189643=CARTESIAN_POINT('Ctrl Pts',(16.94987320244,18.0691160394918,15.8384360194941));
#189644=CARTESIAN_POINT('Ctrl Pts',(16.911577417771,18.1312881001858,15.8428085720615));
#189645=CARTESIAN_POINT('Ctrl Pts',(16.8766042803952,18.1952391320819,15.8471811246288));
#189646=CARTESIAN_POINT('Ctrl Pts',(16.8415948465783,18.259256534771,15.8515582151961));
#189647=CARTESIAN_POINT('Ctrl Pts',(16.8099151769005,18.3250561707614,15.8559353057635));
#189648=CARTESIAN_POINT('Ctrl Pts',(16.7817332906699,18.3922548042025,15.8603123963308));
#189649=CARTESIAN_POINT('Ctrl Pts',(16.7535360132653,18.4594901373113,15.8646918773897));
#189650=CARTESIAN_POINT('Ctrl Pts',(16.728840486062,18.5281255348702,15.8690713584487));
#189651=CARTESIAN_POINT('Ctrl Pts',(16.7077654290803,18.5977606799873,15.8734508395076));
#189652=CARTESIAN_POINT('Ctrl Pts',(16.6866530167015,18.6675192529316,15.8778380831674));
#189653=CARTESIAN_POINT('Ctrl Pts',(16.6691740053289,18.7382806434227,15.8822253268271));
#189654=CARTESIAN_POINT('Ctrl Pts',(16.6553962633245,18.8096329536713,15.8866125704868));
#189655=CARTESIAN_POINT('Ctrl Pts',(16.6460287263817,18.8581456491476,15.8895954734216));
#189656=CARTESIAN_POINT('Ctrl Pts',(16.6383710944437,18.9069313156785,15.8925783763564));
#189657=CARTESIAN_POINT('Ctrl Pts',(16.6324309574258,18.9558597262409,15.8955612792912));
#189658=CARTESIAN_POINT('Ctrl Pts',(16.6222201199426,19.0399655384572,15.9006887598533));
#189659=CARTESIAN_POINT('Ctrl Pts',(16.617056776629,19.1246963446803,15.9058162404154));
#189660=CARTESIAN_POINT('Ctrl Pts',(16.6170004656572,19.2095958660383,15.9109437209775));
#189661=CARTESIAN_POINT('',(16.6170004208928,19.2096650617603,15.6876313494247));
#189662=CARTESIAN_POINT('Ctrl Pts',(16.7454193857226,19.9371102812384,14.9318514580964));
#189663=CARTESIAN_POINT('Ctrl Pts',(16.7539898736387,19.9605820686035,14.9332894712505));
#189664=CARTESIAN_POINT('Ctrl Pts',(16.7629773978124,19.9839061466847,14.9347402980908));
#189665=CARTESIAN_POINT('Ctrl Pts',(16.7777126708588,20.0202157393077,14.9370362397452));
#189666=CARTESIAN_POINT('Ctrl Pts',(16.7831788110021,20.0333058438738,14.9378716807806));
#189667=CARTESIAN_POINT('Ctrl Pts',(16.7921001472685,20.054080620314,14.9392103641091));
#189668=CARTESIAN_POINT('Ctrl Pts',(16.7954704382653,20.061801448952,14.939710719563));
#189669=CARTESIAN_POINT('Ctrl Pts',(16.8015031078453,20.0753994382038,14.9405970664953));
#189670=CARTESIAN_POINT('Ctrl Pts',(16.8041464536429,20.0812849620356,14.9409824018903));
#189671=CARTESIAN_POINT('Ctrl Pts',(16.8096767348222,20.0934492779395,14.9417823977819));
#189672=CARTESIAN_POINT('Ctrl Pts',(16.8125675897148,20.0997261940465,14.9421971898744));
#189673=CARTESIAN_POINT('Ctrl Pts',(16.8200827103448,20.115835715273,14.9432669169788));
#189674=CARTESIAN_POINT('Ctrl Pts',(16.8247519941562,20.1256469857614,14.9439234049188));
#189675=CARTESIAN_POINT('Ctrl Pts',(16.8446948433191,20.1667334551882,14.9466939028832));
#189676=CARTESIAN_POINT('Ctrl Pts',(16.8606622632928,20.197664031381,14.9488319850111));
#189677=CARTESIAN_POINT('Ctrl Pts',(16.9043949234205,20.277486977492,14.9544918295384));
#189678=CARTESIAN_POINT('Ctrl Pts',(16.9333566765409,20.3256891777366,14.9580538176853));
#189679=CARTESIAN_POINT('Ctrl Pts',(17.0332351059343,20.4778524387781,14.9697636317365));
#189680=CARTESIAN_POINT('Ctrl Pts',(17.1115039702421,20.5766567273707,14.9781230611111));
#189681=CARTESIAN_POINT('Ctrl Pts',(17.2668972841675,20.7404771510173,14.9930005545619));
#189682=CARTESIAN_POINT('Ctrl Pts',(17.3407870119797,20.8080764090406,14.9995201489052));
#189683=CARTESIAN_POINT('Ctrl Pts',(17.4267853807552,20.8762245834316,15.0062995441743));
#189684=CARTESIAN_POINT('Ctrl Pts',(17.4344245245433,20.8821931563487,15.0068951758941));
#189685=CARTESIAN_POINT('Ctrl Pts',(17.4457640317482,20.8909281020863,15.0077693341156));
#189686=CARTESIAN_POINT('Ctrl Pts',(17.4494327578418,20.8937350770054,15.0080506260364));
#189687=CARTESIAN_POINT('Ctrl Pts',(17.4559575636312,20.898693489956,15.0085481520704));
#189688=CARTESIAN_POINT('Ctrl Pts',(17.458809932896,20.9008497207262,15.008764721023));
#189689=CARTESIAN_POINT('Ctrl Pts',(17.4649328356837,20.9054539594798,15.0092276133082));
#189690=CARTESIAN_POINT('Ctrl Pts',(17.4682049867575,20.9078997240385,15.0094737804235));
#189691=CARTESIAN_POINT('Ctrl Pts',(17.4772061298521,20.9145870918971,15.0101476987871));
#189692=CARTESIAN_POINT('Ctrl Pts',(17.4829495581171,20.9188093005004,15.0105741179115));
#189693=CARTESIAN_POINT('Ctrl Pts',(17.5137221088844,20.9411928062782,15.0128403498042));
#189694=CARTESIAN_POINT('Ctrl Pts',(17.5391269884115,20.9588340858544,15.0146464277926));
#189695=CARTESIAN_POINT('Ctrl Pts',(17.6171834034302,21.0105391244381,15.0200319022));
#189696=CARTESIAN_POINT('Ctrl Pts',(17.6709725473431,21.0428280908763,15.023524549167));
#189697=CARTESIAN_POINT('Ctrl Pts',(17.8443350941308,21.136683329717,15.0343589198719));
#189698=CARTESIAN_POINT('Ctrl Pts',(17.9683762767184,21.1892772672582,15.04152766775));
#189699=CARTESIAN_POINT('Ctrl Pts',(18.1354764561819,21.2420399640214,15.0512527113468));
#189700=CARTESIAN_POINT('Ctrl Pts',(18.1747299578942,21.2531974787995,15.0535399438182));
#189701=CARTESIAN_POINT('Ctrl Pts',(18.2613894662419,21.2751438718862,15.0586206858394));
#189702=CARTESIAN_POINT('Ctrl Pts',(18.3088928173713,21.2854478761445,15.0614259934544));
#189703=CARTESIAN_POINT('Ctrl Pts',(18.3691073316157,21.2963539688809,15.0650250123058));
#189704=CARTESIAN_POINT('Ctrl Pts',(18.3815281411256,21.2984892606516,15.0657696568682));
#189705=CARTESIAN_POINT('Ctrl Pts',(18.4012400691229,21.3016970430008,15.0669552633267));
#189706=CARTESIAN_POINT('Ctrl Pts',(18.4085191187147,21.3028426066562,15.0673939024762));
#189707=CARTESIAN_POINT('Ctrl Pts',(18.4220931020484,21.3049062908642,15.0682134788143));
#189708=CARTESIAN_POINT('Ctrl Pts',(18.4283864970922,21.3058340873165,15.068594104358));
#189709=CARTESIAN_POINT('Ctrl Pts',(18.4423736161947,21.3078317504683,15.0694415085676));
#189710=CARTESIAN_POINT('Ctrl Pts',(18.4500692117576,21.3088876620265,15.0699087235272));
#189711=CARTESIAN_POINT('Ctrl Pts',(18.4724466382034,21.311832683153,15.0712702336299));
#189712=CARTESIAN_POINT('Ctrl Pts',(18.4871424637311,21.3136101547827,15.0721680370904));
#189713=CARTESIAN_POINT('Ctrl Pts',(18.6040634136054,21.32650918205,15.0793414021644));
#189714=CARTESIAN_POINT('Ctrl Pts',(18.7069418250766,21.3303218337858,15.0858477838725));
#189715=CARTESIAN_POINT('Ctrl Pts',(18.9653686792341,21.3210777729614,15.1026338937291));
#189716=CARTESIAN_POINT('Ctrl Pts',(19.1199578148917,21.2983410167675,15.1131041132348));
#189717=CARTESIAN_POINT('Ctrl Pts',(19.3214647071208,21.2455352974122,15.1265600164924));
#189718=CARTESIAN_POINT('Ctrl Pts',(19.3717727891725,21.23033046406,15.1298978690499));
#189719=CARTESIAN_POINT('Ctrl Pts',(19.4296851277199,21.2104465982146,15.1336748223086));
#189720=CARTESIAN_POINT('Ctrl Pts',(19.4378857914466,21.2075743899462,15.1342080934621));
#189721=CARTESIAN_POINT('Ctrl Pts',(19.4502843215203,21.2031460311206,15.1350117180827));
#189722=CARTESIAN_POINT('Ctrl Pts',(19.4544952029299,21.2016269620328,15.1352841903171));
#189723=CARTESIAN_POINT('Ctrl Pts',(19.4620494559043,21.1988746660993,15.1357721316086));
#189724=CARTESIAN_POINT('Ctrl Pts',(19.4653945446348,21.1976463497611,15.1359878864854));
#189725=CARTESIAN_POINT('Ctrl Pts',(19.4726614168395,21.1949571127201,15.1364559143958));
#189726=CARTESIAN_POINT('Ctrl Pts',(19.4765819620693,21.1934930123824,15.1367079945564));
#189727=CARTESIAN_POINT('Ctrl Pts',(19.487595220487,21.1893429338197,15.1374149877408));
#189728=CARTESIAN_POINT('Ctrl Pts',(19.4946779612244,21.1866304217608,15.1378683428083));
#189729=CARTESIAN_POINT('Ctrl Pts',(19.5371983230854,21.1700836251916,15.1405829221296));
#189730=CARTESIAN_POINT('Ctrl Pts',(19.5722747614423,21.1553333116667,15.1427926142434));
#189731=CARTESIAN_POINT('Ctrl Pts',(19.6869971843577,21.1034080159472,15.1499806697728));
#189732=CARTESIAN_POINT('Ctrl Pts',(19.7647300507507,21.0622184479534,15.1547896859524));
#189733=CARTESIAN_POINT('Ctrl Pts',(19.9882626701981,20.92531359813,15.1690493690483));
#189734=CARTESIAN_POINT('Ctrl Pts',(20.125023331932,20.816332767206,15.1784223776321));
#189735=CARTESIAN_POINT('Ctrl Pts',(20.2630319137663,20.6753371457652,15.1898859646073));
#189736=CARTESIAN_POINT('Ctrl Pts',(20.2789076745533,20.6585780066204,15.1912382687377));
#189737=CARTESIAN_POINT('Ctrl Pts',(20.3009669061003,20.6345150635208,15.1931673763937));
#189738=CARTESIAN_POINT('Ctrl Pts',(20.307380136793,20.6274234400316,15.1937344036085));
#189739=CARTESIAN_POINT('Ctrl Pts',(20.3177190131074,20.6158340556644,15.1946587534172));
#189740=CARTESIAN_POINT('Ctrl Pts',(20.3216741063834,20.6113626556104,15.1950148344409));
#189741=CARTESIAN_POINT('Ctrl Pts',(20.3299107455761,20.6019710392164,15.1957616244884));
#189742=CARTESIAN_POINT('Ctrl Pts',(20.3341885655729,20.597047651748,15.1961524829716));
#189743=CARTESIAN_POINT('Ctrl Pts',(20.3443064345426,20.5852936186386,15.197084160035));
#189744=CARTESIAN_POINT('Ctrl Pts',(20.3501258388067,20.5784454404505,15.1976258215036));
#189745=CARTESIAN_POINT('Ctrl Pts',(20.3695622142201,20.555275662687,15.1994547299663));
#189746=CARTESIAN_POINT('Ctrl Pts',(20.3829765865681,20.5387864960595,15.2007501660214));
#189747=CARTESIAN_POINT('Ctrl Pts',(20.454518435157,20.4480896022527,15.2078448730744));
#189748=CARTESIAN_POINT('Ctrl Pts',(20.5078810015306,20.3702741060108,15.2138291960127));
#189749=CARTESIAN_POINT('Ctrl Pts',(20.6403913997157,20.1463601339531,15.2307281643116));
#189750=CARTESIAN_POINT('Ctrl Pts',(20.7078162184791,19.9941173521913,15.2419109618191));
#189751=CARTESIAN_POINT('Ctrl Pts',(20.769161392288,19.7954406617657,15.2552398611737));
#189752=CARTESIAN_POINT('Ctrl Pts',(20.7803558264263,19.7549495886665,15.2578907564886));
#189753=CARTESIAN_POINT('Ctrl Pts',(20.7921065681289,19.7069250637058,15.2609373336602));
#189754=CARTESIAN_POINT('Ctrl Pts',(20.7938361641377,19.6996914110497,15.2613936398139));
#189755=CARTESIAN_POINT('Ctrl Pts',(20.7965741884452,19.6879673933345,15.2621288605418));
#189756=CARTESIAN_POINT('Ctrl Pts',(20.7976061421072,19.6834826645766,15.2624090751273));
#189757=CARTESIAN_POINT('Ctrl Pts',(20.7994135281255,19.6755091282627,15.2629054123269));
#189758=CARTESIAN_POINT('Ctrl Pts',(20.8001947567421,19.6720216917714,15.2631218638132));
#189759=CARTESIAN_POINT('Ctrl Pts',(20.8018524605339,19.6645327779747,15.2635853007269));
#189760=CARTESIAN_POINT('Ctrl Pts',(20.8027261520414,19.6605307417158,15.2638321257698));
#189761=CARTESIAN_POINT('Ctrl Pts',(20.8050989832853,19.649508305544,15.2645097039309));
#189762=CARTESIAN_POINT('Ctrl Pts',(20.8065740551022,19.6424827019394,15.2649391007146));
#189763=CARTESIAN_POINT('Ctrl Pts',(20.8143549231348,19.6044625841117,15.2672500886656));
#189764=CARTESIAN_POINT('Ctrl Pts',(20.820001603532,19.573335429299,15.2690963467679));
#189765=CARTESIAN_POINT('Ctrl Pts',(20.8505127867128,19.3806475842458,15.2803089196882));
#189766=CARTESIAN_POINT('Ctrl Pts',(20.8572959239024,19.2167691245175,15.288947077949));
#189767=CARTESIAN_POINT('Ctrl Pts',(20.8364521815894,18.9369715422696,15.3043057683836));
#189768=CARTESIAN_POINT('Ctrl Pts',(20.8180851646639,18.8211532181488,15.310841028377));
#189769=CARTESIAN_POINT('Ctrl Pts',(20.7868423565605,18.6935721747176,15.3185359664359));
#189770=CARTESIAN_POINT('Ctrl Pts',(20.7833021632317,18.6797242485116,15.3193776654132));
#189771=CARTESIAN_POINT('Ctrl Pts',(20.7774449090729,18.6577429152904,15.3207244938376));
#189772=CARTESIAN_POINT('Ctrl Pts',(20.7752188323004,18.6495855597734,15.321226680366));
#189773=CARTESIAN_POINT('Ctrl Pts',(20.7712067809272,18.6352229386219,15.322115157907));
#189774=CARTESIAN_POINT('Ctrl Pts',(20.7694411641,18.6290120630748,15.3225007825789));
#189775=CARTESIAN_POINT('Ctrl Pts',(20.7657306820127,18.616183208605,15.3233002847032));
#189776=CARTESIAN_POINT('Ctrl Pts',(20.7637818325093,18.6095664706549,15.3237142883545));
#189777=CARTESIAN_POINT('Ctrl Pts',(20.7586966804201,18.5926076104067,15.3247796723959));
#189778=CARTESIAN_POINT('Ctrl Pts',(20.755513485927,18.5822798598391,15.3254325815888));
#189779=CARTESIAN_POINT('Ctrl Pts',(20.7419000500467,18.5392840059105,15.3281681890784));
#189780=CARTESIAN_POINT('Ctrl Pts',(20.7307563660389,18.5068488895757,15.3302742090506));
#189781=CARTESIAN_POINT('Ctrl Pts',(20.6996742249987,18.423061317881,15.3358289974504));
#189782=CARTESIAN_POINT('Ctrl Pts',(20.6785116348424,18.3721935814454,15.3393161566803));
#189783=CARTESIAN_POINT('Ctrl Pts',(20.6094731207301,18.2229453871187,15.3498858340951));
#189784=CARTESIAN_POINT('Ctrl Pts',(20.5559342397031,18.1273932888991,15.3571167426616));
#189785=CARTESIAN_POINT('Ctrl Pts',(20.4696765519122,17.9980523862437,15.3673864045986));
#189786=CARTESIAN_POINT('Ctrl Pts',(20.4428468031232,17.9605369627796,15.3704265358808));
#189787=CARTESIAN_POINT('Ctrl Pts',(20.4015473515862,17.9066032387941,15.3748628240414));
#189788=CARTESIAN_POINT('Ctrl Pts',(20.3880145265824,17.8894853114626,15.3762810190783));
#189789=CARTESIAN_POINT('Ctrl Pts',(20.341525361071,17.8325133753209,15.381028265932));
#189790=CARTESIAN_POINT('Ctrl Pts',(20.3073714259154,17.7936551332002,15.3843123525774));
#189791=CARTESIAN_POINT('Ctrl Pts',(20.2658813749311,17.7498007449412,15.3880359783541));
#189792=CARTESIAN_POINT('Ctrl Pts',(20.2598985665197,17.743554130336,15.3885667909802));
#189793=CARTESIAN_POINT('Ctrl Pts',(20.2507673947793,17.7341365559843,15.3893674523829));
#189794=CARTESIAN_POINT('Ctrl Pts',(20.2476470837842,17.730938694265,15.3896393970778));
#189795=CARTESIAN_POINT('Ctrl Pts',(20.2420203055254,17.7252084760256,15.3901267768547));
#189796=CARTESIAN_POINT('Ctrl Pts',(20.2395175609509,17.7226725599414,15.390342494809));
#189797=CARTESIAN_POINT('Ctrl Pts',(20.2340564916344,17.7171669799952,15.3908108837112));
#189798=CARTESIAN_POINT('Ctrl Pts',(20.2310957553338,17.7141997896139,15.39106335939));
#189799=CARTESIAN_POINT('Ctrl Pts',(20.2227314692954,17.7058669160822,15.3917725814064));
#189800=CARTESIAN_POINT('Ctrl Pts',(20.2173076902002,17.7005215035763,15.3922277539953));
#189801=CARTESIAN_POINT('Ctrl Pts',(20.1842244208549,17.6682662906918,15.3949765676913));
#189802=CARTESIAN_POINT('Ctrl Pts',(20.1558603352602,17.6420857964822,15.3972171535982));
#189803=CARTESIAN_POINT('Ctrl Pts',(20.058954150256,17.5574280457007,15.4045581070713));
#189804=CARTESIAN_POINT('Ctrl Pts',(19.9873946456709,17.5025480256279,15.4094808085603));
#189805=CARTESIAN_POINT('Ctrl Pts',(19.7703833223275,17.3571155107752,15.4236858801083));
#189806=CARTESIAN_POINT('Ctrl Pts',(19.6172056334296,17.2794412940434,15.4329071361176));
#189807=CARTESIAN_POINT('Ctrl Pts',(19.4344668967409,17.2131067737044,15.4442004797186));
#189808=CARTESIAN_POINT('Ctrl Pts',(19.4124499011301,17.2055232772403,15.4455644100353));
#189809=CARTESIAN_POINT('Ctrl Pts',(19.3811909321228,17.1953301470797,15.4475072852567));
#189810=CARTESIAN_POINT('Ctrl Pts',(19.3720489474315,17.1924176770146,15.448076261037));
#189811=CARTESIAN_POINT('Ctrl Pts',(19.3571816673791,17.1877923195441,15.4490029225743));
#189812=CARTESIAN_POINT('Ctrl Pts',(19.3514682969361,17.1860413312947,15.4493593542314));
#189813=CARTESIAN_POINT('Ctrl Pts',(19.3395085480022,17.1824313245277,15.4501061785426));
#189814=CARTESIAN_POINT('Ctrl Pts',(19.3332608536926,17.1805769158699,15.4504967175602));
#189815=CARTESIAN_POINT('Ctrl Pts',(19.3184050357965,17.176242027617,15.4514263448715));
#189816=CARTESIAN_POINT('Ctrl Pts',(19.3097895856061,17.1737872960114,15.4519662662143));
#189817=CARTESIAN_POINT('Ctrl Pts',(19.2808414063668,17.1657376214908,15.4537832258321));
#189818=CARTESIAN_POINT('Ctrl Pts',(19.2604412156062,17.1603919641542,15.4550683081813));
#189819=CARTESIAN_POINT('Ctrl Pts',(19.1497846573137,17.1331556070415,15.462066148723));
#189820=CARTESIAN_POINT('Ctrl Pts',(19.058253163731,17.116920214522,15.467958349142));
#189821=CARTESIAN_POINT('Ctrl Pts',(18.8138470815258,17.0899782168669,15.4839174380439));
#189822=CARTESIAN_POINT('Ctrl Pts',(18.6603742072936,17.0897540284929,15.4941950117233));
#189823=CARTESIAN_POINT('Ctrl Pts',(18.5049138745307,17.1064288737145,15.5043133508622));
#189824=CARTESIAN_POINT('Ctrl Pts',(18.5016052520021,17.1067916548598,15.5045285402374));
#189825=CARTESIAN_POINT('Ctrl Pts',(18.4463215744407,17.112985336748,15.508121378768));
#189826=CARTESIAN_POINT('Ctrl Pts',(18.3945744225895,17.1207331115901,15.511444043667));
#189827=CARTESIAN_POINT('Ctrl Pts',(18.3346378583765,17.1319920334928,15.51520572589));
#189828=CARTESIAN_POINT('Ctrl Pts',(18.3261223376977,17.1336458983902,15.5157380987637));
#189829=CARTESIAN_POINT('Ctrl Pts',(18.3132311110595,17.1362319279637,15.5165406408463));
#189830=CARTESIAN_POINT('Ctrl Pts',(18.3088479175262,17.1371256744297,15.5168129204609));
#189831=CARTESIAN_POINT('Ctrl Pts',(18.3009783792444,17.1387562949975,15.5173006565556));
#189832=CARTESIAN_POINT('Ctrl Pts',(18.2974910493845,17.1394880802724,15.5175163977796));
#189833=CARTESIAN_POINT('Ctrl Pts',(18.2899095596507,17.141098984263,15.5179845567174));
#189834=CARTESIAN_POINT('Ctrl Pts',(18.2858161685686,17.1419814432685,15.5182367806863));
#189835=CARTESIAN_POINT('Ctrl Pts',(18.2743053499205,17.1444987252268,15.5189445839966));
#189836=CARTESIAN_POINT('Ctrl Pts',(18.266893976798,17.1461613484341,15.5193985996502));
#189837=CARTESIAN_POINT('Ctrl Pts',(18.2222245625897,17.1564350344067,15.5221255551546));
#189838=CARTESIAN_POINT('Ctrl Pts',(18.1851939538965,17.1660150045352,15.5243464149621));
#189839=CARTESIAN_POINT('Ctrl Pts',(18.0632300955745,17.2011196280644,15.5315894552164));
#189840=CARTESIAN_POINT('Ctrl Pts',(17.9796374669179,17.2309770110101,15.5364393202617));
#189841=CARTESIAN_POINT('Ctrl Pts',(17.7391841251487,17.3343086564626,15.5506743656102));
#189842=CARTESIAN_POINT('Ctrl Pts',(17.5892041011794,17.4218480817856,15.5599880976046));
#189843=CARTESIAN_POINT('Ctrl Pts',(17.4330760379047,17.54072306789,15.5713882879402));
#189844=CARTESIAN_POINT('Ctrl Pts',(17.4148345318103,17.5550922157579,15.5727484584683));
#189845=CARTESIAN_POINT('Ctrl Pts',(17.3894034723066,17.5758116226648,15.5746868797984));
#189846=CARTESIAN_POINT('Ctrl Pts',(17.3820146505983,17.5819154527558,15.5752552240178));
#189847=CARTESIAN_POINT('Ctrl Pts',(17.3700880593261,17.5919049121813,15.5761811361066));
#189848=CARTESIAN_POINT('Ctrl Pts',(17.3655247904159,17.5957599915372,15.5765374539416));
#189849=CARTESIAN_POINT('Ctrl Pts',(17.3563677345484,17.6035625901537,15.5772566518401));
#189850=CARTESIAN_POINT('Ctrl Pts',(17.3517744515964,17.6075106119641,15.5776195507566));
#189851=CARTESIAN_POINT('Ctrl Pts',(17.3407774267729,17.617045145513,15.5784935872025));
#189852=CARTESIAN_POINT('Ctrl Pts',(17.3343902949704,17.6226505778043,15.5790055088681));
#189853=CARTESIAN_POINT('Ctrl Pts',(17.3141082723577,17.640667679329,15.5806449335358));
#189854=CARTESIAN_POINT('Ctrl Pts',(17.3003436997171,17.6532241196501,15.5817785065278));
#189855=CARTESIAN_POINT('Ctrl Pts',(17.2684821235173,17.6830691533946,15.5844528387181));
#189856=CARTESIAN_POINT('Ctrl Pts',(17.2505227223724,17.7004999497849,15.5859995790608));
#189857=CARTESIAN_POINT('Ctrl Pts',(17.1883845743239,17.7629864006987,15.5914930531436));
#189858=CARTESIAN_POINT('Ctrl Pts',(17.1459183158394,17.8096913987636,15.5955093279175));
#189859=CARTESIAN_POINT('Ctrl Pts',(17.0460725584953,17.9298797406588,15.6056137560596));
#189860=CARTESIAN_POINT('Ctrl Pts',(16.9913396084864,18.0053877006036,15.6117696252287));
#189861=CARTESIAN_POINT('Ctrl Pts',(16.8765795697267,18.1879280743259,15.6260161984534));
#189862=CARTESIAN_POINT('Ctrl Pts',(16.8205102116619,18.2970795750735,15.6340842561212));
#189863=CARTESIAN_POINT('Ctrl Pts',(16.7706161806151,18.419228364474,15.6422329730794));
#189864=CARTESIAN_POINT('Ctrl Pts',(16.7671004762423,18.4280027994263,15.6428135690498));
#189865=CARTESIAN_POINT('Ctrl Pts',(16.761971558019,18.441056023011,15.6436699308315));
#189866=CARTESIAN_POINT('Ctrl Pts',(16.7603133023376,18.4453168252728,15.6439483053232));
#189867=CARTESIAN_POINT('Ctrl Pts',(16.7573844801105,18.4529150190147,15.6444426227967));
#189868=CARTESIAN_POINT('Ctrl Pts',(16.7561085443978,18.4562502783246,15.6446588844482));
#189869=CARTESIAN_POINT('Ctrl Pts',(16.7533801307651,18.4634367090344,15.6451233012706));
#189870=CARTESIAN_POINT('Ctrl Pts',(16.7519304471216,18.4672888809334,15.645371288754));
#189871=CARTESIAN_POINT('Ctrl Pts',(16.7479520099501,18.477954842668,15.6460553443868));
#189872=CARTESIAN_POINT('Ctrl Pts',(16.7454470684721,18.4847775385847,15.6464900128808));
#189873=CARTESIAN_POINT('Ctrl Pts',(16.7317893099674,18.522577654256,15.6488829192696));
#189874=CARTESIAN_POINT('Ctrl Pts',(16.7213245088896,18.553800934464,15.6508027967598));
#189875=CARTESIAN_POINT('Ctrl Pts',(16.663602434638,18.7403594717851,15.6620105295621));
#189876=CARTESIAN_POINT('Ctrl Pts',(16.6336097086608,18.9004828368032,15.6705926721185));
#189877=CARTESIAN_POINT('Ctrl Pts',(16.6187709866018,19.1114653678293,15.6821718417595));
#189878=CARTESIAN_POINT('Ctrl Pts',(16.6170313866306,19.1605583302494,15.6848817035565));
#189879=CARTESIAN_POINT('Ctrl Pts',(16.6170004208928,19.2096650617603,15.6876313494247));
#189880=CARTESIAN_POINT('Ctrl Pts',(16.6170004192075,19.2096677371557,15.6876314992289));
#189881=CARTESIAN_POINT('Ctrl Pts',(16.6169565169163,19.2794295956352,15.6915376949309));
#189882=CARTESIAN_POINT('Ctrl Pts',(16.6203608902705,19.3491464384918,15.695521234486));
#189883=CARTESIAN_POINT('Ctrl Pts',(16.6282125593119,19.4288414159146,15.7002202367451));
#189884=CARTESIAN_POINT('Ctrl Pts',(16.6293001579621,19.4391100548907,15.7008284403706));
#189885=CARTESIAN_POINT('Ctrl Pts',(16.6312632478519,19.4564336662004,15.7018593105948));
#189886=CARTESIAN_POINT('Ctrl Pts',(16.6320992368905,19.4634929969452,15.7022807376865));
#189887=CARTESIAN_POINT('Ctrl Pts',(16.6337047673432,19.4764896969377,15.7030591573664));
#189888=CARTESIAN_POINT('Ctrl Pts',(16.634463973354,19.4824282873715,15.7034158213631));
#189889=CARTESIAN_POINT('Ctrl Pts',(16.6360832813492,19.4946812512276,15.7041537772539));
#189890=CARTESIAN_POINT('Ctrl Pts',(16.636946723945,19.5009951149655,15.704535171221));
#189891=CARTESIAN_POINT('Ctrl Pts',(16.6389488848926,19.5151590790055,15.7053933371429));
#189892=CARTESIAN_POINT('Ctrl Pts',(16.6401032381611,19.5230068402183,15.7058705994675));
#189893=CARTESIAN_POINT('Ctrl Pts',(16.6431522418392,19.5429558410351,15.7070884172785));
#189894=CARTESIAN_POINT('Ctrl Pts',(16.6451078426903,19.5550473418584,15.7078308944189));
#189895=CARTESIAN_POINT('Ctrl Pts',(16.6571525015344,19.6256277823438,15.7121907880401));
#189896=CARTESIAN_POINT('Ctrl Pts',(16.6695919117635,19.6836836981216,15.7158823675275));
#189897=CARTESIAN_POINT('Ctrl Pts',(16.6997698751888,19.8003540239869,15.7235211230514));
#189898=CARTESIAN_POINT('Ctrl Pts',(16.717645350903,19.8588760239831,15.7274691388482));
#189899=CARTESIAN_POINT('Ctrl Pts',(16.7404566866214,19.9234094087007,15.7319399174074));
#189900=CARTESIAN_POINT('Ctrl Pts',(16.742920533714,19.9302667353381,15.7324164742522));
#189901=CARTESIAN_POINT('Ctrl Pts',(16.7454193680152,19.9371102327436,15.7328935264317));
#189902=CARTESIAN_POINT('Origin',(18.734,19.211,0.));
#189903=CARTESIAN_POINT('',(16.745419290545,19.9371100205779,16.7554728823802));
#189904=CARTESIAN_POINT('',(16.7454193623258,19.9371102171621,16.5356516081066));
#189905=CARTESIAN_POINT('',(16.7454193623258,19.9371102171621,0.));
#189906=CARTESIAN_POINT('Ctrl Pts',(16.745419290545,19.9371100205779,16.7554728823802));
#189907=CARTESIAN_POINT('Ctrl Pts',(16.7246695916352,19.8802833003706,16.7521869364102));
#189908=CARTESIAN_POINT('Ctrl Pts',(16.7063536245855,19.8225613881497,16.7488940155909));
#189909=CARTESIAN_POINT('Ctrl Pts',(16.6648838496181,19.6693480707068,16.740135080757));
#189910=CARTESIAN_POINT('Ctrl Pts',(16.6458617517716,19.5729388012687,16.7345998747667));
#189911=CARTESIAN_POINT('Ctrl Pts',(16.6317631857905,19.4610092327402,16.7279812613245));
#189912=CARTESIAN_POINT('Ctrl Pts',(16.630081116969,19.4464348251301,16.727115924452));
#189913=CARTESIAN_POINT('Ctrl Pts',(16.6277432520215,19.4241464784128,16.725786761891));
#189914=CARTESIAN_POINT('Ctrl Pts',(16.6269780369723,19.4164442857521,16.7253263840921));
#189915=CARTESIAN_POINT('Ctrl Pts',(16.6257184973999,19.4030185094664,16.7245219869061));
#189916=CARTESIAN_POINT('Ctrl Pts',(16.625205197247,19.3972967553643,16.7241785687105));
#189917=CARTESIAN_POINT('Ctrl Pts',(16.6241033853661,19.3844264219209,16.7234047089429));
#189918=CARTESIAN_POINT('Ctrl Pts',(16.6235279049358,19.3772768241441,16.7229738616919));
#189919=CARTESIAN_POINT('Ctrl Pts',(16.6220830309171,19.3581085306041,16.7218161096034));
#189920=CARTESIAN_POINT('Ctrl Pts',(16.621279911401,19.3460852393745,16.7210871332558));
#189921=CARTESIAN_POINT('Ctrl Pts',(16.618172337624,19.292714307176,16.717838498664));
#189922=CARTESIAN_POINT('Ctrl Pts',(16.6169788916403,19.2513134328802,16.7152843270478));
#189923=CARTESIAN_POINT('Ctrl Pts',(16.6170878341668,19.0404276598584,16.7020917041995));
#189924=CARTESIAN_POINT('Ctrl Pts',(16.6375272230776,18.8715947971973,16.6908605299796));
#189925=CARTESIAN_POINT('Ctrl Pts',(16.702560257478,18.6062621558145,16.672847566007));
#189926=CARTESIAN_POINT('Ctrl Pts',(16.7346397979375,18.507423998555,16.666071013703));
#189927=CARTESIAN_POINT('Ctrl Pts',(16.7775028812636,18.4023580070007,16.6590602237326));
#189928=CARTESIAN_POINT('Ctrl Pts',(16.7812238447903,18.3934132191032,16.6584649950007));
#189929=CARTESIAN_POINT('Ctrl Pts',(16.7868091126874,18.3802425294775,16.657591313127));
#189930=CARTESIAN_POINT('Ctrl Pts',(16.7886259927346,18.3759968268016,16.657310098822));
#189931=CARTESIAN_POINT('Ctrl Pts',(16.7918742110363,18.3684745083349,16.6568126585519));
#189932=CARTESIAN_POINT('Ctrl Pts',(16.7932999703368,18.365195542807,16.6565960981773));
#189933=CARTESIAN_POINT('Ctrl Pts',(16.7963728345764,18.3581772384418,16.6561331672323));
#189934=CARTESIAN_POINT('Ctrl Pts',(16.7980224551061,18.3544390616336,16.6558869531772));
#189935=CARTESIAN_POINT('Ctrl Pts',(16.8025810939232,18.3441892523944,16.655212773983));
#189936=CARTESIAN_POINT('Ctrl Pts',(16.8055122412708,18.3376874381741,16.6547861426865));
#189937=CARTESIAN_POINT('Ctrl Pts',(16.8213484150772,18.3030284875306,16.652516757392));
#189938=CARTESIAN_POINT('Ctrl Pts',(16.8348380844036,18.2751407161349,16.6507078494936));
#189939=CARTESIAN_POINT('Ctrl Pts',(16.9233519990827,18.1019550748452,16.6395211976233));
#189940=CARTESIAN_POINT('Ctrl Pts',(17.0143947981724,17.9654490679667,16.6308786786183));
#189941=CARTESIAN_POINT('Ctrl Pts',(17.1964661805042,17.7510195854767,16.6154835399497));
#189942=CARTESIAN_POINT('Ctrl Pts',(17.2800216307166,17.6677908082219,16.6089132926449));
#189943=CARTESIAN_POINT('Ctrl Pts',(17.3809923290847,17.5827298217725,16.6011789747488));
#189944=CARTESIAN_POINT('Ctrl Pts',(17.3920227710195,17.5736269109291,16.6003367972576));
#189945=CARTESIAN_POINT('Ctrl Pts',(17.4097221145588,17.5593194556075,16.5989893461463));
#189946=CARTESIAN_POINT('Ctrl Pts',(17.4163315615324,17.5540418165527,16.5984870197534));
#189947=CARTESIAN_POINT('Ctrl Pts',(17.4280424984634,17.5448050228377,16.5975983792116));
#189948=CARTESIAN_POINT('Ctrl Pts',(17.4331308376923,17.5408293144498,16.5972127321872));
#189949=CARTESIAN_POINT('Ctrl Pts',(17.443691252499,17.5326556067532,16.5964132666152));
#189950=CARTESIAN_POINT('Ctrl Pts',(17.4491658064831,17.5284609485545,16.595999322277));
#189951=CARTESIAN_POINT('Ctrl Pts',(17.4632677550172,17.5177648534525,16.5949342653797));
#189952=CARTESIAN_POINT('Ctrl Pts',(17.4719245154293,17.5113026256377,16.5942816258302));
#189953=CARTESIAN_POINT('Ctrl Pts',(17.5082358350089,17.4846267580573,16.5915486303661));
#189954=CARTESIAN_POINT('Ctrl Pts',(17.536328225208,17.4650204860326,16.5894450084457));
#189955=CARTESIAN_POINT('Ctrl Pts',(17.6107288256385,17.4157353769852,16.5838980506992));
#189956=CARTESIAN_POINT('Ctrl Pts',(17.6577375167945,17.3871657287952,16.5804164588884));
#189957=CARTESIAN_POINT('Ctrl Pts',(17.801346532386,17.3073736054511,16.5698574783396));
#189958=CARTESIAN_POINT('Ctrl Pts',(17.9008524439255,17.261769992505,16.5626316640186));
#189959=CARTESIAN_POINT('Ctrl Pts',(18.039394298169,17.2108298469172,16.5528807495674));
#189960=CARTESIAN_POINT('Ctrl Pts',(18.0757169552015,17.1985832302097,16.5503529715578));
#189961=CARTESIAN_POINT('Ctrl Pts',(18.1433448553178,17.177808749775,16.5457180079641));
#189962=CARTESIAN_POINT('Ctrl Pts',(18.1745528341501,17.169001182349,16.5436066233097));
#189963=CARTESIAN_POINT('Ctrl Pts',(18.212137643054,17.1593203262083,16.5411051345695));
#189964=CARTESIAN_POINT('Ctrl Pts',(18.2183307334069,17.1577550042924,16.5406942824693));
#189965=CARTESIAN_POINT('Ctrl Pts',(18.2666531635486,17.1457737901268,16.5374993986305));
#189966=CARTESIAN_POINT('Ctrl Pts',(18.309090097105,17.13662671331,16.5347576356891));
#189967=CARTESIAN_POINT('Ctrl Pts',(18.3591675801458,17.1274342940059,16.5316198059652));
#189968=CARTESIAN_POINT('Ctrl Pts',(18.3665610632222,17.1261177429526,16.5311590135902));
#189969=CARTESIAN_POINT('Ctrl Pts',(18.3785177425675,17.124054207189,16.5304179989488));
#189970=CARTESIAN_POINT('Ctrl Pts',(18.3830765787805,17.1232827943285,16.5301364438628));
#189971=CARTESIAN_POINT('Ctrl Pts',(18.3911658570303,17.1219412313611,16.5296386267069));
#189972=CARTESIAN_POINT('Ctrl Pts',(18.3946952499603,17.1213650855483,16.5294220283407));
#189973=CARTESIAN_POINT('Ctrl Pts',(18.4022569537474,17.1201503598322,16.5289592658243));
#189974=CARTESIAN_POINT('Ctrl Pts',(18.4062896456748,17.1195145014028,16.5287132568855));
#189975=CARTESIAN_POINT('Ctrl Pts',(18.4173566531271,17.117802295488,16.5280402178807));
#189976=CARTESIAN_POINT('Ctrl Pts',(18.4243946703043,17.116749732627,16.5276145141493));
#189977=CARTESIAN_POINT('Ctrl Pts',(18.4618791162159,17.1113368816409,16.5253588792002));
#189978=CARTESIAN_POINT('Ctrl Pts',(18.492414256584,17.1076047593987,16.523562310079));
#189979=CARTESIAN_POINT('Ctrl Pts',(18.584888629601,17.0983427349107,16.5182155740101));
#189980=CARTESIAN_POINT('Ctrl Pts',(18.6470032789016,17.0948743852522,16.514750696061));
#189981=CARTESIAN_POINT('Ctrl Pts',(18.8561893653951,17.0924221438487,16.5032496679188));
#189982=CARTESIAN_POINT('Ctrl Pts',(19.0029705058823,17.1060159321909,16.4954296952454));
#189983=CARTESIAN_POINT('Ctrl Pts',(19.2201483498836,17.1492320882218,16.4830634215144));
#189984=CARTESIAN_POINT('Ctrl Pts',(19.2923125597153,17.1675929203147,16.4788225186518));
#189985=CARTESIAN_POINT('Ctrl Pts',(19.3758670947347,17.1936087766758,16.473687661536));
#189986=CARTESIAN_POINT('Ctrl Pts',(19.3883419999393,17.1976204404449,16.4729150804174));
#189987=CARTESIAN_POINT('Ctrl Pts',(19.4085551339427,17.2043282518725,16.4716532531572));
#189988=CARTESIAN_POINT('Ctrl Pts',(19.4163164830941,17.2069540056485,16.4711663272382));
#189989=CARTESIAN_POINT('Ctrl Pts',(19.4301121917377,17.2117106840662,16.4702964330498));
#189990=CARTESIAN_POINT('Ctrl Pts',(19.4361525305248,17.2138240501195,16.4699140507445));
#189991=CARTESIAN_POINT('Ctrl Pts',(19.4488620289639,17.218335575704,16.4691062592796));
#189992=CARTESIAN_POINT('Ctrl Pts',(19.4555289026579,17.2207398991496,16.4686806487239));
#189993=CARTESIAN_POINT('Ctrl Pts',(19.4731358310597,17.2271897083577,16.46755159351));
#189994=CARTESIAN_POINT('Ctrl Pts',(19.484054625507,17.2312921679688,16.4668462527708));
#189995=CARTESIAN_POINT('Ctrl Pts',(19.534679482511,17.2507921006258,16.4635514427574));
#189996=CARTESIAN_POINT('Ctrl Pts',(19.5739467578328,17.2672943445876,16.4609250660654));
#189997=CARTESIAN_POINT('Ctrl Pts',(19.6808049399562,17.3160448259265,16.4535752855994));
#189998=CARTESIAN_POINT('Ctrl Pts',(19.747219281087,17.3507098368175,16.4487751085701));
#189999=CARTESIAN_POINT('Ctrl Pts',(19.9505280367823,17.4709481445123,16.4333851190777));
#190000=CARTESIAN_POINT('Ctrl Pts',(20.0795525272035,17.5686822305257,16.4225220026474));
#190001=CARTESIAN_POINT('Ctrl Pts',(20.224495956478,17.7071251808197,16.4097036822652));
#190002=CARTESIAN_POINT('Ctrl Pts',(20.2520178616942,17.7349106104409,16.4072404220939));
#190003=CARTESIAN_POINT('Ctrl Pts',(20.2837411157461,17.7687640199376,16.4043825205715));
#190004=CARTESIAN_POINT('Ctrl Pts',(20.2886986039635,17.774109467504,16.4039353497376));
#190005=CARTESIAN_POINT('Ctrl Pts',(20.2967102016839,17.7828380359052,16.4032119417372));
#190006=CARTESIAN_POINT('Ctrl Pts',(20.2997811254766,17.7862055453039,16.4029344702753));
#190007=CARTESIAN_POINT('Ctrl Pts',(20.3052379551506,17.7922283373583,16.402441138735));
#190008=CARTESIAN_POINT('Ctrl Pts',(20.3076280367449,17.7948797561537,16.4022249649996));
#190009=CARTESIAN_POINT('Ctrl Pts',(20.3127661517649,17.8006087562576,16.4017600432424));
#190010=CARTESIAN_POINT('Ctrl Pts',(20.3155118899632,17.8036883198961,16.4015114665818));
#190011=CARTESIAN_POINT('Ctrl Pts',(20.3230995124472,17.8122486919477,16.4008241221562));
#190012=CARTESIAN_POINT('Ctrl Pts',(20.3279220797709,17.817746652829,16.4003867762728));
#190013=CARTESIAN_POINT('Ctrl Pts',(20.3547444705111,17.848647026923,16.3979508884506));
#190014=CARTESIAN_POINT('Ctrl Pts',(20.3761668454562,17.8745470077442,16.3959923481967));
#190015=CARTESIAN_POINT('Ctrl Pts',(20.4412124468213,17.9571151169236,16.3899642859086));
#190016=CARTESIAN_POINT('Ctrl Pts',(20.482589594342,18.0154927328052,16.3860076714569));
#190017=CARTESIAN_POINT('Ctrl Pts',(20.5429465993985,18.1105063385437,16.3798505009514));
#190018=CARTESIAN_POINT('Ctrl Pts',(20.5639455136523,18.145789414133,16.3776214270986));
#190019=CARTESIAN_POINT('Ctrl Pts',(20.6583766843838,18.3154990533026,16.3670747101152));
#190020=CARTESIAN_POINT('Ctrl Pts',(20.7180951192703,18.4570057854318,16.3587457285326));
#190021=CARTESIAN_POINT('Ctrl Pts',(20.7689033717466,18.626678043596,16.3484638515463));
#190022=CARTESIAN_POINT('Ctrl Pts',(20.7753904899178,18.6497614768637,16.3470600861361));
#190023=CARTESIAN_POINT('Ctrl Pts',(20.7839518867568,18.6823407995586,16.345069942165));
#190024=CARTESIAN_POINT('Ctrl Pts',(20.7863551308774,18.6917489044613,16.344494206495));
#190025=CARTESIAN_POINT('Ctrl Pts',(20.7901377398609,18.7069934945601,16.3435595128754));
#190026=CARTESIAN_POINT('Ctrl Pts',(20.7915571947188,18.7128199601271,16.3432018528114));
#190027=CARTESIAN_POINT('Ctrl Pts',(20.7944636216607,18.7249743655636,16.3424548386266));
#190028=CARTESIAN_POINT('Ctrl Pts',(20.7959462411955,18.7313032723961,16.3420653486577));
#190029=CARTESIAN_POINT('Ctrl Pts',(20.799381494115,18.7462776736658,16.3411425467131));
#190030=CARTESIAN_POINT('Ctrl Pts',(20.8013090161772,18.7549287503857,16.3406084343721));
#190031=CARTESIAN_POINT('Ctrl Pts',(20.8075221734102,18.7836634661622,16.3388309615162));
#190032=CARTESIAN_POINT('Ctrl Pts',(20.8115698005841,18.8037968641545,16.337580026374));
#190033=CARTESIAN_POINT('Ctrl Pts',(20.8314782480676,18.910862404558,16.3308965939813));
#190034=CARTESIAN_POINT('Ctrl Pts',(20.8421754222857,18.9986546603401,16.3253022103307));
#190035=CARTESIAN_POINT('Ctrl Pts',(20.8550353117621,19.2175624178871,16.3111031703415));
#190036=CARTESIAN_POINT('Ctrl Pts',(20.8505699181128,19.3487024208538,16.3023645922308));
#190037=CARTESIAN_POINT('Ctrl Pts',(20.8292590227255,19.5159566727771,16.2913124790122));
#190038=CARTESIAN_POINT('Ctrl Pts',(20.8234988295758,19.5532043442221,16.2888590613911));
#190039=CARTESIAN_POINT('Ctrl Pts',(20.8085427384265,19.635333049971,16.2834921737488));
#190040=CARTESIAN_POINT('Ctrl Pts',(20.7988778753951,19.6801120962688,16.2805945839741));
#190041=CARTESIAN_POINT('Ctrl Pts',(20.7859168049057,19.7319458812973,16.2773008926848));
#190042=CARTESIAN_POINT('Ctrl Pts',(20.7840263901472,19.7393360570858,16.2768327487511));
#190043=CARTESIAN_POINT('Ctrl Pts',(20.780929639554,19.7511752458745,16.2760852869147));
#190044=CARTESIAN_POINT('Ctrl Pts',(20.7797486660075,19.7556307391212,16.2758045640693));
#190045=CARTESIAN_POINT('Ctrl Pts',(20.7776237389928,19.7635430784875,16.2753071022196));
#190046=CARTESIAN_POINT('Ctrl Pts',(20.7766855502521,19.767001424159,16.2750900338363));
#190047=CARTESIAN_POINT('Ctrl Pts',(20.7746697822938,19.7743579643213,16.2746290758649));
#190048=CARTESIAN_POINT('Ctrl Pts',(20.7735898148796,19.7782554486306,16.2743853269422));
#190049=CARTESIAN_POINT('Ctrl Pts',(20.7706253378867,19.7888360036352,16.273724825518));
#190050=CARTESIAN_POINT('Ctrl Pts',(20.7687190874887,19.7955130041981,16.2733093180115));
#190051=CARTESIAN_POINT('Ctrl Pts',(20.758825701485,19.8295315033812,16.2711984871581));
#190052=CARTESIAN_POINT('Ctrl Pts',(20.7503197718666,19.8567206049526,16.2695316531591));
#190053=CARTESIAN_POINT('Ctrl Pts',(20.7236962125246,19.93615886539,16.2646990407753));
#190054=CARTESIAN_POINT('Ctrl Pts',(20.7040766411596,19.9878817649128,16.2616004195423));
#190055=CARTESIAN_POINT('Ctrl Pts',(20.6279151111834,20.1671529447908,16.250841529363));
#190056=CARTESIAN_POINT('Ctrl Pts',(20.5608244880492,20.2898220633271,16.2434223354561));
#190057=CARTESIAN_POINT('Ctrl Pts',(20.4312369283178,20.4795527097187,16.2307030373898));
#190058=CARTESIAN_POINT('Ctrl Pts',(20.375608594012,20.5507602502537,16.2255976687706));
#190059=CARTESIAN_POINT('Ctrl Pts',(20.306488425148,20.6284475178536,16.2195012888534));
#190060=CARTESIAN_POINT('Ctrl Pts',(20.2972674636175,20.6386106391665,16.2186927337745));
#190061=CARTESIAN_POINT('Ctrl Pts',(20.2823192451956,20.6547677183842,16.2173890926125));
#190062=CARTESIAN_POINT('Ctrl Pts',(20.2766543597056,20.660819034635,16.2168966581788));
#190063=CARTESIAN_POINT('Ctrl Pts',(20.2665317263132,20.6715056876137,16.2160194686251));
#190064=CARTESIAN_POINT('Ctrl Pts',(20.2620880977403,20.6761542989883,16.2156353254261));
#190065=CARTESIAN_POINT('Ctrl Pts',(20.2527842164345,20.6857989986069,16.2148329003311));
#190066=CARTESIAN_POINT('Ctrl Pts',(20.2479203387233,20.6907914679354,16.2144144625062));
#190067=CARTESIAN_POINT('Ctrl Pts',(20.2352221115373,20.7036972798069,16.2133247026955));
#190068=CARTESIAN_POINT('Ctrl Pts',(20.2273498981579,20.7115729144436,16.2126517147788));
#190069=CARTESIAN_POINT('Ctrl Pts',(20.1928651768653,20.745532497253,16.2097145428775));
#190070=CARTESIAN_POINT('Ctrl Pts',(20.1656300313635,20.7709720401183,16.2074225248212));
#190071=CARTESIAN_POINT('Ctrl Pts',(20.0914624691273,20.8366711127104,16.2012486613143));
#190072=CARTESIAN_POINT('Ctrl Pts',(20.0434163015008,20.8756136910291,16.1973168952285));
#190073=CARTESIAN_POINT('Ctrl Pts',(19.8779264279346,20.9981448460856,16.1840130226358));
#190074=CARTESIAN_POINT('Ctrl Pts',(19.7536638110197,21.0718425637511,16.1743708179557));
#190075=CARTESIAN_POINT('Ctrl Pts',(19.5561730937709,21.1632103471318,16.1601534545917));
#190076=CARTESIAN_POINT('Ctrl Pts',(19.4878797777643,21.190586187392,16.1554258374913));
#190077=CARTESIAN_POINT('Ctrl Pts',(19.4093591050794,21.2174067927065,16.15030157305));
#190078=CARTESIAN_POINT('Ctrl Pts',(19.4004041024093,21.2203988450572,16.1497216563738));
#190079=CARTESIAN_POINT('Ctrl Pts',(19.3870852358878,21.2247501231999,16.1488660996675));
#190080=CARTESIAN_POINT('Ctrl Pts',(19.3827366467357,21.2261552416896,16.1485878579399));
#190081=CARTESIAN_POINT('Ctrl Pts',(19.3749821542232,21.2286331748907,16.1480936856081));
#190082=CARTESIAN_POINT('Ctrl Pts',(19.3715780610609,21.2297114620852,16.1478774370711));
#190083=CARTESIAN_POINT('Ctrl Pts',(19.3642429340592,21.232014546315,16.1474129469189));
#190084=CARTESIAN_POINT('Ctrl Pts',(19.3603110623449,21.2332364862193,16.1471648735279));
#190085=CARTESIAN_POINT('Ctrl Pts',(19.3494226399989,21.2365855675942,16.1464803387246));
#190086=CARTESIAN_POINT('Ctrl Pts',(19.3424585761159,21.238688359219,16.1460452801959));
#190087=CARTESIAN_POINT('Ctrl Pts',(19.3038226743174,21.2501374563907,16.1436461723351));
#190088=CARTESIAN_POINT('Ctrl Pts',(19.2719444579931,21.2587781812171,16.1417207179608));
#190089=CARTESIAN_POINT('Ctrl Pts',(19.0823016222497,21.3054469577167,16.1305132437402));
#190090=CARTESIAN_POINT('Ctrl Pts',(18.9207760926261,21.3259818990315,16.121935265882));
#190091=CARTESIAN_POINT('Ctrl Pts',(18.6417834485212,21.3292077687061,16.1066601224681));
#190092=CARTESIAN_POINT('Ctrl Pts',(18.5251943999455,21.3209059261457,16.1001448248109));
#190093=CARTESIAN_POINT('Ctrl Pts',(18.3957719800454,21.300855248428,16.0924723578614));
#190094=CARTESIAN_POINT('Ctrl Pts',(18.3816749903978,21.2985249041794,16.0916309482477));
#190095=CARTESIAN_POINT('Ctrl Pts',(18.3592762883116,21.2945888782798,16.0902844963049));
#190096=CARTESIAN_POINT('Ctrl Pts',(18.3509585881051,21.2930758265259,16.0897823942899));
#190097=CARTESIAN_POINT('Ctrl Pts',(18.3363047984326,21.290319411796,16.0888940151354));
#190098=CARTESIAN_POINT('Ctrl Pts',(18.3299648808633,21.2890968001274,16.0885084038623));
#190099=CARTESIAN_POINT('Ctrl Pts',(18.3168631743454,21.2865079995885,16.0877088792968));
#190100=CARTESIAN_POINT('Ctrl Pts',(18.3101022792114,21.2851377264375,16.0872948395577));
#190101=CARTESIAN_POINT('Ctrl Pts',(18.2927644340792,21.2815354448603,16.086229256861));
#190102=CARTESIAN_POINT('Ctrl Pts',(18.2821977599815,21.2792554441323,16.0855761840006));
#190103=CARTESIAN_POINT('Ctrl Pts',(18.2381616067095,21.2694000759662,16.0828389909618));
#190104=CARTESIAN_POINT('Ctrl Pts',(18.2048628859242,21.261092749854,16.0807315152868));
#190105=CARTESIAN_POINT('Ctrl Pts',(18.1186329480229,21.2373394554466,16.0751719718688));
#190106=CARTESIAN_POINT('Ctrl Pts',(18.0660798099717,21.2206293178599,16.0716814313361));
#190107=CARTESIAN_POINT('Ctrl Pts',(17.8183605189002,21.1310723495553,16.0547497765255));
#190108=CARTESIAN_POINT('Ctrl Pts',(17.6340286963579,21.0317481243175,16.0405613082684));
#190109=CARTESIAN_POINT('Ctrl Pts',(17.4635472504763,20.9044164569456,16.0271469099946));
#190110=CARTESIAN_POINT('Ctrl Pts',(17.459929650207,20.9016963742497,16.0268621739342));
#190111=CARTESIAN_POINT('Ctrl Pts',(17.4399644348665,20.8865840077796,16.0252904001417));
#190112=CARTESIAN_POINT('Ctrl Pts',(17.423788203183,20.8739657033604,16.0240156419576));
#190113=CARTESIAN_POINT('Ctrl Pts',(17.4027742875478,20.8570767388507,16.0223607681787));
#190114=CARTESIAN_POINT('Ctrl Pts',(17.3977696868257,20.8530167722384,16.021966734501));
#190115=CARTESIAN_POINT('Ctrl Pts',(17.3897405835027,20.8464421696548,16.021334815623));
#190116=CARTESIAN_POINT('Ctrl Pts',(17.3867044593084,20.8439418837618,16.021095919218));
#190117=CARTESIAN_POINT('Ctrl Pts',(17.3810330768478,20.8392448448374,16.0206498049985));
#190118=CARTESIAN_POINT('Ctrl Pts',(17.37839619008,20.8370501469915,16.0204424447824));
#190119=CARTESIAN_POINT('Ctrl Pts',(17.3721594728651,20.8318335722181,16.0199521149872));
#190120=CARTESIAN_POINT('Ctrl Pts',(17.3685643265438,20.8288060800984,16.0196695545674));
#190121=CARTESIAN_POINT('Ctrl Pts',(17.3573283055216,20.8192800310532,16.0187866327351));
#190122=CARTESIAN_POINT('Ctrl Pts',(17.3497233865365,20.8127390171248,16.0181892933377));
#190123=CARTESIAN_POINT('Ctrl Pts',(17.3318906562942,20.7971791580403,16.0167884017336));
#190124=CARTESIAN_POINT('Ctrl Pts',(17.3217028098532,20.7881149609138,16.0159879186903));
#190125=CARTESIAN_POINT('Ctrl Pts',(17.2862676036678,20.7559692647704,16.0132001988145));
#190126=CARTESIAN_POINT('Ctrl Pts',(17.2614916193388,20.7323738661735,16.0112447046715));
#190127=CARTESIAN_POINT('Ctrl Pts',(17.1836200343751,20.6545274682123,16.0050355499663));
#190128=CARTESIAN_POINT('Ctrl Pts',(17.1328642362608,20.5980166581805,16.0008885283496));
#190129=CARTESIAN_POINT('Ctrl Pts',(16.9773509795776,20.4049278997275,15.987405588632));
#190130=CARTESIAN_POINT('Ctrl Pts',(16.8861939356731,20.2583230267282,15.97814116619));
#190131=CARTESIAN_POINT('Ctrl Pts',(16.8039965162978,20.0812386346228,15.9667992733134));
#190132=CARTESIAN_POINT('Ctrl Pts',(16.7945630666716,20.0600070948626,15.9654384283983));
#190133=CARTESIAN_POINT('Ctrl Pts',(16.7817336785057,20.0298022341832,15.9634992082359));
#190134=CARTESIAN_POINT('Ctrl Pts',(16.7780461753215,20.0209540233104,15.9629307507748));
#190135=CARTESIAN_POINT('Ctrl Pts',(16.7721583255951,20.0065513397011,15.9620047042708));
#190136=CARTESIAN_POINT('Ctrl Pts',(16.7699211488636,20.0010119966965,15.9616483659906));
#190137=CARTESIAN_POINT('Ctrl Pts',(16.7652920189449,19.9894088744396,15.9609015515739));
#190138=CARTESIAN_POINT('Ctrl Pts',(16.7629045691137,19.9833433765759,15.9605109282529));
#190139=CARTESIAN_POINT('Ctrl Pts',(16.7572999093651,19.968909057057,15.9595807591194));
#190140=CARTESIAN_POINT('Ctrl Pts',(16.7541077963288,19.9605306832021,15.9590403776587));
#190141=CARTESIAN_POINT('Ctrl Pts',(16.7491001803603,19.9471319197495,15.9581753838691));
#190142=CARTESIAN_POINT('Ctrl Pts',(16.747250275411,19.9421244949192,15.9578519361455));
#190143=CARTESIAN_POINT('Ctrl Pts',(16.7454193622843,19.9371102170485,15.9575278583994));
#190144=CARTESIAN_POINT('Ctrl Pts',(16.7454193680152,19.9371102327436,15.7328935264317));
#190145=CARTESIAN_POINT('Ctrl Pts',(16.798649296165,20.0828897568259,15.7430556461159));
#190146=CARTESIAN_POINT('Ctrl Pts',(16.8677537179851,20.2223914641028,15.7534874284883));
#190147=CARTESIAN_POINT('Ctrl Pts',(16.9691681762378,20.3806708068013,15.7654348636817));
#190148=CARTESIAN_POINT('Ctrl Pts',(16.9874716141485,20.4078291582142,15.7674874434137));
#190149=CARTESIAN_POINT('Ctrl Pts',(17.0105924212788,20.4404746693608,15.7699474701984));
#190150=CARTESIAN_POINT('Ctrl Pts',(17.0148164431233,20.4463742535236,15.7703917390174));
#190151=CARTESIAN_POINT('Ctrl Pts',(17.021482460663,20.4555841055966,15.7710846669077));
#190152=CARTESIAN_POINT('Ctrl Pts',(17.0239038680462,20.4589091066991,15.7713347044207));
#190153=CARTESIAN_POINT('Ctrl Pts',(17.0284457977148,20.4651078972136,15.7718005762138));
#190154=CARTESIAN_POINT('Ctrl Pts',(17.0305638780919,20.4679833465874,15.7720165672672));
#190155=CARTESIAN_POINT('Ctrl Pts',(17.0354125296699,20.4745309832887,15.7725081525716));
#190156=CARTESIAN_POINT('Ctrl Pts',(17.0381477316739,20.4781996784281,15.7727834194274));
#190157=CARTESIAN_POINT('Ctrl Pts',(17.0465812782217,20.4894352878942,15.7736260085721));
#190158=CARTESIAN_POINT('Ctrl Pts',(17.0523186213081,20.4969729686298,15.7741906742504));
#190159=CARTESIAN_POINT('Ctrl Pts',(17.1322494728731,20.6005357757961,15.7819443090162));
#190160=CARTESIAN_POINT('Ctrl Pts',(17.2145265084586,20.6900616502173,15.7886000137398));
#190161=CARTESIAN_POINT('Ctrl Pts',(17.3839409567636,20.8452498537013,15.8011016927523));
#190162=CARTESIAN_POINT('Ctrl Pts',(17.4693494968485,20.9122025499698,15.8069416369717));
#190163=CARTESIAN_POINT('Ctrl Pts',(17.6043723453465,21.0022394222406,15.8159742098848));
#190164=CARTESIAN_POINT('Ctrl Pts',(17.65036458098,21.0304314974606,15.8190177901784));
#190165=CARTESIAN_POINT('Ctrl Pts',(17.7169499389581,21.0678257620917,15.8234133557038));
#190166=CARTESIAN_POINT('Ctrl Pts',(17.7366921729607,21.0785036228313,15.8247152238287));
#190167=CARTESIAN_POINT('Ctrl Pts',(17.7717692385924,21.0967606971742,15.8270282161289));
#190168=CARTESIAN_POINT('Ctrl Pts',(17.7870333157027,21.1044718161461,15.8280346940689));
#190169=CARTESIAN_POINT('Ctrl Pts',(17.8097462614675,21.1156026250584,15.8295329803547));
#190170=CARTESIAN_POINT('Ctrl Pts',(17.8171244995112,21.1191654661722,15.8300197929981));
#190171=CARTESIAN_POINT('Ctrl Pts',(17.8300551778246,21.1253171859167,15.8308732028732));
#190172=CARTESIAN_POINT('Ctrl Pts',(17.8355985519317,21.1279249768118,15.8312391387822));
#190173=CARTESIAN_POINT('Ctrl Pts',(17.8466658480813,21.1330728571377,15.8319699184297));
#190174=CARTESIAN_POINT('Ctrl Pts',(17.8521895491263,21.135613283971,15.832334746131));
#190175=CARTESIAN_POINT('Ctrl Pts',(17.86543084042,21.1416341676935,15.8332095647526));
#190176=CARTESIAN_POINT('Ctrl Pts',(17.8731584706618,21.1450921727126,15.8337203218163));
#190177=CARTESIAN_POINT('Ctrl Pts',(17.9011809216221,21.1574306108246,15.8355733565837));
#190178=CARTESIAN_POINT('Ctrl Pts',(17.9215935298959,21.1660384673653,15.8369248828483));
#190179=CARTESIAN_POINT('Ctrl Pts',(18.113850674268,21.2435811101518,15.8496743496089));
#190180=CARTESIAN_POINT('Ctrl Pts',(18.2938780018495,21.2899988859761,15.861867295555));
#190181=CARTESIAN_POINT('Ctrl Pts',(18.5574473246742,21.3221582929071,15.8793984992523));
#190182=CARTESIAN_POINT('Ctrl Pts',(18.6377947894787,21.3273427106033,15.8846846200392));
#190183=CARTESIAN_POINT('Ctrl Pts',(18.7543554995945,21.328210086877,15.8921156550172));
#190184=CARTESIAN_POINT('Ctrl Pts',(18.7904675704436,21.3275549065075,15.8943844381591));
#190185=CARTESIAN_POINT('Ctrl Pts',(18.8340115187408,21.3256495013035,15.8970659502459));
#190186=CARTESIAN_POINT('Ctrl Pts',(18.8414738174711,21.3252833773237,15.897523565532));
#190187=CARTESIAN_POINT('Ctrl Pts',(18.8530883657383,21.3246518799665,15.8982326484044));
#190188=CARTESIAN_POINT('Ctrl Pts',(18.8572419497409,21.3244137623882,15.8984855997222));
#190189=CARTESIAN_POINT('Ctrl Pts',(18.8649541242802,21.3239488237626,15.8989540628619));
#190190=CARTESIAN_POINT('Ctrl Pts',(18.8685128101065,21.3237252586885,15.899169748845));
#190191=CARTESIAN_POINT('Ctrl Pts',(18.8765703417387,21.3231986242381,15.8996570276594));
#190192=CARTESIAN_POINT('Ctrl Pts',(18.8810687826348,21.3228901734265,15.8999283156869));
#190193=CARTESIAN_POINT('Ctrl Pts',(18.8926787532497,21.3220568210232,15.9006266089437));
#190194=CARTESIAN_POINT('Ctrl Pts',(18.8997887441138,21.3215103515271,15.901052433695));
#190195=CARTESIAN_POINT('Ctrl Pts',(18.9433832031951,21.3179380468659,15.9036529671433));
#190196=CARTESIAN_POINT('Ctrl Pts',(18.9797892582683,21.314001964283,15.9057800767962));
#190197=CARTESIAN_POINT('Ctrl Pts',(19.1851259419455,21.2863959549331,15.9176159526282));
#190198=CARTESIAN_POINT('Ctrl Pts',(19.3508232772645,21.2433198871099,15.9265904750258));
#190199=CARTESIAN_POINT('Ctrl Pts',(19.5983315838293,21.1458696185412,15.9412226533094));
#190200=CARTESIAN_POINT('Ctrl Pts',(19.6846225248531,21.1049649598781,15.9465714627196));
#190201=CARTESIAN_POINT('Ctrl Pts',(19.7865231736233,21.0479380994773,15.9533711087051));
#190202=CARTESIAN_POINT('Ctrl Pts',(19.8050306942982,21.0372091377588,15.9546263239892));
#190203=CARTESIAN_POINT('Ctrl Pts',(19.8310973880839,21.021565519011,15.9564246174336));
#190204=CARTESIAN_POINT('Ctrl Pts',(19.8387930384578,21.01687998381,15.9569593528522));
#190205=CARTESIAN_POINT('Ctrl Pts',(19.852011147903,21.0087159585043,15.9578845469219));
#190206=CARTESIAN_POINT('Ctrl Pts',(19.8575479032991,21.0052607675078,15.9582741443272));
#190207=CARTESIAN_POINT('Ctrl Pts',(19.8681142197278,20.998598812867,15.959021634657));
#190208=CARTESIAN_POINT('Ctrl Pts',(19.8731463853986,20.9953962818427,15.9593793680039));
#190209=CARTESIAN_POINT('Ctrl Pts',(19.8861873008786,20.9870192395026,15.9603110193446));
#190210=CARTESIAN_POINT('Ctrl Pts',(19.8941746799327,20.9818118541448,15.9608861606494));
#190211=CARTESIAN_POINT('Ctrl Pts',(19.9212440039383,20.9639022047959,15.9628509405072));
#190212=CARTESIAN_POINT('Ctrl Pts',(19.9401541806515,20.9509443934031,15.9642501627349));
#190213=CARTESIAN_POINT('Ctrl Pts',(20.1027544055856,20.8356013387163,15.9765200618686));
#190214=CARTESIAN_POINT('Ctrl Pts',(20.2333075397069,20.7159489120623,15.9881030304245));
#190215=CARTESIAN_POINT('Ctrl Pts',(20.4033899281471,20.5157156642508,16.0054603550539));
#190216=CARTESIAN_POINT('Ctrl Pts',(20.4552181534272,20.4465386132608,16.0111498467561));
#190217=CARTESIAN_POINT('Ctrl Pts',(20.5233718654834,20.3429254651327,16.0190667520285));
#190218=CARTESIAN_POINT('Ctrl Pts',(20.5432236627923,20.3109168489621,16.0214351157531));
#190219=CARTESIAN_POINT('Ctrl Pts',(20.5660251228071,20.2718629202117,16.0242178888107));
#190220=CARTESIAN_POINT('Ctrl Pts',(20.5698030123328,20.2653118561174,16.0246811472086));
#190221=CARTESIAN_POINT('Ctrl Pts',(20.5756146198721,20.2551082633819,16.025397051872));
#190222=CARTESIAN_POINT('Ctrl Pts',(20.5776727154793,20.2514697942198,16.0256512273712));
#190223=CARTESIAN_POINT('Ctrl Pts',(20.5814655033656,20.2447180056834,16.0261208109839));
#190224=CARTESIAN_POINT('Ctrl Pts',(20.5832030958854,20.2416064291786,16.0263364004861));
#190225=CARTESIAN_POINT('Ctrl Pts',(20.5871085248795,20.2345711451223,16.0268220143414));
#190226=CARTESIAN_POINT('Ctrl Pts',(20.5892717554082,20.2306449423905,16.0270917427712));
#190227=CARTESIAN_POINT('Ctrl Pts',(20.5956051302825,20.2190631605582,16.0278837328058));
#190228=CARTESIAN_POINT('Ctrl Pts',(20.5997405354619,20.2113885530217,16.0284038314477));
#190229=CARTESIAN_POINT('Ctrl Pts',(20.6288246234771,20.156605750428,16.032084565807));
#190230=CARTESIAN_POINT('Ctrl Pts',(20.6520357953407,20.1085913849861,16.0351439694482));
#190231=CARTESIAN_POINT('Ctrl Pts',(20.6801803883366,20.0442802424138,16.0390920077543));
#190232=CARTESIAN_POINT('Ctrl Pts',(20.6867643316702,20.0287319563941,16.040035283504));
#190233=CARTESIAN_POINT('Ctrl Pts',(20.7494957787683,19.8755090618825,16.049236327001));
#190234=CARTESIAN_POINT('Ctrl Pts',(20.791178896703,19.7323578258933,16.0571182818916));
#190235=CARTESIAN_POINT('Ctrl Pts',(20.8284375704663,19.525355079745,16.0687553370241));
#190236=CARTESIAN_POINT('Ctrl Pts',(20.8367008493418,19.4642511355015,16.0722143614867));
#190237=CARTESIAN_POINT('Ctrl Pts',(20.845656773595,19.3658460812898,16.0778853085104));
#190238=CARTESIAN_POINT('Ctrl Pts',(20.8480505961337,19.3287347319099,16.0800463871473));
#190239=CARTESIAN_POINT('Ctrl Pts',(20.8498893628458,19.2804623105875,16.0828940205839));
#190240=CARTESIAN_POINT('Ctrl Pts',(20.8502252226781,19.2693404503735,16.0835526163589));
#190241=CARTESIAN_POINT('Ctrl Pts',(20.8506288016836,19.2512501195905,16.0846281304933));
#190242=CARTESIAN_POINT('Ctrl Pts',(20.8507498196273,19.2442829621142,16.0850433744891));
#190243=CARTESIAN_POINT('Ctrl Pts',(20.8509163828866,19.2308844498395,16.0858439581539));
#190244=CARTESIAN_POINT('Ctrl Pts',(20.8509670221201,19.2244532271033,16.0862291335997));
#190245=CARTESIAN_POINT('Ctrl Pts',(20.8510158621952,19.2097287994672,16.0871131019139));
#190246=CARTESIAN_POINT('Ctrl Pts',(20.8509946380104,19.2014356748257,16.0876124982341));
#190247=CARTESIAN_POINT('Ctrl Pts',(20.8508088180962,19.1794069845139,16.0889431699681));
#190248=CARTESIAN_POINT('Ctrl Pts',(20.8505592628824,19.1656727041993,16.0897770911394));
#190249=CARTESIAN_POINT('Ctrl Pts',(20.847642924968,19.0611738681957,16.0961556453316));
#190250=CARTESIAN_POINT('Ctrl Pts',(20.8392729666025,18.970674733558,16.1018787170834));
#190251=CARTESIAN_POINT('Ctrl Pts',(20.8032169518968,18.7421961862168,16.1168166293391));
#190252=CARTESIAN_POINT('Ctrl Pts',(20.7675461240913,18.6059206361268,16.1262086367561));
#190253=CARTESIAN_POINT('Ctrl Pts',(20.6997948919733,18.423426085226,16.138950396088));
#190254=CARTESIAN_POINT('Ctrl Pts',(20.6790024772245,18.3733912655459,16.1424578490892));
#190255=CARTESIAN_POINT('Ctrl Pts',(20.6445440617357,18.2986954054887,16.1476623608274));
#190256=CARTESIAN_POINT('Ctrl Pts',(20.6322682925969,18.2734201622335,16.1494176254365));
#190257=CARTESIAN_POINT('Ctrl Pts',(20.6163492017089,18.2422387982106,16.1515689505226));
#190258=CARTESIAN_POINT('Ctrl Pts',(20.6131758667208,18.2360975185967,16.1519919686407));
#190259=CARTESIAN_POINT('Ctrl Pts',(20.6081015072515,18.2263940681131,16.1526591202728));
#190260=CARTESIAN_POINT('Ctrl Pts',(20.6062203077014,18.2228216655634,16.1529044713041));
#190261=CARTESIAN_POINT('Ctrl Pts',(20.6026494985042,18.2160874898472,16.1533664366449));
#190262=CARTESIAN_POINT('Ctrl Pts',(20.6009620989376,18.2129246659584,16.153583179108));
#190263=CARTESIAN_POINT('Ctrl Pts',(20.5970811346228,18.2056945541227,16.1540781451266));
#190264=CARTESIAN_POINT('Ctrl Pts',(20.5948822835497,18.2016301562877,16.1543560288928));
#190265=CARTESIAN_POINT('Ctrl Pts',(20.5889995002765,18.1908408711129,16.1550928209504));
#190266=CARTESIAN_POINT('Ctrl Pts',(20.5852922715274,18.1841286722828,16.1555502857045));
#190267=CARTESIAN_POINT('Ctrl Pts',(20.5587898300362,18.136754170811,16.1587736854552));
#190268=CARTESIAN_POINT('Ctrl Pts',(20.5346916604486,18.0968311278959,16.1614620175247));
#190269=CARTESIAN_POINT('Ctrl Pts',(20.5068104135783,18.0539118424543,16.1643572851687));
#190270=CARTESIAN_POINT('Ctrl Pts',(20.5043155392453,18.0500983423103,16.1646145830395));
#190271=CARTESIAN_POINT('Ctrl Pts',(20.488969728268,18.0268062605546,16.1661865693144));
#190272=CARTESIAN_POINT('Ctrl Pts',(20.4758094394637,18.0075327208593,16.1674893430066));
#190273=CARTESIAN_POINT('Ctrl Pts',(20.4360570578272,17.9513329362194,16.171305918791));
#190274=CARTESIAN_POINT('Ctrl Pts',(20.4085897080285,17.9150413268474,16.1737939066428));
#190275=CARTESIAN_POINT('Ctrl Pts',(20.3112066931709,17.794643740989,16.1822246670852));
#190276=CARTESIAN_POINT('Ctrl Pts',(20.2359567802148,17.7150819033435,16.1881126748508));
#190277=CARTESIAN_POINT('Ctrl Pts',(20.114050299562,17.604703929634,16.1972568195374));
#190278=CARTESIAN_POINT('Ctrl Pts',(20.0717731715553,17.5693276236869,16.2003642261836));
#190279=CARTESIAN_POINT('Ctrl Pts',(20.0010165055719,17.5146701011694,16.2055080717713));
#190280=CARTESIAN_POINT('Ctrl Pts',(19.9733622008392,17.4943616893447,16.2075051263755));
#190281=CARTESIAN_POINT('Ctrl Pts',(19.9363628904862,17.4685507726437,16.2101657079852));
#190282=CARTESIAN_POINT('Ctrl Pts',(19.9274509037726,17.4624346554793,16.2108057081413));
#190283=CARTESIAN_POINT('Ctrl Pts',(19.9127752658781,17.4525275216718,16.2118584073516));
#190284=CARTESIAN_POINT('Ctrl Pts',(19.90703916,17.4486959082331,16.2122695651647));
#190285=CARTESIAN_POINT('Ctrl Pts',(19.895897860404,17.441332219655,16.2130676327694));
#190286=CARTESIAN_POINT('Ctrl Pts',(19.8904950265971,17.437796700086,16.2134544071935));
#190287=CARTESIAN_POINT('Ctrl Pts',(19.8779803864307,17.4296888652459,16.2143497908));
#190288=CARTESIAN_POINT('Ctrl Pts',(19.8708572297909,17.4251343501905,16.2148590561349));
#190289=CARTESIAN_POINT('Ctrl Pts',(19.8516216643843,17.4129969343518,16.2162333858252));
#190290=CARTESIAN_POINT('Ctrl Pts',(19.8394596046722,17.4054939059916,16.2171013783888));
#190291=CARTESIAN_POINT('Ctrl Pts',(19.7271455684354,17.3377652633615,16.225109693091));
#190292=CARTESIAN_POINT('Ctrl Pts',(19.6222596899661,17.2858160057403,16.2325518841576));
#190293=CARTESIAN_POINT('Ctrl Pts',(19.3623086207889,17.1828452886543,16.250815473679));
#190294=CARTESIAN_POINT('Ctrl Pts',(19.2045739553356,17.140554760647,16.261777048255));
#190295=CARTESIAN_POINT('Ctrl Pts',(19.0114487639915,17.1120087278553,16.2741813369229));
#190296=CARTESIAN_POINT('Ctrl Pts',(18.9792379167669,17.108001947539,16.2762152492726));
#190297=CARTESIAN_POINT('Ctrl Pts',(18.9397465779168,17.1040093253315,16.2786560409544));
#190298=CARTESIAN_POINT('Ctrl Pts',(18.932543626788,17.1033183852372,16.2790990806765));
#190299=CARTESIAN_POINT('Ctrl Pts',(18.921245130674,17.1022930161781,16.2797905194299));
#190300=CARTESIAN_POINT('Ctrl Pts',(18.9171519926541,17.1019335641496,16.2800402873708));
#190301=CARTESIAN_POINT('Ctrl Pts',(18.9094985901133,17.1012839043892,16.2805059252253));
#190302=CARTESIAN_POINT('Ctrl Pts',(18.9059386769187,17.1009907936646,16.2807219502892));
#190303=CARTESIAN_POINT('Ctrl Pts',(18.8978098879825,17.1003422066326,16.2812139604061));
#190304=CARTESIAN_POINT('Ctrl Pts',(18.8932405980202,17.0999925549749,16.2814896158611));
#190305=CARTESIAN_POINT('Ctrl Pts',(18.8791897228984,17.0989632329472,16.2823345783945));
#190306=CARTESIAN_POINT('Ctrl Pts',(18.8697045159721,17.0983325739754,16.2829012070692));
#190307=CARTESIAN_POINT('Ctrl Pts',(18.7843094169465,17.0932322598706,16.2879711816293));
#190308=CARTESIAN_POINT('Ctrl Pts',(18.7082055370106,17.0927912042934,16.2922673184702));
#190309=CARTESIAN_POINT('Ctrl Pts',(18.5898142193461,17.0984888947453,16.2988269151612));
#190310=CARTESIAN_POINT('Ctrl Pts',(18.5474631514448,17.1018065770426,16.3011484917261));
#190311=CARTESIAN_POINT('Ctrl Pts',(18.3965607753392,17.1182089445687,16.3094124871073));
#190312=CARTESIAN_POINT('Ctrl Pts',(18.2889612819218,17.1384220680059,16.3152990684544));
#190313=CARTESIAN_POINT('Ctrl Pts',(18.1302306210038,17.181176224433,16.3244398970179));
#190314=CARTESIAN_POINT('Ctrl Pts',(18.0776353898719,17.197568382791,16.3275454029792));
#190315=CARTESIAN_POINT('Ctrl Pts',(17.9934267504993,17.2274637329885,16.3326863827338));
#190316=CARTESIAN_POINT('Ctrl Pts',(17.9613968971506,17.2397189166488,16.3346825297147));
#190317=CARTESIAN_POINT('Ctrl Pts',(17.9196834614535,17.256852010237,16.337342073475));
#190318=CARTESIAN_POINT('Ctrl Pts',(17.9097185867692,17.2610343756639,16.3379819668263));
#190319=CARTESIAN_POINT('Ctrl Pts',(17.8934466771799,17.2680108877178,16.339034535108));
#190320=CARTESIAN_POINT('Ctrl Pts',(17.8871204258572,17.2707599210099,16.3394456695499));
#190321=CARTESIAN_POINT('Ctrl Pts',(17.874898385376,17.2761420960069,16.3402437237786));
#190322=CARTESIAN_POINT('Ctrl Pts',(17.8690009795456,17.2787713939406,16.3406305083675));
#190323=CARTESIAN_POINT('Ctrl Pts',(17.8554086032966,17.2849061140036,16.3415259621137));
#190324=CARTESIAN_POINT('Ctrl Pts',(17.8477224607008,17.288430724232,16.342035287747));
#190325=CARTESIAN_POINT('Ctrl Pts',(17.82710102126,17.2980369714698,16.3434098856754));
#190326=CARTESIAN_POINT('Ctrl Pts',(17.8142060341976,17.3042036419934,16.3442780879574));
#190327=CARTESIAN_POINT('Ctrl Pts',(17.6962262749071,17.3620994183613,16.3523026074465));
#190328=CARTESIAN_POINT('Ctrl Pts',(17.5955586539415,17.422326998344,16.3597622125767));
#190329=CARTESIAN_POINT('Ctrl Pts',(17.367434025814,17.5858981856016,16.3780996977287));
#190330=CARTESIAN_POINT('Ctrl Pts',(17.2459722509986,17.6963277257559,16.389119972739));
#190331=CARTESIAN_POINT('Ctrl Pts',(17.117757460286,17.8433599360849,16.4015037920746));
#190332=CARTESIAN_POINT('Ctrl Pts',(17.0976052266923,17.8675374279079,16.4034746846704));
#190333=CARTESIAN_POINT('Ctrl Pts',(17.0735333306354,17.897763231609,16.4058504009895));
#190334=CARTESIAN_POINT('Ctrl Pts',(17.0690967026126,17.9033924963277,16.4062891936979));
#190335=CARTESIAN_POINT('Ctrl Pts',(17.0621710203954,17.9122723065533,16.4069754851807));
#190336=CARTESIAN_POINT('Ctrl Pts',(17.0596627079737,17.9155076642614,16.4072243201402));
#190337=CARTESIAN_POINT('Ctrl Pts',(17.0549819730716,17.9215814330644,16.4076891564889));
#190338=CARTESIAN_POINT('Ctrl Pts',(17.0528073788356,17.9244180374856,16.4079053073909));
#190339=CARTESIAN_POINT('Ctrl Pts',(17.0478470220042,17.9309225227607,16.4083988249066));
#190340=CARTESIAN_POINT('Ctrl Pts',(17.0450660431875,17.9345939896003,16.4086758541378));
#190341=CARTESIAN_POINT('Ctrl Pts',(17.0378179753301,17.9442281002328,16.4093988628795));
#190342=CARTESIAN_POINT('Ctrl Pts',(17.0333702970708,17.9502053600729,16.4098435184231));
#190343=CARTESIAN_POINT('Ctrl Pts',(17.0039151614196,17.9902297453776,16.4127958637098));
#190344=CARTESIAN_POINT('Ctrl Pts',(16.9798982154478,18.0249978788322,16.4152399451527));
#190345=CARTESIAN_POINT('Ctrl Pts',(16.9164802646476,18.1229502658144,16.4218683499696));
#190346=CARTESIAN_POINT('Ctrl Pts',(16.879345473118,18.1875312487987,16.4259561004834));
#190347=CARTESIAN_POINT('Ctrl Pts',(16.7951473099761,18.3536567690705,16.4361043535853));
#190348=CARTESIAN_POINT('Ctrl Pts',(16.7525863198119,18.4572187109612,16.4421169523245));
#190349=CARTESIAN_POINT('Ctrl Pts',(16.6925866267997,18.6440362425383,16.4530200342531));
#190350=CARTESIAN_POINT('Ctrl Pts',(16.6716050222464,18.7258804430973,16.4578124414119));
#190351=CARTESIAN_POINT('Ctrl Pts',(16.6528673353708,18.8226990582388,16.4636013851176));
#190352=CARTESIAN_POINT('Ctrl Pts',(16.6503087130178,18.8366720756136,16.4644395967754));
#190353=CARTESIAN_POINT('Ctrl Pts',(16.6465902583743,18.8581998192184,16.4657356130468));
#190354=CARTESIAN_POINT('Ctrl Pts',(16.6453303599058,18.8657370144409,16.4661902340614));
#190355=CARTESIAN_POINT('Ctrl Pts',(16.6431068637687,18.879496549896,16.4670218101922));
#190356=CARTESIAN_POINT('Ctrl Pts',(16.6421301613088,18.88571670621,16.4673983444065));
#190357=CARTESIAN_POINT('Ctrl Pts',(16.640058022992,18.8993085841728,16.4682224938568));
#190358=CARTESIAN_POINT('Ctrl Pts',(16.6389737394845,18.9066818978219,16.4686704574311));
#190359=CARTESIAN_POINT('Ctrl Pts',(16.6361094461709,18.9269007237399,16.4699013269525));
#190360=CARTESIAN_POINT('Ctrl Pts',(16.6344085230054,18.9397569491901,16.4706867213659));
#190361=CARTESIAN_POINT('Ctrl Pts',(16.6263685201414,19.0051410896655,16.4746955644089));
#190362=CARTESIAN_POINT('Ctrl Pts',(16.6218825847436,19.057873946071,16.4779768426548));
#190363=CARTESIAN_POINT('Ctrl Pts',(16.6177663611262,19.1446700859844,16.4834601060915));
#190364=CARTESIAN_POINT('Ctrl Pts',(16.616974210654,19.1786565835547,16.4856276638605));
#190365=CARTESIAN_POINT('Ctrl Pts',(16.6171022081697,19.3432687734638,16.496218879237));
#190366=CARTESIAN_POINT('Ctrl Pts',(16.6292932870494,19.473594526131,16.504910420684));
#190367=CARTESIAN_POINT('Ctrl Pts',(16.6709615317538,19.6953469514709,16.5197603295542));
#190368=CARTESIAN_POINT('Ctrl Pts',(16.6947819252022,19.7874664799454,16.5259401167032));
#190369=CARTESIAN_POINT('Ctrl Pts',(16.7277657538097,19.8868749541636,16.5324111822769));
#190370=CARTESIAN_POINT('Ctrl Pts',(16.7308789356001,19.8960465778259,16.5330062690486));
#190371=CARTESIAN_POINT('Ctrl Pts',(16.7355692054707,19.9095590038365,16.5338797830683));
#190372=CARTESIAN_POINT('Ctrl Pts',(16.7370976771217,19.9139163792231,16.5341609699816));
#190373=CARTESIAN_POINT('Ctrl Pts',(16.7398349366887,19.9216387860205,16.5346583799414));
#190374=CARTESIAN_POINT('Ctrl Pts',(16.7410380033822,19.9250057875421,16.5348749372459));
#190375=CARTESIAN_POINT('Ctrl Pts',(16.7432997957639,19.931285569357,16.5352782394492));
#190376=CARTESIAN_POINT('Ctrl Pts',(16.7443563783493,19.9341990484388,16.5354651119654));
#190377=CARTESIAN_POINT('Ctrl Pts',(16.7454193623258,19.9371102171621,16.5356516081066));
#190378=CARTESIAN_POINT('Origin',(18.734,19.211,0.));
#190379=CARTESIAN_POINT('',(16.7454193509487,19.937110186004,17.5536949115506));
#190380=CARTESIAN_POINT('',(16.7454194652257,19.9371104989717,17.3329785907215));
#190381=CARTESIAN_POINT('',(16.7454193623258,19.9371102171621,0.));
#190382=CARTESIAN_POINT('',(16.6170009797991,19.2127872412316,17.5117108633035));
#190383=CARTESIAN_POINT('Ctrl Pts',(16.7454193509487,19.937110186004,17.5536949115506));
#190384=CARTESIAN_POINT('Ctrl Pts',(16.7414203484773,19.9261582133096,17.5529593386965));
#190385=CARTESIAN_POINT('Ctrl Pts',(16.7375110411194,19.9151710662913,17.5522275673665));
#190386=CARTESIAN_POINT('Ctrl Pts',(16.7285976735804,19.8894486603001,17.5505296495991));
#190387=CARTESIAN_POINT('Ctrl Pts',(16.7236654571562,19.874691294042,17.5495671222079));
#190388=CARTESIAN_POINT('Ctrl Pts',(16.71712756313,19.8543878070169,17.5482599832547));
#190389=CARTESIAN_POINT('Ctrl Pts',(16.7153813400418,19.8488879245489,17.5479076128735));
#190390=CARTESIAN_POINT('Ctrl Pts',(16.7126398285665,19.8401292920733,17.5473492557316));
#190391=CARTESIAN_POINT('Ctrl Pts',(16.7116298969789,19.8368752076809,17.5471424223113));
#190392=CARTESIAN_POINT('Ctrl Pts',(16.7095583186972,19.8301430390956,17.5467158036132));
#190393=CARTESIAN_POINT('Ctrl Pts',(16.7084977766896,19.8266646549669,17.5464960889765));
#190394=CARTESIAN_POINT('Ctrl Pts',(16.7059888775804,19.8183592714762,17.5459731353955));
#190395=CARTESIAN_POINT('Ctrl Pts',(16.7045487725742,19.8135297619212,17.545670377959));
#190396=CARTESIAN_POINT('Ctrl Pts',(16.6997356750759,19.7971756124328,17.5446495209159));
#190397=CARTESIAN_POINT('Ctrl Pts',(16.6964434236498,19.785627188258,17.5439359715136));
#190398=CARTESIAN_POINT('Ctrl Pts',(16.6887613677531,19.7577839608348,17.5422317975928));
#190399=CARTESIAN_POINT('Ctrl Pts',(16.6844677230005,19.7414632360976,17.5412461317108));
#190400=CARTESIAN_POINT('Ctrl Pts',(16.6690505818285,19.6798768158442,17.5375704593111));
#190401=CARTESIAN_POINT('Ctrl Pts',(16.6592272448662,19.6342967519587,17.5349384179573));
#190402=CARTESIAN_POINT('Ctrl Pts',(16.6284575288223,19.4644733677277,17.5253353954585));
#190403=CARTESIAN_POINT('Ctrl Pts',(16.6171072209053,19.3387629515357,17.518611897998));
#190404=CARTESIAN_POINT('Ctrl Pts',(16.6170007560366,19.2127891501584,17.5117113586358));
#190405=CARTESIAN_POINT('Ctrl Pts',(16.6170007544063,19.2127872200763,17.5117112529106));
#190406=CARTESIAN_POINT('Ctrl Pts',(16.616930473988,19.1295386070637,17.5071510947737));
#190407=CARTESIAN_POINT('Ctrl Pts',(16.6217706304624,19.0463629764936,17.5025270244436));
#190408=CARTESIAN_POINT('Ctrl Pts',(16.6354866257038,18.9297561389935,17.4958024094825));
#190409=CARTESIAN_POINT('Ctrl Pts',(16.6402990166117,18.8959246220188,17.4938228583187));
#190410=CARTESIAN_POINT('Ctrl Pts',(16.6476156658052,18.8521206747072,17.4912164872332));
#190411=CARTESIAN_POINT('Ctrl Pts',(16.649376831497,18.8420281854468,17.4906129779659));
#190412=CARTESIAN_POINT('Ctrl Pts',(16.6524780221122,18.8249879314239,17.4895887618969));
#190413=CARTESIAN_POINT('Ctrl Pts',(16.6537797605833,18.8180333154182,17.4891692683912));
#190414=CARTESIAN_POINT('Ctrl Pts',(16.6564245117204,18.8042850546055,17.4883369974055));
#190415=CARTESIAN_POINT('Ctrl Pts',(16.6577660445911,18.7974912129556,17.4879242716445));
#190416=CARTESIAN_POINT('Ctrl Pts',(16.6604207091026,18.784386028315,17.4871252790189));
#190417=CARTESIAN_POINT('Ctrl Pts',(16.6617293838868,18.7780738531304,17.4867391587643));
#190418=CARTESIAN_POINT('Ctrl Pts',(16.6648076564294,18.7635601250018,17.4858483485752));
#190419=CARTESIAN_POINT('Ctrl Pts',(16.6665972140381,18.755362958199,17.4853430235871));
#190420=CARTESIAN_POINT('Ctrl Pts',(16.6715176924695,18.733450374863,17.4839861829964));
#190421=CARTESIAN_POINT('Ctrl Pts',(16.6747366394142,18.7197553459859,17.4831318540082));
#190422=CARTESIAN_POINT('Ctrl Pts',(16.7030000973699,18.6046704834507,17.475898054269));
#190423=CARTESIAN_POINT('Ctrl Pts',(16.7353754886842,18.5052447401283,17.4692799484978));
#190424=CARTESIAN_POINT('Ctrl Pts',(16.8068616716935,18.330706537951,17.4570211598824));
#190425=CARTESIAN_POINT('Ctrl Pts',(16.84339386114,18.2547646976231,17.4514527207453));
#190426=CARTESIAN_POINT('Ctrl Pts',(16.9294015456653,18.1002834487083,17.4397718882579));
#190427=CARTESIAN_POINT('Ctrl Pts',(16.9797192639681,18.0224006313024,17.4336727871492));
#190428=CARTESIAN_POINT('Ctrl Pts',(17.0536149814904,17.922989537048,17.4258114738714));
#190429=CARTESIAN_POINT('Ctrl Pts',(17.0728039593309,17.8983337371465,17.4238554125912));
#190430=CARTESIAN_POINT('Ctrl Pts',(17.0970484780719,17.8685657004768,17.421495043113));
#190431=CARTESIAN_POINT('Ctrl Pts',(17.1015923491996,17.8630439923162,17.4210572723664));
#190432=CARTESIAN_POINT('Ctrl Pts',(17.1087791026728,17.8544002934178,17.4203722198341));
#190433=CARTESIAN_POINT('Ctrl Pts',(17.1114031545307,17.8512628170358,17.4201236096888));
#190434=CARTESIAN_POINT('Ctrl Pts',(17.1163377107054,17.8453973866933,17.4196589644846));
#190435=CARTESIAN_POINT('Ctrl Pts',(17.1186460052478,17.842667711582,17.4194427812764));
#190436=CARTESIAN_POINT('Ctrl Pts',(17.1239478200855,17.8364301605862,17.4189488915101));
#190437=CARTESIAN_POINT('Ctrl Pts',(17.1269458898656,17.8329262162364,17.418671524249));
#190438=CARTESIAN_POINT('Ctrl Pts',(17.1348298900091,17.8237726398275,17.4179470525435));
#190439=CARTESIAN_POINT('Ctrl Pts',(17.1397343612873,17.8181389636981,17.4175012808001));
#190440=CARTESIAN_POINT('Ctrl Pts',(17.1728156020896,17.7805428039361,17.4145262679844));
#190441=CARTESIAN_POINT('Ctrl Pts',(17.2019240875876,17.749408927122,17.4120617505356));
#190442=CARTESIAN_POINT('Ctrl Pts',(17.2835612398275,17.6672126147658,17.4054834610824));
#190443=CARTESIAN_POINT('Ctrl Pts',(17.3378328228301,17.6179617963119,17.4014605943982));
#190444=CARTESIAN_POINT('Ctrl Pts',(17.4635842510242,17.5152170791767,17.3926105447383));
#190445=CARTESIAN_POINT('Ctrl Pts',(17.5361100384896,17.4632313231011,17.3878053013982));
#190446=CARTESIAN_POINT('Ctrl Pts',(17.6722748825049,17.3780970939397,17.3789766371124));
#190447=CARTESIAN_POINT('Ctrl Pts',(17.7347273956491,17.3433152454516,17.3749940799317));
#190448=CARTESIAN_POINT('Ctrl Pts',(17.8232465646735,17.2997284884751,17.3693501776409));
#190449=CARTESIAN_POINT('Ctrl Pts',(17.8479069289927,17.2881714621802,17.3677782221454));
#190450=CARTESIAN_POINT('Ctrl Pts',(17.8909907883034,17.2689851299114,17.3650281590181));
#190451=CARTESIAN_POINT('Ctrl Pts',(17.9093120960237,17.2611343360064,17.363857573677));
#190452=CARTESIAN_POINT('Ctrl Pts',(17.9358134126304,17.2502186788277,17.3621616175449));
#190453=CARTESIAN_POINT('Ctrl Pts',(17.9439061442885,17.2469437601221,17.3616433615108));
#190454=CARTESIAN_POINT('Ctrl Pts',(17.9580666703696,17.2413150445504,17.3607358023873));
#190455=CARTESIAN_POINT('Ctrl Pts',(17.9641255312305,17.2389389825277,17.3603472556564));
#190456=CARTESIAN_POINT('Ctrl Pts',(17.97577869884,17.2344309272184,17.3595994741014));
#190457=CARTESIAN_POINT('Ctrl Pts',(17.9813712894228,17.2322946495549,17.3592403877503));
#190458=CARTESIAN_POINT('Ctrl Pts',(17.9960068062144,17.2267751472188,17.3583000898127));
#190459=CARTESIAN_POINT('Ctrl Pts',(18.0050638725999,17.2234300420342,17.3577176096683));
#190460=CARTESIAN_POINT('Ctrl Pts',(18.0363822393942,17.2121058840081,17.3557012625556));
#190461=CARTESIAN_POINT('Ctrl Pts',(18.0587535187793,17.2044381780524,17.3542571197202));
#190462=CARTESIAN_POINT('Ctrl Pts',(18.2381690003453,17.146284060849,17.3426406855067));
#190463=CARTESIAN_POINT('Ctrl Pts',(18.4004692061848,17.1139454284606,17.3318560948795));
#190464=CARTESIAN_POINT('Ctrl Pts',(18.6921302354154,17.0905654657266,17.3125201350039));
#190465=CARTESIAN_POINT('Ctrl Pts',(18.8200952954898,17.0918987612435,17.3040735677056));
#190466=CARTESIAN_POINT('Ctrl Pts',(18.9590371432447,17.1059609150673,17.2954131970075));
#190467=CARTESIAN_POINT('Ctrl Pts',(18.9708939612514,17.1072622475489,17.294678389854));
#190468=CARTESIAN_POINT('Ctrl Pts',(18.9877305204638,17.1092542774094,17.2936416071261));
#190469=CARTESIAN_POINT('Ctrl Pts',(18.9927195257287,17.1098625776392,17.2933352176531));
#190470=CARTESIAN_POINT('Ctrl Pts',(19.0013121031797,17.1109413232773,17.2928090081105));
#190471=CARTESIAN_POINT('Ctrl Pts',(19.0049167015928,17.1114032892573,17.2925887141459));
#190472=CARTESIAN_POINT('Ctrl Pts',(19.0119022544193,17.112316848304,17.2921626898538));
#190473=CARTESIAN_POINT('Ctrl Pts',(19.0152833066568,17.1127673303466,17.2919568956588));
#190474=CARTESIAN_POINT('Ctrl Pts',(19.0244000666724,17.1140044544689,17.2914030419323));
#190475=CARTESIAN_POINT('Ctrl Pts',(19.0301337095775,17.1148064630038,17.2910558438993));
#190476=CARTESIAN_POINT('Ctrl Pts',(19.0513878827432,17.1178683934739,17.2897727522869));
#190477=CARTESIAN_POINT('Ctrl Pts',(19.0668868804549,17.1202773144989,17.2888449040199));
#190478=CARTESIAN_POINT('Ctrl Pts',(19.2153882629564,17.1450513384769,17.280017649029));
#190479=CARTESIAN_POINT('Ctrl Pts',(19.346012391733,17.1799093107208,17.2727250319537));
#190480=CARTESIAN_POINT('Ctrl Pts',(19.618846629008,17.281456511595,17.2569159311043));
#190481=CARTESIAN_POINT('Ctrl Pts',(19.7587481388918,17.3519746174461,17.2484122719691));
#190482=CARTESIAN_POINT('Ctrl Pts',(19.9074393412255,17.4488474200087,17.2380773236331));
#190483=CARTESIAN_POINT('Ctrl Pts',(19.9250879514431,17.460728293646,17.236828896074));
#190484=CARTESIAN_POINT('Ctrl Pts',(19.9499351351986,17.478005029731,17.2350386566563));
#190485=CARTESIAN_POINT('Ctrl Pts',(19.9572833632808,17.4831841448488,17.2345050845135));
#190486=CARTESIAN_POINT('Ctrl Pts',(19.9699058781282,17.492201522096,17.2335812678179));
#190487=CARTESIAN_POINT('Ctrl Pts',(19.9751958619946,17.4960176741622,17.2331918776204));
#190488=CARTESIAN_POINT('Ctrl Pts',(19.9852927117957,17.5033726466368,17.2324443409335));
#190489=CARTESIAN_POINT('Ctrl Pts',(19.9901024196535,17.506907473535,17.2320863518811));
#190490=CARTESIAN_POINT('Ctrl Pts',(20.0025746258844,17.5161552372449,17.2311530586132));
#190491=CARTESIAN_POINT('Ctrl Pts',(20.0102134354006,17.5218997620351,17.2305765225276));
#190492=CARTESIAN_POINT('Ctrl Pts',(20.0361503299252,17.541681166325,17.2286018776703));
#190493=CARTESIAN_POINT('Ctrl Pts',(20.0542573221229,17.5559648379697,17.2271940542857));
#190494=CARTESIAN_POINT('Ctrl Pts',(20.2073793976364,17.6808669288303,17.2150304062749));
#190495=CARTESIAN_POINT('Ctrl Pts',(20.328444417153,17.8074765799318,17.2035794475477));
#190496=CARTESIAN_POINT('Ctrl Pts',(20.4849106737322,18.0178159966541,17.1862579529661));
#190497=CARTESIAN_POINT('Ctrl Pts',(20.5328232904217,18.0913514136052,17.1804778773838));
#190498=CARTESIAN_POINT('Ctrl Pts',(20.5947632614437,18.2007067832672,17.1724526911396));
#190499=CARTESIAN_POINT('Ctrl Pts',(20.6125949374181,18.234263712583,17.1700627034925));
#190500=CARTESIAN_POINT('Ctrl Pts',(20.6328909410748,18.2750728286973,17.1672580005521));
#190501=CARTESIAN_POINT('Ctrl Pts',(20.6362305181192,18.2818791596311,17.166793555187));
#190502=CARTESIAN_POINT('Ctrl Pts',(20.6413564681519,18.2924697544619,17.1660762162998));
#190503=CARTESIAN_POINT('Ctrl Pts',(20.6431682672592,18.2962415419581,17.1658217838991));
#190504=CARTESIAN_POINT('Ctrl Pts',(20.646502347866,18.3032354554579,17.1653519628884));
#190505=CARTESIAN_POINT('Ctrl Pts',(20.6480276637371,18.3064560255739,17.165136391378));
#190506=CARTESIAN_POINT('Ctrl Pts',(20.6514510839316,18.313731708694,17.1646511167101));
#190507=CARTESIAN_POINT('Ctrl Pts',(20.6533444549331,18.3177889890859,17.1643817076547));
#190508=CARTESIAN_POINT('Ctrl Pts',(20.6588758918186,18.3297410353772,17.1635915240095));
#190509=CARTESIAN_POINT('Ctrl Pts',(20.6624782718708,18.3376523473332,17.163072897647));
#190510=CARTESIAN_POINT('Ctrl Pts',(20.6876027188414,18.3937425194552,17.1594254734656));
#190511=CARTESIAN_POINT('Ctrl Pts',(20.7073674778092,18.4426933163723,17.156395851925));
#190512=CARTESIAN_POINT('Ctrl Pts',(20.7307136085991,18.5073810616213,17.1525263830605));
#190513=CARTESIAN_POINT('Ctrl Pts',(20.7359729435373,18.5224876930344,17.151632075838));
#190514=CARTESIAN_POINT('Ctrl Pts',(20.7571582551636,18.5856352070148,17.1479270871854));
#190515=CARTESIAN_POINT('Ctrl Pts',(20.7715305716548,18.6341811708897,17.1451583091965));
#190516=CARTESIAN_POINT('Ctrl Pts',(20.8114262041999,18.7891481114983,17.136445862166));
#190517=CARTESIAN_POINT('Ctrl Pts',(20.8304482396653,18.8970532673305,17.1305550253318));
#190518=CARTESIAN_POINT('Ctrl Pts',(20.8463899414147,19.0608590013463,17.1214043031633));
#190519=CARTESIAN_POINT('Ctrl Pts',(20.8495851896341,19.1159618914489,17.118293126052));
#190520=CARTESIAN_POINT('Ctrl Pts',(20.8512712110308,19.2054561438526,17.1131435958702));
#190521=CARTESIAN_POINT('Ctrl Pts',(20.8510825746819,19.2397974004838,17.1111447413852));
#190522=CARTESIAN_POINT('Ctrl Pts',(20.8497365106307,19.2849251393151,17.1084821016704));
#190523=CARTESIAN_POINT('Ctrl Pts',(20.849331352959,19.2957299785332,17.1078418897695));
#190524=CARTESIAN_POINT('Ctrl Pts',(20.8485321285317,19.3134230094889,17.106788930932));
#190525=CARTESIAN_POINT('Ctrl Pts',(20.8481871241254,19.3203133016414,17.1063777267286));
#190526=CARTESIAN_POINT('Ctrl Pts',(20.8474540518868,19.3336485109807,17.105579632429));
#190527=CARTESIAN_POINT('Ctrl Pts',(20.8470701669998,19.3400935884754,17.1051928780356));
#190528=CARTESIAN_POINT('Ctrl Pts',(20.8461156322335,19.3549722417584,17.1042976330661));
#190529=CARTESIAN_POINT('Ctrl Pts',(20.8455239453633,19.3634043150389,17.1037884869775));
#190530=CARTESIAN_POINT('Ctrl Pts',(20.8437966433915,19.3860746690637,17.1024146878706));
#190531=CARTESIAN_POINT('Ctrl Pts',(20.8425674160037,19.4003051839901,17.1015471101614));
#190532=CARTESIAN_POINT('Ctrl Pts',(20.8276357658058,19.5549022464232,17.0920635745424));
#190533=CARTESIAN_POINT('Ctrl Pts',(20.800086049783,19.6935500670748,17.0829980847195));
#190534=CARTESIAN_POINT('Ctrl Pts',(20.7307977874838,19.9208012566434,17.0673681974679));
#190535=CARTESIAN_POINT('Ctrl Pts',(20.6963367493345,20.011158676072,17.0609429129385));
#190536=CARTESIAN_POINT('Ctrl Pts',(20.6352759178837,20.1433303756454,17.0514418293443));
#190537=CARTESIAN_POINT('Ctrl Pts',(20.6131859944018,20.1870894826534,17.0482795978475));
#190538=CARTESIAN_POINT('Ctrl Pts',(20.5769535408538,20.2530657487165,17.0435263954882));
#190539=CARTESIAN_POINT('Ctrl Pts',(20.5638832171873,20.2758503823164,17.0418877376068));
#190540=CARTESIAN_POINT('Ctrl Pts',(20.5469192652692,20.3041872837718,17.039858978104));
#190541=CARTESIAN_POINT('Ctrl Pts',(20.5434191230558,20.3099709458204,17.0394453929742));
#190542=CARTESIAN_POINT('Ctrl Pts',(20.5378020768602,20.3191530109787,17.0387897005556));
#190543=CARTESIAN_POINT('Ctrl Pts',(20.535703167923,20.3225622895445,17.038546444553));
#190544=CARTESIAN_POINT('Ctrl Pts',(20.5317022680612,20.3290198856707,17.0380861006124));
#190545=CARTESIAN_POINT('Ctrl Pts',(20.5298022124471,20.3320692767492,17.0378688976334));
#190546=CARTESIAN_POINT('Ctrl Pts',(20.525408522584,20.3390808577069,17.0373698646123));
#190547=CARTESIAN_POINT('Ctrl Pts',(20.5229095033285,20.3430396221755,17.037088394243));
#190548=CARTESIAN_POINT('Ctrl Pts',(20.5161719682598,20.3536347098248,17.036335753413));
#190549=CARTESIAN_POINT('Ctrl Pts',(20.5119094776156,20.3602558019482,17.0358661267749));
#190550=CARTESIAN_POINT('Ctrl Pts',(20.4795886579271,20.4098508002853,17.0323525780418));
#190551=CARTESIAN_POINT('Ctrl Pts',(20.4500104122655,20.4518191597275,17.0294028668135));
#190552=CARTESIAN_POINT('Ctrl Pts',(20.4053607853312,20.5105171054204,17.0252482225053));
#190553=CARTESIAN_POINT('Ctrl Pts',(20.3915053631782,20.528143728822,17.0239966578021));
#190554=CARTESIAN_POINT('Ctrl Pts',(20.3484468106026,20.5811663733807,17.0202087884638));
#190555=CARTESIAN_POINT('Ctrl Pts',(20.3183701347066,20.6158366138006,17.0176997317918));
#190556=CARTESIAN_POINT('Ctrl Pts',(20.2128849770733,20.7297317374043,17.0092478498465));
#190557=CARTESIAN_POINT('Ctrl Pts',(20.1324763160936,20.8040819111105,17.003359649536));
#190558=CARTESIAN_POINT('Ctrl Pts',(20.0034491766804,20.9060590566062,16.9942150573862));
#190559=CARTESIAN_POINT('Ctrl Pts',(19.9588952919317,20.9385292460355,16.9911073943248));
#190560=CARTESIAN_POINT('Ctrl Pts',(19.8846331954191,20.9883320871173,16.9859631620631));
#190561=CARTESIAN_POINT('Ctrl Pts',(19.8556797664559,21.0067450830241,16.9839659849589));
#190562=CARTESIAN_POINT('Ctrl Pts',(19.8170337082652,21.0300227657868,16.9813052632023));
#190563=CARTESIAN_POINT('Ctrl Pts',(19.8077321066733,21.0355287589483,16.980665248559));
#190564=CARTESIAN_POINT('Ctrl Pts',(19.7924259741928,21.0444314937842,16.9796125315376));
#190565=CARTESIAN_POINT('Ctrl Pts',(19.7864462110751,21.0478705877955,16.9792013705023));
#190566=CARTESIAN_POINT('Ctrl Pts',(19.7748369701807,21.0544720209546,16.9784033009444));
#190567=CARTESIAN_POINT('Ctrl Pts',(19.7692096168251,21.0576379554037,16.9780165278119));
#190568=CARTESIAN_POINT('Ctrl Pts',(19.7561804678972,21.064889848985,16.9771211534612));
#190569=CARTESIAN_POINT('Ctrl Pts',(19.7487685396473,21.0689572892891,16.9766118961335));
#190570=CARTESIAN_POINT('Ctrl Pts',(19.7287641987546,21.0797796511759,16.9752376022316));
#190571=CARTESIAN_POINT('Ctrl Pts',(19.7161275964603,21.0864515627783,16.9743696376872));
#190572=CARTESIAN_POINT('Ctrl Pts',(19.5995630777364,21.1464945087051,16.9663634624318));
#190573=CARTESIAN_POINT('Ctrl Pts',(19.4914683028102,21.1912960388545,16.9589235698457));
#190574=CARTESIAN_POINT('Ctrl Pts',(19.2253450817259,21.2766062084589,16.9406693399547));
#190575=CARTESIAN_POINT('Ctrl Pts',(19.0652416449195,21.3082429602711,16.9297150924791));
#190576=CARTESIAN_POINT('Ctrl Pts',(18.8706224461329,21.3238380446791,16.9173081087366));
#190577=CARTESIAN_POINT('Ctrl Pts',(18.8380911363972,21.3256904268354,16.9152661940177));
#190578=CARTESIAN_POINT('Ctrl Pts',(18.7982878150827,21.327036048333,16.9128171542623));
#190579=CARTESIAN_POINT('Ctrl Pts',(18.79104624345,21.3272436557768,16.9123735860038));
#190580=CARTESIAN_POINT('Ctrl Pts',(18.7796940488719,21.3275107965473,16.9116815068343));
#190581=CARTESIAN_POINT('Ctrl Pts',(18.7755841549982,21.3275955345131,16.9114316229184));
#190582=CARTESIAN_POINT('Ctrl Pts',(18.7679028238339,21.3277315266311,16.9109658844978));
#190583=CARTESIAN_POINT('Ctrl Pts',(18.7643315428923,21.3277857130647,16.9107498741445));
#190584=CARTESIAN_POINT('Ctrl Pts',(18.7561806632489,21.3278887529587,16.9102580471941));
#190585=CARTESIAN_POINT('Ctrl Pts',(18.7516010414213,21.3279317840853,16.9099825592453));
#190586=CARTESIAN_POINT('Ctrl Pts',(18.737529994505,21.3280183340717,16.9091386203851));
#190587=CARTESIAN_POINT('Ctrl Pts',(18.728038236965,21.3280128843792,16.9085728384662));
#190588=CARTESIAN_POINT('Ctrl Pts',(18.6430857502993,21.3273927443314,16.9035378425769));
#190589=CARTESIAN_POINT('Ctrl Pts',(18.5676994108747,21.3228073609024,16.8992726834526));
#190590=CARTESIAN_POINT('Ctrl Pts',(18.4499369703859,21.3092971492502,16.8927104657092));
#190591=CARTESIAN_POINT('Ctrl Pts',(18.4073210773131,21.3030859934696,16.8903567839326));
#190592=CARTESIAN_POINT('Ctrl Pts',(18.257273188316,21.2765198749099,16.88206062279));
#190593=CARTESIAN_POINT('Ctrl Pts',(18.1512622912255,21.2491503091685,16.8761737784865));
#190594=CARTESIAN_POINT('Ctrl Pts',(17.9957374727907,21.1958655312112,16.8670323388026));
#190595=CARTESIAN_POINT('Ctrl Pts',(17.944351198209,21.1759877509655,16.8639264826521));
#190596=CARTESIAN_POINT('Ctrl Pts',(17.8623236988634,21.1405194965256,16.8587849748045));
#190597=CARTESIAN_POINT('Ctrl Pts',(17.8311832956771,21.1261466950256,16.8567886605093));
#190598=CARTESIAN_POINT('Ctrl Pts',(17.7907072919277,21.1062584691937,16.8541289253531));
#190599=CARTESIAN_POINT('Ctrl Pts',(17.7810444136654,21.1014183246231,16.8534890122342));
#190600=CARTESIAN_POINT('Ctrl Pts',(17.7652756103087,21.0933680928034,16.8524364196687));
#190601=CARTESIAN_POINT('Ctrl Pts',(17.75914749017,21.0902017354009,16.8520252808494));
#190602=CARTESIAN_POINT('Ctrl Pts',(17.7473130818168,21.084013512501,16.8512272240081));
#190603=CARTESIAN_POINT('Ctrl Pts',(17.7416049228073,21.0809953748221,16.8508404412153));
#190604=CARTESIAN_POINT('Ctrl Pts',(17.7284538494114,21.0739646899568,16.8499450002009));
#190605=CARTESIAN_POINT('Ctrl Pts',(17.7210210265246,21.0699335902732,16.8494356855626));
#190606=CARTESIAN_POINT('Ctrl Pts',(17.7010895427968,21.0589689596216,16.8480611367164));
#190607=CARTESIAN_POINT('Ctrl Pts',(17.6886367880156,21.0519532931682,16.8471929728479));
#190608=CARTESIAN_POINT('Ctrl Pts',(17.5748395001307,20.9863149641814,16.8391714645458));
#190609=CARTESIAN_POINT('Ctrl Pts',(17.4784668057012,20.9195153888113,16.8317150962354));
#190610=CARTESIAN_POINT('Ctrl Pts',(17.2619534841887,20.7411909050002,16.8133917575097));
#190611=CARTESIAN_POINT('Ctrl Pts',(17.1482481552742,20.6230185634499,16.8023828327524));
#190612=CARTESIAN_POINT('Ctrl Pts',(17.0301009742324,20.4677494869167,16.7899952032352));
#190613=CARTESIAN_POINT('Ctrl Pts',(17.011497487052,20.4421281432195,16.7880122696032));
#190614=CARTESIAN_POINT('Ctrl Pts',(16.9893870660052,20.4101940089906,16.7856241026111));
#190615=CARTESIAN_POINT('Ctrl Pts',(16.9853295342578,20.4042695279387,16.7851844865034));
#190616=CARTESIAN_POINT('Ctrl Pts',(16.9790045276265,20.3949327154509,16.7844971968478));
#190617=CARTESIAN_POINT('Ctrl Pts',(16.9767167238365,20.3915343157823,16.7842481807965));
#190618=CARTESIAN_POINT('Ctrl Pts',(16.9724515995538,20.3851588500349,16.7837831898338));
#190619=CARTESIAN_POINT('Ctrl Pts',(16.9704719751159,20.3821834518541,16.783567064313));
#190620=CARTESIAN_POINT('Ctrl Pts',(16.9659608172581,20.3753657583851,16.7830738437987));
#190621=CARTESIAN_POINT('Ctrl Pts',(16.9634342741474,20.3715202205749,16.7827970846572));
#190622=CARTESIAN_POINT('Ctrl Pts',(16.956857907152,20.3614391611396,16.7820752443567));
#190623=CARTESIAN_POINT('Ctrl Pts',(16.952828319885,20.3551904261489,16.7816314802075));
#190624=CARTESIAN_POINT('Ctrl Pts',(16.9262800447879,20.3135415232443,16.7786970898218));
#190625=CARTESIAN_POINT('Ctrl Pts',(16.9047834059043,20.2774972702517,16.7762691956215));
#190626=CARTESIAN_POINT('Ctrl Pts',(16.8738106304476,20.2218688113429,16.7726515058379));
#190627=CARTESIAN_POINT('Ctrl Pts',(16.8635425440734,20.202740490925,16.7714299744964));
#190628=CARTESIAN_POINT('Ctrl Pts',(16.8457274024794,20.1682915448323,16.7692639724233));
#190629=CARTESIAN_POINT('Ctrl Pts',(16.8380682053848,20.1530313973742,16.7683161241542));
#190630=CARTESIAN_POINT('Ctrl Pts',(16.7987610646652,20.072294322494,16.7633540324268));
#190631=CARTESIAN_POINT('Ctrl Pts',(16.7703355363631,20.0053475663791,16.7594186474677));
#190632=CARTESIAN_POINT('Ctrl Pts',(16.745419290545,19.9371100205779,16.7554728823802));
#190633=CARTESIAN_POINT('',(16.6170000778107,19.2115739777624,17.2909082101745));
#190634=CARTESIAN_POINT('Ctrl Pts',(16.7454193623258,19.9371102171621,16.5356516081066));
#190635=CARTESIAN_POINT('Ctrl Pts',(16.7457579270419,19.9380374362303,16.5357110078854));
#190636=CARTESIAN_POINT('Ctrl Pts',(16.746097141146,19.9389644209246,16.535770369483));
#190637=CARTESIAN_POINT('Ctrl Pts',(16.7488929535339,19.9465881286455,16.5362583831511));
#190638=CARTESIAN_POINT('Ctrl Pts',(16.7513827741961,19.9532727397506,16.5366850890955));
#190639=CARTESIAN_POINT('Ctrl Pts',(16.7648702367006,19.9889314964981,16.5389555861235));
#190640=CARTESIAN_POINT('Ctrl Pts',(16.7764699454952,20.0176757416178,16.5407654918082));
#190641=CARTESIAN_POINT('Ctrl Pts',(16.8532263803271,20.1964619756451,16.5519560748687));
#190642=CARTESIAN_POINT('Ctrl Pts',(16.9349647288499,20.3387983677051,16.5606012098924));
#190643=CARTESIAN_POINT('Ctrl Pts',(17.1022875670835,20.5649019296998,16.5759957205492));
#190644=CARTESIAN_POINT('Ctrl Pts',(17.1800410112516,20.653477735829,16.5825621375124));
#190645=CARTESIAN_POINT('Ctrl Pts',(17.2750386749147,20.745055200382,16.5902921444315));
#190646=CARTESIAN_POINT('Ctrl Pts',(17.2854344415822,20.7548754204719,16.5911342712664));
#190647=CARTESIAN_POINT('Ctrl Pts',(17.302135585813,20.7703347407435,16.592481656417));
#190648=CARTESIAN_POINT('Ctrl Pts',(17.308376759431,20.7760427812323,16.5929839679614));
#190649=CARTESIAN_POINT('Ctrl Pts',(17.319442938089,20.78604254412,16.5938725911452));
#190650=CARTESIAN_POINT('Ctrl Pts',(17.3242537156305,20.7903499008994,16.5942582357428));
#190651=CARTESIAN_POINT('Ctrl Pts',(17.3342433739037,20.7992121883772,16.5950577050286));
#190652=CARTESIAN_POINT('Ctrl Pts',(17.3394249520335,20.803763950323,16.5954716555505));
#190653=CARTESIAN_POINT('Ctrl Pts',(17.3527797461909,20.8153803540355,16.5965367467642));
#190654=CARTESIAN_POINT('Ctrl Pts',(17.3609848906973,20.8224078356514,16.5971894146369));
#190655=CARTESIAN_POINT('Ctrl Pts',(17.3954326590546,20.8514572865475,16.5999226849536));
#190656=CARTESIAN_POINT('Ctrl Pts',(17.4221529064202,20.8729024107565,16.6020265592615));
#190657=CARTESIAN_POINT('Ctrl Pts',(17.4930983449378,20.9270644688671,16.6075743411489));
#190658=CARTESIAN_POINT('Ctrl Pts',(17.5380969765532,20.9587211793533,16.6110565188951));
#190659=CARTESIAN_POINT('Ctrl Pts',(17.6611866071554,21.0383342983285,16.62047828248));
#190660=CARTESIAN_POINT('Ctrl Pts',(17.7412413697173,21.0830329263447,16.6265050377394));
#190661=CARTESIAN_POINT('Ctrl Pts',(17.8723898801252,21.1454760000262,16.6361026834803));
#190662=CARTESIAN_POINT('Ctrl Pts',(17.9217075117375,21.1666969277956,16.6396525695417));
#190663=CARTESIAN_POINT('Ctrl Pts',(18.0061492647197,21.1992855884015,16.645587353291));
#190664=CARTESIAN_POINT('Ctrl Pts',(18.0408614375712,21.2116512478337,16.6479873919274));
#190665=CARTESIAN_POINT('Ctrl Pts',(18.1208698697374,21.2378204369147,16.6534054472326));
#190666=CARTESIAN_POINT('Ctrl Pts',(18.166344682353,21.2510239785951,16.6564034789483));
#190667=CARTESIAN_POINT('Ctrl Pts',(18.2196941546928,21.2645914524403,16.6597974588999));
#190668=CARTESIAN_POINT('Ctrl Pts',(18.2271712134952,21.2664495715927,16.660270346673));
#190669=CARTESIAN_POINT('Ctrl Pts',(18.2391594373556,21.2693593638258,16.6610239029978));
#190670=CARTESIAN_POINT('Ctrl Pts',(18.2436641187745,21.2704371021254,16.6613060123664));
#190671=CARTESIAN_POINT('Ctrl Pts',(18.251662817074,21.2723230466462,16.6618050379573));
#190672=CARTESIAN_POINT('Ctrl Pts',(18.2551553924461,21.2731371688642,16.6620222910668));
#190673=CARTESIAN_POINT('Ctrl Pts',(18.2625783347428,21.2748475873717,16.6624826519642));
#190674=CARTESIAN_POINT('Ctrl Pts',(18.2665091890719,21.2757415316925,16.6627256241678));
#190675=CARTESIAN_POINT('Ctrl Pts',(18.2771600474854,21.2781317457495,16.6633818261994));
#190676=CARTESIAN_POINT('Ctrl Pts',(18.2838849033741,21.2796064872907,16.6637938384153));
#190677=CARTESIAN_POINT('Ctrl Pts',(18.317749162965,21.2868598630743,16.6658575511443));
#190678=CARTESIAN_POINT('Ctrl Pts',(18.3449945059042,21.2921376271542,16.6674822598694));
#190679=CARTESIAN_POINT('Ctrl Pts',(18.4247168713605,21.305960395674,16.6721534260782));
#190680=CARTESIAN_POINT('Ctrl Pts',(18.4774237807726,21.3130667281444,16.6751379419198));
#190681=CARTESIAN_POINT('Ctrl Pts',(18.6704687303813,21.3317240874825,16.6858684342286));
#190682=CARTESIAN_POINT('Ctrl Pts',(18.811594194508,21.3312566479023,16.6933519748958));
#190683=CARTESIAN_POINT('Ctrl Pts',(19.0430318898356,21.3073376209347,16.7062220314881));
#190684=CARTESIAN_POINT('Ctrl Pts',(19.1337093392212,21.2919520849106,16.7114143684209));
#190685=CARTESIAN_POINT('Ctrl Pts',(19.2364859219334,21.2675471915215,16.7176070959298));
#190686=CARTESIAN_POINT('Ctrl Pts',(19.2498461555622,21.264236757693,16.7184180606212));
#190687=CARTESIAN_POINT('Ctrl Pts',(19.2712107174565,21.2587213083957,16.7197248455258));
#190688=CARTESIAN_POINT('Ctrl Pts',(19.2792361441767,21.256599045731,16.7202179933901));
#190689=CARTESIAN_POINT('Ctrl Pts',(19.2934579135764,21.2527485697684,16.7210960034869));
#190690=CARTESIAN_POINT('Ctrl Pts',(19.2996592840608,21.2510392035841,16.7214802498331));
#190691=CARTESIAN_POINT('Ctrl Pts',(19.3125582924535,21.2474203412335,16.7222824353548));
#190692=CARTESIAN_POINT('Ctrl Pts',(19.3192544820815,21.2455060072057,16.7227005281973));
#190693=CARTESIAN_POINT('Ctrl Pts',(19.3366078332922,21.2404521994704,16.7237883953779));
#190694=CARTESIAN_POINT('Ctrl Pts',(19.3472498419153,21.2372618425813,16.7244598248488));
#190695=CARTESIAN_POINT('Ctrl Pts',(19.3932465779149,21.2230769808748,16.7273808314691));
#190696=CARTESIAN_POINT('Ctrl Pts',(19.4283328473901,21.211240348809,16.7296578649472));
#190697=CARTESIAN_POINT('Ctrl Pts',(19.5206065862157,21.1773907392149,16.7357809755207));
#190698=CARTESIAN_POINT('Ctrl Pts',(19.5771763743947,21.1538059500415,16.7396759623199));
#190699=CARTESIAN_POINT('Ctrl Pts',(19.7735699908022,21.061732250791,16.7536842802609));
#190700=CARTESIAN_POINT('Ctrl Pts',(19.9067696523316,20.9803278550712,16.764129980957));
#190701=CARTESIAN_POINT('Ctrl Pts',(20.0425160994926,20.8752510856814,16.775289953845));
#190702=CARTESIAN_POINT('Ctrl Pts',(20.0550829503678,20.8652931775248,16.7763279658382));
#190703=CARTESIAN_POINT('Ctrl Pts',(20.1049344442333,20.8248607370822,16.7804617133952));
#190704=CARTESIAN_POINT('Ctrl Pts',(20.1412906942533,20.7932583288355,16.7835131409363));
#190705=CARTESIAN_POINT('Ctrl Pts',(20.1822126353908,20.7551597162058,16.7869607241291));
#190706=CARTESIAN_POINT('Ctrl Pts',(20.1878561349835,20.7498474289041,16.7874364685001));
#190707=CARTESIAN_POINT('Ctrl Pts',(20.1968353279329,20.7413017289243,16.7881936921878));
#190708=CARTESIAN_POINT('Ctrl Pts',(20.200189711718,20.7380881796405,16.7884766341143));
#190709=CARTESIAN_POINT('Ctrl Pts',(20.2061162129768,20.7323729749374,16.7889766018864));
#190710=CARTESIAN_POINT('Ctrl Pts',(20.2086925803809,20.7298757906693,16.7891939691256));
#190711=CARTESIAN_POINT('Ctrl Pts',(20.2141446022139,20.7245643841674,16.7896539863386));
#190712=CARTESIAN_POINT('Ctrl Pts',(20.2170185800709,20.7217485165535,16.7898965037252));
#190713=CARTESIAN_POINT('Ctrl Pts',(20.2247636935695,20.7141166060536,16.790550189983));
#190714=CARTESIAN_POINT('Ctrl Pts',(20.229619559553,20.7092850387931,16.7909601571455));
#190715=CARTESIAN_POINT('Ctrl Pts',(20.2537291333173,20.6850621027084,16.7929968607804));
#190716=CARTESIAN_POINT('Ctrl Pts',(20.2726305374248,20.6653218181132,16.7945974445035));
#190717=CARTESIAN_POINT('Ctrl Pts',(20.3263480706006,20.6070002168663,16.7991773014619));
#190718=CARTESIAN_POINT('Ctrl Pts',(20.3601341123824,20.5674945862847,16.8020974820705));
#190719=CARTESIAN_POINT('Ctrl Pts',(20.478758729307,20.417978218912,16.8126674599353));
#190720=CARTESIAN_POINT('Ctrl Pts',(20.5541676236854,20.3009411253167,16.8200533415536));
#190721=CARTESIAN_POINT('Ctrl Pts',(20.6610705710436,20.092571824974,16.8329863507533));
#190722=CARTESIAN_POINT('Ctrl Pts',(20.6987904790488,20.0049552655127,16.8383624153762));
#190723=CARTESIAN_POINT('Ctrl Pts',(20.735086711388,19.9020375608247,16.844759331942));
#190724=CARTESIAN_POINT('Ctrl Pts',(20.7395660722882,19.8889274688676,16.8455755240188));
#190725=CARTESIAN_POINT('Ctrl Pts',(20.7465313976245,19.8678681178285,16.8468891268809));
#190726=CARTESIAN_POINT('Ctrl Pts',(20.7490997357537,19.8599463788213,16.8473838201566));
#190727=CARTESIAN_POINT('Ctrl Pts',(20.753570210642,19.8458752594715,16.8482636107686));
#190728=CARTESIAN_POINT('Ctrl Pts',(20.7554911773017,19.8397319376968,16.8486480836222));
#190729=CARTESIAN_POINT('Ctrl Pts',(20.759428708455,19.8269349673162,16.8494497650739));
#190730=CARTESIAN_POINT('Ctrl Pts',(20.761440569367,19.8202799626503,16.8498671224901));
#190731=CARTESIAN_POINT('Ctrl Pts',(20.7665666279569,19.8030170007673,16.8509509528514));
#190732=CARTESIAN_POINT('Ctrl Pts',(20.7696305459446,19.792394443933,16.8516190579823));
#190733=CARTESIAN_POINT('Ctrl Pts',(20.7824568424691,19.7465812201874,16.8545058825182));
#190734=CARTESIAN_POINT('Ctrl Pts',(20.7913904592462,19.7111668886165,16.8567512686278));
#190735=CARTESIAN_POINT('Ctrl Pts',(20.8125908938157,19.6169072666622,16.8627677048293));
#190736=CARTESIAN_POINT('Ctrl Pts',(20.8232747011317,19.5577434073214,16.8665855784685));
#190737=CARTESIAN_POINT('Ctrl Pts',(20.8540465067234,19.3330236263938,16.8812213746667));
#190738=CARTESIAN_POINT('Ctrl Pts',(20.8570717085548,19.1657621641039,16.8924428367485));
#190739=CARTESIAN_POINT('Ctrl Pts',(20.8350135869871,18.9456702212581,16.9067490150706));
#190740=CARTESIAN_POINT('Ctrl Pts',(20.8274881582066,18.8916781997032,16.9102151942044));
#190741=CARTESIAN_POINT('Ctrl Pts',(20.8163427134714,18.8294051445217,16.9141180341984));
#190742=CARTESIAN_POINT('Ctrl Pts',(20.8147450813297,18.8207875928471,16.9146559826978));
#190743=CARTESIAN_POINT('Ctrl Pts',(20.8122475798632,18.8077678327293,16.9154652414464));
#190744=CARTESIAN_POINT('Ctrl Pts',(20.8113871603971,18.8033582815667,16.915738714241));
#190745=CARTESIAN_POINT('Ctrl Pts',(20.8098189048571,18.7954550803654,16.9162277245389));
#190746=CARTESIAN_POINT('Ctrl Pts',(20.8091162795078,18.7919604635481,16.9164435534477));
#190747=CARTESIAN_POINT('Ctrl Pts',(20.8075720175998,18.784378976305,16.9169109149297));
#190748=CARTESIAN_POINT('Ctrl Pts',(20.8067271268241,18.7802928274928,16.917162259105));
#190749=CARTESIAN_POINT('Ctrl Pts',(20.8043242462623,18.7688425942054,16.9178651108676));
#190750=CARTESIAN_POINT('Ctrl Pts',(20.8027390369547,18.7614841971655,16.91831508965));
#190751=CARTESIAN_POINT('Ctrl Pts',(20.7931189259515,18.7179574644438,16.9209675675613));
#190752=CARTESIAN_POINT('Ctrl Pts',(20.7841743813364,18.6819942569394,16.9231212376629));
#190753=CARTESIAN_POINT('Ctrl Pts',(20.7518830240575,18.5653276602424,16.9300381770224));
#190754=CARTESIAN_POINT('Ctrl Pts',(20.7246760644106,18.485771968048,16.9346463484564));
#190755=CARTESIAN_POINT('Ctrl Pts',(20.624603497871,18.2416466683001,16.9490128152082));
#190756=CARTESIAN_POINT('Ctrl Pts',(20.5354830636128,18.0846431388546,16.9586593033433));
#190757=CARTESIAN_POINT('Ctrl Pts',(20.4140080002074,17.9226774527702,16.9704278643016));
#190758=CARTESIAN_POINT('Ctrl Pts',(20.4001305797781,17.9047799958198,16.9717549303042));
#190759=CARTESIAN_POINT('Ctrl Pts',(20.380034776555,17.879704178865,16.9736541721479));
#190760=CARTESIAN_POINT('Ctrl Pts',(20.3740508124741,17.8723393346163,16.9742169841273));
#190761=CARTESIAN_POINT('Ctrl Pts',(20.3642304058494,17.8604174201315,16.9751363389146));
#190762=CARTESIAN_POINT('Ctrl Pts',(20.3604238461326,17.8558358207159,16.975491667119));
#190763=CARTESIAN_POINT('Ctrl Pts',(20.3524014206963,17.8462624676364,16.9762384161879));
#190764=CARTESIAN_POINT('Ctrl Pts',(20.3481816859415,17.8412740514836,16.9766299933147));
#190765=CARTESIAN_POINT('Ctrl Pts',(20.3380621118027,17.8294227679942,16.9775662377315));
#190766=CARTESIAN_POINT('Ctrl Pts',(20.3321412602634,17.822578084736,16.9781117698801));
#190767=CARTESIAN_POINT('Ctrl Pts',(20.3119201134858,17.7995025498768,16.9799674600976));
#190768=CARTESIAN_POINT('Ctrl Pts',(20.2974153672065,17.7834534083499,16.9812861371627));
#190769=CARTESIAN_POINT('Ctrl Pts',(20.2162434483324,17.6963597958894,16.98860094668));
#190770=CARTESIAN_POINT('Ctrl Pts',(20.1449878787224,17.6297696927172,16.994795233597));
#190771=CARTESIAN_POINT('Ctrl Pts',(19.9646963641727,17.4832017145389,17.0099096971113));
#190772=CARTESIAN_POINT('Ctrl Pts',(19.8520898680962,17.4082873325656,17.0189377606499));
#190773=CARTESIAN_POINT('Ctrl Pts',(19.673575503724,17.3127247438807,17.0321304690865));
#190774=CARTESIAN_POINT('Ctrl Pts',(19.6125298070876,17.2837121742191,17.0364595397366));
#190775=CARTESIAN_POINT('Ctrl Pts',(19.5416245342323,17.2540845962664,17.0412040168048));
#190776=CARTESIAN_POINT('Ctrl Pts',(19.533030003088,17.2505596548048,17.0417744639915));
#190777=CARTESIAN_POINT('Ctrl Pts',(19.5202008942851,17.2453963361491,17.0426187874855));
#190778=CARTESIAN_POINT('Ctrl Pts',(19.5159839312644,17.2437148804379,17.0428951690419));
#190779=CARTESIAN_POINT('Ctrl Pts',(19.5084429393208,17.2407360924661,17.0433873153194));
#190780=CARTESIAN_POINT('Ctrl Pts',(19.5051210184411,17.2394335904819,17.0436033876423));
#190781=CARTESIAN_POINT('Ctrl Pts',(19.4979393851144,17.2366386501435,17.0440689404596));
#190782=CARTESIAN_POINT('Ctrl Pts',(19.494078597153,17.2351491324597,17.0443182450771));
#190783=CARTESIAN_POINT('Ctrl Pts',(19.4833303712375,17.231038560833,17.0450096590298));
#190784=CARTESIAN_POINT('Ctrl Pts',(19.4764335009835,17.228442105236,17.0454503187627));
#190785=CARTESIAN_POINT('Ctrl Pts',(19.4372004693585,17.2139055405397,17.0479407600401));
#190786=CARTESIAN_POINT('Ctrl Pts',(19.4045880380314,17.202719847369,17.0499484041586));
#190787=CARTESIAN_POINT('Ctrl Pts',(19.3006675955519,17.1698904206573,17.0561926336432));
#190788=CARTESIAN_POINT('Ctrl Pts',(19.2284791510635,17.1512105553931,17.0603066919223));
#190789=CARTESIAN_POINT('Ctrl Pts',(18.964904718397,17.0976665462423,17.0749992300359));
#190790=CARTESIAN_POINT('Ctrl Pts',(18.7699560274011,17.0853948146125,17.0853523920085));
#190791=CARTESIAN_POINT('Ctrl Pts',(18.5550373548284,17.10147248897,17.0979001947344));
#190792=CARTESIAN_POINT('Ctrl Pts',(18.5340276179722,17.1033603374155,17.0991376021045));
#190793=CARTESIAN_POINT('Ctrl Pts',(18.5048014842644,17.1064273996779,17.1008752684889));
#190794=CARTESIAN_POINT('Ctrl Pts',(18.496558077905,17.1073414915208,17.1013672014366));
#190795=CARTESIAN_POINT('Ctrl Pts',(18.4823262254644,17.1090043455886,17.1022197185278));
#190796=CARTESIAN_POINT('Ctrl Pts',(18.4763351774992,17.1097303223911,17.1025795813548));
#190797=CARTESIAN_POINT('Ctrl Pts',(18.4639237946304,17.1112881732013,17.1033271738693));
#190798=CARTESIAN_POINT('Ctrl Pts',(18.4575040148025,17.1121239005052,17.103715021666));
#190799=CARTESIAN_POINT('Ctrl Pts',(18.4424577301492,17.114152856131,17.1046267920114));
#190800=CARTESIAN_POINT('Ctrl Pts',(18.4338346022621,17.1153698870456,17.1051514623112));
#190801=CARTESIAN_POINT('Ctrl Pts',(18.4057712341489,17.1195073925186,17.1068660343564));
#190802=CARTESIAN_POINT('Ctrl Pts',(18.3863645598273,17.1226453821957,17.1080627934563));
#190803=CARTESIAN_POINT('Ctrl Pts',(18.2867785682032,17.1401746396328,17.1142628546294));
#190804=CARTESIAN_POINT('Ctrl Pts',(18.207443565215,17.1589131869396,17.1194029667741));
#190805=CARTESIAN_POINT('Ctrl Pts',(17.9776814634974,17.227384209843,17.1348669479345));
#190806=CARTESIAN_POINT('Ctrl Pts',(17.8315362136191,17.2894636750079,17.1454942249207));
#190807=CARTESIAN_POINT('Ctrl Pts',(17.6386458723129,17.3982998841389,17.1598922888129));
#190808=CARTESIAN_POINT('Ctrl Pts',(17.5850214087633,17.4318057485674,17.1639327519656));
#190809=CARTESIAN_POINT('Ctrl Pts',(17.5254014008468,17.4728794815531,17.1684018676483));
#190810=CARTESIAN_POINT('Ctrl Pts',(17.5178649502775,17.4781442476707,17.1689663448772));
#190811=CARTESIAN_POINT('Ctrl Pts',(17.5066738915779,17.4860709986418,17.169803577061));
#190812=CARTESIAN_POINT('Ctrl Pts',(17.5029932433529,17.4886957870032,17.1700787773126));
#190813=CARTESIAN_POINT('Ctrl Pts',(17.496506876361,17.4933528387723,17.1705634374976));
#190814=CARTESIAN_POINT('Ctrl Pts',(17.4936977193714,17.4953802126407,17.1707732277142));
#190815=CARTESIAN_POINT('Ctrl Pts',(17.4908825941583,17.4974224221021,17.1709833504218));
#190816=CARTESIAN_POINT('Ctrl Pts',(17.4908716997384,17.4974303255281,17.1709841635864));
#190817=CARTESIAN_POINT('Ctrl Pts',(17.4908500946672,17.4974459993784,17.1709857761959));
#190818=CARTESIAN_POINT('Ctrl Pts',(17.4908393836709,17.4974537700478,17.1709865756665));
#190819=CARTESIAN_POINT('Ctrl Pts',(17.4908181408182,17.4974691817272,17.1709881612336));
#190820=CARTESIAN_POINT('Ctrl Pts',(17.4908076091093,17.4974768226251,17.1709889473191));
#190821=CARTESIAN_POINT('Ctrl Pts',(17.490786721538,17.4974919771359,17.1709905063618));
#190822=CARTESIAN_POINT('Ctrl Pts',(17.4907763655008,17.4974994908707,17.1709912793322));
#190823=CARTESIAN_POINT('Ctrl Pts',(17.4907563393645,17.4975140209408,17.1709927740718));
#190824=CARTESIAN_POINT('Ctrl Pts',(17.4907466691971,17.4975210373074,17.1709934958465));
#190825=CARTESIAN_POINT('Ctrl Pts',(17.4907273644813,17.4975350444458,17.1709949367345));
#190826=CARTESIAN_POINT('Ctrl Pts',(17.4907177303752,17.497542034896,17.170995655815));
#190827=CARTESIAN_POINT('Ctrl Pts',(17.490698498942,17.4975559893572,17.1709970912282));
#190828=CARTESIAN_POINT('Ctrl Pts',(17.4906889011106,17.4975629537333,17.1709978075986));
#190829=CARTESIAN_POINT('Ctrl Pts',(17.4906697409776,17.4975768569501,17.1709992376849));
#190830=CARTESIAN_POINT('Ctrl Pts',(17.490660178835,17.4975837956746,17.170999951389));
#190831=CARTESIAN_POINT('Ctrl Pts',(17.487358510376,17.4999796782725,17.1712463825647));
#190832=CARTESIAN_POINT('Ctrl Pts',(17.4840732641445,17.5023781282419,17.171491437748));
#190833=CARTESIAN_POINT('Ctrl Pts',(17.477282283717,17.5073660672984,17.171997729333));
#190834=CARTESIAN_POINT('Ctrl Pts',(17.4737775886552,17.5099569465248,17.1722588692457));
#190835=CARTESIAN_POINT('Ctrl Pts',(17.4648864425515,17.5165723715022,17.1729210555884));
#190836=CARTESIAN_POINT('Ctrl Pts',(17.4595110734997,17.5206118230398,17.1733211102986));
#190837=CARTESIAN_POINT('Ctrl Pts',(17.4440634507962,17.5323358888336,17.1744702402052));
#190838=CARTESIAN_POINT('Ctrl Pts',(17.4340406358823,17.5400855296944,17.1752151597165));
#190839=CARTESIAN_POINT('Ctrl Pts',(17.399889519129,17.5669844747819,17.1777533680757));
#190840=CARTESIAN_POINT('Ctrl Pts',(17.3761089298929,17.586570914311,17.1795208528137));
#190841=CARTESIAN_POINT('Ctrl Pts',(17.2575602376774,17.6886346155539,17.1883808123201));
#190842=CARTESIAN_POINT('Ctrl Pts',(17.1698348093949,17.7789165765252,17.19511241989));
#190843=CARTESIAN_POINT('Ctrl Pts',(17.0690602118355,17.9030110439496,17.2038141847654));
#190844=CARTESIAN_POINT('Ctrl Pts',(17.0481391182054,17.9300891420151,17.2056822771101));
#190845=CARTESIAN_POINT('Ctrl Pts',(16.9656574075929,18.0423680161385,17.2133427635454));
#190846=CARTESIAN_POINT('Ctrl Pts',(16.9098332437536,18.1315799084601,17.2192442854583));
#190847=CARTESIAN_POINT('Ctrl Pts',(16.8543055473955,18.2370204989898,17.2262274650637));
#190848=CARTESIAN_POINT('Ctrl Pts',(16.8478684790826,18.2495452818439,17.2270568985404));
#190849=CARTESIAN_POINT('Ctrl Pts',(16.8377945246964,18.269637020233,17.2283877586346));
#190850=CARTESIAN_POINT('Ctrl Pts',(16.8340767980751,18.2771631363358,17.2288863517731));
#190851=CARTESIAN_POINT('Ctrl Pts',(16.8275830681521,18.2905082582108,17.2297706527729));
#190852=CARTESIAN_POINT('Ctrl Pts',(16.8247886863266,18.2963182394621,17.2301557144048));
#190853=CARTESIAN_POINT('Ctrl Pts',(16.8190486272531,18.3083936780619,17.23095620865));
#190854=CARTESIAN_POINT('Ctrl Pts',(16.816107062717,18.3146609950827,17.231371778131));
#190855=CARTESIAN_POINT('Ctrl Pts',(16.8086037967711,18.3308535466727,17.2324457831657));
#190856=CARTESIAN_POINT('Ctrl Pts',(16.804088118517,18.3407997693523,17.2331057955402));
#190857=CARTESIAN_POINT('Ctrl Pts',(16.7852989170205,18.3830504873978,17.2359110825272));
#190858=CARTESIAN_POINT('Ctrl Pts',(16.7717586557371,18.4156730375422,17.2380811902301));
#190859=CARTESIAN_POINT('Ctrl Pts',(16.7383836134081,18.5021313866184,17.2438466495949));
#190860=CARTESIAN_POINT('Ctrl Pts',(16.7199110919727,18.5564586143804,17.2474841213431));
#190861=CARTESIAN_POINT('Ctrl Pts',(16.6461257273694,18.8063336336557,17.2642610289432));
#190862=CARTESIAN_POINT('Ctrl Pts',(16.616945001367,19.0084357473791,17.2780828555683));
#190863=CARTESIAN_POINT('Ctrl Pts',(16.6170000778107,19.2115739777624,17.2909082101745));
#190864=CARTESIAN_POINT('Ctrl Pts',(16.617000078448,19.2115763236151,17.2909083582825));
#190865=CARTESIAN_POINT('Ctrl Pts',(16.6170043638434,19.2273177950194,17.2919022126078));
#190866=CARTESIAN_POINT('Ctrl Pts',(16.6171842237099,19.2430592943021,17.2928889421261));
#190867=CARTESIAN_POINT('Ctrl Pts',(16.6177851449818,19.2696677192771,17.2945431885913));
#190868=CARTESIAN_POINT('Ctrl Pts',(16.6181143695731,19.2805357749806,17.2952150009985));
#190869=CARTESIAN_POINT('Ctrl Pts',(16.6187085001659,19.2961682425581,17.2961753174121));
#190870=CARTESIAN_POINT('Ctrl Pts',(16.6189057980453,19.3009348467959,17.2964673297887));
#190871=CARTESIAN_POINT('Ctrl Pts',(16.619279118516,19.3092719287477,17.2969766219361));
#190872=CARTESIAN_POINT('Ctrl Pts',(16.6194480741323,19.312842681655,17.2971942834138));
#190873=CARTESIAN_POINT('Ctrl Pts',(16.6197955281192,19.3198119123319,17.297618170331));
#190874=CARTESIAN_POINT('Ctrl Pts',(16.6199731786469,19.323210429224,17.297824442496));
#190875=CARTESIAN_POINT('Ctrl Pts',(16.6203449444749,19.3300079695181,17.298236131484));
#190876=CARTESIAN_POINT('Ctrl Pts',(16.6205390638766,19.3334069541103,17.2984415483144));
#190877=CARTESIAN_POINT('Ctrl Pts',(16.6210263182197,19.3415917677725,17.2989351657796));
#190878=CARTESIAN_POINT('Ctrl Pts',(16.6213275158841,19.3463771235785,17.2992229173022));
#190879=CARTESIAN_POINT('Ctrl Pts',(16.6224923796179,19.3639326315363,17.3002755809276));
#190880=CARTESIAN_POINT('Ctrl Pts',(16.6234556133261,19.3766961998604,17.3010351247462));
#190881=CARTESIAN_POINT('Ctrl Pts',(16.6267051711631,19.415109240068,17.3033056984767));
#190882=CARTESIAN_POINT('Ctrl Pts',(16.629343841443,19.4407273490183,17.3047993510392));
#190883=CARTESIAN_POINT('Ctrl Pts',(16.6408529428832,19.5354696449089,17.3102675854388));
#190884=CARTESIAN_POINT('Ctrl Pts',(16.6526677492806,19.6041954381617,17.314124798583));
#190885=CARTESIAN_POINT('Ctrl Pts',(16.6879369732018,19.7621933541582,17.3229825713365));
#190886=CARTESIAN_POINT('Ctrl Pts',(16.7138584209825,19.8506750620402,17.3279387938027));
#190887=CARTESIAN_POINT('Ctrl Pts',(16.7454194652257,19.9371104989717,17.3329785907215));
#190888=CARTESIAN_POINT('Origin',(18.734,19.211,0.));
#190889=CARTESIAN_POINT('',(16.7454193519082,19.9371101886317,18.3568545479166));
#190890=CARTESIAN_POINT('',(16.7454193782244,19.9371102607032,18.1318062886951));
#190891=CARTESIAN_POINT('',(16.7454193623258,19.9371102171621,0.));
#190892=CARTESIAN_POINT('Ctrl Pts',(16.7454193519082,19.9371101886317,18.3568545479166));
#190893=CARTESIAN_POINT('Ctrl Pts',(16.740076494339,19.9224778320914,18.3558520679459));
#190894=CARTESIAN_POINT('Ctrl Pts',(16.7348945232057,19.9077848210586,18.3548454931849));
#190895=CARTESIAN_POINT('Ctrl Pts',(16.6860061867035,19.7641286466884,18.3450068997072));
#190896=CARTESIAN_POINT('Ctrl Pts',(16.6546780663117,19.6312935582155,18.3359031838316));
#190897=CARTESIAN_POINT('Ctrl Pts',(16.6262469231319,19.4223145563828,18.322121638853));
#190898=CARTESIAN_POINT('Ctrl Pts',(16.6200989586563,19.3477543266621,18.3173148259657));
#190899=CARTESIAN_POINT('Ctrl Pts',(16.617649086585,19.2641628394303,18.3121557615785));
#190900=CARTESIAN_POINT('Ctrl Pts',(16.6174451484744,19.2553062410246,18.3116120546279));
#190901=CARTESIAN_POINT('Ctrl Pts',(16.6172222392365,19.2419958500716,18.3107995510631));
#190902=CARTESIAN_POINT('Ctrl Pts',(16.6171617203538,19.2375429811444,18.3105285125938));
#190903=CARTESIAN_POINT('Ctrl Pts',(16.6170816556437,19.2298703476926,18.3100628702711));
#190904=CARTESIAN_POINT('Ctrl Pts',(16.61705540401,19.226650708558,18.309867894064));
#190905=CARTESIAN_POINT('Ctrl Pts',(16.6170125976616,19.2193608843705,18.3094273900038));
#190906=CARTESIAN_POINT('Ctrl Pts',(16.6170004354123,19.2152907137506,18.3091821108928));
#190907=CARTESIAN_POINT('Ctrl Pts',(16.6169992761201,19.2041601536932,18.3085131255452));
#190908=CARTESIAN_POINT('Ctrl Pts',(16.6170338608298,19.197099740555,18.308090719101));
#190909=CARTESIAN_POINT('Ctrl Pts',(16.6174008058345,19.160040260732,18.3058831615146));
#190910=CARTESIAN_POINT('Ctrl Pts',(16.6183355228245,19.1300489516173,18.3041297092626));
#190911=CARTESIAN_POINT('Ctrl Pts',(16.6230423579442,19.0403336687759,18.298956773104));
#190912=CARTESIAN_POINT('Ctrl Pts',(16.6287092855466,18.9807366743784,18.2956161886736));
#190913=CARTESIAN_POINT('Ctrl Pts',(16.6597465945341,18.7559400282549,18.2831216772672));
#190914=CARTESIAN_POINT('Ctrl Pts',(16.7021118177646,18.593717083346,18.2742743143245));
#190915=CARTESIAN_POINT('Ctrl Pts',(16.7847366131576,18.3830080322236,18.2615097650854));
#190916=CARTESIAN_POINT('Ctrl Pts',(16.8086669963622,18.3287923457201,18.2581084204706));
#190917=CARTESIAN_POINT('Ctrl Pts',(16.8402461663869,18.2646727461113,18.2539094734308));
#190918=CARTESIAN_POINT('Ctrl Pts',(16.845749831968,18.2537382033796,18.2531870918306));
#190919=CARTESIAN_POINT('Ctrl Pts',(16.8549745051634,18.2357999819467,18.2519912824719));
#190920=CARTESIAN_POINT('Ctrl Pts',(16.8586406319954,18.2287682943024,18.2515197857228));
#190921=CARTESIAN_POINT('Ctrl Pts',(16.8653239031246,18.2161234984386,18.2506668736345));
#190922=CARTESIAN_POINT('Ctrl Pts',(16.868327061841,18.2105030760462,18.250285957569));
#190923=CARTESIAN_POINT('Ctrl Pts',(16.8748002290214,18.1985190135426,18.2494698382465));
#190924=CARTESIAN_POINT('Ctrl Pts',(16.8782776275804,18.1921594772435,18.2490343747704));
#190925=CARTESIAN_POINT('Ctrl Pts',(16.8877882533566,18.1749764805655,18.2478512605664));
#190926=CARTESIAN_POINT('Ctrl Pts',(16.8938838922957,18.1641880559534,18.2471013779622));
#190927=CARTESIAN_POINT('Ctrl Pts',(16.9256762180647,18.1090559138824,18.2432322935626));
#190928=CARTESIAN_POINT('Ctrl Pts',(16.9528805237454,18.065605584064,18.2400586925772));
#190929=CARTESIAN_POINT('Ctrl Pts',(17.0774365498924,17.8818493423726,18.226076661577));
#190930=CARTESIAN_POINT('Ctrl Pts',(17.1899788020233,17.7526358939629,18.2147047222254));
#190931=CARTESIAN_POINT('Ctrl Pts',(17.3851544770935,17.5767493254368,18.197426436311));
#190932=CARTESIAN_POINT('Ctrl Pts',(17.4574777109291,17.5196530990333,18.1914503969016));
#190933=CARTESIAN_POINT('Ctrl Pts',(17.5412586688597,17.4619572346241,18.1851656251151));
#190934=CARTESIAN_POINT('Ctrl Pts',(17.5492592078464,17.4565280732736,18.1845715864903));
#190935=CARTESIAN_POINT('Ctrl Pts',(17.56113269998,17.4485889841799,18.1836993116582));
#190936=CARTESIAN_POINT('Ctrl Pts',(17.5649769841914,17.4460366911517,18.1834183268371));
#190937=CARTESIAN_POINT('Ctrl Pts',(17.5718145274698,17.4415292573937,18.1829211401122));
#190938=CARTESIAN_POINT('Ctrl Pts',(17.5748044214367,17.4395691114763,18.1827046050697));
#190939=CARTESIAN_POINT('Ctrl Pts',(17.5812240312247,17.4353836901448,18.1822415595434));
#190940=CARTESIAN_POINT('Ctrl Pts',(17.5846552220479,17.4331607789077,18.1819952064571));
#190941=CARTESIAN_POINT('Ctrl Pts',(17.594098515162,17.4270816667536,18.1813202541874));
#190942=CARTESIAN_POINT('Ctrl Pts',(17.6001237909021,17.4232458892285,18.1808929939474));
#190943=CARTESIAN_POINT('Ctrl Pts',(17.6325054999265,17.4028607917225,18.1786142275692));
#190944=CARTESIAN_POINT('Ctrl Pts',(17.6592065247687,17.3868627389999,18.1767968998646));
#190945=CARTESIAN_POINT('Ctrl Pts',(17.8286695720217,17.2903416613725,18.1655816897482));
#190946=CARTESIAN_POINT('Ctrl Pts',(17.9800402574271,17.2260292886871,18.1569209865215));
#190947=CARTESIAN_POINT('Ctrl Pts',(18.2497879317054,17.1467893202156,18.1415316130463));
#190948=CARTESIAN_POINT('Ctrl Pts',(18.364779749836,17.1231546591343,18.1349895556366));
#190949=CARTESIAN_POINT('Ctrl Pts',(18.4953200969613,17.1074493715658,18.1272869662159));
#190950=CARTESIAN_POINT('Ctrl Pts',(18.5095292559827,17.1058857008095,18.1264451712769));
#190951=CARTESIAN_POINT('Ctrl Pts',(18.5321672416965,17.1036262685549,18.1250982179376));
#190952=CARTESIAN_POINT('Ctrl Pts',(18.5405864376635,17.1028368903122,18.1245960033195));
#190953=CARTESIAN_POINT('Ctrl Pts',(18.5554424107499,17.1015337449926,18.123707492998));
#190954=CARTESIAN_POINT('Ctrl Pts',(18.5618772684991,17.1009989437043,18.1233218637923));
#190955=CARTESIAN_POINT('Ctrl Pts',(18.5751908612632,17.0999537583577,18.1225223688771));
#190956=CARTESIAN_POINT('Ctrl Pts',(18.5820698377484,17.0994475377237,18.1221083770503));
#190957=CARTESIAN_POINT('Ctrl Pts',(18.5997320092373,17.0982345414584,18.1210430584122));
#190958=CARTESIAN_POINT('Ctrl Pts',(18.6105182665399,17.0975767033387,18.1203902031609));
#190959=CARTESIAN_POINT('Ctrl Pts',(18.6555453165899,17.0951764432361,18.1176551189331));
#190960=CARTESIAN_POINT('Ctrl Pts',(18.6898192893575,17.0941834492349,18.1155495794422));
#190961=CARTESIAN_POINT('Ctrl Pts',(18.7791606206309,17.0937656782698,18.1099963604658));
#190962=CARTESIAN_POINT('Ctrl Pts',(18.8342054556308,17.0956563630508,18.1065103172253));
#190963=CARTESIAN_POINT('Ctrl Pts',(18.998174968728,17.1077026260574,18.0959427836498));
#190964=CARTESIAN_POINT('Ctrl Pts',(19.1064471912572,17.1241536040697,18.0887128958368));
#190965=CARTESIAN_POINT('Ctrl Pts',(19.2565114809359,17.1590082109158,18.0785361081056));
#190966=CARTESIAN_POINT('Ctrl Pts',(19.2997378818415,17.17050266466,18.0755875793002));
#190967=CARTESIAN_POINT('Ctrl Pts',(19.3667238994199,17.190607586601,18.0710173663246));
#190968=CARTESIAN_POINT('Ctrl Pts',(19.3907483694794,17.1982887223917,18.0693781228253));
#190969=CARTESIAN_POINT('Ctrl Pts',(19.4618604547071,17.222433685406,18.0645357795359));
#190970=CARTESIAN_POINT('Ctrl Pts',(19.5085132254562,17.2401354792261,18.0613717201597));
#190971=CARTESIAN_POINT('Ctrl Pts',(19.5617049774984,17.2624994109848,18.0578132630285));
#190972=CARTESIAN_POINT('Ctrl Pts',(19.5688924915254,17.2655682723176,18.0573334910496));
#190973=CARTESIAN_POINT('Ctrl Pts',(19.5803423212537,17.2705321620781,18.0565710998989));
#190974=CARTESIAN_POINT('Ctrl Pts',(19.5846155746587,17.2724015630198,18.0562869871464));
#190975=CARTESIAN_POINT('Ctrl Pts',(19.5921673990151,17.2757350034144,18.0557856904529));
#190976=CARTESIAN_POINT('Ctrl Pts',(19.5954484665941,17.2771932795947,18.055568158783));
#190977=CARTESIAN_POINT('Ctrl Pts',(19.6023887666971,17.2802990771642,18.0551086066885));
#190978=CARTESIAN_POINT('Ctrl Pts',(19.6060470222461,17.281948654086,18.0548667147028));
#190979=CARTESIAN_POINT('Ctrl Pts',(19.6158937415444,17.2864224616233,18.054216485923));
#190980=CARTESIAN_POINT('Ctrl Pts',(19.6220733808811,17.289266161603,18.0538093291238));
#190981=CARTESIAN_POINT('Ctrl Pts',(19.6524929943149,17.3034425000545,18.0518090906745));
#190982=CARTESIAN_POINT('Ctrl Pts',(19.6765314979828,17.3152047783861,18.0502410513488));
#190983=CARTESIAN_POINT('Ctrl Pts',(19.7451552828336,17.3504111613286,18.0457830748306));
#190984=CARTESIAN_POINT('Ctrl Pts',(19.7891371305345,17.3749956032445,18.0429485404463));
#190985=CARTESIAN_POINT('Ctrl Pts',(19.9451388821755,17.4696550482877,18.0328294029101));
#190986=CARTESIAN_POINT('Ctrl Pts',(20.0514153025267,17.548604440817,18.0257921617174));
#190987=CARTESIAN_POINT('Ctrl Pts',(20.2269410679448,17.7064655857836,18.0128055916103));
#190988=CARTESIAN_POINT('Ctrl Pts',(20.2990038251029,17.7815750039524,18.0069651109322));
#190989=CARTESIAN_POINT('Ctrl Pts',(20.3742143762197,17.8724995571169,18.000050190486));
#190990=CARTESIAN_POINT('Ctrl Pts',(20.3830665550343,17.8834209558686,17.9992221360428));
#190991=CARTESIAN_POINT('Ctrl Pts',(20.3970252909831,17.9009976222521,17.9978930722773));
#190992=CARTESIAN_POINT('Ctrl Pts',(20.4022022975667,17.9075965937368,17.9973948842505));
#190993=CARTESIAN_POINT('Ctrl Pts',(20.411288395844,17.919321174687,17.9965110528354));
#190994=CARTESIAN_POINT('Ctrl Pts',(20.4152135692636,17.9244342287701,17.9961260534136));
#190995=CARTESIAN_POINT('Ctrl Pts',(20.4233078228384,17.9350783515179,17.995325441143));
#190996=CARTESIAN_POINT('Ctrl Pts',(20.4274732275811,17.9406121068507,17.9949096902034));
#190997=CARTESIAN_POINT('Ctrl Pts',(20.438145688577,17.9549362736984,17.9938346874009));
#190998=CARTESIAN_POINT('Ctrl Pts',(20.4446118559668,17.9637567664559,17.9931738531268));
#190999=CARTESIAN_POINT('Ctrl Pts',(20.4717390818637,18.0013687726289,17.9903603920129));
#191000=CARTESIAN_POINT('Ctrl Pts',(20.4917428545349,18.0306252112488,17.9881827514338));
#191001=CARTESIAN_POINT('Ctrl Pts',(20.5423272094405,18.108746233145,17.9823923506699));
#191002=CARTESIAN_POINT('Ctrl Pts',(20.5716613084003,18.1583791528563,17.9787370157447));
#191003=CARTESIAN_POINT('Ctrl Pts',(20.6747923302676,18.3503551352019,17.9647013992251));
#191004=CARTESIAN_POINT('Ctrl Pts',(20.7343605191413,18.499708991169,17.9539398307783));
#191005=CARTESIAN_POINT('Ctrl Pts',(20.7802600837489,18.6681255173914,17.9425861667266));
#191006=CARTESIAN_POINT('Ctrl Pts',(20.7838765009978,18.6819448244828,17.9416604713825));
#191007=CARTESIAN_POINT('Ctrl Pts',(20.7892582138368,18.7033938796504,17.9402338167324));
#191008=CARTESIAN_POINT('Ctrl Pts',(20.7911214725792,18.7109984513307,17.9397299691526));
#191009=CARTESIAN_POINT('Ctrl Pts',(20.80304652801,18.7608637340246,17.9364396271177));
#191010=CARTESIAN_POINT('Ctrl Pts',(20.8118484655297,18.8034186662922,17.9336950004071));
#191011=CARTESIAN_POINT('Ctrl Pts',(20.8206295294387,18.8536169637691,17.9305542994598));
#191012=CARTESIAN_POINT('Ctrl Pts',(20.821884531409,18.8610234078396,17.9300933683794));
#191013=CARTESIAN_POINT('Ctrl Pts',(20.8238483803386,18.8729998063972,17.929352174678));
#191014=CARTESIAN_POINT('Ctrl Pts',(20.8245817101916,18.8775656022116,17.9290705782175));
#191015=CARTESIAN_POINT('Ctrl Pts',(20.8258556216553,18.8856665601731,17.9285727152734));
#191016=CARTESIAN_POINT('Ctrl Pts',(20.8264022115365,18.8892007228718,17.9283561122643));
#191017=CARTESIAN_POINT('Ctrl Pts',(20.8275535386188,18.8967719871733,17.9278933700577));
#191018=CARTESIAN_POINT('Ctrl Pts',(20.828155554004,18.9008094466465,17.9276473859137));
#191019=CARTESIAN_POINT('Ctrl Pts',(20.8297747227331,18.911888108136,17.926974484709));
#191020=CARTESIAN_POINT('Ctrl Pts',(20.8307680778246,18.9189328101458,17.9265488930767));
#191021=CARTESIAN_POINT('Ctrl Pts',(20.8358632932361,18.9564335439481,17.9242949130991));
#191022=CARTESIAN_POINT('Ctrl Pts',(20.8393373739792,18.9869728837622,17.9224998288459));
#191023=CARTESIAN_POINT('Ctrl Pts',(20.8478187974684,19.0794140115214,17.917159128473));
#191024=CARTESIAN_POINT('Ctrl Pts',(20.8507692325605,19.1414736032094,17.9136985749968));
#191025=CARTESIAN_POINT('Ctrl Pts',(20.8515020647841,19.3504777029911,17.9022076870108));
#191026=CARTESIAN_POINT('Ctrl Pts',(20.836726033996,19.4970296331771,17.894393777087));
#191027=CARTESIAN_POINT('Ctrl Pts',(20.7917426403449,19.7139446565672,17.8820237681741));
#191028=CARTESIAN_POINT('Ctrl Pts',(20.7727375162154,19.7861571054887,17.8777714523651));
#191029=CARTESIAN_POINT('Ctrl Pts',(20.7459588025204,19.8696977498765,17.8726239499246));
#191030=CARTESIAN_POINT('Ctrl Pts',(20.7418402415141,19.8821471535625,17.8718508507838));
#191031=CARTESIAN_POINT('Ctrl Pts',(20.7349598914134,19.9023144657568,17.8705883435627));
#191032=CARTESIAN_POINT('Ctrl Pts',(20.7322684274895,19.9100561253736,17.8701012598875));
#191033=CARTESIAN_POINT('Ctrl Pts',(20.7273954921333,19.9238143996634,17.8692311891521));
#191034=CARTESIAN_POINT('Ctrl Pts',(20.725231555384,19.9298371497625,17.8688487889445));
#191035=CARTESIAN_POINT('Ctrl Pts',(20.7206142430144,19.9425073868644,17.8680410685596));
#191036=CARTESIAN_POINT('Ctrl Pts',(20.7181547393491,19.9491525425025,17.8676155475376));
#191037=CARTESIAN_POINT('Ctrl Pts',(20.7115607172459,19.9666973638918,17.866486982612));
#191038=CARTESIAN_POINT('Ctrl Pts',(20.7073694928482,19.9775753272612,17.8657820455699));
#191039=CARTESIAN_POINT('Ctrl Pts',(20.6874757396769,20.0279633644001,17.8624919759757));
#191040=CARTESIAN_POINT('Ctrl Pts',(20.6706760015987,20.0670270203303,17.859870065302));
#191041=CARTESIAN_POINT('Ctrl Pts',(20.6211523552231,20.1732491068526,17.8525365727408));
#191042=CARTESIAN_POINT('Ctrl Pts',(20.5860349627057,20.2392178570208,17.847748635772));
#191043=CARTESIAN_POINT('Ctrl Pts',(20.4781659525271,20.4183274708986,17.8341270287711));
#191044=CARTESIAN_POINT('Ctrl Pts',(20.3980195168164,20.5265954937742,17.8251332411692));
#191045=CARTESIAN_POINT('Ctrl Pts',(20.2985350816605,20.6372278452781,17.8154547656744));
#191046=CARTESIAN_POINT('Ctrl Pts',(20.2888085551305,20.6478250622142,17.8145225033542));
#191047=CARTESIAN_POINT('Ctrl Pts',(20.2756203479755,20.661903089272,17.8132778759741));
#191048=CARTESIAN_POINT('Ctrl Pts',(20.2722536162943,20.6654720294137,17.8129618104336));
#191049=CARTESIAN_POINT('Ctrl Pts',(20.2370057730656,20.702577605314,17.8096703805597));
#191050=CARTESIAN_POINT('Ctrl Pts',(20.2040429620984,20.7350749666842,17.8067416687523));
#191051=CARTESIAN_POINT('Ctrl Pts',(20.1644172472134,20.7716582064957,17.8034169227904));
#191052=CARTESIAN_POINT('Ctrl Pts',(20.1587674340117,20.7768177740928,17.8029473428258));
#191053=CARTESIAN_POINT('Ctrl Pts',(20.1496642432143,20.7850409965516,17.8021980355265));
#191054=CARTESIAN_POINT('Ctrl Pts',(20.1462286617711,20.7881241283246,17.8019168924313));
#191055=CARTESIAN_POINT('Ctrl Pts',(20.1401076462442,20.7935811617298,17.8014189573226));
#191056=CARTESIAN_POINT('Ctrl Pts',(20.1374262373114,20.7959595084525,17.8012018336539));
#191057=CARTESIAN_POINT('Ctrl Pts',(20.1317093346962,20.8010043834955,17.8007410599272));
#191058=CARTESIAN_POINT('Ctrl Pts',(20.1286722511425,20.8036690291311,17.8004975489827));
#191059=CARTESIAN_POINT('Ctrl Pts',(20.1204086158847,20.8108775304631,17.7998383653363));
#191060=CARTESIAN_POINT('Ctrl Pts',(20.1151673126897,20.8154045063707,17.7994239292089));
#191061=CARTESIAN_POINT('Ctrl Pts',(20.0884293472343,20.8382702761116,17.7973276717859));
#191062=CARTESIAN_POINT('Ctrl Pts',(20.0665881731456,20.8562040435523,17.7956738720474));
#191063=CARTESIAN_POINT('Ctrl Pts',(20.0014877940827,20.9075105336547,17.7908914905463));
#191064=CARTESIAN_POINT('Ctrl Pts',(19.9572864013886,20.9396539575593,17.7878284188086));
#191065=CARTESIAN_POINT('Ctrl Pts',(19.791190389639,21.0508743040341,17.7767813704655));
#191066=CARTESIAN_POINT('Ctrl Pts',(19.6624951683983,21.1190586362279,17.769066338311));
#191067=CARTESIAN_POINT('Ctrl Pts',(19.4900493056413,21.1888117463425,17.7587442219642));
#191068=CARTESIAN_POINT('Ctrl Pts',(19.4518374871976,21.2029987335442,17.7564601158652));
#191069=CARTESIAN_POINT('Ctrl Pts',(19.3669280580991,21.2317627633867,17.7513661083166));
#191070=CARTESIAN_POINT('Ctrl Pts',(19.3200880239051,21.2458416052626,17.7485438158493));
#191071=CARTESIAN_POINT('Ctrl Pts',(19.2605913014438,21.2614999657773,17.7449256079353));
#191072=CARTESIAN_POINT('Ctrl Pts',(19.2483492267546,21.2646049695469,17.7441794064999));
#191073=CARTESIAN_POINT('Ctrl Pts',(19.2289158894502,21.2693492537257,17.7429918703078));
#191074=CARTESIAN_POINT('Ctrl Pts',(19.2217424611133,21.2710608431452,17.7425528712005));
#191075=CARTESIAN_POINT('Ctrl Pts',(19.2083653142325,21.2741788607841,17.7417329608899));
#191076=CARTESIAN_POINT('Ctrl Pts',(19.2021639001992,21.2755948813547,17.7413523634577));
#191077=CARTESIAN_POINT('Ctrl Pts',(19.1883831752845,21.2786762679187,17.7405054514086));
#191078=CARTESIAN_POINT('Ctrl Pts',(19.1808009267746,21.2803279460318,17.7400387030168));
#191079=CARTESIAN_POINT('Ctrl Pts',(19.158764846024,21.2850014148626,17.7386798823254));
#191080=CARTESIAN_POINT('Ctrl Pts',(19.1442884852242,21.2879136681212,17.737784322947));
#191081=CARTESIAN_POINT('Ctrl Pts',(19.0300817511341,21.3096483698409,17.7306950507874));
#191082=CARTESIAN_POINT('Ctrl Pts',(18.9291597447491,21.3214257443406,17.7242767301331));
#191083=CARTESIAN_POINT('Ctrl Pts',(18.6828357156602,21.3323499372098,17.7082809931213));
#191084=CARTESIAN_POINT('Ctrl Pts',(18.5376112155749,21.3238585078112,17.6985569461534));
#191085=CARTESIAN_POINT('Ctrl Pts',(18.380196148862,21.2982754887016,17.6881851794455));
#191086=CARTESIAN_POINT('Ctrl Pts',(18.3660141538637,21.2958219497368,17.6872526275887));
#191087=CARTESIAN_POINT('Ctrl Pts',(18.337192810706,21.2905324877367,17.6853625878601));
#191088=CARTESIAN_POINT('Ctrl Pts',(18.3225560957591,21.287686121191,17.6844054578225));
#191089=CARTESIAN_POINT('Ctrl Pts',(18.271970368763,21.2772930154982,17.6811095646575));
#191090=CARTESIAN_POINT('Ctrl Pts',(18.2361862742989,21.2689650327601,17.6787991238542));
#191091=CARTESIAN_POINT('Ctrl Pts',(18.1937265790424,21.2579109865741,17.6760973079634));
#191092=CARTESIAN_POINT('Ctrl Pts',(18.1868275058744,21.2560775587583,17.6756595669895));
#191093=CARTESIAN_POINT('Ctrl Pts',(18.1755837192479,21.2530285523958,17.6749483729101));
#191094=CARTESIAN_POINT('Ctrl Pts',(18.1712334496022,21.2518339378875,17.6746737518077));
#191095=CARTESIAN_POINT('Ctrl Pts',(18.1634514332855,21.2496701666862,17.6741835083521));
#191096=CARTESIAN_POINT('Ctrl Pts',(18.1600182987725,21.2487062405505,17.6739675881933));
#191097=CARTESIAN_POINT('Ctrl Pts',(18.1525865592529,21.2465993479337,17.6735009629067));
#191098=CARTESIAN_POINT('Ctrl Pts',(18.148588894267,21.245453276032,17.6732504411495));
#191099=CARTESIAN_POINT('Ctrl Pts',(18.1374263951272,21.2422175251994,17.67255220832));
#191100=CARTESIAN_POINT('Ctrl Pts',(18.1302691144494,21.2401017032923,17.6721059938375));
#191101=CARTESIAN_POINT('Ctrl Pts',(18.0886728884794,21.2275655281857,17.6695205676724));
#191102=CARTESIAN_POINT('Ctrl Pts',(18.0544906744736,21.2163057208929,17.6674273527095));
#191103=CARTESIAN_POINT('Ctrl Pts',(17.9453227525449,21.1772328106099,17.6607946101409));
#191104=CARTESIAN_POINT('Ctrl Pts',(17.8716166476411,21.1460401074211,17.6563959346594));
#191105=CARTESIAN_POINT('Ctrl Pts',(17.6755087981349,21.0496091444333,17.6444820654423));
#191106=CARTESIAN_POINT('Ctrl Pts',(17.5574798616707,20.976413758155,17.6370529466826));
#191107=CARTESIAN_POINT('Ctrl Pts',(17.3992536746686,20.8553309886138,17.6258273988771));
#191108=CARTESIAN_POINT('Ctrl Pts',(17.3526695995275,20.8163963633845,17.6223454084903));
#191109=CARTESIAN_POINT('Ctrl Pts',(17.298710166962,20.7672082799283,17.6180565504279));
#191110=CARTESIAN_POINT('Ctrl Pts',(17.2896683243945,20.7588201176285,17.6173288102015));
#191111=CARTESIAN_POINT('Ctrl Pts',(17.2749135851657,20.744890207889,17.616125942372));
#191112=CARTESIAN_POINT('Ctrl Pts',(17.2691576504602,20.7393943287523,17.6156527858108));
#191113=CARTESIAN_POINT('Ctrl Pts',(17.2588471254062,20.7294378932487,17.6147980768227));
#191114=CARTESIAN_POINT('Ctrl Pts',(17.254281414801,20.7249889518481,17.6144170329893));
#191115=CARTESIAN_POINT('Ctrl Pts',(17.2454688079982,20.7163237866073,17.6136765292058));
#191116=CARTESIAN_POINT('Ctrl Pts',(17.2412195536362,20.7121100392367,17.6133171801826));
#191117=CARTESIAN_POINT('Ctrl Pts',(17.2296415438039,20.7005309977516,17.6123317158141));
#191118=CARTESIAN_POINT('Ctrl Pts',(17.2223491273089,20.6931297483877,17.6117040045766));
#191119=CARTESIAN_POINT('Ctrl Pts',(17.1924047914128,20.6622876319879,17.6090969754829));
#191120=CARTESIAN_POINT('Ctrl Pts',(17.1702422612203,20.6383798116048,17.6070966336874));
#191121=CARTESIAN_POINT('Ctrl Pts',(17.1143839115119,20.5752598173887,17.6018645272729));
#191122=CARTESIAN_POINT('Ctrl Pts',(17.0815581444142,20.5353097642489,17.5985993595146));
#191123=CARTESIAN_POINT('Ctrl Pts',(17.0065533484709,20.4368911293803,17.5906680724658));
#191124=CARTESIAN_POINT('Ctrl Pts',(16.9658348215739,20.3773925694132,17.585960920878));
#191125=CARTESIAN_POINT('Ctrl Pts',(16.8548579529873,20.196026187114,17.5719542995044));
#191126=CARTESIAN_POINT('Ctrl Pts',(16.7936223883586,20.0691226949405,17.5625613341293));
#191127=CARTESIAN_POINT('Ctrl Pts',(16.7454193509487,19.937110186004,17.5536949115506));
#191128=CARTESIAN_POINT('Ctrl Pts',(16.7454194652257,19.9371104989717,17.3329785907215));
#191129=CARTESIAN_POINT('Ctrl Pts',(16.7725602230355,20.0114402087829,17.337312538183));
#191130=CARTESIAN_POINT('Ctrl Pts',(16.8038714332608,20.0842567474831,17.3417076801611));
#191131=CARTESIAN_POINT('Ctrl Pts',(16.8585886909295,20.1940592153942,17.3487130099493));
#191132=CARTESIAN_POINT('Ctrl Pts',(16.8791370174813,20.2323010954823,17.351227264728));
#191133=CARTESIAN_POINT('Ctrl Pts',(16.9067169244504,20.2800478814102,17.354474763141));
#191134=CARTESIAN_POINT('Ctrl Pts',(16.9126730514641,20.2901640047262,17.3551691378256));
#191135=CARTESIAN_POINT('Ctrl Pts',(16.922367974912,20.3063213550115,17.3562886166596));
#191136=CARTESIAN_POINT('Ctrl Pts',(16.9260536348083,20.3123942998627,17.3567117784607));
#191137=CARTESIAN_POINT('Ctrl Pts',(16.9331155510599,20.3238994151,17.3575180641209));
#191138=CARTESIAN_POINT('Ctrl Pts',(16.9364860010985,20.3293350700601,17.3579009712056));
#191139=CARTESIAN_POINT('Ctrl Pts',(16.9442142253304,20.3416734800604,17.3587746784973));
#191140=CARTESIAN_POINT('Ctrl Pts',(16.9485873779769,20.3485664393469,17.3592660448912));
#191141=CARTESIAN_POINT('Ctrl Pts',(16.9600300737485,20.3663738803427,17.3605440298342));
#191142=CARTESIAN_POINT('Ctrl Pts',(16.9671604315237,20.3772486999079,17.3613329088659));
#191143=CARTESIAN_POINT('Ctrl Pts',(17.0144890708334,20.4480013749436,17.3665216444505));
#191144=CARTESIAN_POINT('Ctrl Pts',(17.0576204015997,20.5058512421002,17.3710323454314));
#191145=CARTESIAN_POINT('Ctrl Pts',(17.2306337501685,20.7147388944703,17.3883674657624));
#191146=CARTESIAN_POINT('Ctrl Pts',(17.3786300076174,20.8493823399726,17.4018661683172));
#191147=CARTESIAN_POINT('Ctrl Pts',(17.5665601941078,20.9772301617461,17.4164314443218));
#191148=CARTESIAN_POINT('Ctrl Pts',(17.5901988043808,20.9926294971176,17.4182203772666));
#191149=CARTESIAN_POINT('Ctrl Pts',(17.6242426301299,21.0138503324909,17.4207286344568));
#191150=CARTESIAN_POINT('Ctrl Pts',(17.6343992249504,21.0200629869978,17.4214685155628));
#191151=CARTESIAN_POINT('Ctrl Pts',(17.6501248709692,21.0295007847042,17.4226005253173));
#191152=CARTESIAN_POINT('Ctrl Pts',(17.6556569496467,21.0327866690262,17.4229961934352));
#191153=CARTESIAN_POINT('Ctrl Pts',(17.6648578343665,21.0381951163327,17.4236499206005));
#191154=CARTESIAN_POINT('Ctrl Pts',(17.6685181442491,21.0403319488982,17.4239088543012));
#191155=CARTESIAN_POINT('Ctrl Pts',(17.6756226674773,21.0444509027633,17.4244092059258));
#191156=CARTESIAN_POINT('Ctrl Pts',(17.6790660900925,21.0464343456439,17.4246507070899));
#191157=CARTESIAN_POINT('Ctrl Pts',(17.6855282267345,21.0501324021827,17.4251020046766));
#191158=CARTESIAN_POINT('Ctrl Pts',(17.6885455380733,21.0518492660505,17.425311941548));
#191159=CARTESIAN_POINT('Ctrl Pts',(17.6955600060432,21.0558177213636,17.4257981909739));
#191160=CARTESIAN_POINT('Ctrl Pts',(17.6995602624646,21.0580637445477,17.4260741439447));
#191161=CARTESIAN_POINT('Ctrl Pts',(17.7118939679995,21.0649361120022,17.4269209261227));
#191162=CARTESIAN_POINT('Ctrl Pts',(17.7202515174681,21.0695192680961,17.427489060156));
#191163=CARTESIAN_POINT('Ctrl Pts',(17.8328301191873,21.130270338079,17.4350701511583));
#191164=CARTESIAN_POINT('Ctrl Pts',(17.9415692934468,21.1776640467935,17.4415759625947));
#191165=CARTESIAN_POINT('Ctrl Pts',(18.1572750850971,21.2508620152078,17.4539777147496));
#191166=CARTESIAN_POINT('Ctrl Pts',(18.2634015776809,21.277926440636,17.4598663184589));
#191167=CARTESIAN_POINT('Ctrl Pts',(18.4457333716214,21.3096481423162,17.4701568104535));
#191168=CARTESIAN_POINT('Ctrl Pts',(18.5209629135362,21.3186136102335,17.4744487915918));
#191169=CARTESIAN_POINT('Ctrl Pts',(18.6153647853529,21.3247577549594,17.4799719546709));
#191170=CARTESIAN_POINT('Ctrl Pts',(18.634238700449,21.3257325622059,17.481082862363));
#191171=CARTESIAN_POINT('Ctrl Pts',(18.6616875168986,21.3267819755726,17.4827090989354));
#191172=CARTESIAN_POINT('Ctrl Pts',(18.6702541489368,21.3270574015245,17.4832181384105));
#191173=CARTESIAN_POINT('Ctrl Pts',(18.685271813099,21.3274489577095,17.484113224062));
#191174=CARTESIAN_POINT('Ctrl Pts',(18.6917221828792,21.3275876337977,17.4844985587245));
#191175=CARTESIAN_POINT('Ctrl Pts',(18.7042449731198,21.327799593116,17.4852483935255));
#191176=CARTESIAN_POINT('Ctrl Pts',(18.7103172792509,21.3278762378995,17.4856127843977));
#191177=CARTESIAN_POINT('Ctrl Pts',(18.7248286622531,21.3279969546946,17.4864855297316));
#191178=CARTESIAN_POINT('Ctrl Pts',(18.7332677890517,21.3280166934304,17.4869946421783));
#191179=CARTESIAN_POINT('Ctrl Pts',(18.7636879697191,21.3279059512566,17.4888355887479));
#191180=CARTESIAN_POINT('Ctrl Pts',(18.7856659630545,21.3274835820525,17.4901765150419));
#191181=CARTESIAN_POINT('Ctrl Pts',(18.9943959182488,21.3202192132553,17.5030191343461));
#191182=CARTESIAN_POINT('Ctrl Pts',(19.1794431472078,21.2890192375423,17.5153328733916));
#191183=CARTESIAN_POINT('Ctrl Pts',(19.4337333284128,21.2105880421159,17.5328997662787));
#191184=CARTESIAN_POINT('Ctrl Pts',(19.5081522198843,21.1829708667613,17.5381086118322));
#191185=CARTESIAN_POINT('Ctrl Pts',(19.613663764567,21.1369186202309,17.545445853199));
#191186=CARTESIAN_POINT('Ctrl Pts',(19.6461112997014,21.1217653438801,17.5476949252236));
#191187=CARTESIAN_POINT('Ctrl Pts',(19.6848311993081,21.1024715356176,17.5503563393242));
#191188=CARTESIAN_POINT('Ctrl Pts',(19.6914839790253,21.0991125425504,17.5508128018216));
#191189=CARTESIAN_POINT('Ctrl Pts',(19.7018192539775,21.0938255804594,17.5515204904599));
#191190=CARTESIAN_POINT('Ctrl Pts',(19.7055139677165,21.0919218181571,17.551773191109));
#191191=CARTESIAN_POINT('Ctrl Pts',(19.7123683348977,21.0883644075471,17.5522414270306));
#191192=CARTESIAN_POINT('Ctrl Pts',(19.715529386381,21.0867136725522,17.5524571349789));
#191193=CARTESIAN_POINT('Ctrl Pts',(19.7226827107308,21.0829550950428,17.5529447647721));
#191194=CARTESIAN_POINT('Ctrl Pts',(19.7266724113118,21.080842470649,17.5532163799525));
#191195=CARTESIAN_POINT('Ctrl Pts',(19.738477290575,21.0745431245641,17.55401907963));
#191196=CARTESIAN_POINT('Ctrl Pts',(19.7462730722755,21.0703199933709,17.5545479127832));
#191197=CARTESIAN_POINT('Ctrl Pts',(19.8041311381396,21.0385053590631,17.5584650810947));
#191198=CARTESIAN_POINT('Ctrl Pts',(19.8530887934576,21.0089427107954,17.561736838516));
#191199=CARTESIAN_POINT('Ctrl Pts',(20.0368146583173,20.8875849393916,17.5740815581704));
#191200=CARTESIAN_POINT('Ctrl Pts',(20.1620079583049,20.782325195681,17.582678033751));
#191201=CARTESIAN_POINT('Ctrl Pts',(20.3155037972149,20.6196208636332,17.5950627299056));
#191202=CARTESIAN_POINT('Ctrl Pts',(20.3552033109749,20.5737420894667,17.598468683245));
#191203=CARTESIAN_POINT('Ctrl Pts',(20.4157132092362,20.4974217060215,17.6040604539571));
#191204=CARTESIAN_POINT('Ctrl Pts',(20.4377944175734,20.4680300180912,17.6061972623089));
#191205=CARTESIAN_POINT('Ctrl Pts',(20.4655214805814,20.4290497353363,17.6090172787097));
#191206=CARTESIAN_POINT('Ctrl Pts',(20.4718734630607,20.4199696500724,17.6096732086634));
#191207=CARTESIAN_POINT('Ctrl Pts',(20.4820974114008,20.4051075563819,17.6107454500564));
#191208=CARTESIAN_POINT('Ctrl Pts',(20.486012723312,20.3993555156311,17.611160106472));
#191209=CARTESIAN_POINT('Ctrl Pts',(20.4934941140897,20.3882471569856,17.6119603079193));
#191210=CARTESIAN_POINT('Ctrl Pts',(20.4970642730603,20.3828936700007,17.612345692792));
#191211=CARTESIAN_POINT('Ctrl Pts',(20.5051918090715,20.3705851487282,17.613231205232));
#191212=CARTESIAN_POINT('Ctrl Pts',(20.509732705614,20.3636194067449,17.6137319433897));
#191213=CARTESIAN_POINT('Ctrl Pts',(20.5217064717902,20.3450129289898,17.6150685229631));
#191214=CARTESIAN_POINT('Ctrl Pts',(20.5290665674428,20.3333260473929,17.6159070475437));
#191215=CARTESIAN_POINT('Ctrl Pts',(20.5854499806287,20.2418229028816,17.6224656555343));
#191216=CARTESIAN_POINT('Ctrl Pts',(20.6292349291666,20.1589152438195,17.6283760579522));
#191217=CARTESIAN_POINT('Ctrl Pts',(20.7243942421536,19.9455787281531,17.6434834160732));
#191218=CARTESIAN_POINT('Ctrl Pts',(20.7685887250795,19.8124311045116,17.6528409103574));
#191219=CARTESIAN_POINT('Ctrl Pts',(20.8108330231094,19.6247658258836,17.6654197906971));
#191220=CARTESIAN_POINT('Ctrl Pts',(20.8204433040419,19.5732052543762,17.6688111360771));
#191221=CARTESIAN_POINT('Ctrl Pts',(20.8321596304407,19.4941446232171,17.6738646684591));
#191222=CARTESIAN_POINT('Ctrl Pts',(20.8356596809801,19.4668739241012,17.6755814310299));
#191223=CARTESIAN_POINT('Ctrl Pts',(20.8393686706081,19.4327179916943,17.6776923869868));
#191224=CARTESIAN_POINT('Ctrl Pts',(20.840076441674,19.4258909766083,17.6781123660756));
#191225=CARTESIAN_POINT('Ctrl Pts',(20.8411467367856,19.4150535281288,17.6787758268793));
#191226=CARTESIAN_POINT('Ctrl Pts',(20.8415310355407,19.4110453637206,17.6790205037693));
#191227=CARTESIAN_POINT('Ctrl Pts',(20.8422360871946,19.4034642028226,17.6794819380338));
#191228=CARTESIAN_POINT('Ctrl Pts',(20.8425591900312,19.3998915324176,17.6796988193664));
#191229=CARTESIAN_POINT('Ctrl Pts',(20.8432793871146,19.3916958660629,17.680195052501));
#191230=CARTESIAN_POINT('Ctrl Pts',(20.8436703646585,19.3870723781251,17.6804740582949));
#191231=CARTESIAN_POINT('Ctrl Pts',(20.8446723395946,19.3747408351391,17.6812157964933));
#191232=CARTESIAN_POINT('Ctrl Pts',(20.845256320476,19.3670305726508,17.6816770544119));
#191233=CARTESIAN_POINT('Ctrl Pts',(20.8491566389808,19.3114963005168,17.6849823602183));
#191234=CARTESIAN_POINT('Ctrl Pts',(20.8508902084216,19.2635711109657,17.6877443047049));
#191235=CARTESIAN_POINT('Ctrl Pts',(20.8510570524012,19.1871956969861,17.6920596577943));
#191236=CARTESIAN_POINT('Ctrl Pts',(20.8505464969716,19.1587674833856,17.6936468781337));
#191237=CARTESIAN_POINT('Ctrl Pts',(20.8478034290527,19.0868097947237,17.6976346678849));
#191238=CARTESIAN_POINT('Ctrl Pts',(20.8447990599264,19.0433227144897,17.700017126262));
#191239=CARTESIAN_POINT('Ctrl Pts',(20.8295555435786,18.8911737271371,17.70834212114));
#191240=CARTESIAN_POINT('Ctrl Pts',(20.8102459993496,18.7833979125856,17.7142292058674));
#191241=CARTESIAN_POINT('Ctrl Pts',(20.7636355968937,18.6043751919849,17.7245155785706));
#191242=CARTESIAN_POINT('Ctrl Pts',(20.7406605717448,18.5322320554643,17.7288049202135));
#191243=CARTESIAN_POINT('Ctrl Pts',(20.7071864917377,18.4438096833279,17.7343249019519));
#191244=CARTESIAN_POINT('Ctrl Pts',(20.7002617025218,18.4262320112675,17.7354354298721));
#191245=CARTESIAN_POINT('Ctrl Pts',(20.6898551431418,18.4008190931522,17.7370612112782));
#191246=CARTESIAN_POINT('Ctrl Pts',(20.6865594462201,18.3929082884802,17.7375701803849));
#191247=CARTESIAN_POINT('Ctrl Pts',(20.6806986091872,18.3790774378798,17.7384651846463));
#191248=CARTESIAN_POINT('Ctrl Pts',(20.6781542540807,18.3731486651598,17.7388505086908));
#191249=CARTESIAN_POINT('Ctrl Pts',(20.6731622914622,18.3616617336639,17.7396003542655));
#191250=CARTESIAN_POINT('Ctrl Pts',(20.670717786855,18.3561022890567,17.7399647666774));
#191251=CARTESIAN_POINT('Ctrl Pts',(20.6648188047324,18.3428416127585,17.7408376143543));
#191252=CARTESIAN_POINT('Ctrl Pts',(20.6613421451503,18.3351504156846,17.7413468080064));
#191253=CARTESIAN_POINT('Ctrl Pts',(20.6486422874153,18.3074971154198,17.7431883478214));
#191254=CARTESIAN_POINT('Ctrl Pts',(20.6391544393805,18.2876587542672,17.7445297937903));
#191255=CARTESIAN_POINT('Ctrl Pts',(20.5461505869449,18.10073343788,17.7573680789841));
#191256=CARTESIAN_POINT('Ctrl Pts',(20.4411872885948,17.9452729316278,17.7696761601614));
#191257=CARTESIAN_POINT('Ctrl Pts',(20.2645484207317,17.7462785429009,17.7872413535598));
#191258=CARTESIAN_POINT('Ctrl Pts',(20.2085640850832,17.6899313409217,17.7924537833828));
#191259=CARTESIAN_POINT('Ctrl Pts',(20.1229114919839,17.6129084003772,17.7997953804239));
#191260=CARTESIAN_POINT('Ctrl Pts',(20.0956731975029,17.5896368855449,17.8020453713521));
#191261=CARTESIAN_POINT('Ctrl Pts',(20.062067851755,17.5623701647259,17.8047077227985));
#191262=CARTESIAN_POINT('Ctrl Pts',(20.0562551626246,17.5577045511064,17.805164239308));
#191263=CARTESIAN_POINT('Ctrl Pts',(20.0471626993015,17.5504850191746,17.8058719932761));
#191264=CARTESIAN_POINT('Ctrl Pts',(20.0438999058625,17.5479099502163,17.8061247056742));
#191265=CARTESIAN_POINT('Ctrl Pts',(20.0378236828778,17.5431434350395,17.8065929522284));
#191266=CARTESIAN_POINT('Ctrl Pts',(20.035012327124,17.5409495090687,17.80680865913));
#191267=CARTESIAN_POINT('Ctrl Pts',(20.0286295671,17.5359944292625,17.8072962723943));
#191268=CARTESIAN_POINT('Ctrl Pts',(20.0250548760241,17.5332375954943,17.80756787218));
#191269=CARTESIAN_POINT('Ctrl Pts',(20.0144344205575,17.5251010476585,17.8083704842008));
#191270=CARTESIAN_POINT('Ctrl Pts',(20.0073635530933,17.519754053747,17.8088992458226));
#191271=CARTESIAN_POINT('Ctrl Pts',(19.9544765039958,17.4802805509821,17.8128143882614));
#191272=CARTESIAN_POINT('Ctrl Pts',(19.9073249707374,17.447973497681,17.8160843276193));
#191273=CARTESIAN_POINT('Ctrl Pts',(19.7306678475249,17.3371636798078,17.8277759767483));
#191274=CARTESIAN_POINT('Ctrl Pts',(19.5941509554465,17.270702279564,17.8357918015864));
#191275=CARTESIAN_POINT('Ctrl Pts',(19.3644865293258,17.1879402901132,17.8492377616149));
#191276=CARTESIAN_POINT('Ctrl Pts',(19.2753073678149,17.1622766631443,17.8544436038009));
#191277=CARTESIAN_POINT('Ctrl Pts',(19.1641540250916,17.1380551351852,17.8610701491971));
#191278=CARTESIAN_POINT('Ctrl Pts',(19.1435029882135,17.1338769527762,17.8623066903037));
#191279=CARTESIAN_POINT('Ctrl Pts',(19.113990854512,17.1283631754571,17.8640828166579));
#191280=CARTESIAN_POINT('Ctrl Pts',(19.1051779039577,17.1267744478308,17.864614341065));
#191281=CARTESIAN_POINT('Ctrl Pts',(19.0899348883612,17.1241263046655,17.865535735873));
#191282=CARTESIAN_POINT('Ctrl Pts',(19.0835094765311,17.1230405680707,17.8659247640197));
#191283=CARTESIAN_POINT('Ctrl Pts',(19.0711818098217,17.1210159942013,17.8666723941034));
#191284=CARTESIAN_POINT('Ctrl Pts',(19.0652803833428,17.1200724489254,17.8670308423987));
#191285=CARTESIAN_POINT('Ctrl Pts',(19.0498904953804,17.1176786369862,17.8679670756449));
#191286=CARTESIAN_POINT('Ctrl Pts',(19.0403961045692,17.1162679034589,17.8685461078308));
#191287=CARTESIAN_POINT('Ctrl Pts',(19.0078136638254,17.1116528635474,17.8705383402355));
#191288=CARTESIAN_POINT('Ctrl Pts',(18.9846831061629,17.1087654189029,17.8719614902819));
#191289=CARTESIAN_POINT('Ctrl Pts',(18.7917146785541,17.0879066359558,17.8839119481677));
#191290=CARTESIAN_POINT('Ctrl Pts',(18.6203523441901,17.0901702205066,17.8951011230179));
#191291=CARTESIAN_POINT('Ctrl Pts',(18.3616209376551,17.1250503161618,17.9123532550351));
#191292=CARTESIAN_POINT('Ctrl Pts',(18.2729392378524,17.1428420709198,17.9183162893897));
#191293=CARTESIAN_POINT('Ctrl Pts',(18.1483250946236,17.1762596863198,17.9265592877393));
#191294=CARTESIAN_POINT('Ctrl Pts',(18.1112673324332,17.1872935738502,17.9289921554776));
#191295=CARTESIAN_POINT('Ctrl Pts',(18.0672904398798,17.2017102234611,17.9318402844786));
#191296=CARTESIAN_POINT('Ctrl Pts',(18.0600636236669,17.2041226224891,17.9323070444057));
#191297=CARTESIAN_POINT('Ctrl Pts',(18.0488803793875,17.2079229466031,17.9330271792049));
#191298=CARTESIAN_POINT('Ctrl Pts',(18.0449148714206,17.2092836707796,17.9332821118388));
#191299=CARTESIAN_POINT('Ctrl Pts',(18.037586813933,17.2118225770069,17.9337523971078));
#191300=CARTESIAN_POINT('Ctrl Pts',(18.0342232243212,17.2129974577437,17.9339679355811));
#191301=CARTESIAN_POINT('Ctrl Pts',(18.0266492261547,17.2156644803741,17.9344525589975));
#191302=CARTESIAN_POINT('Ctrl Pts',(18.0224405771749,17.2171614554408,17.9347213533454));
#191303=CARTESIAN_POINT('Ctrl Pts',(18.0101011300934,17.2215945221116,17.9355080658885));
#191304=CARTESIAN_POINT('Ctrl Pts',(18.0019834281366,17.2245671484785,17.9360238640294));
#191305=CARTESIAN_POINT('Ctrl Pts',(17.9455371131738,17.2456302717825,17.9395997093367));
#191306=CARTESIAN_POINT('Ctrl Pts',(17.8978616827471,17.2654343910455,17.9425649576661));
#191307=CARTESIAN_POINT('Ctrl Pts',(17.8310733511714,17.2960872205023,17.9467037793076));
#191308=CARTESIAN_POINT('Ctrl Pts',(17.811334977799,17.3055192761789,17.9479249859216));
#191309=CARTESIAN_POINT('Ctrl Pts',(17.6684463234817,17.3765401560088,17.9567751509095));
#191310=CARTESIAN_POINT('Ctrl Pts',(17.5514174581383,17.4497082187226,17.9640985395546));
#191311=CARTESIAN_POINT('Ctrl Pts',(17.3704328064643,17.5890856997746,17.9766927958227));
#191312=CARTESIAN_POINT('Ctrl Pts',(17.3021869424851,17.6490044419046,17.9817933042145));
#191313=CARTESIAN_POINT('Ctrl Pts',(17.2232621475937,17.7278297618872,17.9882924156419));
#191314=CARTESIAN_POINT('Ctrl Pts',(17.2087435234247,17.7427645117518,17.9895150372841));
#191315=CARTESIAN_POINT('Ctrl Pts',(17.188329651391,17.7643930634187,17.9912746222048));
#191316=CARTESIAN_POINT('Ctrl Pts',(17.1822523881096,17.7709139606174,17.9918037316272));
#191317=CARTESIAN_POINT('Ctrl Pts',(17.1718088759356,17.7822627039517,17.9927222751508));
#191318=CARTESIAN_POINT('Ctrl Pts',(17.1674233461454,17.7870727001132,17.9931108812248));
#191319=CARTESIAN_POINT('Ctrl Pts',(17.1590478682053,17.7963443500479,17.9938586422213));
#191320=CARTESIAN_POINT('Ctrl Pts',(17.1550545168643,17.8008028557936,17.9942176480252));
#191321=CARTESIAN_POINT('Ctrl Pts',(17.1446737496373,17.8124921690202,17.9951574342582));
#191322=CARTESIAN_POINT('Ctrl Pts',(17.1383168156392,17.819749751579,17.9957394805563));
#191323=CARTESIAN_POINT('Ctrl Pts',(17.1165781267832,17.8449133613392,17.9977528026145));
#191324=CARTESIAN_POINT('Ctrl Pts',(17.1014468237556,17.8630325388784,17.999194313112));
#191325=CARTESIAN_POINT('Ctrl Pts',(16.9829318799082,18.0098729067035,18.010816152123));
#191326=CARTESIAN_POINT('Ctrl Pts',(16.8946445826061,18.150010919624,18.021610011477));
#191327=CARTESIAN_POINT('Ctrl Pts',(16.7685612817754,18.4141145820774,18.040949937191));
#191328=CARTESIAN_POINT('Ctrl Pts',(16.7241006265763,18.5340310221172,18.0493910395935));
#191329=CARTESIAN_POINT('Ctrl Pts',(16.6875909745639,18.6687441998302,18.0580465200214));
#191330=CARTESIAN_POINT('Ctrl Pts',(16.684568363399,18.6802823404743,18.0587812938641));
#191331=CARTESIAN_POINT('Ctrl Pts',(16.6804108697503,18.6967180319683,18.0598180380657));
#191332=CARTESIAN_POINT('Ctrl Pts',(16.6791957303689,18.7015947848483,18.0601244218867));
#191333=CARTESIAN_POINT('Ctrl Pts',(16.6771318955092,18.7100051828676,18.060650624776));
#191334=CARTESIAN_POINT('Ctrl Pts',(16.6762749145256,18.7135367556761,18.0608709177079));
#191335=CARTESIAN_POINT('Ctrl Pts',(16.6746311948272,18.7203873639313,18.0612969424028));
#191336=CARTESIAN_POINT('Ctrl Pts',(16.673843383718,18.7237060936567,18.0615027380218));
#191337=CARTESIAN_POINT('Ctrl Pts',(16.6717400399649,18.7326629061109,18.0620566006581));
#191338=CARTESIAN_POINT('Ctrl Pts',(16.6704395975616,18.7383045531905,18.0624038061267));
#191339=CARTESIAN_POINT('Ctrl Pts',(16.6657019231811,18.7592499785667,18.0636869544939));
#191340=CARTESIAN_POINT('Ctrl Pts',(16.6624115604281,18.7745869090283,18.064614851161));
#191341=CARTESIAN_POINT('Ctrl Pts',(16.6325545374803,18.9217095916557,18.0734167669213));
#191342=CARTESIAN_POINT('Ctrl Pts',(16.6184239749364,19.055726048318,18.0806878996701));
#191343=CARTESIAN_POINT('Ctrl Pts',(16.6170404620324,19.1964794404447,18.088331826678));
#191344=CARTESIAN_POINT('Ctrl Pts',(16.6170066729089,19.2027668310727,18.0886732592247));
#191345=CARTESIAN_POINT('Ctrl Pts',(16.6168668547703,19.3548927710488,18.0969354872158));
#191346=CARTESIAN_POINT('Ctrl Pts',(16.6318021056912,19.5003359780539,18.1048962031172));
#191347=CARTESIAN_POINT('Ctrl Pts',(16.6664676958081,19.6666057136677,18.1147554617558));
#191348=CARTESIAN_POINT('Ctrl Pts',(16.6717720454849,19.6900429933476,18.1161622442136));
#191349=CARTESIAN_POINT('Ctrl Pts',(16.679780444527,19.7228256319992,18.1181559734912));
#191350=CARTESIAN_POINT('Ctrl Pts',(16.6821518243893,19.7322509176174,18.118732225555));
#191351=CARTESIAN_POINT('Ctrl Pts',(16.68609161862,19.7474664424257,18.1196675334439));
#191352=CARTESIAN_POINT('Ctrl Pts',(16.6876199074602,19.7532669988962,18.1200252880178));
#191353=CARTESIAN_POINT('Ctrl Pts',(16.6908553251685,19.7653384122078,18.1207723208982));
#191354=CARTESIAN_POINT('Ctrl Pts',(16.6925667172331,19.7716080521106,18.1211617342632));
#191355=CARTESIAN_POINT('Ctrl Pts',(16.6966783608732,19.7864024424684,18.1220840319993));
#191356=CARTESIAN_POINT('Ctrl Pts',(16.699103276067,19.7949201582881,18.1226177143265));
#191357=CARTESIAN_POINT('Ctrl Pts',(16.7073169333128,19.823098686354,18.1243922887777));
#191358=CARTESIAN_POINT('Ctrl Pts',(16.7133375993579,19.8426901700239,18.1256407216567));
#191359=CARTESIAN_POINT('Ctrl Pts',(16.7277680314605,19.8873285000079,18.128519727433));
#191360=CARTESIAN_POINT('Ctrl Pts',(16.7363623469838,19.9123059881422,18.1301558675295));
#191361=CARTESIAN_POINT('Ctrl Pts',(16.7454193782244,19.9371102607032,18.1318062886951));
#191362=CARTESIAN_POINT('Origin',(18.734,19.211,0.));
#191363=CARTESIAN_POINT('',(16.7477767826476,19.936270776259,19.1554367658253));
#191364=CARTESIAN_POINT('',(16.7454193714968,19.9371102422787,18.9348454715054));
#191365=CARTESIAN_POINT('',(16.7454193623258,19.9371102171621,0.));
#191366=CARTESIAN_POINT('',(16.6180378694014,19.2091158125652,19.1109437209775));
#191367=CARTESIAN_POINT('Ctrl Pts',(16.6180378694014,19.2091158125652,19.1109437209775));
#191368=CARTESIAN_POINT('Ctrl Pts',(16.6201500192997,19.4559462490499,19.1257747359268));
#191369=CARTESIAN_POINT('Ctrl Pts',(16.6645218722682,19.7034418982865,19.1406057508761));
#191370=CARTESIAN_POINT('Ctrl Pts',(16.7477767826476,19.936270776259,19.1554367658253));
#191371=CARTESIAN_POINT('Ctrl Pts',(16.6170008744685,19.2090758122038,19.1115401841555));
#191372=CARTESIAN_POINT('Ctrl Pts',(16.6171446318861,19.0509133251653,19.1011782561604));
#191373=CARTESIAN_POINT('Ctrl Pts',(16.6350118723612,18.8932596446619,19.0905432530762));
#191374=CARTESIAN_POINT('Ctrl Pts',(16.6745229994948,18.7204833194059,19.079322975751));
#191375=CARTESIAN_POINT('Ctrl Pts',(16.6790219066614,18.7019644230679,19.0781267294454));
#191376=CARTESIAN_POINT('Ctrl Pts',(16.6870567960829,18.6707348074463,19.0761231159487));
#191377=CARTESIAN_POINT('Ctrl Pts',(16.6904625692902,18.6579920906677,19.0753094665024));
#191378=CARTESIAN_POINT('Ctrl Pts',(16.6953858358077,18.6402385095914,19.0741821138998));
#191379=CARTESIAN_POINT('Ctrl Pts',(16.696803075031,18.6352004866086,19.0738629058709));
#191380=CARTESIAN_POINT('Ctrl Pts',(16.6992465311558,18.6266364092212,19.0733215531984));
#191381=CARTESIAN_POINT('Ctrl Pts',(16.7002632616391,18.6231076927154,19.0730988626086));
#191382=CARTESIAN_POINT('Ctrl Pts',(16.7022279707194,18.6163549685451,19.0726734366951));
#191383=CARTESIAN_POINT('Ctrl Pts',(16.7031744467514,18.6131305618798,19.0724706126738));
#191384=CARTESIAN_POINT('Ctrl Pts',(16.7056983609903,18.6046073662642,19.071935282468));
#191385=CARTESIAN_POINT('Ctrl Pts',(16.7072888975922,18.5993124375942,19.0716035366446));
#191386=CARTESIAN_POINT('Ctrl Pts',(16.712985869796,18.5806132784766,19.0704346777269));
#191387=CARTESIAN_POINT('Ctrl Pts',(16.7172047908137,18.5672433372347,19.0696038727208));
#191388=CARTESIAN_POINT('Ctrl Pts',(16.7728160464388,18.3969234067356,19.0590717551862));
#191389=CARTESIAN_POINT('Ctrl Pts',(16.8422782435161,18.24644367624,19.0502965055289));
#191390=CARTESIAN_POINT('Ctrl Pts',(16.977247552425,18.0260063150719,19.0362193600941));
#191391=CARTESIAN_POINT('Ctrl Pts',(17.0311543347221,17.9497689381889,19.0310910973721));
#191392=CARTESIAN_POINT('Ctrl Pts',(17.1208715353498,17.8391686547966,19.0229954307018));
#191393=CARTESIAN_POINT('Ctrl Pts',(17.1531525290882,17.8020907039695,19.0201570650561));
#191394=CARTESIAN_POINT('Ctrl Pts',(17.1948767039491,17.7574071160473,19.0165592066886));
#191395=CARTESIAN_POINT('Ctrl Pts',(17.203134859877,17.7487125089201,19.0158504009069));
#191396=CARTESIAN_POINT('Ctrl Pts',(17.2157051973563,17.735701009314,19.0147761657928));
#191397=CARTESIAN_POINT('Ctrl Pts',(17.2199629962938,17.7313317365476,19.0144131009373));
#191398=CARTESIAN_POINT('Ctrl Pts',(17.2286998576546,17.7224433280528,19.0136696899763));
#191399=CARTESIAN_POINT('Ctrl Pts',(17.2331805232222,17.7179258622221,19.0132892752671));
#191400=CARTESIAN_POINT('Ctrl Pts',(17.2428809663014,17.7082335337445,19.0124674578117));
#191401=CARTESIAN_POINT('Ctrl Pts',(17.2481074531288,17.7030655313342,19.0120257590825));
#191402=CARTESIAN_POINT('Ctrl Pts',(17.2623110340044,17.6891664326575,19.0108282464363));
#191403=CARTESIAN_POINT('Ctrl Pts',(17.2713387540473,17.6804877039545,19.0100701614586));
#191404=CARTESIAN_POINT('Ctrl Pts',(17.3151231024102,17.6391371547627,19.0064074842921));
#191405=CARTESIAN_POINT('Ctrl Pts',(17.3508980821952,17.6075683786899,19.0034563260724));
#191406=CARTESIAN_POINT('Ctrl Pts',(17.4044074251072,17.5634743082188,18.9990976615589));
#191407=CARTESIAN_POINT('Ctrl Pts',(17.4213179024832,17.5499693014145,18.9977279099325));
#191408=CARTESIAN_POINT('Ctrl Pts',(17.5359996072933,17.4612275727666,18.988491042975));
#191409=CARTESIAN_POINT('Ctrl Pts',(17.6399710417779,17.3944088906082,18.9803477036228));
#191410=CARTESIAN_POINT('Ctrl Pts',(17.8256695346015,17.2968170893918,18.9664878059363));
#191411=CARTESIAN_POINT('Ctrl Pts',(17.9045801611799,17.2613269292849,18.9607924778697));
#191412=CARTESIAN_POINT('Ctrl Pts',(18.0206872900517,17.2174369719483,18.9528685869228));
#191413=CARTESIAN_POINT('Ctrl Pts',(18.0562824698198,17.2050568492692,18.9504988218728));
#191414=CARTESIAN_POINT('Ctrl Pts',(18.0993990009962,17.191339687713,18.9477146269606));
#191415=CARTESIAN_POINT('Ctrl Pts',(18.1066188021647,17.189085303102,18.947251291168));
#191416=CARTESIAN_POINT('Ctrl Pts',(18.117847702612,17.1856450132175,18.9465352929473));
#191417=CARTESIAN_POINT('Ctrl Pts',(18.1218484095555,17.1844322347686,18.9462811006578));
#191418=CARTESIAN_POINT('Ctrl Pts',(18.1292663852579,17.1822075127206,18.9458115015063));
#191419=CARTESIAN_POINT('Ctrl Pts',(18.1326825870252,17.1811923563079,18.9455959131568));
#191420=CARTESIAN_POINT('Ctrl Pts',(18.1404012307193,17.1789198854211,18.9451103214075));
#191421=CARTESIAN_POINT('Ctrl Pts',(18.1447050996938,17.1776676090021,18.9448406138121));
#191422=CARTESIAN_POINT('Ctrl Pts',(18.1573895663868,17.1740205263338,18.9440487418058));
#191423=CARTESIAN_POINT('Ctrl Pts',(18.1657811310127,17.171663762121,18.9435287393929));
#191424=CARTESIAN_POINT('Ctrl Pts',(18.2255697927548,17.155269862724,18.9398497134708));
#191425=CARTESIAN_POINT('Ctrl Pts',(18.2774706936795,17.1431243553732,18.9367918179557));
#191426=CARTESIAN_POINT('Ctrl Pts',(18.3462353565157,17.1297482997449,18.9328519248876));
#191427=CARTESIAN_POINT('Ctrl Pts',(18.3627294652925,17.1267427535456,18.9319152393935));
#191428=CARTESIAN_POINT('Ctrl Pts',(18.5244232211533,17.0992593978775,18.922799715624));
#191429=CARTESIAN_POINT('Ctrl Pts',(18.6717693275649,17.0897971408996,18.9149907051229));
#191430=CARTESIAN_POINT('Ctrl Pts',(18.8815354652985,17.0982173395463,18.9033840281849));
#191431=CARTESIAN_POINT('Ctrl Pts',(18.9440143547471,17.1035108859474,18.8998691598699));
#191432=CARTESIAN_POINT('Ctrl Pts',(19.0308678364961,17.1147702745931,18.8948446728013));
#191433=CARTESIAN_POINT('Ctrl Pts',(19.0555132099377,17.118408602556,18.8934033807674));
#191434=CARTESIAN_POINT('Ctrl Pts',(19.0985484524535,17.1255399609929,18.8908560572443));
#191435=CARTESIAN_POINT('Ctrl Pts',(19.1169671350349,17.1288435964872,18.8897559561322));
#191436=CARTESIAN_POINT('Ctrl Pts',(19.1437211571363,17.1340092801898,18.8881426764918));
#191437=CARTESIAN_POINT('Ctrl Pts',(19.1520931746421,17.1356783452091,18.8876356451222));
#191438=CARTESIAN_POINT('Ctrl Pts',(19.1667692138209,17.138696603749,18.8867428793555));
#191439=CARTESIAN_POINT('Ctrl Pts',(19.1730776325759,17.1400240489814,18.8863578449666));
#191440=CARTESIAN_POINT('Ctrl Pts',(19.1853266308028,17.1426600196209,18.8856076916917));
#191441=CARTESIAN_POINT('Ctrl Pts',(19.191267832834,17.1439653776579,18.8852426778275));
#191442=CARTESIAN_POINT('Ctrl Pts',(19.2054753784591,17.1471512081117,18.8843669771951));
#191443=CARTESIAN_POINT('Ctrl Pts',(19.2137361658393,17.1490557533757,18.8838555208074));
#191444=CARTESIAN_POINT('Ctrl Pts',(19.2436129849782,17.1561331879254,18.8819972936995));
#191445=CARTESIAN_POINT('Ctrl Pts',(19.2651580661746,17.1615966576936,18.8806412066991));
#191446=CARTESIAN_POINT('Ctrl Pts',(19.4646170644369,17.2155325742307,18.8679328061335));
#191447=CARTESIAN_POINT('Ctrl Pts',(19.6355380335178,17.2867095772915,18.8557929015899));
#191448=CARTESIAN_POINT('Ctrl Pts',(19.8650839116962,17.4196624368959,18.8382772653005));
#191449=CARTESIAN_POINT('Ctrl Pts',(19.9327485112884,17.4642187231329,18.832956966012));
#191450=CARTESIAN_POINT('Ctrl Pts',(20.0267770771401,17.534178586528,18.8254845213215));
#191451=CARTESIAN_POINT('Ctrl Pts',(20.0552970612864,17.5565583830546,18.8232070864157));
#191452=CARTESIAN_POINT('Ctrl Pts',(20.0889935523643,17.5844277109654,18.8205167584507));
#191453=CARTESIAN_POINT('Ctrl Pts',(20.0947317457668,17.589225028463,18.8200586409381));
#191454=CARTESIAN_POINT('Ctrl Pts',(20.1036234852616,17.5967392305256,18.8193489506928));
#191455=CARTESIAN_POINT('Ctrl Pts',(20.1067945806816,17.599435119772,18.819095890203));
#191456=CARTESIAN_POINT('Ctrl Pts',(20.1126674640503,17.6044578322296,18.818627327821));
#191457=CARTESIAN_POINT('Ctrl Pts',(20.1153712989724,17.6067821070972,18.8184116511215));
#191458=CARTESIAN_POINT('Ctrl Pts',(20.1214793240839,17.6120595901345,18.8179245239223));
#191459=CARTESIAN_POINT('Ctrl Pts',(20.1248799553518,17.6150168360146,18.817653377421));
#191460=CARTESIAN_POINT('Ctrl Pts',(20.1349148347956,17.6237997680625,18.816853344491));
#191461=CARTESIAN_POINT('Ctrl Pts',(20.1415222057417,17.629656205282,18.8163266872344));
#191462=CARTESIAN_POINT('Ctrl Pts',(20.1898927829367,17.6730727902719,18.8124703669765));
#191463=CARTESIAN_POINT('Ctrl Pts',(20.2301869412565,17.712243946896,18.8092532249539));
#191464=CARTESIAN_POINT('Ctrl Pts',(20.3730796475201,17.862668644287,18.7976120775301));
#191465=CARTESIAN_POINT('Ctrl Pts',(20.465226287986,17.9832211992772,18.7896009979635));
#191466=CARTESIAN_POINT('Ctrl Pts',(20.5973880215622,18.2009674269824,18.7755780329373));
#191467=CARTESIAN_POINT('Ctrl Pts',(20.6444839278699,18.2931613175155,18.7697622949186));
#191468=CARTESIAN_POINT('Ctrl Pts',(20.6904114891585,18.4020731394506,18.7628289767306));
#191469=CARTESIAN_POINT('Ctrl Pts',(20.6960256337505,18.4157868358518,18.7619550699364));
#191470=CARTESIAN_POINT('Ctrl Pts',(20.7043637100952,18.4367802394936,18.7606154479331));
#191471=CARTESIAN_POINT('Ctrl Pts',(20.7071923592345,18.444018058483,18.7601532661381));
#191472=CARTESIAN_POINT('Ctrl Pts',(20.7122640596845,18.4572090606539,18.7593102765595));
#191473=CARTESIAN_POINT('Ctrl Pts',(20.7145202575037,18.4631571165473,18.7589299156492));
#191474=CARTESIAN_POINT('Ctrl Pts',(20.71933097412,18.4760141617821,18.7581071835731));
#191475=CARTESIAN_POINT('Ctrl Pts',(20.7218763051152,18.4829264785713,18.7576645109143));
#191476=CARTESIAN_POINT('Ctrl Pts',(20.7286748283063,18.5016905595348,18.7564618263254));
#191477=CARTESIAN_POINT('Ctrl Pts',(20.7328583885205,18.5135670749731,18.755699510201));
#191478=CARTESIAN_POINT('Ctrl Pts',(20.7526313999011,18.5713393798464,18.7519855029524));
#191479=CARTESIAN_POINT('Ctrl Pts',(20.7667463907695,18.6177210225686,18.7489856587955));
#191480=CARTESIAN_POINT('Ctrl Pts',(20.7897993786112,18.7040028423859,18.7433682729105));
#191481=CARTESIAN_POINT('Ctrl Pts',(20.7991975642982,18.7437571254747,18.7407660864017));
#191482=CARTESIAN_POINT('Ctrl Pts',(20.8345936369177,18.9155365054141,18.7294716584824));
#191483=CARTESIAN_POINT('Ctrl Pts',(20.8491209798667,19.049598811803,18.7205051558096));
#191484=CARTESIAN_POINT('Ctrl Pts',(20.8516254590161,19.2468084022229,18.7075444977657));
#191485=CARTESIAN_POINT('Ctrl Pts',(20.8496363024119,19.3095086864417,18.7034626440817));
#191486=CARTESIAN_POINT('Ctrl Pts',(20.8425144307473,19.4028647468615,18.6975223401024));
#191487=CARTESIAN_POINT('Ctrl Pts',(20.839486884562,19.4336441061345,18.6955864335863));
#191488=CARTESIAN_POINT('Ctrl Pts',(20.8349328272353,19.4714247792975,18.6932469393481));
#191489=CARTESIAN_POINT('Ctrl Pts',(20.8340440306902,19.4784974443281,18.6928105715904));
#191490=CARTESIAN_POINT('Ctrl Pts',(20.8325896919388,19.489616211027,18.6921272202171));
#191491=CARTESIAN_POINT('Ctrl Pts',(20.8320481419577,19.4936653194835,18.6918789189539));
#191492=CARTESIAN_POINT('Ctrl Pts',(20.8310106013006,19.5012556176519,18.6914145351768));
#191493=CARTESIAN_POINT('Ctrl Pts',(20.8305173653483,19.5047970771597,18.69119830639));
#191494=CARTESIAN_POINT('Ctrl Pts',(20.8293663494303,19.5129109141838,18.6907038996592));
#191495=CARTESIAN_POINT('Ctrl Pts',(20.8287025761784,19.5174823921645,18.6904260636672));
#191496=CARTESIAN_POINT('Ctrl Pts',(20.8265994626474,19.5316407128541,18.6895677129786));
#191497=CARTESIAN_POINT('Ctrl Pts',(20.8251092083838,19.5412200243705,18.688990001313));
#191498=CARTESIAN_POINT('Ctrl Pts',(20.8075258664512,19.6493498686095,18.6824997969179));
#191499=CARTESIAN_POINT('Ctrl Pts',(20.7845428933871,19.7466671043616,18.6769464824106));
#191500=CARTESIAN_POINT('Ctrl Pts',(20.7039194330605,20.0048593052985,18.6621439395176));
#191501=CARTESIAN_POINT('Ctrl Pts',(20.633573517495,20.1609545822545,18.653067698507));
#191502=CARTESIAN_POINT('Ctrl Pts',(20.5300529974278,20.3320465585058,18.6416591573074));
#191503=CARTESIAN_POINT('Ctrl Pts',(20.5143266916917,20.3568571070566,18.6399671516229));
#191504=CARTESIAN_POINT('Ctrl Pts',(20.4863141012396,20.3990816559,18.6370162701542));
#191505=CARTESIAN_POINT('Ctrl Pts',(20.4742714985293,20.4166524346378,18.6357663111838));
#191506=CARTESIAN_POINT('Ctrl Pts',(20.4567698132821,20.441379645134,18.6339742543207));
#191507=CARTESIAN_POINT('Ctrl Pts',(20.4515268272503,20.448687963337,18.6334404193319));
#191508=CARTESIAN_POINT('Ctrl Pts',(20.4424010758871,20.4612389058725,18.6325162915029));
#191509=CARTESIAN_POINT('Ctrl Pts',(20.4385403287738,20.4664974408433,18.6321268545737));
#191510=CARTESIAN_POINT('Ctrl Pts',(20.4311012300654,20.4765323118091,18.6313793287589));
#191511=CARTESIAN_POINT('Ctrl Pts',(20.4275268604804,20.4813115322708,18.6310213977949));
#191512=CARTESIAN_POINT('Ctrl Pts',(20.4181787953514,20.4937010709986,18.6300884772442));
#191513=CARTESIAN_POINT('Ctrl Pts',(20.412373760527,20.5012874747701,18.6295122577315));
#191514=CARTESIAN_POINT('Ctrl Pts',(20.3923987975938,20.527029189114,18.6275398506332));
#191515=CARTESIAN_POINT('Ctrl Pts',(20.3779844348143,20.5449919455557,18.6261339782034));
#191516=CARTESIAN_POINT('Ctrl Pts',(20.2515399471054,20.6974008857603,18.6139442887581));
#191517=CARTESIAN_POINT('Ctrl Pts',(20.1235499347325,20.8176869054586,18.6024611893005));
#191518=CARTESIAN_POINT('Ctrl Pts',(19.9117078059211,20.9723414260378,18.5851311314825));
#191519=CARTESIAN_POINT('Ctrl Pts',(19.8380318327756,21.0194343873001,18.579373310981));
#191520=CARTESIAN_POINT('Ctrl Pts',(19.7285100650725,21.0802447153362,18.5713747003021));
#191521=CARTESIAN_POINT('Ctrl Pts',(19.694876561165,21.0977545474171,18.5689900008643));
#191522=CARTESIAN_POINT('Ctrl Pts',(19.6539766352162,21.1176697134146,18.5661906590325));
#191523=CARTESIAN_POINT('Ctrl Pts',(19.6471467563052,21.1209501068958,18.5657265026955));
#191524=CARTESIAN_POINT('Ctrl Pts',(19.6365187160276,21.1259847172551,18.5650095130134));
#191525=CARTESIAN_POINT('Ctrl Pts',(19.6327327985033,21.1277644241518,18.5647551431406));
#191526=CARTESIAN_POINT('Ctrl Pts',(19.6257120429482,21.1310394089649,18.5642853799682));
#191527=CARTESIAN_POINT('Ctrl Pts',(19.622478732703,21.1325377283185,18.5640698041362));
#191528=CARTESIAN_POINT('Ctrl Pts',(19.6151733639526,21.1359006624295,18.563584447185));
#191529=CARTESIAN_POINT('Ctrl Pts',(19.6110991744573,21.1377605187399,18.56331496061));
#191530=CARTESIAN_POINT('Ctrl Pts',(19.5990944870889,21.1431946577611,18.5625243387259));
#191531=CARTESIAN_POINT('Ctrl Pts',(19.5911477153395,21.1467330567638,18.5620053552151));
#191532=CARTESIAN_POINT('Ctrl Pts',(19.5346679266463,21.1714653726992,18.5583462580914));
#191533=CARTESIAN_POINT('Ctrl Pts',(19.4853721754551,21.1908824359157,18.5553060530459));
#191534=CARTESIAN_POINT('Ctrl Pts',(19.432975422838,21.2092814964535,18.5521819430909));
#191535=CARTESIAN_POINT('Ctrl Pts',(19.4305534542855,21.2101270260325,18.5520377726349));
#191536=CARTESIAN_POINT('Ctrl Pts',(19.28888825286,21.2592948382756,18.5436185346475));
#191537=CARTESIAN_POINT('Ctrl Pts',(19.1449736961195,21.2929507341865,18.5358030041243));
#191538=CARTESIAN_POINT('Ctrl Pts',(18.9017575108409,21.3236045397095,18.522332865265));
#191539=CARTESIAN_POINT('Ctrl Pts',(18.8040736013577,21.3290951267861,18.5168602208469));
#191540=CARTESIAN_POINT('Ctrl Pts',(18.6847002070269,21.3275368045576,18.5099105016166));
#191541=CARTESIAN_POINT('Ctrl Pts',(18.6630400081951,21.3269213461122,18.50863931014));
#191542=CARTESIAN_POINT('Ctrl Pts',(18.6323459828862,21.3255773757285,18.5068220743304));
#191543=CARTESIAN_POINT('Ctrl Pts',(18.6233010650617,21.3251231655373,18.5062846177478));
#191544=CARTESIAN_POINT('Ctrl Pts',(18.6077349656487,21.3242413129037,18.5053561970239));
#191545=CARTESIAN_POINT('Ctrl Pts',(18.6012122893559,21.3238414819593,18.5049661102912));
#191546=CARTESIAN_POINT('Ctrl Pts',(18.5887491436962,21.3230195679499,18.5042187088812));
#191547=CARTESIAN_POINT('Ctrl Pts',(18.5828083906047,21.3226026053172,18.5038615587449));
#191548=CARTESIAN_POINT('Ctrl Pts',(18.5674130575754,21.3214567540521,18.5029336683251));
#191549=CARTESIAN_POINT('Ctrl Pts',(18.5579615510795,21.3206894036886,18.502361724281));
#191550=CARTESIAN_POINT('Ctrl Pts',(18.5259969567312,21.3178779622611,18.5004194999191));
#191551=CARTESIAN_POINT('Ctrl Pts',(18.5035121648374,21.3155368396718,18.4990399320636));
#191552=CARTESIAN_POINT('Ctrl Pts',(18.3020367776365,21.2912917518554,18.4865540263959));
#191553=CARTESIAN_POINT('Ctrl Pts',(18.126522023175,21.2469644250179,18.4746992431691));
#191554=CARTESIAN_POINT('Ctrl Pts',(17.8809239452282,21.1503173711543,18.457266167439));
#191555=CARTESIAN_POINT('Ctrl Pts',(17.8049400283445,21.1150850862071,18.4517595274105));
#191556=CARTESIAN_POINT('Ctrl Pts',(17.6986815510754,21.0579356125403,18.4440621110421));
#191557=CARTESIAN_POINT('Ctrl Pts',(17.6665878142559,21.0395751442088,18.441738211702));
#191558=CARTESIAN_POINT('Ctrl Pts',(17.628560205465,21.0164773447493,18.4390005974839));
#191559=CARTESIAN_POINT('Ctrl Pts',(17.6221518897594,21.0125380554962,18.4385398221759));
#191560=CARTESIAN_POINT('Ctrl Pts',(17.612222573122,21.0063611908496,18.4378269185483));
#191561=CARTESIAN_POINT('Ctrl Pts',(17.6086870339041,21.0041472694934,18.4375732810896));
#191562=CARTESIAN_POINT('Ctrl Pts',(17.6021424115697,21.0000221089793,18.4371041920685));
#191563=CARTESIAN_POINT('Ctrl Pts',(17.5991316390303,20.9981137374163,18.4368885622889));
#191564=CARTESIAN_POINT('Ctrl Pts',(17.5923359204867,20.9937821869968,18.4364022263877));
#191565=CARTESIAN_POINT('Ctrl Pts',(17.5885538720852,20.9913545617728,18.4361318200516));
#191566=CARTESIAN_POINT('Ctrl Pts',(17.5774136148093,20.9841536481285,18.4353359899103));
#191567=CARTESIAN_POINT('Ctrl Pts',(17.5700772025157,20.9793465875771,18.4348127605566));
#191568=CARTESIAN_POINT('Ctrl Pts',(17.5172409369551,20.9442552397793,18.43104915654));
#191569=CARTESIAN_POINT('Ctrl Pts',(17.4728950096634,20.9122617776047,18.4279152663074));
#191570=CARTESIAN_POINT('Ctrl Pts',(17.2972524478794,20.7748971618022,18.4153889431912));
#191571=CARTESIAN_POINT('Ctrl Pts',(17.1775040230281,20.6557649172382,18.4065304719811));
#191572=CARTESIAN_POINT('Ctrl Pts',(17.0365796713678,20.4774622475054,18.3939311490437));
#191573=CARTESIAN_POINT('Ctrl Pts',(17.0019842701858,20.4297219305364,18.3906172155171));
#191574=CARTESIAN_POINT('Ctrl Pts',(16.9495311525094,20.3505862367684,18.3851630442936));
#191575=CARTESIAN_POINT('Ctrl Pts',(16.9304053321228,20.3200680350769,18.3830687233733));
#191576=CARTESIAN_POINT('Ctrl Pts',(16.9064660612584,20.2796111120302,18.3802971022042));
#191577=CARTESIAN_POINT('Ctrl Pts',(16.900938149018,20.2701006796203,18.3796459090695));
#191578=CARTESIAN_POINT('Ctrl Pts',(16.8920438950786,20.2545204238581,18.3785794813268));
#191579=CARTESIAN_POINT('Ctrl Pts',(16.8886327968082,20.2484762894096,18.3781658675899));
#191580=CARTESIAN_POINT('Ctrl Pts',(16.8821134589856,20.2367907801168,18.3773663281304));
#191581=CARTESIAN_POINT('Ctrl Pts',(16.8790011194907,20.2311517716744,18.3769805552877));
#191582=CARTESIAN_POINT('Ctrl Pts',(16.8719106759571,20.218165407329,18.3760922253791));
#191583=CARTESIAN_POINT('Ctrl Pts',(16.8679502574876,20.2108085635652,18.3755890447085));
#191584=CARTESIAN_POINT('Ctrl Pts',(16.8574949080592,20.19110825083,18.3742416889693));
#191585=CARTESIAN_POINT('Ctrl Pts',(16.8510783244572,20.1787238720736,18.3733947618489));
#191586=CARTESIAN_POINT('Ctrl Pts',(16.8071710292921,20.0918900903104,18.3674560690453));
#191587=CARTESIAN_POINT('Ctrl Pts',(16.773994207962,20.0153674650894,18.3622160460457));
#191588=CARTESIAN_POINT('Ctrl Pts',(16.7454193519082,19.9371101886317,18.3568545479166));
#191589=CARTESIAN_POINT('',(16.6170000449378,19.2114361958265,18.8870727828678));
#191590=CARTESIAN_POINT('Ctrl Pts',(16.7454193782244,19.9371102607032,18.1318062886951));
#191591=CARTESIAN_POINT('Ctrl Pts',(16.7665449537571,19.9949663638349,18.1356559052053));
#191592=CARTESIAN_POINT('Ctrl Pts',(16.7901879214744,20.0518800190739,18.139584314016));
#191593=CARTESIAN_POINT('Ctrl Pts',(16.8711047761691,20.2249340166287,18.15195208795));
#191594=CARTESIAN_POINT('Ctrl Pts',(16.9365617184093,20.336900875137,18.1605860036748));
#191595=CARTESIAN_POINT('Ctrl Pts',(17.0275714615357,20.4642053831557,18.1708506020951));
#191596=CARTESIAN_POINT('Ctrl Pts',(17.0437392986115,20.4859278119496,18.1726183621046));
#191597=CARTESIAN_POINT('Ctrl Pts',(17.095497683323,20.5527523667523,18.1780952033794));
#191598=CARTESIAN_POINT('Ctrl Pts',(17.1325132652244,20.5967239096791,18.1817560584367));
#191599=CARTESIAN_POINT('Ctrl Pts',(17.1772633068432,20.6456911367769,18.185849319262));
#191600=CARTESIAN_POINT('Ctrl Pts',(17.1832926155107,20.6522058852875,18.1863942407597));
#191601=CARTESIAN_POINT('Ctrl Pts',(17.1924515228629,20.6619781849337,18.18721189061));
#191602=CARTESIAN_POINT('Ctrl Pts',(17.1955507761671,20.6652638643242,18.1874868475182));
#191603=CARTESIAN_POINT('Ctrl Pts',(17.2011159217117,20.6711260633838,18.18797745277));
#191604=CARTESIAN_POINT('Ctrl Pts',(17.2035778220657,20.6737062850552,18.1881934007897));
#191605=CARTESIAN_POINT('Ctrl Pts',(17.2089219372367,20.679278980206,18.1886598162157));
#191606=CARTESIAN_POINT('Ctrl Pts',(17.2118064353551,20.6822691846401,18.1889101017006));
#191607=CARTESIAN_POINT('Ctrl Pts',(17.2198843538614,20.6905939437266,18.1896070094328));
#191608=CARTESIAN_POINT('Ctrl Pts',(17.2250971983932,20.6959096831909,18.1900521442742));
#191609=CARTESIAN_POINT('Ctrl Pts',(17.255454605516,20.726541371441,18.1926187489927));
#191610=CARTESIAN_POINT('Ctrl Pts',(17.281209555976,20.7512475116724,18.194695001097));
#191611=CARTESIAN_POINT('Ctrl Pts',(17.3658493623777,20.828427487669,18.2012494845455));
#191612=CARTESIAN_POINT('Ctrl Pts',(17.427048535344,20.8782695198108,18.2055906619453));
#191613=CARTESIAN_POINT('Ctrl Pts',(17.5646212964521,20.9780709037051,18.2148598840472));
#191614=CARTESIAN_POINT('Ctrl Pts',(17.6417263091053,21.026743426643,18.2197669245028));
#191615=CARTESIAN_POINT('Ctrl Pts',(17.8150509427724,21.1211080523016,18.2306130365245));
#191616=CARTESIAN_POINT('Ctrl Pts',(17.9120569164847,21.164813054697,18.2365759953428));
#191617=CARTESIAN_POINT('Ctrl Pts',(18.0251851485167,21.2058607629054,18.2436279209302));
#191618=CARTESIAN_POINT('Ctrl Pts',(18.0384920188413,21.2105390946066,18.2444587012989));
#191619=CARTESIAN_POINT('Ctrl Pts',(18.0597973702612,21.2177910682802,18.2457913157012));
#191620=CARTESIAN_POINT('Ctrl Pts',(18.0677662835199,21.2204507233563,18.2462903043328));
#191621=CARTESIAN_POINT('Ctrl Pts',(18.0818792508801,21.2250678010382,18.2471750640675));
#191622=CARTESIAN_POINT('Ctrl Pts',(18.0880168470452,21.2270447275024,18.2475601867311));
#191623=CARTESIAN_POINT('Ctrl Pts',(18.1007601273753,21.2310851854218,18.2483605671249));
#191624=CARTESIAN_POINT('Ctrl Pts',(18.1073670820502,21.2331444253601,18.2487759605331));
#191625=CARTESIAN_POINT('Ctrl Pts',(18.1244158141738,21.2383665564719,18.2498489969937));
#191626=CARTESIAN_POINT('Ctrl Pts',(18.1348720626799,21.2414811601326,18.250508211446));
#191627=CARTESIAN_POINT('Ctrl Pts',(18.1791643279064,21.2543025884172,18.2533055846432));
#191628=CARTESIAN_POINT('Ctrl Pts',(18.2132140304609,21.2632450709468,18.2554684022502));
#191629=CARTESIAN_POINT('Ctrl Pts',(18.3030415831973,21.2844570968317,18.2612097600631));
#191630=CARTESIAN_POINT('Ctrl Pts',(18.3591177588786,21.2953252835938,18.2648299836604));
#191631=CARTESIAN_POINT('Ctrl Pts',(18.5659272519748,21.3267915790369,18.2782974683967));
#191632=CARTESIAN_POINT('Ctrl Pts',(18.718316899986,21.3333971617287,18.2884831801166));
#191633=CARTESIAN_POINT('Ctrl Pts',(18.8925927867251,21.3221718057037,18.2998897881684));
#191634=CARTESIAN_POINT('Ctrl Pts',(18.9150845518902,21.3203616334931,18.3013563073899));
#191635=CARTESIAN_POINT('Ctrl Pts',(18.9886351993013,21.3132570303254,18.3061255942552));
#191636=CARTESIAN_POINT('Ctrl Pts',(19.0395351343045,21.3064648466792,18.3093846065088));
#191637=CARTESIAN_POINT('Ctrl Pts',(19.0979042913866,21.296503458526,18.3130367114465));
#191638=CARTESIAN_POINT('Ctrl Pts',(19.1056593158684,21.2951354001472,18.3135201822506));
#191639=CARTESIAN_POINT('Ctrl Pts',(19.1180124292984,21.2928850523483,18.3142873155793));
#191640=CARTESIAN_POINT('Ctrl Pts',(19.1226154509021,21.2920307420452,18.3145725003787));
#191641=CARTESIAN_POINT('Ctrl Pts',(19.1307460429651,21.2904938053331,18.3150750176731));
#191642=CARTESIAN_POINT('Ctrl Pts',(19.134274757541,21.2898174590978,18.315292703696));
#191643=CARTESIAN_POINT('Ctrl Pts',(19.1417317873122,21.2883684838018,18.3157518476623));
#191644=CARTESIAN_POINT('Ctrl Pts',(19.14565963046,21.2875936957285,18.3159931809005));
#191645=CARTESIAN_POINT('Ctrl Pts',(19.1562137238959,21.2854807226222,18.3166403226643));
#191646=CARTESIAN_POINT('Ctrl Pts',(19.1628358662414,21.2841219211182,18.3170449704413));
#191647=CARTESIAN_POINT('Ctrl Pts',(19.195151363831,21.2773296161408,18.3190132744816));
#191648=CARTESIAN_POINT('Ctrl Pts',(19.2207498426422,21.2714498044258,18.3205528397991));
#191649=CARTESIAN_POINT('Ctrl Pts',(19.2937720852216,21.2532401077807,18.3249053749511));
#191650=CARTESIAN_POINT('Ctrl Pts',(19.3408879592056,21.2397378051114,18.3276660300718));
#191651=CARTESIAN_POINT('Ctrl Pts',(19.4793729662792,21.1947940102237,18.3357496452728));
#191652=CARTESIAN_POINT('Ctrl Pts',(19.5691050828594,21.1587218701743,18.3409511662204));
#191653=CARTESIAN_POINT('Ctrl Pts',(19.7830122397995,21.0552211243247,18.3538817866873));
#191654=CARTESIAN_POINT('Ctrl Pts',(19.9034877900003,20.9812737111969,18.3616606841721));
#191655=CARTESIAN_POINT('Ctrl Pts',(20.0270785078051,20.8872580288922,18.3707579161789));
#191656=CARTESIAN_POINT('Ctrl Pts',(20.0383583019562,20.8784958506703,18.3715990288217));
#191657=CARTESIAN_POINT('Ctrl Pts',(20.0561708874211,20.86436765215,18.3729450942776));
#191658=CARTESIAN_POINT('Ctrl Pts',(20.0627618151563,20.8590753878817,18.3734471094479));
#191659=CARTESIAN_POINT('Ctrl Pts',(20.0743309016171,20.8496713400315,18.3743353873944));
#191660=CARTESIAN_POINT('Ctrl Pts',(20.0793223030421,20.8455759651918,18.3747209847905));
#191661=CARTESIAN_POINT('Ctrl Pts',(20.0896082653568,20.8370574488203,18.3755205321053));
#191662=CARTESIAN_POINT('Ctrl Pts',(20.0949000892878,20.8326311359836,18.3759346087247));
#191663=CARTESIAN_POINT('Ctrl Pts',(20.1084298949,20.8212013465263,18.3770003949));
#191664=CARTESIAN_POINT('Ctrl Pts',(20.116635952907,20.814160543204,18.3776536354871));
#191665=CARTESIAN_POINT('Ctrl Pts',(20.1506772402487,20.784497322077,18.3803924556932));
#191666=CARTESIAN_POINT('Ctrl Pts',(20.1760128535243,20.7613118844096,18.3825014255533));
#191667=CARTESIAN_POINT('Ctrl Pts',(20.2405626244418,20.6992886434286,18.3880658515075));
#191668=CARTESIAN_POINT('Ctrl Pts',(20.2788399216034,20.6595174558916,18.3915598646953));
#191669=CARTESIAN_POINT('Ctrl Pts',(20.3882818318116,20.536527037678,18.4021427062645));
#191670=CARTESIAN_POINT('Ctrl Pts',(20.4545894559892,20.4492401893505,18.4093798808806));
#191671=CARTESIAN_POINT('Ctrl Pts',(20.5426730035151,20.3124651811051,18.4201261952941));
#191672=CARTESIAN_POINT('Ctrl Pts',(20.5698016848622,20.2666306595719,18.4236353136285));
#191673=CARTESIAN_POINT('Ctrl Pts',(20.6009789285807,20.2091117480658,18.4278934234894));
#191674=CARTESIAN_POINT('Ctrl Pts',(20.6066912146194,20.198352522856,18.4286838262523));
#191675=CARTESIAN_POINT('Ctrl Pts',(20.637139710341,20.13978711272,18.432951190868));
#191676=CARTESIAN_POINT('Ctrl Pts',(20.6601409685388,20.0910956134165,18.4363738886176));
#191677=CARTESIAN_POINT('Ctrl Pts',(20.6846909389624,20.0335388798155,18.4402340422234));
#191678=CARTESIAN_POINT('Ctrl Pts',(20.6880693495739,20.0254804056937,18.4407703510372));
#191679=CARTESIAN_POINT('Ctrl Pts',(20.6931070014911,20.0132523852791,18.4415776351982));
#191680=CARTESIAN_POINT('Ctrl Pts',(20.6948029916941,20.0090982155089,18.4418507576983));
#191681=CARTESIAN_POINT('Ctrl Pts',(20.6978224474137,20.001634617435,18.4423393931503));
#191682=CARTESIAN_POINT('Ctrl Pts',(20.6991507687937,19.9983272253324,18.4425551955531));
#191683=CARTESIAN_POINT('Ctrl Pts',(20.7020176287673,19.9911365642681,18.443022787671));
#191684=CARTESIAN_POINT('Ctrl Pts',(20.7035530247087,19.9872521044091,18.4432743874316));
#191685=CARTESIAN_POINT('Ctrl Pts',(20.7078303174843,19.9763364181887,18.4439786765076));
#191686=CARTESIAN_POINT('Ctrl Pts',(20.7105461590321,19.9692949560225,18.4444298269297));
#191687=CARTESIAN_POINT('Ctrl Pts',(20.7264927428894,19.9272818726399,18.4471036398129));
#191688=CARTESIAN_POINT('Ctrl Pts',(20.7388336321318,19.8919769054545,18.4492765532668));
#191689=CARTESIAN_POINT('Ctrl Pts',(20.7762416755458,19.7751069186339,18.456285751501));
#191690=CARTESIAN_POINT('Ctrl Pts',(20.7973162790691,19.6923480108486,18.4609621616113));
#191691=CARTESIAN_POINT('Ctrl Pts',(20.8467478729529,19.433793505942,18.4752908852577));
#191692=CARTESIAN_POINT('Ctrl Pts',(20.8579935547105,19.255556975611,18.4848437177853));
#191693=CARTESIAN_POINT('Ctrl Pts',(20.8453865527207,19.0552567752956,18.4965080512658));
#191694=CARTESIAN_POINT('Ctrl Pts',(20.8435862765752,19.0325208436504,18.497844335318));
#191695=CARTESIAN_POINT('Ctrl Pts',(20.8405147972411,19.0003463530487,18.4997544878449));
#191696=CARTESIAN_POINT('Ctrl Pts',(20.8395466552243,18.9908799687692,18.5003188428228));
#191697=CARTESIAN_POINT('Ctrl Pts',(20.8378682528908,18.9754943476607,18.5012400251024));
#191698=CARTESIAN_POINT('Ctrl Pts',(20.8371967456192,18.9695709505824,18.5015956279512));
#191699=CARTESIAN_POINT('Ctrl Pts',(20.8357373280767,18.9571657267569,18.5023423866502));
#191700=CARTESIAN_POINT('Ctrl Pts',(20.8349444316096,18.9506845599857,18.5027336962554));
#191701=CARTESIAN_POINT('Ctrl Pts',(20.8329839852107,18.935252449023,18.5036682472012));
#191702=CARTESIAN_POINT('Ctrl Pts',(20.8317891513394,18.9263051552649,18.5042123452468));
#191703=CARTESIAN_POINT('Ctrl Pts',(20.8275561403065,18.8960816070693,18.5060580797892));
#191704=CARTESIAN_POINT('Ctrl Pts',(20.8242512778151,18.8748446059281,18.5073681118313));
#191705=CARTESIAN_POINT('Ctrl Pts',(20.7903457929804,18.6768583042241,18.5197078120399));
#191706=CARTESIAN_POINT('Ctrl Pts',(20.73772467273,18.5046519942206,18.5314807501534));
#191707=CARTESIAN_POINT('Ctrl Pts',(20.6145053173395,18.2312396779801,18.5512939042678));
#191708=CARTESIAN_POINT('Ctrl Pts',(20.5556497141551,18.1257214266051,18.5592315852164));
#191709=CARTESIAN_POINT('Ctrl Pts',(20.4828072967564,18.0179148619257,18.5672674139715));
#191710=CARTESIAN_POINT('Ctrl Pts',(20.477439876999,18.010085135871,18.5678505137086));
#191711=CARTESIAN_POINT('Ctrl Pts',(20.4694049094193,17.9985315358726,18.5687098421683));
#191712=CARTESIAN_POINT('Ctrl Pts',(20.4667777354081,17.9947799143557,18.5689887053815));
#191713=CARTESIAN_POINT('Ctrl Pts',(20.4620801068341,17.9881177891895,18.5694835579186));
#191714=CARTESIAN_POINT('Ctrl Pts',(20.4600144454931,17.9852039762845,18.5696998686232));
#191715=CARTESIAN_POINT('Ctrl Pts',(20.4555555970028,17.9789479624314,18.5701640189079));
#191716=CARTESIAN_POINT('Ctrl Pts',(20.4531600542267,17.9756075095498,18.5704116927634));
#191717=CARTESIAN_POINT('Ctrl Pts',(20.4465162232933,17.9663998004366,18.5710939992904));
#191718=CARTESIAN_POINT('Ctrl Pts',(20.4422474813891,17.9605472749548,18.5715272440639));
#191719=CARTESIAN_POINT('Ctrl Pts',(20.4186218522516,17.9285028628964,18.573897678806));
#191720=CARTESIAN_POINT('Ctrl Pts',(20.3986914371649,17.9027368867428,18.575797351968));
#191721=CARTESIAN_POINT('Ctrl Pts',(20.2757125870309,17.7511138193147,18.5870061519822));
#191722=CARTESIAN_POINT('Ctrl Pts',(20.1590242846884,17.6370041360469,18.5956034784095));
#191723=CARTESIAN_POINT('Ctrl Pts',(19.9380209488694,17.4658126054789,18.6109075402293));
#191724=CARTESIAN_POINT('Ctrl Pts',(19.8398805650126,17.4020311229246,18.6174314177453));
#191725=CARTESIAN_POINT('Ctrl Pts',(19.7244191993803,17.3399140882788,18.6251124701548));
#191726=CARTESIAN_POINT('Ctrl Pts',(19.7117831477673,17.3332798982191,18.625952917221));
#191727=CARTESIAN_POINT('Ctrl Pts',(19.6915608505614,17.3229222447065,18.6272981165492));
#191728=CARTESIAN_POINT('Ctrl Pts',(19.6840175829805,17.3191154946899,18.6277999371518));
#191729=CARTESIAN_POINT('Ctrl Pts',(19.6706708857595,17.3124799629136,18.6286879885203));
#191730=CARTESIAN_POINT('Ctrl Pts',(19.6648768938411,17.3096323641821,18.6290735549969));
#191731=CARTESIAN_POINT('Ctrl Pts',(19.6528633353563,17.3037960818025,18.6298731538759));
#191732=CARTESIAN_POINT('Ctrl Pts',(19.6466420073641,17.3008112189391,18.6302873135494));
#191733=CARTESIAN_POINT('Ctrl Pts',(19.6306292815823,17.2932247323674,18.6313535573939));
#191734=CARTESIAN_POINT('Ctrl Pts',(19.6208170900383,17.2886676958066,18.6320071751333));
#191735=CARTESIAN_POINT('Ctrl Pts',(19.5796667597815,17.2699385242901,18.6347496561466));
#191736=CARTESIAN_POINT('Ctrl Pts',(19.5480219742388,17.2564565933254,18.6368619879219));
#191737=CARTESIAN_POINT('Ctrl Pts',(19.4646753299354,17.2233227787322,18.6424374044971));
#191738=CARTESIAN_POINT('Ctrl Pts',(19.4125095371365,17.2049164641964,18.6459392365308));
#191739=CARTESIAN_POINT('Ctrl Pts',(19.2550228870426,17.1561941485145,18.6565370893406));
#191740=CARTESIAN_POINT('Ctrl Pts',(19.1480107101045,17.1319897530977,18.6637814049215));
#191741=CARTESIAN_POINT('Ctrl Pts',(18.9810768829046,17.107635602741,18.6749249270913));
#191742=CARTESIAN_POINT('Ctrl Pts',(18.9222032790448,17.1015524895205,18.6788228337887));
#191743=CARTESIAN_POINT('Ctrl Pts',(18.8037935472515,17.094315268071,18.6865187755934));
#191744=CARTESIAN_POINT('Ctrl Pts',(18.744304140804,17.09318966923,18.6903128167868));
#191745=CARTESIAN_POINT('Ctrl Pts',(18.6758959977996,17.094778607705,18.6945356910558));
#191746=CARTESIAN_POINT('Ctrl Pts',(18.666952217849,17.0950430870013,18.6950850283632));
#191747=CARTESIAN_POINT('Ctrl Pts',(18.6534812830421,17.0955269385285,18.6959079869443));
#191748=CARTESIAN_POINT('Ctrl Pts',(18.6489528466993,17.0957041530343,18.6961838790378));
#191749=CARTESIAN_POINT('Ctrl Pts',(18.640860676204,17.0960468578927,18.6966754947986));
#191750=CARTESIAN_POINT('Ctrl Pts',(18.6372967698725,17.0962068155843,18.6968915233459));
#191751=CARTESIAN_POINT('Ctrl Pts',(18.6295941199418,17.0965720436191,18.6973573676377));
#191752=CARTESIAN_POINT('Ctrl Pts',(18.6254555824869,17.0967804559084,18.697607005447));
#191753=CARTESIAN_POINT('Ctrl Pts',(18.6139331641101,17.0973946346634,18.6983002841973));
#191754=CARTESIAN_POINT('Ctrl Pts',(18.6065506746623,17.0978269454219,18.6987424627533));
#191755=CARTESIAN_POINT('Ctrl Pts',(18.5643658561525,17.1005191181522,18.7012584247532));
#191756=CARTESIAN_POINT('Ctrl Pts',(18.529619128739,17.1036001629456,18.7032890514265));
#191757=CARTESIAN_POINT('Ctrl Pts',(18.4195022309583,17.1161138704015,18.7096361156139));
#191758=CARTESIAN_POINT('Ctrl Pts',(18.3445522496515,17.1287442579842,18.7138253050929));
#191759=CARTESIAN_POINT('Ctrl Pts',(18.1744392097267,17.1669205804375,18.7233438065338));
#191760=CARTESIAN_POINT('Ctrl Pts',(18.0800600090312,17.1951301249886,18.7286362770021));
#191761=CARTESIAN_POINT('Ctrl Pts',(17.8917257986939,17.2660468443853,18.7397119167156));
#191762=CARTESIAN_POINT('Ctrl Pts',(17.7982479124415,17.3092553546494,18.7454933415189));
#191763=CARTESIAN_POINT('Ctrl Pts',(17.6949024064275,17.3664948393134,18.7524163990381));
#191764=CARTESIAN_POINT('Ctrl Pts',(17.6815990441225,17.374052720817,18.7533180106836));
#191765=CARTESIAN_POINT('Ctrl Pts',(17.6614319006682,17.3858010209012,18.7547013154574));
#191766=CARTESIAN_POINT('Ctrl Pts',(17.6545079581591,17.3898875460632,18.755179249551));
#191767=CARTESIAN_POINT('Ctrl Pts',(17.6422722633395,17.3972033768201,18.7560292580482));
#191768=CARTESIAN_POINT('Ctrl Pts',(17.6369511133171,17.4004168397428,18.75640075079));
#191769=CARTESIAN_POINT('Ctrl Pts',(17.6256915133991,17.4072844138341,18.7571907726096));
#191770=CARTESIAN_POINT('Ctrl Pts',(17.6197568199446,17.4109445144278,18.7576095189449));
#191771=CARTESIAN_POINT('Ctrl Pts',(17.6076380683345,17.4185014015234,18.7584694650207));
#191772=CARTESIAN_POINT('Ctrl Pts',(17.6014558993608,17.4224010274365,18.7589107661908));
#191773=CARTESIAN_POINT('Ctrl Pts',(17.5861792008668,17.432148314861,18.7600078201595));
#191774=CARTESIAN_POINT('Ctrl Pts',(17.5771091164892,17.4380337336869,18.760664972019));
#191775=CARTESIAN_POINT('Ctrl Pts',(17.4618289665899,17.5140982533416,18.7690926509832));
#191776=CARTESIAN_POINT('Ctrl Pts',(17.3621323002869,17.5936368096121,18.7772270133833));
#191777=CARTESIAN_POINT('Ctrl Pts',(17.1693316058984,17.7781723023871,18.7947151941702));
#191778=CARTESIAN_POINT('Ctrl Pts',(17.0782666057596,17.8844519064824,18.8040697644315));
#191779=CARTESIAN_POINT('Ctrl Pts',(16.9730966445309,18.0350534162858,18.8158636918841));
#191780=CARTESIAN_POINT('Ctrl Pts',(16.9489979196492,18.0719656773321,18.8186490011286));
#191781=CARTESIAN_POINT('Ctrl Pts',(16.9221428448272,18.1160481514842,18.8218304611239));
#191782=CARTESIAN_POINT('Ctrl Pts',(16.9182527490838,18.1225112191654,18.8222933463612));
#191783=CARTESIAN_POINT('Ctrl Pts',(16.9120541681013,18.1329353445121,18.8230340459933));
#191784=CARTESIAN_POINT('Ctrl Pts',(16.9097238995672,18.1368832809758,18.8233132260267));
#191785=CARTESIAN_POINT('Ctrl Pts',(16.905596592062,18.1439279329991,18.8238089559392));
#191786=CARTESIAN_POINT('Ctrl Pts',(16.9037945655925,18.1470216699099,18.8240258268366));
#191787=CARTESIAN_POINT('Ctrl Pts',(16.8999660993169,18.1536329257218,18.8244874865521));
#191788=CARTESIAN_POINT('Ctrl Pts',(16.8979419308249,18.1571516969334,18.8247321289133));
#191789=CARTESIAN_POINT('Ctrl Pts',(16.89244908921,18.1667641993224,18.8253975816574));
#191790=CARTESIAN_POINT('Ctrl Pts',(16.8890005134409,18.1728694387596,18.8258171151877));
#191791=CARTESIAN_POINT('Ctrl Pts',(16.8712703330513,18.2046257557163,18.8279837742874));
#191792=CARTESIAN_POINT('Ctrl Pts',(16.8574923532728,18.2305561313607,18.8297005802777));
#191793=CARTESIAN_POINT('Ctrl Pts',(16.8181649353578,18.3084392362931,18.8347281266977));
#191794=CARTESIAN_POINT('Ctrl Pts',(16.7942008718324,18.3611645926916,18.837965108499));
#191795=CARTESIAN_POINT('Ctrl Pts',(16.6940055028755,18.6080157288271,18.8526529722907));
#191796=CARTESIAN_POINT('Ctrl Pts',(16.6445611156937,18.8117328808028,18.8636104206104));
#191797=CARTESIAN_POINT('Ctrl Pts',(16.6232302280078,19.046446771021,18.8772499189784));
#191798=CARTESIAN_POINT('Ctrl Pts',(16.621292764556,19.0735415207636,18.8788369296319));
#191799=CARTESIAN_POINT('Ctrl Pts',(16.6193445967681,19.110870313191,18.8810434756792));
#191800=CARTESIAN_POINT('Ctrl Pts',(16.6188859028633,19.1210790394894,18.8816489840458));
#191801=CARTESIAN_POINT('Ctrl Pts',(16.618271724327,19.1373794158982,18.8826192367807));
#191802=CARTESIAN_POINT('Ctrl Pts',(16.6180685938414,19.1434691912992,18.8829824843594));
#191803=CARTESIAN_POINT('Ctrl Pts',(16.6177137006869,19.1556923160984,18.8837131460156));
#191804=CARTESIAN_POINT('Ctrl Pts',(16.6175623044106,19.161825616239,18.8840805679802));
#191805=CARTESIAN_POINT('Ctrl Pts',(16.6172825438745,19.1755831188097,18.8849065375177));
#191806=CARTESIAN_POINT('Ctrl Pts',(16.6171687078969,19.1832075021295,18.885365536024));
#191807=CARTESIAN_POINT('Ctrl Pts',(16.6170306367634,19.1977001167314,18.8862404348957));
#191808=CARTESIAN_POINT('Ctrl Pts',(16.6169986298215,19.2045681769785,18.8866560843466));
#191809=CARTESIAN_POINT('Ctrl Pts',(16.6170000449378,19.2114361958265,18.8870727828678));
#191810=CARTESIAN_POINT('Ctrl Pts',(16.6170000447709,19.2114353848898,18.8870727336665));
#191811=CARTESIAN_POINT('Ctrl Pts',(16.6170021622649,19.2217314122616,18.8876974172358));
#191812=CARTESIAN_POINT('Ctrl Pts',(16.6170793917548,19.2320271783322,18.8883244488401));
#191813=CARTESIAN_POINT('Ctrl Pts',(16.61753901209,19.2630888551937,18.8902234410339));
#191814=CARTESIAN_POINT('Ctrl Pts',(16.6181518837126,19.2838495921527,18.8915025022528));
#191815=CARTESIAN_POINT('Ctrl Pts',(16.6269496222173,19.4826435974031,18.9038465954591));
#191816=CARTESIAN_POINT('Ctrl Pts',(16.6572801772349,19.658954821958,18.9156267936816));
#191817=CARTESIAN_POINT('Ctrl Pts',(16.7203860615788,19.8655869711512,18.9298814848752));
#191818=CARTESIAN_POINT('Ctrl Pts',(16.7324248545875,19.9015224718576,18.9323739729723));
#191819=CARTESIAN_POINT('Ctrl Pts',(16.7454193714968,19.9371102422787,18.9348454715054));
#191820=CARTESIAN_POINT('Origin',(18.734,19.211,0.));
#191821=CARTESIAN_POINT('',(16.7454193617555,19.9371102156003,19.9537492222746));
#191822=CARTESIAN_POINT('',(16.7454193946088,19.9371103055747,19.7345260524097));
#191823=CARTESIAN_POINT('',(16.7454193623258,19.9371102171621,0.));
#191824=CARTESIAN_POINT('',(16.620085879662,19.211828459305,19.9109956432659));
#191825=CARTESIAN_POINT('Ctrl Pts',(16.7454193617555,19.9371102156003,19.9537492222746));
#191826=CARTESIAN_POINT('Ctrl Pts',(16.7274346612152,19.8878559474318,19.9507625090015));
#191827=CARTESIAN_POINT('Ctrl Pts',(16.711283767598,19.8379440837176,19.9478475408055));
#191828=CARTESIAN_POINT('Ctrl Pts',(16.6439835662993,19.6001371164755,19.9342646372123));
#191829=CARTESIAN_POINT('Ctrl Pts',(16.6170670033202,19.4064030010435,19.9239833213256));
#191830=CARTESIAN_POINT('Ctrl Pts',(16.617000124922,19.2117272686678,19.9127739632071));
#191831=CARTESIAN_POINT('Ctrl Pts',(16.7477767826476,19.936270776259,19.1554367658253));
#191832=CARTESIAN_POINT('Ctrl Pts',(16.835152879605,20.1806248752966,19.1710019282197));
#191833=CARTESIAN_POINT('Ctrl Pts',(17.3199689711641,21.0303283365173,19.2289590261745));
#191834=CARTESIAN_POINT('Ctrl Pts',(19.0938031815268,21.6882711475642,19.3293080596899));
#191835=CARTESIAN_POINT('Ctrl Pts',(21.0117476411797,20.2493623677241,19.4564838663713));
#191836=CARTESIAN_POINT('Ctrl Pts',(20.8400000149027,17.8578205193086,19.5836596730528));
#191837=CARTESIAN_POINT('Ctrl Pts',(18.7361280844105,16.7077369418621,19.7108354797341));
#191838=CARTESIAN_POINT('Ctrl Pts',(16.9296977525301,17.6912382419271,19.8199301623757));
#191839=CARTESIAN_POINT('Ctrl Pts',(16.6216054888487,18.8061996502611,19.8866329094569));
#191840=CARTESIAN_POINT('Ctrl Pts',(16.620175975625,19.2118314138068,19.9109437209775));
#191841=CARTESIAN_POINT('Ctrl Pts',(16.7454193714968,19.9371102422787,18.9348454715054));
#191842=CARTESIAN_POINT('Ctrl Pts',(16.7585801455699,19.9731533371889,18.9373485914015));
#191843=CARTESIAN_POINT('Ctrl Pts',(16.7727212540933,20.008839748599,18.9398301656811));
#191844=CARTESIAN_POINT('Ctrl Pts',(16.8015898582272,20.0762761626567,18.9445019017568));
#191845=CARTESIAN_POINT('Ctrl Pts',(16.8161467769515,20.1080792261891,18.9466972924739));
#191846=CARTESIAN_POINT('Ctrl Pts',(16.8347318678157,20.146160058031,18.9493038779225));
#191847=CARTESIAN_POINT('Ctrl Pts',(16.8380127503703,20.1527940990628,18.9497571382522));
#191848=CARTESIAN_POINT('Ctrl Pts',(16.8431853658365,20.1631166947162,18.9504609528935));
#191849=CARTESIAN_POINT('Ctrl Pts',(16.8450532193502,20.1668170545023,18.9507129562211));
#191850=CARTESIAN_POINT('Ctrl Pts',(16.848548828532,20.1736918542105,18.9511805641631));
#191851=CARTESIAN_POINT('Ctrl Pts',(16.8501737235963,20.1768676341751,18.9513963373115));
#191852=CARTESIAN_POINT('Ctrl Pts',(16.8538802699165,20.1840669668173,18.9518849621267));
#191853=CARTESIAN_POINT('Ctrl Pts',(16.8559668079206,20.1880879447033,18.9521575018739));
#191854=CARTESIAN_POINT('Ctrl Pts',(16.8622089495612,20.2000233411172,18.952965474331));
#191855=CARTESIAN_POINT('Ctrl Pts',(16.8664018512445,20.2079182849687,18.953498611539));
#191856=CARTESIAN_POINT('Ctrl Pts',(16.8987523988646,20.2679116849539,18.9575416544899));
#191857=CARTESIAN_POINT('Ctrl Pts',(16.9290377073851,20.3188395825676,18.960926348901));
#191858=CARTESIAN_POINT('Ctrl Pts',(17.0709023836289,20.5361012589682,18.9754504885729));
#191859=CARTESIAN_POINT('Ctrl Pts',(17.2036165909359,20.6873886003564,18.9858918624293));
#191860=CARTESIAN_POINT('Ctrl Pts',(17.3974419635339,20.8536618643551,19.0003465948215));
#191861=CARTESIAN_POINT('Ctrl Pts',(17.440646787567,20.8878906016631,19.0035195065488));
#191862=CARTESIAN_POINT('Ctrl Pts',(17.4925426493952,20.9258051810881,19.0072998698884));
#191863=CARTESIAN_POINT('Ctrl Pts',(17.4999853085875,20.9311688579501,19.0078412982107));
#191864=CARTESIAN_POINT('Ctrl Pts',(17.5142302202002,20.9412946654857,19.0088763111339));
#191865=CARTESIAN_POINT('Ctrl Pts',(17.5210261011059,20.9460654923446,19.0093695513505));
#191866=CARTESIAN_POINT('Ctrl Pts',(17.533045020102,20.9543978601523,19.0102410150682));
#191867=CARTESIAN_POINT('Ctrl Pts',(17.5382563028456,20.9579762367882,19.0106185907259));
#191868=CARTESIAN_POINT('Ctrl Pts',(17.5485073269588,20.9649478426138,19.0113607979005));
#191869=CARTESIAN_POINT('Ctrl Pts',(17.5535458058536,20.9683428256232,19.0117253579882));
#191870=CARTESIAN_POINT('Ctrl Pts',(17.5656263519771,20.9764074358049,19.0125989070148));
#191871=CARTESIAN_POINT('Ctrl Pts',(17.5726818581997,20.981056656177,19.0131086570988));
#191872=CARTESIAN_POINT('Ctrl Pts',(17.5982467684564,20.997683986732,19.0149542436543));
#191873=CARTESIAN_POINT('Ctrl Pts',(17.6169146811909,21.0094146919493,19.0162992320329));
#191874=CARTESIAN_POINT('Ctrl Pts',(17.7949162185152,21.1174280242474,19.0291029593766));
#191875=CARTESIAN_POINT('Ctrl Pts',(17.9660863529535,21.1925718334782,19.0413666858505));
#191876=CARTESIAN_POINT('Ctrl Pts',(18.2214554473875,21.2665662278038,19.0589192011326));
#191877=CARTESIAN_POINT('Ctrl Pts',(18.2992863674331,21.2844223395579,19.0641603309251));
#191878=CARTESIAN_POINT('Ctrl Pts',(18.4133637890882,21.3038861651082,19.0715367863243));
#191879=CARTESIAN_POINT('Ctrl Pts',(18.4489341675892,21.3090271462841,19.0737941187758));
#191880=CARTESIAN_POINT('Ctrl Pts',(18.4920288750255,21.3141392324147,19.0764639576536));
#191881=CARTESIAN_POINT('Ctrl Pts',(18.4994419650273,21.3149788944479,19.076920904734));
#191882=CARTESIAN_POINT('Ctrl Pts',(18.5109934642135,21.3162254924305,19.0776291794747));
#191883=CARTESIAN_POINT('Ctrl Pts',(18.5151288104673,21.3166594435146,19.0778819855174));
#191884=CARTESIAN_POINT('Ctrl Pts',(18.5228130357383,21.317442921688,19.0783503168764));
#191885=CARTESIAN_POINT('Ctrl Pts',(18.5263614855395,21.3177956625623,19.0785660154931));
#191886=CARTESIAN_POINT('Ctrl Pts',(18.5344020118421,21.3185744358125,19.0790534972824));
#191887=CARTESIAN_POINT('Ctrl Pts',(18.5388945577166,21.318995072723,19.0793249745745));
#191888=CARTESIAN_POINT('Ctrl Pts',(18.5522075302532,21.3201986415674,19.0801268892954));
#191889=CARTESIAN_POINT('Ctrl Pts',(18.5610316884447,21.3209406107836,19.0806550819175));
#191890=CARTESIAN_POINT('Ctrl Pts',(18.6265559244888,21.3260363097504,19.084554172067));
#191891=CARTESIAN_POINT('Ctrl Pts',(18.6834115366662,21.3281596160968,19.0878097049991));
#191892=CARTESIAN_POINT('Ctrl Pts',(18.8919307797714,21.3275401986158,19.0995029860789));
#191893=CARTESIAN_POINT('Ctrl Pts',(19.0430921722761,21.3107981313767,19.1075312893274));
#191894=CARTESIAN_POINT('Ctrl Pts',(19.2817209477189,21.2580198864463,19.1209921795625));
#191895=CARTESIAN_POINT('Ctrl Pts',(19.3708436865335,21.2320680080381,19.1261994000153));
#191896=CARTESIAN_POINT('Ctrl Pts',(19.4777737216926,21.193153798485,19.132827613407));
#191897=CARTESIAN_POINT('Ctrl Pts',(19.4974659976883,21.1856525398362,19.1340643357322));
#191898=CARTESIAN_POINT('Ctrl Pts',(19.5253629264923,21.174546261387,19.1358406773342));
#191899=CARTESIAN_POINT('Ctrl Pts',(19.5336621393182,21.1711810276657,19.1363722330577));
#191900=CARTESIAN_POINT('Ctrl Pts',(19.5479630240476,21.1652762501154,19.1372936648727));
#191901=CARTESIAN_POINT('Ctrl Pts',(19.5539748258749,21.1627614479615,19.1376826985251));
#191902=CARTESIAN_POINT('Ctrl Pts',(19.5654775095669,21.1578872250532,19.1384303270526));
#191903=CARTESIAN_POINT('Ctrl Pts',(19.570970206988,21.1555322284465,19.1387887682277));
#191904=CARTESIAN_POINT('Ctrl Pts',(19.5852581125548,21.1493345293332,19.1397249559992));
#191905=CARTESIAN_POINT('Ctrl Pts',(19.5940372166824,21.1454552470841,19.1403039495925));
#191906=CARTESIAN_POINT('Ctrl Pts',(19.6240420362155,21.1319521904511,19.1422959109654));
#191907=CARTESIAN_POINT('Ctrl Pts',(19.6451344606136,21.1220379563974,19.1437188249316));
#191908=CARTESIAN_POINT('Ctrl Pts',(19.8194757360087,21.036548623844,19.1556742181414));
#191909=CARTESIAN_POINT('Ctrl Pts',(19.9631935520853,20.9430354670292,19.1668692990661));
#191910=CARTESIAN_POINT('Ctrl Pts',(20.163275311066,20.7752931537508,19.1841228700873));
#191911=CARTESIAN_POINT('Ctrl Pts',(20.2286876589771,20.7129160372257,19.1900816354081));
#191912=CARTESIAN_POINT('Ctrl Pts',(20.3161222087,20.6181500885464,19.1983195648311));
#191913=CARTESIAN_POINT('Ctrl Pts',(20.3415437868181,20.5890368150142,19.2007514439698));
#191914=CARTESIAN_POINT('Ctrl Pts',(20.3710073540054,20.553368784506,19.2035985726797));
#191915=CARTESIAN_POINT('Ctrl Pts',(20.375827200553,20.5474694079019,19.2040652798183));
#191916=CARTESIAN_POINT('Ctrl Pts',(20.3832500207663,20.5382832944963,19.2047853508607));
#191917=CARTESIAN_POINT('Ctrl Pts',(20.3858751951312,20.5350146960136,19.2050402720945));
#191918=CARTESIAN_POINT('Ctrl Pts',(20.3907134801515,20.5289537697198,19.2055105467556));
#191919=CARTESIAN_POINT('Ctrl Pts',(20.3929292327542,20.5261636762991,19.2057260859543));
#191920=CARTESIAN_POINT('Ctrl Pts',(20.3979072400023,20.5198627322616,19.2062107240824));
#191921=CARTESIAN_POINT('Ctrl Pts',(20.4006654241092,20.5163487350725,19.2064795323371));
#191922=CARTESIAN_POINT('Ctrl Pts',(20.4087290697404,20.5060082204455,19.2072663233106));
#191923=CARTESIAN_POINT('Ctrl Pts',(20.4140039335281,20.4991578075568,19.2077821853406));
#191924=CARTESIAN_POINT('Ctrl Pts',(20.4504840553929,20.4511761982057,19.2113595949867));
#191925=CARTESIAN_POINT('Ctrl Pts',(20.4802202107964,20.4089442489124,19.2143262493077));
#191926=CARTESIAN_POINT('Ctrl Pts',(20.5938196131342,20.2343747626169,19.2260563218993));
#191927=CARTESIAN_POINT('Ctrl Pts',(20.6644243904402,20.0940025802169,19.2343354390815));
#191928=CARTESIAN_POINT('Ctrl Pts',(20.7513203842857,19.8596922831932,19.2480963203755));
#191929=CARTESIAN_POINT('Ctrl Pts',(20.7779278710348,19.7702308594589,19.25333061389));
#191930=CARTESIAN_POINT('Ctrl Pts',(20.8032262249534,19.6587035343242,19.259991594395));
#191931=CARTESIAN_POINT('Ctrl Pts',(20.8075922762007,19.6380253495216,19.2612318716746));
#191932=CARTESIAN_POINT('Ctrl Pts',(20.8133686373703,19.6084864271854,19.2630124352959));
#191933=CARTESIAN_POINT('Ctrl Pts',(20.8150334230137,19.5996763157297,19.2635446047835));
#191934=CARTESIAN_POINT('Ctrl Pts',(20.817811795883,19.5844432890972,19.2644667621255));
#191935=CARTESIAN_POINT('Ctrl Pts',(20.8189517837562,19.578025269946,19.2648559039174));
#191936=CARTESIAN_POINT('Ctrl Pts',(20.8210796981587,19.5657154107885,19.2656035028531));
#191937=CARTESIAN_POINT('Ctrl Pts',(20.8220723633208,19.559824445124,19.2659618051557));
#191938=CARTESIAN_POINT('Ctrl Pts',(20.8245928406269,19.5444703283729,19.2668971051403));
#191939=CARTESIAN_POINT('Ctrl Pts',(20.8260813251085,19.5350009407245,19.2674753451747));
#191940=CARTESIAN_POINT('Ctrl Pts',(20.8309568445244,19.5025487437142,19.2694620086315));
#191941=CARTESIAN_POINT('Ctrl Pts',(20.8340297689101,19.4795210978309,19.2708803071689));
#191942=CARTESIAN_POINT('Ctrl Pts',(20.8566712892558,19.2855541510819,19.2829032001196));
#191943=CARTESIAN_POINT('Ctrl Pts',(20.8557080873532,19.1128960935249,19.2941807801964));
#191944=CARTESIAN_POINT('Ctrl Pts',(20.8225257674408,18.8535806484862,19.3114560055292));
#191945=CARTESIAN_POINT('Ctrl Pts',(20.8055620072477,18.7656672026526,19.3173566856285));
#191946=CARTESIAN_POINT('Ctrl Pts',(20.7734306829032,18.641888048593,19.3255255834195));
#191947=CARTESIAN_POINT('Ctrl Pts',(20.7627627904003,18.6049571859185,19.327943955215));
#191948=CARTESIAN_POINT('Ctrl Pts',(20.7487855197581,18.5610875733975,19.3307774126211));
#191949=CARTESIAN_POINT('Ctrl Pts',(20.7464374254655,18.5538527824783,19.3312433958096));
#191950=CARTESIAN_POINT('Ctrl Pts',(20.7427355112127,18.5426526355085,19.3319625924328));
#191951=CARTESIAN_POINT('Ctrl Pts',(20.7414088538667,18.5386784640151,19.3322173572816));
#191952=CARTESIAN_POINT('Ctrl Pts',(20.738932127636,18.5313318019756,19.3326874865056));
#191953=CARTESIAN_POINT('Ctrl Pts',(20.7377853524391,18.527958304721,19.3329030357343));
#191954=CARTESIAN_POINT('Ctrl Pts',(20.7351805794009,18.5203587959934,19.3333878761254));
#191955=CARTESIAN_POINT('Ctrl Pts',(20.7337177140957,18.5161345102697,19.3336568755223));
#191956=CARTESIAN_POINT('Ctrl Pts',(20.7293815173173,18.5037400714216,19.3344447452187));
#191957=CARTESIAN_POINT('Ctrl Pts',(20.7264713783391,18.4955827661252,19.3349614860924));
#191958=CARTESIAN_POINT('Ctrl Pts',(20.7057458574912,18.4385953023374,19.3385604267274));
#191959=CARTESIAN_POINT('Ctrl Pts',(20.6861858916074,18.3904136617868,19.3415464283923));
#191960=CARTESIAN_POINT('Ctrl Pts',(20.6401176740412,18.2879350372741,19.3478724572773));
#191961=CARTESIAN_POINT('Ctrl Pts',(20.613019857548,18.2339541350921,19.3511892495194));
#191962=CARTESIAN_POINT('Ctrl Pts',(20.5798101110025,18.1743050770372,19.3549125206352));
#191963=CARTESIAN_POINT('Ctrl Pts',(20.5759311443023,18.167428732909,19.3553426295591));
#191964=CARTESIAN_POINT('Ctrl Pts',(20.51786864747,18.0658321488365,19.361712715805));
#191965=CARTESIAN_POINT('Ctrl Pts',(20.4564797032099,17.9754193587445,19.3675896939138));
#191966=CARTESIAN_POINT('Ctrl Pts',(20.3413893847018,17.8312663816574,19.3778486639829));
#191967=CARTESIAN_POINT('Ctrl Pts',(20.2912758399324,17.7749443854973,19.3821204508981));
#191968=CARTESIAN_POINT('Ctrl Pts',(20.2250083159948,17.7080234638109,19.3876192747057));
#191969=CARTESIAN_POINT('Ctrl Pts',(20.2115679999666,17.6948083768271,19.388727274167));
#191970=CARTESIAN_POINT('Ctrl Pts',(20.1917686239179,17.6758540965962,19.3903500248149));
#191971=CARTESIAN_POINT('Ctrl Pts',(20.1855481252386,17.6699710118079,19.3908585250338));
#191972=CARTESIAN_POINT('Ctrl Pts',(20.1745788875875,17.6597221148441,19.3917529871309));
#191973=CARTESIAN_POINT('Ctrl Pts',(20.1698455343674,17.6553399444762,19.3921382405874));
#191974=CARTESIAN_POINT('Ctrl Pts',(20.1606152207652,17.6468724720768,19.3928881586286));
#191975=CARTESIAN_POINT('Ctrl Pts',(20.1561205516585,17.6427847574136,19.3932527150816));
#191976=CARTESIAN_POINT('Ctrl Pts',(20.1453330802512,17.6330585154702,19.3941262468744));
#191977=CARTESIAN_POINT('Ctrl Pts',(20.1390240312726,17.6274382360262,19.3946359832916));
#191978=CARTESIAN_POINT('Ctrl Pts',(20.1161325144858,17.6072903189353,19.3964814969577));
#191979=CARTESIAN_POINT('Ctrl Pts',(20.0993574525924,17.5929845496074,19.3978264252587));
#191980=CARTESIAN_POINT('Ctrl Pts',(19.9387768353313,17.4603170087698,19.4106353626249));
#191981=CARTESIAN_POINT('Ctrl Pts',(19.7801893562623,17.3611789023002,19.4229051906479));
#191982=CARTESIAN_POINT('Ctrl Pts',(19.5381685271012,17.2510619644581,19.4404589304331));
#191983=CARTESIAN_POINT('Ctrl Pts',(19.4637951469279,17.2221699746354,19.4456956537772));
#191984=CARTESIAN_POINT('Ctrl Pts',(19.3538073638813,17.1864463071912,19.4530667592979));
#191985=CARTESIAN_POINT('Ctrl Pts',(19.3193705705721,17.1762222545161,19.4553229664325));
#191986=CARTESIAN_POINT('Ctrl Pts',(19.2774855883302,17.1649384037487,19.4579916577795));
#191987=CARTESIAN_POINT('Ctrl Pts',(19.2702727999851,17.1630361018366,19.4584485389591));
#191988=CARTESIAN_POINT('Ctrl Pts',(19.259024140222,17.160132881136,19.4591567339893));
#191989=CARTESIAN_POINT('Ctrl Pts',(19.2549952027171,17.1591056834024,19.4594095256949));
#191990=CARTESIAN_POINT('Ctrl Pts',(19.2475051808882,17.157219547865,19.4598778440479));
#191991=CARTESIAN_POINT('Ctrl Pts',(19.2440449855488,17.1563574935375,19.4600935439111));
#191992=CARTESIAN_POINT('Ctrl Pts',(19.2362011946599,17.1544243699067,19.4605810457456));
#191993=CARTESIAN_POINT('Ctrl Pts',(19.2318163541602,17.1533585733641,19.46085254173));
#191994=CARTESIAN_POINT('Ctrl Pts',(19.2204825065344,17.1506420739839,19.4615517260124));
#191995=CARTESIAN_POINT('Ctrl Pts',(19.213528428697,17.1490124874761,19.4619782287922));
#191996=CARTESIAN_POINT('Ctrl Pts',(19.1706994361624,17.1392045263411,19.4645904096547));
#191997=CARTESIAN_POINT('Ctrl Pts',(19.1346222372207,17.1319268717651,19.4667279980098));
#191998=CARTESIAN_POINT('Ctrl Pts',(18.9307616996669,17.096307481435,19.4785481417348));
#191999=CARTESIAN_POINT('Ctrl Pts',(18.7602181564017,17.0873323709365,19.4875020295683));
#192000=CARTESIAN_POINT('Ctrl Pts',(18.49506777165,17.1053562507386,19.5021197903009));
#192001=CARTESIAN_POINT('Ctrl Pts',(18.4002683933502,17.1182878037721,19.5074782417262));
#192002=CARTESIAN_POINT('Ctrl Pts',(18.2857006414421,17.1418999000927,19.514289567983));
#192003=CARTESIAN_POINT('Ctrl Pts',(18.264795305158,17.1465401570512,19.5155460337669));
#192004=CARTESIAN_POINT('Ctrl Pts',(18.2351957923485,17.1535830257775,19.5173458105961));
#192005=CARTESIAN_POINT('Ctrl Pts',(18.2264406028694,17.1557253959756,19.5178807598492));
#192006=CARTESIAN_POINT('Ctrl Pts',(18.2113694560071,17.1595154357243,19.5188062072329));
#192007=CARTESIAN_POINT('Ctrl Pts',(18.2050468998075,17.1611365364247,19.5191958428496));
#192008=CARTESIAN_POINT('Ctrl Pts',(18.1929617117897,17.1642948085163,19.519943325187));
#192009=CARTESIAN_POINT('Ctrl Pts',(18.1871978726386,17.1658271460491,19.5203010119377));
#192010=CARTESIAN_POINT('Ctrl Pts',(18.172240217665,17.1698714438103,19.5212323636647));
#192011=CARTESIAN_POINT('Ctrl Pts',(18.163056828562,17.1724211503392,19.521807250392));
#192012=CARTESIAN_POINT('Ctrl Pts',(18.1318698905208,17.1813072563259,19.5237702288979));
#192013=CARTESIAN_POINT('Ctrl Pts',(18.1099526571315,17.1879384211769,19.525167880527));
#192014=CARTESIAN_POINT('Ctrl Pts',(17.9198016564213,17.2488534802855,19.5374567847258));
#192015=CARTESIAN_POINT('Ctrl Pts',(17.7589032007386,17.3236473035647,19.54906343178));
#192016=CARTESIAN_POINT('Ctrl Pts',(17.5362478090133,17.4632887554085,19.5664272026954));
#192017=CARTESIAN_POINT('Ctrl Pts',(17.4661479045323,17.513455342853,19.5721005278551));
#192018=CARTESIAN_POINT('Ctrl Pts',(17.3701133608509,17.5914582036778,19.5799980769635));
#192019=CARTESIAN_POINT('Ctrl Pts',(17.3415659197429,17.6159356972641,19.582362553619));
#192020=CARTESIAN_POINT('Ctrl Pts',(17.308078630144,17.6462334421172,19.5851413824312));
#192021=CARTESIAN_POINT('Ctrl Pts',(17.3025006758277,17.651334708172,19.585604426057));
#192022=CARTESIAN_POINT('Ctrl Pts',(17.2938810828393,17.6593028736466,19.5863200711913));
#192023=CARTESIAN_POINT('Ctrl Pts',(17.2908204753074,17.6621490298603,19.5865742001909));
#192024=CARTESIAN_POINT('Ctrl Pts',(17.2851656038936,17.6674389890509,19.5870437409577));
#192025=CARTESIAN_POINT('Ctrl Pts',(17.2825691051605,17.6698802578435,19.5872593338399));
#192026=CARTESIAN_POINT('Ctrl Pts',(17.2767199459259,17.6754076234548,19.5877450095963));
#192027=CARTESIAN_POINT('Ctrl Pts',(17.2734709263437,17.6784974946967,19.5880147962159));
#192028=CARTESIAN_POINT('Ctrl Pts',(17.2639304848178,17.687628509944,19.5888071153665));
#192029=CARTESIAN_POINT('Ctrl Pts',(17.2576664645815,17.6936983245562,19.5893274822458));
#192030=CARTESIAN_POINT('Ctrl Pts',(17.2133360265989,17.7371888149357,19.5930127586802));
#192031=CARTESIAN_POINT('Ctrl Pts',(17.1766560206251,17.7760020625543,19.5960761603608));
#192032=CARTESIAN_POINT('Ctrl Pts',(17.132465941483,17.8264550157788,19.5998478811659));
#192033=CARTESIAN_POINT('Ctrl Pts',(17.1235520946257,17.8368334491352,19.6006131075048));
#192034=CARTESIAN_POINT('Ctrl Pts',(17.0811101336374,17.8872290511397,19.604282006823));
#192035=CARTESIAN_POINT('Ctrl Pts',(17.0489682802044,17.9283921402587,19.6071384933003));
#192036=CARTESIAN_POINT('Ctrl Pts',(16.9542697452041,18.0593822573851,19.615939036211));
#192037=CARTESIAN_POINT('Ctrl Pts',(16.8971322488468,18.1528983059434,19.6218308921262));
#192038=CARTESIAN_POINT('Ctrl Pts',(16.813078747798,18.3179720091444,19.6321302032128));
#192039=CARTESIAN_POINT('Ctrl Pts',(16.7823335285292,18.3873291412583,19.636427835384));
#192040=CARTESIAN_POINT('Ctrl Pts',(16.7486505848235,18.4758575711171,19.6419578096697));
#192041=CARTESIAN_POINT('Ctrl Pts',(16.7421624441066,18.493622966858,19.6430695301577));
#192042=CARTESIAN_POINT('Ctrl Pts',(16.7330803287254,18.5195645535797,19.644696740902));
#192043=CARTESIAN_POINT('Ctrl Pts',(16.7302965253457,18.5276736578911,19.6452059309915));
#192044=CARTESIAN_POINT('Ctrl Pts',(16.725504182462,18.5419146669503,19.6461011909323));
#192045=CARTESIAN_POINT('Ctrl Pts',(16.7234742631139,18.5480392984,19.6464865484062));
#192046=CARTESIAN_POINT('Ctrl Pts',(16.7195884541046,18.5599454756006,19.6472363604058));
#192047=CARTESIAN_POINT('Ctrl Pts',(16.7177293756122,18.5657259202373,19.6476007053494));
#192048=CARTESIAN_POINT('Ctrl Pts',(16.7133468280937,18.5795564707534,19.6484732322496));
#192049=CARTESIAN_POINT('Ctrl Pts',(16.7108465750286,18.587613773359,19.6489821713322));
#192050=CARTESIAN_POINT('Ctrl Pts',(16.7020108021116,18.6167010056546,19.6508218523817));
#192051=CARTESIAN_POINT('Ctrl Pts',(16.6959546563562,18.6378137168152,19.6521616702444));
#192052=CARTESIAN_POINT('Ctrl Pts',(16.6414577136117,18.8395937628833,19.6650134957142));
#192053=CARTESIAN_POINT('Ctrl Pts',(16.6168436525267,19.0258066914941,19.6773392599676));
#192054=CARTESIAN_POINT('Ctrl Pts',(16.6170536900505,19.2757905700977,19.6938412690976));
#192055=CARTESIAN_POINT('Ctrl Pts',(16.6199199093842,19.3387716912197,19.6979837650249));
#192056=CARTESIAN_POINT('Ctrl Pts',(16.6300811408575,19.4512138925938,19.7052635137628));
#192057=CARTESIAN_POINT('Ctrl Pts',(16.6363255963833,19.5007244264126,19.7084278687014));
#192058=CARTESIAN_POINT('Ctrl Pts',(16.6455655237812,19.5576864818788,19.711986617993));
#192059=CARTESIAN_POINT('Ctrl Pts',(16.6468596259024,19.5653940480585,19.7124664019341));
#192060=CARTESIAN_POINT('Ctrl Pts',(16.6489941842195,19.5776899281943,19.7132288084176));
#192061=CARTESIAN_POINT('Ctrl Pts',(16.6498071586511,19.5822828521593,19.713512924633));
#192062=CARTESIAN_POINT('Ctrl Pts',(16.6512728103081,19.5904065696733,19.7140142252334));
#192063=CARTESIAN_POINT('Ctrl Pts',(16.6519192986531,19.5939384357997,19.714231757366));
#192064=CARTESIAN_POINT('Ctrl Pts',(16.6533073565621,19.6014141734707,19.7146913079822));
#192065=CARTESIAN_POINT('Ctrl Pts',(16.6540511534524,19.60535757843,19.7149331980395));
#192066=CARTESIAN_POINT('Ctrl Pts',(16.6560859627934,19.6159796595447,19.7155834164187));
#192067=CARTESIAN_POINT('Ctrl Pts',(16.6573979718346,19.6226543333368,19.7159905648095));
#192068=CARTESIAN_POINT('Ctrl Pts',(16.6640292674551,19.6555515422671,19.7179906964502));
#192069=CARTESIAN_POINT('Ctrl Pts',(16.6698134445377,19.6816792138249,19.7195586405791));
#192070=CARTESIAN_POINT('Ctrl Pts',(16.6879077566179,19.756648145912,19.7240162630924));
#192071=CARTESIAN_POINT('Ctrl Pts',(16.7014678348523,19.8051708858565,19.7268505491724));
#192072=CARTESIAN_POINT('Ctrl Pts',(16.7257202826567,19.881355665803,19.731284302869));
#192073=CARTESIAN_POINT('Ctrl Pts',(16.735280380112,19.9093428335651,19.73290946559));
#192074=CARTESIAN_POINT('Ctrl Pts',(16.7454193946088,19.9371103055747,19.7345260524097));
#192075=CARTESIAN_POINT('Origin',(18.734,19.211,0.));
#192076=CARTESIAN_POINT('',(16.7454193572566,19.9371102032791,20.755413683557));
#192077=CARTESIAN_POINT('',(16.7454193623258,19.9371102171621,20.5336910458214));
#192078=CARTESIAN_POINT('',(16.7454193623258,19.9371102171621,0.));
#192079=CARTESIAN_POINT('Ctrl Pts',(16.7454193572565,19.9371102032791,20.755413683557));
#192080=CARTESIAN_POINT('Ctrl Pts',(16.7360405234064,19.9114246153868,20.7536067709888));
#192081=CARTESIAN_POINT('Ctrl Pts',(16.7271552312975,19.8855460612012,20.7517981507751));
#192082=CARTESIAN_POINT('Ctrl Pts',(16.6954799915782,19.7871126977697,20.7449759971118));
#192083=CARTESIAN_POINT('Ctrl Pts',(16.6761041950082,19.7135297019902,20.7399903579701));
#192084=CARTESIAN_POINT('Ctrl Pts',(16.6536719560301,19.6048809317995,20.7329253866806));
#192085=CARTESIAN_POINT('Ctrl Pts',(16.6474610431052,19.5705309000379,20.7307344299769));
#192086=CARTESIAN_POINT('Ctrl Pts',(16.640966352227,19.5287323593999,20.7281324028596));
#192087=CARTESIAN_POINT('Ctrl Pts',(16.6398690489289,19.5214178899481,20.7276794301417));
#192088=CARTESIAN_POINT('Ctrl Pts',(16.638216799776,19.5099965700239,20.7269759736824));
#192089=CARTESIAN_POINT('Ctrl Pts',(16.6376355527492,19.5058936693283,20.7267240430256));
#192090=CARTESIAN_POINT('Ctrl Pts',(16.6365763773633,19.4982557595705,20.7262565239903));
#192091=CARTESIAN_POINT('Ctrl Pts',(16.6360953412418,19.4947212844061,20.7260407673694));
#192092=CARTESIAN_POINT('Ctrl Pts',(16.6350235901553,19.4866946828845,20.7255521198264));
#192093=CARTESIAN_POINT('Ctrl Pts',(16.6344383623656,19.4822018766634,20.725279541175));
#192094=CARTESIAN_POINT('Ctrl Pts',(16.6327408111968,19.4688348488033,20.7244712559344));
#192095=CARTESIAN_POINT('Ctrl Pts',(16.6316702786934,19.4599552913088,20.7239378480796));
#192096=CARTESIAN_POINT('Ctrl Pts',(16.6239226573551,19.3920751822681,20.7198852923423));
#192097=CARTESIAN_POINT('Ctrl Pts',(16.6196735634268,19.3328182834744,20.716492044051));
#192098=CARTESIAN_POINT('Ctrl Pts',(16.617322962857,19.2531770715579,20.7120327766097));
#192099=CARTESIAN_POINT('Ctrl Pts',(16.617015959299,19.2328903772815,20.7109057039679));
#192100=CARTESIAN_POINT('Ctrl Pts',(16.6168948154794,19.0728053060273,20.7020607908922));
#192101=CARTESIAN_POINT('Ctrl Pts',(16.6306360838822,18.9333414187302,20.6946257313364));
#192102=CARTESIAN_POINT('Ctrl Pts',(16.67575019094,18.7075305319075,20.681879489083));
#192103=CARTESIAN_POINT('Ctrl Pts',(16.6991411766927,18.6200512110003,20.6767637970216));
#192104=CARTESIAN_POINT('Ctrl Pts',(16.7324403978102,18.521335896224,20.6706560331205));
#192105=CARTESIAN_POINT('Ctrl Pts',(16.7369541254703,18.5083726599828,20.6698472613802));
#192106=CARTESIAN_POINT('Ctrl Pts',(16.7443954423061,18.4876526260788,20.6685433693409));
#192107=CARTESIAN_POINT('Ctrl Pts',(16.747243134023,18.4798674047311,20.6680509030762));
#192108=CARTESIAN_POINT('Ctrl Pts',(16.7523808176238,18.4660733160688,20.6671737171445));
#192109=CARTESIAN_POINT('Ctrl Pts',(16.7546526122558,18.4600577481487,20.6667896098438));
#192110=CARTESIAN_POINT('Ctrl Pts',(16.759443379556,18.4475448853049,20.6659873210957));
#192111=CARTESIAN_POINT('Ctrl Pts',(16.7619670934187,18.4410494996128,20.6655689840444));
#192112=CARTESIAN_POINT('Ctrl Pts',(16.7686050585362,18.4242118372076,20.6644796217732));
#192113=CARTESIAN_POINT('Ctrl Pts',(16.7727688479728,18.4138894368112,20.6638069323112));
#192114=CARTESIAN_POINT('Ctrl Pts',(16.7912114314484,18.3691880444909,20.660872359401));
#192115=CARTESIAN_POINT('Ctrl Pts',(16.8063135236491,18.3351579117907,20.6585826975868));
#192116=CARTESIAN_POINT('Ctrl Pts',(16.8488257062101,18.2457962822775,20.6524166966283));
#192117=CARTESIAN_POINT('Ctrl Pts',(16.8777709759424,18.1912387444737,20.6484905850074));
#192118=CARTESIAN_POINT('Ctrl Pts',(16.983280513165,18.0117849697807,20.6350415605223));
#192119=CARTESIAN_POINT('Ctrl Pts',(17.0704029012234,17.8935878040075,20.625236349674));
#192120=CARTESIAN_POINT('Ctrl Pts',(17.1821607821435,17.770907906973,20.6144037596385));
#192121=CARTESIAN_POINT('Ctrl Pts',(17.195508363814,17.7566569480662,20.6131348281491));
#192122=CARTESIAN_POINT('Ctrl Pts',(17.2456831712661,17.7045501633054,20.6084613457109));
#192123=CARTESIAN_POINT('Ctrl Pts',(17.2837290690397,17.6678884260932,20.6051051910233));
#192124=CARTESIAN_POINT('Ctrl Pts',(17.3295906258319,17.6268917727283,20.6013107135223));
#192125=CARTESIAN_POINT('Ctrl Pts',(17.3361072842789,17.6211382049882,20.600777191963));
#192126=CARTESIAN_POINT('Ctrl Pts',(17.3460336042793,17.6124824593865,20.599973286667));
#192127=CARTESIAN_POINT('Ctrl Pts',(17.3494172446117,17.6095507695739,20.5997007814424));
#192128=CARTESIAN_POINT('Ctrl Pts',(17.3555106504386,17.6043050039595,20.599212817212));
#192129=CARTESIAN_POINT('Ctrl Pts',(17.3582169678206,17.6019870273679,20.5989970721733));
#192130=CARTESIAN_POINT('Ctrl Pts',(17.3641139118961,17.5969620162716,20.5985291006686));
#192131=CARTESIAN_POINT('Ctrl Pts',(17.3673067049495,17.5942576132054,20.5982770668745));
#192132=CARTESIAN_POINT('Ctrl Pts',(17.3763062272574,17.5866804253261,20.5975703516761));
#192133=CARTESIAN_POINT('Ctrl Pts',(17.3821312080661,17.5818292801102,20.5971172261746));
#192134=CARTESIAN_POINT('Ctrl Pts',(17.4172901011271,17.552866753344,20.5944070627941));
#192135=CARTESIAN_POINT('Ctrl Pts',(17.4472443095138,17.5295152340343,20.5922013604281));
#192136=CARTESIAN_POINT('Ctrl Pts',(17.5483211305015,17.4550023281803,20.5850329287542));
#192137=CARTESIAN_POINT('Ctrl Pts',(17.621993752691,17.4074460801967,20.5802384872086));
#192138=CARTESIAN_POINT('Ctrl Pts',(17.8507219828837,17.2791596527319,20.5659712393524));
#192139=CARTESIAN_POINT('Ctrl Pts',(18.013003440267,17.212914815332,20.5565783590459));
#192140=CARTESIAN_POINT('Ctrl Pts',(18.2038288681461,17.1613319378261,20.5450925151874));
#192141=CARTESIAN_POINT('Ctrl Pts',(18.2261824781215,17.1556796120311,20.5437418037939));
#192142=CARTESIAN_POINT('Ctrl Pts',(18.2579259575103,17.1482024222837,20.5418145608796));
#192143=CARTESIAN_POINT('Ctrl Pts',(18.2672432067356,17.1460742308853,20.5412477787274));
#192144=CARTESIAN_POINT('Ctrl Pts',(18.2824025517023,17.1427194641068,20.5403237036973));
#192145=CARTESIAN_POINT('Ctrl Pts',(18.2882360530709,17.1414543655773,20.5399676506763));
#192146=CARTESIAN_POINT('Ctrl Pts',(18.3004557869014,17.1388583614571,20.5392208176931));
#192147=CARTESIAN_POINT('Ctrl Pts',(18.3068429680259,17.1375322709405,20.5388298878124));
#192148=CARTESIAN_POINT('Ctrl Pts',(18.3220482928485,17.1344486187132,20.5378978528599));
#192149=CARTESIAN_POINT('Ctrl Pts',(18.3308716521666,17.1327176853411,20.5373559034082));
#192150=CARTESIAN_POINT('Ctrl Pts',(18.3606150748435,17.1270792691438,20.5355251291983));
#192151=CARTESIAN_POINT('Ctrl Pts',(18.3815824373881,17.1234311449693,20.5342280935267));
#192152=CARTESIAN_POINT('Ctrl Pts',(18.5599586830884,17.0951592204248,20.5231357202773));
#192153=CARTESIAN_POINT('Ctrl Pts',(18.7196001142215,17.0880664030753,20.512767393336));
#192154=CARTESIAN_POINT('Ctrl Pts',(19.0098595657144,17.1079241099886,20.4935492169254));
#192155=CARTESIAN_POINT('Ctrl Pts',(19.1401117332352,17.1291484027072,20.484806486761));
#192156=CARTESIAN_POINT('Ctrl Pts',(19.2827906698167,17.1663079376869,20.4756083278399));
#192157=CARTESIAN_POINT('Ctrl Pts',(19.2979808493031,17.1704455498151,20.4746342580374));
#192158=CARTESIAN_POINT('Ctrl Pts',(19.3187013255591,17.1763386072796,20.4733140308221));
#192159=CARTESIAN_POINT('Ctrl Pts',(19.3242722228199,17.1779477803255,20.4729599180036));
#192160=CARTESIAN_POINT('Ctrl Pts',(19.3331114559787,17.1805404187054,20.4723994731689));
#192161=CARTESIAN_POINT('Ctrl Pts',(19.3363840983638,17.181508919365,20.4721922835853));
#192162=CARTESIAN_POINT('Ctrl Pts',(19.343135687307,17.1835247439,20.4717655043878));
#192163=CARTESIAN_POINT('Ctrl Pts',(19.3466142814251,17.1845731096357,20.4715459830207));
#192164=CARTESIAN_POINT('Ctrl Pts',(19.3548927620743,17.1870913120957,20.4710243987543));
#192165=CARTESIAN_POINT('Ctrl Pts',(19.3596901894528,17.1885692874724,20.4707228105293));
#192166=CARTESIAN_POINT('Ctrl Pts',(19.3758346181164,17.1936059533133,20.4697100255666));
#192167=CARTESIAN_POINT('Ctrl Pts',(19.3871571164829,17.1972432588737,20.4690032816683));
#192168=CARTESIAN_POINT('Ctrl Pts',(19.5222534827858,17.2419017272187,20.4606065190369));
#192169=CARTESIAN_POINT('Ctrl Pts',(19.6420314235768,17.2941848349504,20.4535133207687));
#192170=CARTESIAN_POINT('Ctrl Pts',(19.8982625207909,17.435476969937,20.4376172869786));
#192171=CARTESIAN_POINT('Ctrl Pts',(20.0307900535159,17.529834386761,20.428838921153));
#192172=CARTESIAN_POINT('Ctrl Pts',(20.1688705616499,17.6542731541333,20.4180456363176));
#192173=CARTESIAN_POINT('Ctrl Pts',(20.1862277694474,17.6704525518004,20.4166562195909));
#192174=CARTESIAN_POINT('Ctrl Pts',(20.2102693970498,17.6936301882928,20.4146831158096));
#192175=CARTESIAN_POINT('Ctrl Pts',(20.2171837810385,17.700388089184,20.4141098265459));
#192176=CARTESIAN_POINT('Ctrl Pts',(20.228305950999,17.7114085239148,20.4131780419522));
#192177=CARTESIAN_POINT('Ctrl Pts',(20.2325424151096,17.7156420163315,20.4128208286025));
#192178=CARTESIAN_POINT('Ctrl Pts',(20.2413434535371,17.7245118420871,20.412073895761));
#192179=CARTESIAN_POINT('Ctrl Pts',(20.2459047272847,17.729151348928,20.4116840366554));
#192180=CARTESIAN_POINT('Ctrl Pts',(20.2566525961092,17.7401848423212,20.4107588149818));
#192181=CARTESIAN_POINT('Ctrl Pts',(20.2628203769044,17.746596910724,20.4102226404731));
#192182=CARTESIAN_POINT('Ctrl Pts',(20.283224528661,17.7680786142498,20.4084312197407));
#192183=CARTESIAN_POINT('Ctrl Pts',(20.2972795993635,17.7833180984901,20.4071682347395));
#192184=CARTESIAN_POINT('Ctrl Pts',(20.3711079567019,17.8657654173804,20.4003747605943));
#192185=CARTESIAN_POINT('Ctrl Pts',(20.4267690679071,17.9365166427092,20.3946763524443));
#192186=CARTESIAN_POINT('Ctrl Pts',(20.5545411153404,18.1221220128579,20.3800734122205));
#192187=CARTESIAN_POINT('Ctrl Pts',(20.6204437707324,18.240767324393,20.371023215521));
#192188=CARTESIAN_POINT('Ctrl Pts',(20.7047480655799,18.4341176291726,20.3572297754403));
#192189=CARTESIAN_POINT('Ctrl Pts',(20.7312131745221,18.5049290342137,20.3523672098846));
#192190=CARTESIAN_POINT('Ctrl Pts',(20.7566811408368,18.5860679108787,20.3471148050684));
#192191=CARTESIAN_POINT('Ctrl Pts',(20.7594631137464,18.5951442570876,20.3465316864768));
#192192=CARTESIAN_POINT('Ctrl Pts',(20.7634966847071,18.6086270399203,20.3456723383378));
#192193=CARTESIAN_POINT('Ctrl Pts',(20.7647951422279,18.6130191746498,20.3453934740385));
#192194=CARTESIAN_POINT('Ctrl Pts',(20.7670808066898,18.6208439272097,20.3448986234403));
#192195=CARTESIAN_POINT('Ctrl Pts',(20.7680735885011,18.6242748565138,20.344682315733));
#192196=CARTESIAN_POINT('Ctrl Pts',(20.770190244178,18.6316596982541,20.3442181766255));
#192197=CARTESIAN_POINT('Ctrl Pts',(20.7713112837345,18.6356143644983,20.3439705109225));
#192198=CARTESIAN_POINT('Ctrl Pts',(20.7743759483835,18.6465467646867,20.3432882379141));
#192199=CARTESIAN_POINT('Ctrl Pts',(20.7762953124382,18.6535313229972,20.3428550183408));
#192200=CARTESIAN_POINT('Ctrl Pts',(20.7866460997443,18.6919688314418,20.3404849055409));
#192201=CARTESIAN_POINT('Ctrl Pts',(20.7943873030811,18.723605099902,20.3385855181239));
#192202=CARTESIAN_POINT('Ctrl Pts',(20.8364003226817,18.9142532930349,20.3273768860303));
#192203=CARTESIAN_POINT('Ctrl Pts',(20.8529854148541,19.0766185712416,20.3187795159991));
#192204=CARTESIAN_POINT('Ctrl Pts',(20.8492493029358,19.3561189756619,20.3034769374846));
#192205=CARTESIAN_POINT('Ctrl Pts',(20.8380201751821,19.4725969651671,20.2969546458735));
#192206=CARTESIAN_POINT('Ctrl Pts',(20.8147015453552,19.6016075761323,20.2892743087989));
#192207=CARTESIAN_POINT('Ctrl Pts',(20.8120175823736,19.6156431907405,20.2884328051853));
#192208=CARTESIAN_POINT('Ctrl Pts',(20.8075198239715,19.6379379582523,20.2870862350652));
#192209=CARTESIAN_POINT('Ctrl Pts',(20.8057982552639,19.6462154258775,20.2865841097929));
#192210=CARTESIAN_POINT('Ctrl Pts',(20.8026745717422,19.6607957376827,20.2856957086019));
#192211=CARTESIAN_POINT('Ctrl Pts',(20.8012931104012,19.6671029310064,20.285310098715));
#192212=CARTESIAN_POINT('Ctrl Pts',(20.7983761289868,19.6801351416822,20.2845105958341));
#192213=CARTESIAN_POINT('Ctrl Pts',(20.7968365513906,19.686859163605,20.2840965764881));
#192214=CARTESIAN_POINT('Ctrl Pts',(20.7928002866257,19.7040995917253,20.2830310859916));
#192215=CARTESIAN_POINT('Ctrl Pts',(20.7902558947911,19.7146045233325,20.2823780853774));
#192216=CARTESIAN_POINT('Ctrl Pts',(20.7793002306081,19.7583690818196,20.2796415347955));
#192217=CARTESIAN_POINT('Ctrl Pts',(20.7701619401166,19.791439731883,20.2775346424721));
#192218=CARTESIAN_POINT('Ctrl Pts',(20.7442602346618,19.8770178220103,20.271976989016));
#192219=CARTESIAN_POINT('Ctrl Pts',(20.7262436205413,19.9291159277158,20.2684877867773));
#192220=CARTESIAN_POINT('Ctrl Pts',(20.6664544650889,20.0823648364326,20.2579141975199));
#192221=CARTESIAN_POINT('Ctrl Pts',(20.6188549990231,20.1810387129481,20.2506814311898));
#192222=CARTESIAN_POINT('Ctrl Pts',(20.5395024012637,20.3174330896548,20.2402577092099));
#192223=CARTESIAN_POINT('Ctrl Pts',(20.5137261904854,20.3584354126835,20.2370658065293));
#192224=CARTESIAN_POINT('Ctrl Pts',(20.4766412853106,20.4131661283792,20.2327528104882));
#192225=CARTESIAN_POINT('Ctrl Pts',(20.466532949448,20.4276888070272,20.2316031723067));
#192226=CARTESIAN_POINT('Ctrl Pts',(20.4252231428441,20.4854798161267,20.2270120691498));
#192227=CARTESIAN_POINT('Ctrl Pts',(20.392570622119,20.527692465452,20.2236210422723));
#192228=CARTESIAN_POINT('Ctrl Pts',(20.3527633195014,20.575320471957,20.2197919159971));
#192229=CARTESIAN_POINT('Ctrl Pts',(20.347129931257,20.5819766101782,20.2192567223926));
#192230=CARTESIAN_POINT('Ctrl Pts',(20.3385381903742,20.5920019165778,20.2184507840164));
#192231=CARTESIAN_POINT('Ctrl Pts',(20.3356100771738,20.5953967131972,20.2181779024872));
#192232=CARTESIAN_POINT('Ctrl Pts',(20.3303348968112,20.6014735159223,20.2176895258111));
#192233=CARTESIAN_POINT('Ctrl Pts',(20.3279918318567,20.6041589075969,20.2174737425564));
#192234=CARTESIAN_POINT('Ctrl Pts',(20.3228860001873,20.6099809681146,20.2170059934483));
#192235=CARTESIAN_POINT('Ctrl Pts',(20.3201207309398,20.6131153655511,20.216754218622));
#192236=CARTESIAN_POINT('Ctrl Pts',(20.3123276496866,20.6218961655882,20.2160489478122));
#192237=CARTESIAN_POINT('Ctrl Pts',(20.3072787890959,20.6275239198566,20.2155969976132));
#192238=CARTESIAN_POINT('Ctrl Pts',(20.2769247814778,20.6609957750554,20.2129085161081));
#192239=CARTESIAN_POINT('Ctrl Pts',(20.250909449883,20.6881901513942,20.210722371243));
#192240=CARTESIAN_POINT('Ctrl Pts',(20.1629330384616,20.775376880385,20.2036492250293));
#192241=CARTESIAN_POINT('Ctrl Pts',(20.0980283284796,20.8322815061929,20.1989254518203));
#192242=CARTESIAN_POINT('Ctrl Pts',(19.8901866664579,20.9931630123345,20.1846219515936));
#192243=CARTESIAN_POINT('Ctrl Pts',(19.7375871759269,21.0833457862731,20.1751335931527));
#192244=CARTESIAN_POINT('Ctrl Pts',(19.5545465211021,21.1626447596673,20.1635411669508));
#192245=CARTESIAN_POINT('Ctrl Pts',(19.5333788633068,21.1714099657586,20.1621989074792));
#192246=CARTESIAN_POINT('Ctrl Pts',(19.5032080725475,21.1833333431225,20.1602816822511));
#192247=CARTESIAN_POINT('Ctrl Pts',(19.4943189799726,21.1867770419358,20.1597163275187));
#192248=CARTESIAN_POINT('Ctrl Pts',(19.4798309069186,21.1922775760549,20.1587939581265));
#192249=CARTESIAN_POINT('Ctrl Pts',(19.4742458956537,21.1943710162095,20.1584381742932));
#192250=CARTESIAN_POINT('Ctrl Pts',(19.4625309178412,21.1987057884483,20.1576913988496));
#192251=CARTESIAN_POINT('Ctrl Pts',(19.4563992920302,21.2009424265729,20.1573002550875));
#192252=CARTESIAN_POINT('Ctrl Pts',(19.4417770756449,21.2061996955185,20.1563667729603));
#192253=CARTESIAN_POINT('Ctrl Pts',(19.4332773991719,21.20919451728,20.1558235830666));
#192254=CARTESIAN_POINT('Ctrl Pts',(19.4045268851145,21.2191187231953,20.1539841510221));
#192255=CARTESIAN_POINT('Ctrl Pts',(19.3841906717087,21.2257950634593,20.1526795911252));
#192256=CARTESIAN_POINT('Ctrl Pts',(19.2725841393161,21.2605696324252,20.1454989502379));
#192257=CARTESIAN_POINT('Ctrl Pts',(19.1796055673667,21.2827721807551,20.1394327631581));
#192258=CARTESIAN_POINT('Ctrl Pts',(18.9174387483159,21.3269086169007,20.1221549648676));
#192259=CARTESIAN_POINT('Ctrl Pts',(18.7466315512495,21.3348070588791,20.1106593089952));
#192260=CARTESIAN_POINT('Ctrl Pts',(18.540137215944,21.3194242056132,20.0974444597342));
#192261=CARTESIAN_POINT('Ctrl Pts',(18.5036195834844,21.3157471696094,20.0951364750847));
#192262=CARTESIAN_POINT('Ctrl Pts',(18.4601344208153,21.3102230867747,20.0924371611454));
#192263=CARTESIAN_POINT('Ctrl Pts',(18.4530597181988,21.3092879890239,20.09199956308));
#192264=CARTESIAN_POINT('Ctrl Pts',(18.4415211199964,21.3077034721454,20.0912885523864));
#192265=CARTESIAN_POINT('Ctrl Pts',(18.4370543994273,21.3070755369323,20.0910139727803));
#192266=CARTESIAN_POINT('Ctrl Pts',(18.4290601394359,21.3059256303732,20.0905237723634));
#192267=CARTESIAN_POINT('Ctrl Pts',(18.4255318936259,21.3054090200606,20.0903078539851));
#192268=CARTESIAN_POINT('Ctrl Pts',(18.4178911011047,21.3042705183525,20.0898411977077));
#192269=CARTESIAN_POINT('Ctrl Pts',(18.4137790897344,21.3036454234477,20.0895906433677));
#192270=CARTESIAN_POINT('Ctrl Pts',(18.4022912549831,21.3018644256533,20.0888922292462));
#192271=CARTESIAN_POINT('Ctrl Pts',(18.3949195806381,21.3006816051628,20.0884458673054));
#192272=CARTESIAN_POINT('Ctrl Pts',(18.3520181323961,21.2935648644531,20.0858578672664));
#192273=CARTESIAN_POINT('Ctrl Pts',(18.3166358985153,21.2867635022141,20.0837623328045));
#192274=CARTESIAN_POINT('Ctrl Pts',(18.2031781593225,21.2619353364722,20.0771188420649));
#192275=CARTESIAN_POINT('Ctrl Pts',(18.1259430232486,21.2403783037761,20.0727122632516));
#192276=CARTESIAN_POINT('Ctrl Pts',(17.8744321063013,21.1545254361515,20.0582244897316));
#192277=CARTESIAN_POINT('Ctrl Pts',(17.7074238363211,21.0717212179973,20.0482960852484));
#192278=CARTESIAN_POINT('Ctrl Pts',(17.5350110583752,20.9558790549349,20.0362152447816));
#192279=CARTESIAN_POINT('Ctrl Pts',(17.5168619472329,20.9432679656353,20.0349197419333));
#192280=CARTESIAN_POINT('Ctrl Pts',(17.4920448525922,20.9254410011361,20.0331134932818));
#192281=CARTESIAN_POINT('Ctrl Pts',(17.4852053367591,20.9204655364926,20.0326119737449));
#192282=CARTESIAN_POINT('Ctrl Pts',(17.4735025671535,20.9118445433144,20.0317473342323));
#192283=CARTESIAN_POINT('Ctrl Pts',(17.4686248260444,20.9082187857452,20.0313849848891));
#192284=CARTESIAN_POINT('Ctrl Pts',(17.4587692539056,20.9008267684271,20.0306488192116));
#192285=CARTESIAN_POINT('Ctrl Pts',(17.4537923346029,20.8970593984915,20.0302749615523));
#192286=CARTESIAN_POINT('Ctrl Pts',(17.4422650104339,20.8882531158872,20.0294041018187));
#192287=CARTESIAN_POINT('Ctrl Pts',(17.4357273382998,20.8831977726572,20.028906453325));
#192288=CARTESIAN_POINT('Ctrl Pts',(17.4220467693018,20.8724905006463,20.0278571079414));
#192289=CARTESIAN_POINT('Ctrl Pts',(17.4149104277188,20.8668305044623,20.0273050948379));
#192290=CARTESIAN_POINT('Ctrl Pts',(17.3960102361514,20.8516406053842,20.0258306232565));
#192291=CARTESIAN_POINT('Ctrl Pts',(17.3843118766357,20.8420303967656,20.0249049528496));
#192292=CARTESIAN_POINT('Ctrl Pts',(17.3489534044081,20.812342501638,20.0220665889949));
#192293=CARTESIAN_POINT('Ctrl Pts',(17.3256315849277,20.791870054702,20.0201380780432));
#192294=CARTESIAN_POINT('Ctrl Pts',(17.1786346376612,20.6569976316224,20.0076111770037));
#192295=CARTESIAN_POINT('Ctrl Pts',(17.0685545541891,20.528704513821,19.9964228356037));
#192296=CARTESIAN_POINT('Ctrl Pts',(16.9197639325812,20.3064650164272,19.9788045468916));
#192297=CARTESIAN_POINT('Ctrl Pts',(16.8705050518759,20.2203994973653,19.9723517881039));
#192298=CARTESIAN_POINT('Ctrl Pts',(16.823235326096,20.1224611060637,19.9656327721567));
#192299=CARTESIAN_POINT('Ctrl Pts',(16.8190812888893,20.1137011271451,19.965037099068));
#192300=CARTESIAN_POINT('Ctrl Pts',(16.8130369086222,20.1007253175875,19.9641628924462));
#192301=CARTESIAN_POINT('Ctrl Pts',(16.8111000205983,20.0965314841057,19.9638815930442));
#192302=CARTESIAN_POINT('Ctrl Pts',(16.8076882729761,20.0890802443734,19.9633840592414));
#192303=CARTESIAN_POINT('Ctrl Pts',(16.8062079245864,20.0858254110856,19.9631674899564));
#192304=CARTESIAN_POINT('Ctrl Pts',(16.8030539888957,20.0788439893014,19.9627046029928));
#192305=CARTESIAN_POINT('Ctrl Pts',(16.8013829439056,20.0751163131825,19.9624584414997));
#192306=CARTESIAN_POINT('Ctrl Pts',(16.7968258155018,20.0648711758014,19.9617845528517));
#192307=CARTESIAN_POINT('Ctrl Pts',(16.7939618108712,20.0583438699625,19.9613581576325));
#192308=CARTESIAN_POINT('Ctrl Pts',(16.7788510569385,20.023426951888,19.9590922720175));
#192309=CARTESIAN_POINT('Ctrl Pts',(16.7671936889874,19.9947844752305,19.9572865043125));
#192310=CARTESIAN_POINT('Ctrl Pts',(16.7525148722082,19.9563258362801,19.9549187002088));
#192311=CARTESIAN_POINT('Ctrl Pts',(16.7489321373149,19.9467305698026,19.9543325877505));
#192312=CARTESIAN_POINT('Ctrl Pts',(16.7454193617555,19.9371102156003,19.9537492222746));
#192313=CARTESIAN_POINT('',(16.6170003908425,19.209713599163,20.489056279057));
#192314=CARTESIAN_POINT('Ctrl Pts',(16.7454193946088,19.9371103055747,19.7345260524097));
#192315=CARTESIAN_POINT('Ctrl Pts',(16.7805470626998,20.0333135944443,19.7401268852385));
#192316=CARTESIAN_POINT('Ctrl Pts',(16.8226235252127,20.1268794616034,19.745631482775));
#192317=CARTESIAN_POINT('Ctrl Pts',(16.9207547019587,20.3085630814941,19.7569906986618));
#192318=CARTESIAN_POINT('Ctrl Pts',(16.9768430326951,20.3962841744325,19.7628328189229));
#192319=CARTESIAN_POINT('Ctrl Pts',(17.0475681360481,20.4907789738437,19.769749572138));
#192320=CARTESIAN_POINT('Ctrl Pts',(17.0561041186966,20.501950057493,19.7705776639458));
#192321=CARTESIAN_POINT('Ctrl Pts',(17.0699092553026,20.5196486712185,19.7719067762762));
#192322=CARTESIAN_POINT('Ctrl Pts',(17.0751071271934,20.5262314567147,19.7724049751719));
#192323=CARTESIAN_POINT('Ctrl Pts',(17.0843685901543,20.5378182854468,19.7732888190482));
#192324=CARTESIAN_POINT('Ctrl Pts',(17.0884161970686,20.5428350111995,19.7736738200008));
#192325=CARTESIAN_POINT('Ctrl Pts',(17.0968603405106,20.5532036758737,19.7744744286734));
#192326=CARTESIAN_POINT('Ctrl Pts',(17.1012603512762,20.5585526742631,19.7748901744508));
#192327=CARTESIAN_POINT('Ctrl Pts',(17.1126754383053,20.572291765164,19.7759651493995));
#192328=CARTESIAN_POINT('Ctrl Pts',(17.1197293575681,20.5806491850875,19.7766259608276));
#192329=CARTESIAN_POINT('Ctrl Pts',(17.1499117134608,20.615851909523,19.7794391960059));
#192330=CARTESIAN_POINT('Ctrl Pts',(17.1736463817918,20.6421676824092,19.7816166285068));
#192331=CARTESIAN_POINT('Ctrl Pts',(17.2376864189761,20.7096845787293,19.7874063402134));
#192332=CARTESIAN_POINT('Ctrl Pts',(17.2790311926336,20.7498549764321,19.7910611815857));
#192333=CARTESIAN_POINT('Ctrl Pts',(17.4217679794718,20.8776377509441,19.8033999130543));
#192334=CARTESIAN_POINT('Ctrl Pts',(17.529826925751,20.9573093523303,19.8123263237655));
#192335=CARTESIAN_POINT('Ctrl Pts',(17.7216270381622,21.0724091734604,19.8270271244417));
#192336=CARTESIAN_POINT('Ctrl Pts',(17.80144724644,21.1136540023846,19.8328476536774));
#192337=CARTESIAN_POINT('Ctrl Pts',(17.8924920045399,21.1535875654797,19.8389896565287));
#192338=CARTESIAN_POINT('Ctrl Pts',(17.9013574932526,21.1574040228163,19.8395826580494));
#192339=CARTESIAN_POINT('Ctrl Pts',(17.9144966605514,21.162954030924,19.8404537064101));
#192340=CARTESIAN_POINT('Ctrl Pts',(17.9187502547679,21.164734402634,19.8407344909505));
#192341=CARTESIAN_POINT('Ctrl Pts',(17.9263117552837,21.1678703274467,19.8412314564469));
#192342=CARTESIAN_POINT('Ctrl Pts',(17.929617307847,21.169231412355,19.841447969433));
#192343=CARTESIAN_POINT('Ctrl Pts',(17.9367125497266,21.1721319314229,19.8419111153251));
#192344=CARTESIAN_POINT('Ctrl Pts',(17.9405032468856,21.1736687530651,19.8421575900616));
#192345=CARTESIAN_POINT('Ctrl Pts',(17.9509339838556,21.1778624157423,19.8428332194433));
#192346=CARTESIAN_POINT('Ctrl Pts',(17.9575831405749,21.1804966392008,19.8432610306678));
#192347=CARTESIAN_POINT('Ctrl Pts',(17.9933579525023,21.1944603619384,19.8455480568529));
#192348=CARTESIAN_POINT('Ctrl Pts',(18.0227200880706,21.20517821939,19.8473727993063));
#192349=CARTESIAN_POINT('Ctrl Pts',(18.2073708574236,21.2679822392131,19.8585872814208));
#192350=CARTESIAN_POINT('Ctrl Pts',(18.3680441301276,21.3025551193941,19.8672421666823));
#192351=CARTESIAN_POINT('Ctrl Pts',(18.6477495096441,21.3294853917348,19.8826236758113));
#192352=CARTESIAN_POINT('Ctrl Pts',(18.7651027494354,21.3310110440876,19.8891640380702));
#192353=CARTESIAN_POINT('Ctrl Pts',(18.8962303216199,21.3218232170155,19.8968647194791));
#192354=CARTESIAN_POINT('Ctrl Pts',(18.9104790371467,21.3206797067965,19.8977064905335));
#192355=CARTESIAN_POINT('Ctrl Pts',(18.9331364609452,21.3186302271001,19.8990534126916));
#192356=CARTESIAN_POINT('Ctrl Pts',(18.9415533622446,21.3178180042235,19.8995556202262));
#192357=CARTESIAN_POINT('Ctrl Pts',(18.956388435896,21.3162966719657,19.9004441221694));
#192358=CARTESIAN_POINT('Ctrl Pts',(18.9628086892139,21.3156085801699,19.900829750119));
#192359=CARTESIAN_POINT('Ctrl Pts',(18.976080573831,21.3141247165323,19.9016292465067));
#192360=CARTESIAN_POINT('Ctrl Pts',(18.9829316571802,21.3133248097802,19.9020432410822));
#192361=CARTESIAN_POINT('Ctrl Pts',(19.0005059948045,21.3111857859422,19.9031085753757));
#192362=CARTESIAN_POINT('Ctrl Pts',(19.0112230288435,21.3097980289294,19.903761443622));
#192363=CARTESIAN_POINT('Ctrl Pts',(19.0558970773738,21.3036650139636,19.9064966551947));
#192364=CARTESIAN_POINT('Ctrl Pts',(19.0897453576836,21.2981774274413,19.9086023117608));
#192365=CARTESIAN_POINT('Ctrl Pts',(19.1775688371452,21.2817408814741,19.9141559136908));
#192366=CARTESIAN_POINT('Ctrl Pts',(19.2312738317926,21.2695040754118,19.9176422294214));
#192367=CARTESIAN_POINT('Ctrl Pts',(19.3900378934093,21.2267537787853,19.9282102873744));
#192368=CARTESIAN_POINT('Ctrl Pts',(19.4932690724207,21.1901806444038,19.9354404253612));
#192369=CARTESIAN_POINT('Ctrl Pts',(19.634390802547,21.1275114817911,19.9456404683942));
#192370=CARTESIAN_POINT('Ctrl Pts',(19.6749837641712,21.1079105393085,19.9486119402491));
#192371=CARTESIAN_POINT('Ctrl Pts',(19.7364749287004,21.0757585908294,19.9531456245587));
#192372=CARTESIAN_POINT('Ctrl Pts',(19.7578336592083,21.0641177206193,19.9547265542514));
#192373=CARTESIAN_POINT('Ctrl Pts',(19.7915869761196,21.0449598340191,19.9572299348011));
#192374=CARTESIAN_POINT('Ctrl Pts',(19.8041128999637,21.0376793051336,19.9581600680417));
#192375=CARTESIAN_POINT('Ctrl Pts',(19.8484719080412,21.0112833219707,19.9614555833422));
#192376=CARTESIAN_POINT('Ctrl Pts',(19.8798777158681,20.9914584579295,19.9637917492203));
#192377=CARTESIAN_POINT('Ctrl Pts',(19.9167022035744,20.9668347886799,19.9665197989439));
#192378=CARTESIAN_POINT('Ctrl Pts',(19.922636439096,20.9628229723573,19.9669590639339));
#192379=CARTESIAN_POINT('Ctrl Pts',(19.9322809326386,20.9562312813646,19.9676722333617));
#192380=CARTESIAN_POINT('Ctrl Pts',(19.9360034380581,20.9536695483513,19.9679473164054));
#192381=CARTESIAN_POINT('Ctrl Pts',(19.9426492444671,20.9490646488065,19.9684380578908));
#192382=CARTESIAN_POINT('Ctrl Pts',(19.9455756008995,20.9470260031171,19.9686540167094));
#192383=CARTESIAN_POINT('Ctrl Pts',(19.9518986256577,20.9425972934144,19.9691203547043));
#192384=CARTESIAN_POINT('Ctrl Pts',(19.9552934061132,20.9402046338719,19.969370552499));
#192385=CARTESIAN_POINT('Ctrl Pts',(19.964748380087,20.9334989845705,19.9700669672735));
#192386=CARTESIAN_POINT('Ctrl Pts',(19.9707929851895,20.9291639742603,19.9705117002635));
#192387=CARTESIAN_POINT('Ctrl Pts',(20.0056100942491,20.9039152356506,19.9730713354316));
#192388=CARTESIAN_POINT('Ctrl Pts',(20.03387654675,20.8823095244511,19.9751413066173));
#192389=CARTESIAN_POINT('Ctrl Pts',(20.1226969457606,20.8108014748794,19.9816669705971));
#192390=CARTESIAN_POINT('Ctrl Pts',(20.1810298673512,20.7582396210203,19.9859869949952));
#192391=CARTESIAN_POINT('Ctrl Pts',(20.3688915608898,20.5690230915093,20.0005307360924));
#192392=CARTESIAN_POINT('Ctrl Pts',(20.4830603932303,20.4184266466493,20.0105818978737));
#192393=CARTESIAN_POINT('Ctrl Pts',(20.5865933410782,20.2357262818972,20.0227986534416));
#192394=CARTESIAN_POINT('Ctrl Pts',(20.5970665410432,20.2165590740867,20.0240792321911));
#192395=CARTESIAN_POINT('Ctrl Pts',(20.6111621403572,20.1897860554178,20.0258679249136));
#192396=CARTESIAN_POINT('Ctrl Pts',(20.6150387543368,20.1823151110964,20.0263670485749));
#192397=CARTESIAN_POINT('Ctrl Pts',(20.6216328117126,20.1694196241617,20.0272286537558));
#192398=CARTESIAN_POINT('Ctrl Pts',(20.6243716967252,20.1640061148144,20.0275903770529));
#192399=CARTESIAN_POINT('Ctrl Pts',(20.6299765784718,20.1528086227341,20.0283386596843));
#192400=CARTESIAN_POINT('Ctrl Pts',(20.6328394636301,20.1470231609843,20.0287253230792));
#192401=CARTESIAN_POINT('Ctrl Pts',(20.6394509551753,20.1335071653448,20.0296287933117));
#192402=CARTESIAN_POINT('Ctrl Pts',(20.6431790309871,20.1257667664114,20.0301463084128));
#192403=CARTESIAN_POINT('Ctrl Pts',(20.6550044132437,20.1008271857208,20.0318142253026));
#192404=CARTESIAN_POINT('Ctrl Pts',(20.6629170329179,20.083541929807,20.0329709764449));
#192405=CARTESIAN_POINT('Ctrl Pts',(20.7015148573212,19.9961325578467,20.0388257950106));
#192406=CARTESIAN_POINT('Ctrl Pts',(20.72861048136,19.9244946414693,20.043644154093));
#192407=CARTESIAN_POINT('Ctrl Pts',(20.7850309776545,19.7467681221194,20.0556360630776));
#192408=CARTESIAN_POINT('Ctrl Pts',(20.8100805763456,19.6395575137347,20.0629079184764));
#192409=CARTESIAN_POINT('Ctrl Pts',(20.8373788536954,19.4609783705657,20.0748398799709));
#192410=CARTESIAN_POINT('Ctrl Pts',(20.8445566189063,19.3905648603529,20.0794962740809));
#192411=CARTESIAN_POINT('Ctrl Pts',(20.8506449076473,19.2723891232429,20.0871139899832));
#192412=CARTESIAN_POINT('Ctrl Pts',(20.8514902735322,19.2247838650631,20.0901289736452));
#192413=CARTESIAN_POINT('Ctrl Pts',(20.8506066481979,19.1694682112493,20.0935400235903));
#192414=CARTESIAN_POINT('Ctrl Pts',(20.8504411285165,19.1617501639017,20.0940138646602));
#192415=CARTESIAN_POINT('Ctrl Pts',(20.8501086334049,19.1493984864199,20.0947686451762));
#192416=CARTESIAN_POINT('Ctrl Pts',(20.8499686494859,19.144764283186,20.0950510326945));
#192417=CARTESIAN_POINT('Ctrl Pts',(20.8496933692947,19.136545772432,20.0955503727749));
#192418=CARTESIAN_POINT('Ctrl Pts',(20.8495641866245,19.1329613052336,20.0957676637308));
#192419=CARTESIAN_POINT('Ctrl Pts',(20.8492705657769,19.1253515144805,20.0962279082554));
#192420=CARTESIAN_POINT('Ctrl Pts',(20.8491037478303,19.1213263357981,20.096470727247));
#192421=CARTESIAN_POINT('Ctrl Pts',(20.8486212457494,19.1104354760286,20.097126082872));
#192422=CARTESIAN_POINT('Ctrl Pts',(20.8482836127381,19.1035707473647,20.0975374072481));
#192423=CARTESIAN_POINT('Ctrl Pts',(20.8464222024677,19.0691427258884,20.0995919961669));
#192424=CARTESIAN_POINT('Ctrl Pts',(20.844392755631,19.0416080598258,20.1012085538598));
#192425=CARTESIAN_POINT('Ctrl Pts',(20.8369190796479,18.9615940218318,20.105848778859));
#192426=CARTESIAN_POINT('Ctrl Pts',(20.8300509740369,18.9092665579418,20.1088114779129));
#192427=CARTESIAN_POINT('Ctrl Pts',(20.7977660018846,18.7187767986166,20.1195046036215));
#192428=CARTESIAN_POINT('Ctrl Pts',(20.7605765171409,18.5829843098432,20.1269707900731));
#192429=CARTESIAN_POINT('Ctrl Pts',(20.6769538441643,18.3652923313724,20.1398647528729));
#192430=CARTESIAN_POINT('Ctrl Pts',(20.6380460426288,18.2810017721445,20.1451035846945));
#192431=CARTESIAN_POINT('Ctrl Pts',(20.5871539680724,18.1874280943189,20.151347910443));
#192432=CARTESIAN_POINT('Ctrl Pts',(20.5804488810899,18.1753815414966,20.1521601887897));
#192433=CARTESIAN_POINT('Ctrl Pts',(20.5695155346613,18.1561821276042,20.1534686868267));
#192434=CARTESIAN_POINT('Ctrl Pts',(20.5653619288175,18.1489870506517,20.1539622228432));
#192435=CARTESIAN_POINT('Ctrl Pts',(20.5579168272317,18.1362638466598,20.1548406791175));
#192436=CARTESIAN_POINT('Ctrl Pts',(20.5546422631488,18.1307258958111,20.1552249813267));
#192437=CARTESIAN_POINT('Ctrl Pts',(20.5477720625339,18.1192269619934,20.1560270363756));
#192438=CARTESIAN_POINT('Ctrl Pts',(20.5441721700265,18.1132686237487,20.1564449416546));
#192439=CARTESIAN_POINT('Ctrl Pts',(20.5347581610594,18.0978593218574,20.1575317820132));
#192440=CARTESIAN_POINT('Ctrl Pts',(20.5288990662031,18.0884362117197,20.1582023663874));
#192441=CARTESIAN_POINT('Ctrl Pts',(20.5032384178612,18.0478810382046,20.1611146526714));
#192442=CARTESIAN_POINT('Ctrl Pts',(20.4826999273373,18.0172250656141,20.1633836083767));
#192443=CARTESIAN_POINT('Ctrl Pts',(20.4261259377924,17.9373769227243,20.1694794267445));
#192444=CARTESIAN_POINT('Ctrl Pts',(20.3887504048321,17.8891808210077,20.1733546605553));
#192445=CARTESIAN_POINT('Ctrl Pts',(20.2460841536001,17.7207597717741,20.1876064954377));
#192446=CARTESIAN_POINT('Ctrl Pts',(20.1293613244571,17.6109453342754,20.1983402021048));
#192447=CARTESIAN_POINT('Ctrl Pts',(19.9535183201071,17.4795155616797,20.212584583217));
#192448=CARTESIAN_POINT('Ctrl Pts',(19.9041312881027,17.4457641914325,20.2163996055444));
#192449=CARTESIAN_POINT('Ctrl Pts',(19.8457736883397,17.4094094489429,20.2206428440517));
#192450=CARTESIAN_POINT('Ctrl Pts',(19.8381401366158,17.4047210035659,20.2211928459624));
#192451=CARTESIAN_POINT('Ctrl Pts',(19.8265983438678,17.3977326680455,20.2220166028003));
#192452=CARTESIAN_POINT('Ctrl Pts',(19.8227122100215,17.3953967165732,20.2222926349463));
#192453=CARTESIAN_POINT('Ctrl Pts',(19.8157549108881,17.3912450601887,20.2227844018599));
#192454=CARTESIAN_POINT('Ctrl Pts',(19.8126866420369,17.3894246221711,20.22300044229));
#192455=CARTESIAN_POINT('Ctrl Pts',(19.8060460975571,17.3855073756232,20.2234662008151));
#192456=CARTESIAN_POINT('Ctrl Pts',(19.8024722768783,17.3834132985931,20.2237157415701));
#192457=CARTESIAN_POINT('Ctrl Pts',(19.7925074601183,17.3776136435188,20.2244084792046));
#192458=CARTESIAN_POINT('Ctrl Pts',(19.7861031076829,17.3739309676242,20.2248502174031));
#192459=CARTESIAN_POINT('Ctrl Pts',(19.7494580374532,17.3531135500383,20.2273587604739));
#192460=CARTESIAN_POINT('Ctrl Pts',(19.7188163475538,17.3366910170099,20.2293827060384));
#192461=CARTESIAN_POINT('Ctrl Pts',(19.6203559111956,17.2870025110269,20.2356997644838));
#192462=CARTESIAN_POINT('Ctrl Pts',(19.5511515493561,17.2566054018991,20.2398670157916));
#192463=CARTESIAN_POINT('Ctrl Pts',(19.3000572068204,17.1619912996553,20.2545191107828));
#192464=CARTESIAN_POINT('Ctrl Pts',(19.1112297217029,17.11897946783,20.2647930551012));
#192465=CARTESIAN_POINT('Ctrl Pts',(18.8979688673466,17.1002520111478,20.2772544091793));
#192466=CARTESIAN_POINT('Ctrl Pts',(18.8767201785455,17.098708882788,20.2785039623406));
#192467=CARTESIAN_POINT('Ctrl Pts',(18.8471370296364,17.0970088964751,20.2802560129076));
#192468=CARTESIAN_POINT('Ctrl Pts',(18.8388190312226,17.09658014081,20.2807500000378));
#192469=CARTESIAN_POINT('Ctrl Pts',(18.8244610976723,17.0959249848619,20.2816051097492));
#192470=CARTESIAN_POINT('Ctrl Pts',(18.818422283562,17.0956753424768,20.2819655005176));
#192471=CARTESIAN_POINT('Ctrl Pts',(18.8059186518273,17.0952120742832,20.2827132709647));
#192472=CARTESIAN_POINT('Ctrl Pts',(18.7994537654975,17.0950022111942,20.2831007646839));
#192473=CARTESIAN_POINT('Ctrl Pts',(18.7843172615155,17.0945802839226,20.2840100903042));
#192474=CARTESIAN_POINT('Ctrl Pts',(18.7756451482221,17.0943918833336,20.2845326583244));
#192475=CARTESIAN_POINT('Ctrl Pts',(18.7475081826927,17.0939535976432,20.2862334359272));
#192476=CARTESIAN_POINT('Ctrl Pts',(18.7280414207869,17.0939188970806,20.2874183505551));
#192477=CARTESIAN_POINT('Ctrl Pts',(18.6285949667789,17.0951132122844,20.29351518871));
#192478=CARTESIAN_POINT('Ctrl Pts',(18.5487404276439,17.1006058582918,20.2985588631999));
#192479=CARTESIAN_POINT('Ctrl Pts',(18.3723972888642,17.1228212624269,20.3100131654662));
#192480=CARTESIAN_POINT('Ctrl Pts',(18.2763681228698,17.141744676083,20.3164671589653));
#192481=CARTESIAN_POINT('Ctrl Pts',(18.0612387107882,17.1998491680736,20.3311923030113));
#192482=CARTESIAN_POINT('Ctrl Pts',(17.9435941958999,17.2431074206821,20.3394426661579));
#192483=CARTESIAN_POINT('Ctrl Pts',(17.8219457184588,17.3005198555948,20.3477493475554));
#192484=CARTESIAN_POINT('Ctrl Pts',(17.8134698778202,17.3045893159384,20.3483268093222));
#192485=CARTESIAN_POINT('Ctrl Pts',(17.8009218382442,17.3107171376273,20.3491794559844));
#192486=CARTESIAN_POINT('Ctrl Pts',(17.7968288621003,17.3127323497037,20.3494572174077));
#192487=CARTESIAN_POINT('Ctrl Pts',(17.7895445854272,17.3163481281665,20.3499508664201));
#192488=CARTESIAN_POINT('Ctrl Pts',(17.78635079617,17.317943547413,20.3501670692646));
#192489=CARTESIAN_POINT('Ctrl Pts',(17.7795515706867,17.321361538303,20.3506268270691));
#192490=CARTESIAN_POINT('Ctrl Pts',(17.775947323457,17.3231863466594,20.3508702389337));
#192491=CARTESIAN_POINT('Ctrl Pts',(17.7660977018342,17.3282086231039,20.3515346566113));
#192492=CARTESIAN_POINT('Ctrl Pts',(17.759862899825,17.331426872689,20.3519543782937));
#192493=CARTESIAN_POINT('Ctrl Pts',(17.7459578152103,17.3386921063875,20.3528887991308));
#192494=CARTESIAN_POINT('Ctrl Pts',(17.7382961244232,17.3427553679701,20.3534025287024));
#192495=CARTESIAN_POINT('Ctrl Pts',(17.7147287723702,17.3554401187007,20.3549799132406));
#192496=CARTESIAN_POINT('Ctrl Pts',(17.6989080902324,17.3642187212862,20.3560347793412));
#192497=CARTESIAN_POINT('Ctrl Pts',(17.6383226561558,17.398859633915,20.3600663122138));
#192498=CARTESIAN_POINT('Ctrl Pts',(17.5943958034201,17.4261569971446,20.3629722905541));
#192499=CARTESIAN_POINT('Ctrl Pts',(17.4369736985797,17.5321672644307,20.3734853469438));
#192500=CARTESIAN_POINT('Ctrl Pts',(17.3302571194892,17.6203193537634,20.3808298521585));
#192501=CARTESIAN_POINT('Ctrl Pts',(17.2120043418183,17.7392340795373,20.3900862402313));
#192502=CARTESIAN_POINT('Ctrl Pts',(17.1915692349662,17.760664534775,20.3917311305545));
#192503=CARTESIAN_POINT('Ctrl Pts',(17.1571320820595,17.798330288426,20.3945912674749));
#192504=CARTESIAN_POINT('Ctrl Pts',(17.1429146323016,17.8143628033448,20.3957994704802));
#192505=CARTESIAN_POINT('Ctrl Pts',(17.0965111966335,17.8683185987888,20.3998406338136));
#192506=CARTESIAN_POINT('Ctrl Pts',(17.0654202744549,17.9071579633068,20.4027101610731));
#192507=CARTESIAN_POINT('Ctrl Pts',(17.0281429210351,17.9572448386846,20.40638173292));
#192508=CARTESIAN_POINT('Ctrl Pts',(17.020650371766,17.9675035507768,20.4071322401939));
#192509=CARTESIAN_POINT('Ctrl Pts',(17.0089449006436,17.9838371975018,20.4083251152093));
#192510=CARTESIAN_POINT('Ctrl Pts',(17.004670615591,17.9898679359931,20.4087651114938));
#192511=CARTESIAN_POINT('Ctrl Pts',(16.9967775819607,18.0011290477236,20.4095859554126));
#192512=CARTESIAN_POINT('Ctrl Pts',(16.9931506404327,18.0063535967648,20.4099664834204));
#192513=CARTESIAN_POINT('Ctrl Pts',(16.985162515901,18.0179717723015,20.4108120677589));
#192514=CARTESIAN_POINT('Ctrl Pts',(16.9808127554928,18.0243731078845,20.4112775510116));
#192515=CARTESIAN_POINT('Ctrl Pts',(16.9683214435626,18.0429745882338,20.4126290795128));
#192516=CARTESIAN_POINT('Ctrl Pts',(16.9602715797871,18.0552354904494,20.4135185545034));
#192517=CARTESIAN_POINT('Ctrl Pts',(16.8994020535194,18.1500808520732,20.4203899755883));
#192518=CARTESIAN_POINT('Ctrl Pts',(16.8522561196807,18.2361490912158,20.4265808788633));
#192519=CARTESIAN_POINT('Ctrl Pts',(16.7513598311468,18.4551496144258,20.4421983674838));
#192520=CARTESIAN_POINT('Ctrl Pts',(16.7048136308439,18.5908626529497,20.4517799896776));
#192521=CARTESIAN_POINT('Ctrl Pts',(16.6660226853087,18.75720883082,20.4629186771635));
#192522=CARTESIAN_POINT('Ctrl Pts',(16.6602607809698,18.7843123468051,20.4647138075176));
#192523=CARTESIAN_POINT('Ctrl Pts',(16.6468711365671,18.8539948770933,20.4692668138028));
#192524=CARTESIAN_POINT('Ctrl Pts',(16.6400127083412,18.8967113399598,20.4719989740541));
#192525=CARTESIAN_POINT('Ctrl Pts',(16.6335056830049,18.9470513191892,20.4751271756401));
#192526=CARTESIAN_POINT('Ctrl Pts',(16.6325834879834,18.9544967277273,20.4755875030988));
#192527=CARTESIAN_POINT('Ctrl Pts',(16.6311572014184,18.9665362577807,20.4763279181513));
#192528=CARTESIAN_POINT('Ctrl Pts',(16.6306285495627,18.9711273270536,20.47660933514));
#192529=CARTESIAN_POINT('Ctrl Pts',(16.6297175168382,18.9792738303376,20.4771069988277));
#192530=CARTESIAN_POINT('Ctrl Pts',(16.6293291064467,18.9828285356172,20.4773235810695));
#192531=CARTESIAN_POINT('Ctrl Pts',(16.6285936556295,18.9897210230322,20.4777424113166));
#192532=CARTESIAN_POINT('Ctrl Pts',(16.6282455464677,18.9930586263391,20.4779447207648));
#192533=CARTESIAN_POINT('Ctrl Pts',(16.6274962892663,19.0004117718269,20.4783893508548));
#192534=CARTESIAN_POINT('Ctrl Pts',(16.6270986830446,19.0044276727148,20.4786314740247));
#192535=CARTESIAN_POINT('Ctrl Pts',(16.6261439843123,19.0143598980449,20.4792285971133));
#192536=CARTESIAN_POINT('Ctrl Pts',(16.6256003107858,19.0202775184922,20.4795828709947));
#192537=CARTESIAN_POINT('Ctrl Pts',(16.6234160991776,19.045203167999,20.4810691240488));
#192538=CARTESIAN_POINT('Ctrl Pts',(16.6220075782698,19.0642312782726,20.4821890740203));
#192539=CARTESIAN_POINT('Ctrl Pts',(16.618313691022,19.1253454546686,20.485746544444));
#192540=CARTESIAN_POINT('Ctrl Pts',(16.617027658706,19.167483096034,20.488139347873));
#192541=CARTESIAN_POINT('Ctrl Pts',(16.6170004413563,19.2096329951322,20.4904971933207));
#192542=CARTESIAN_POINT('Ctrl Pts',(16.7454193623258,19.9371102171621,20.5336910458214));
#192543=CARTESIAN_POINT('Ctrl Pts',(16.7207024854735,19.8694186993037,20.5293719537179));
#192544=CARTESIAN_POINT('Ctrl Pts',(16.6994546553919,19.8004872844824,20.5250528616144));
#192545=CARTESIAN_POINT('Ctrl Pts',(16.6817841755687,19.7307106983252,20.5207337695109));
#192546=CARTESIAN_POINT('Ctrl Pts',(16.664105969176,19.6609036017547,20.5164127888472));
#192547=CARTESIAN_POINT('Ctrl Pts',(16.6500083234449,19.5902510850496,20.5120918081835));
#192548=CARTESIAN_POINT('Ctrl Pts',(16.6395483092999,19.5191576144172,20.5077708275198));
#192549=CARTESIAN_POINT('Ctrl Pts',(16.6290728051449,19.4479588629934,20.5034434480088));
#192550=CARTESIAN_POINT('Ctrl Pts',(16.6222457279572,19.3763183482269,20.4991160684978));
#192551=CARTESIAN_POINT('Ctrl Pts',(16.6190721590219,19.3046441533458,20.4947886889867));
#192552=CARTESIAN_POINT('Ctrl Pts',(16.6176708338065,19.2729956028858,20.4928778856768));
#192553=CARTESIAN_POINT('Ctrl Pts',(16.6169811726879,19.2413404642854,20.4909670823669));
#192554=CARTESIAN_POINT('Ctrl Pts',(16.6170003908425,19.209713599163,20.489056279057));
#192555=CARTESIAN_POINT('Origin',(18.734,19.211,0.));
#192556=CARTESIAN_POINT('',(16.7454193623258,19.9371102171621,21.5555703650724));
#192557=CARTESIAN_POINT('',(16.7454193623258,19.9371102171621,21.3335535344094));
#192558=CARTESIAN_POINT('',(16.7454193623258,19.9371102171621,0.));
#192559=CARTESIAN_POINT('',(16.617000615865,19.2093852021581,21.5109437210328));
#192560=CARTESIAN_POINT('Ctrl Pts',(16.617000615865,19.2093852021581,21.5109437210328));
#192561=CARTESIAN_POINT('Ctrl Pts',(16.616945967273,19.2810294864738,21.5152671813527));
#192562=CARTESIAN_POINT('Ctrl Pts',(16.6205324536961,19.3528082880785,21.5195906416726));
#192563=CARTESIAN_POINT('Ctrl Pts',(16.6277745362619,19.424315015649,21.5239141019925));
#192564=CARTESIAN_POINT('Ctrl Pts',(16.6350090203951,19.4957467179695,21.5282330261142));
#192565=CARTESIAN_POINT('Ctrl Pts',(16.6458914490245,19.5669064212152,21.5325519502359));
#192566=CARTESIAN_POINT('Ctrl Pts',(16.6603842611256,19.6373880480177,21.5368708743575));
#192567=CARTESIAN_POINT('Ctrl Pts',(16.6748666461647,19.7078189658007,21.5411866911672));
#192568=CARTESIAN_POINT('Ctrl Pts',(16.6929541627611,19.7775722897502,21.5455025079768));
#192569=CARTESIAN_POINT('Ctrl Pts',(16.7145577235046,19.8462494721786,21.5498183247864));
#192570=CARTESIAN_POINT('Ctrl Pts',(16.7241553313425,19.8767600288495,21.5517356715484));
#192571=CARTESIAN_POINT('Ctrl Pts',(16.734446215425,19.9070583229105,21.5536530183104));
#192572=CARTESIAN_POINT('Ctrl Pts',(16.7454193623258,19.9371102171621,21.5555703650724));
#192573=CARTESIAN_POINT('Ctrl Pts',(16.6170005689228,19.209447963039,21.5099894604535));
#192574=CARTESIAN_POINT('Ctrl Pts',(16.6170514760726,19.1400099213996,21.5054225788889));
#192575=CARTESIAN_POINT('Ctrl Pts',(16.6205187490176,19.0706094573942,21.500900893449));
#192576=CARTESIAN_POINT('Ctrl Pts',(16.6297026242345,18.9782623033322,21.4950376253733));
#192577=CARTESIAN_POINT('Ctrl Pts',(16.6323979093154,18.9550643922718,21.493577929973));
#192578=CARTESIAN_POINT('Ctrl Pts',(16.636285362927,18.9258334914824,21.491759204291));
#192579=CARTESIAN_POINT('Ctrl Pts',(16.6371205628695,18.919755662051,21.4913821743009));
#192580=CARTESIAN_POINT('Ctrl Pts',(16.6385604188819,18.9096050541681,21.4907544778988));
#192581=CARTESIAN_POINT('Ctrl Pts',(16.6391505510601,18.9055302986921,21.490503036672));
#192582=CARTESIAN_POINT('Ctrl Pts',(16.6402462936381,18.8981169249711,21.4900465848008));
#192583=CARTESIAN_POINT('Ctrl Pts',(16.6407480096755,18.8947777570839,21.4898413593182));
#192584=CARTESIAN_POINT('Ctrl Pts',(16.6417946532316,18.8879234771462,21.4894208785397));
#192585=CARTESIAN_POINT('Ctrl Pts',(16.642340448676,18.8844085510559,21.4892056795509));
#192586=CARTESIAN_POINT('Ctrl Pts',(16.6435934062289,18.8764714851954,21.4887207018444));
#192587=CARTESIAN_POINT('Ctrl Pts',(16.6443057399722,18.8720502176448,21.4884512204746));
#192588=CARTESIAN_POINT('Ctrl Pts',(16.646501210917,18.8586935344663,21.4876390532523));
#192589=CARTESIAN_POINT('Ctrl Pts',(16.6480276910177,18.849765210832,21.4870987813851));
#192590=CARTESIAN_POINT('Ctrl Pts',(16.6601845708611,18.7813079893189,21.4829745480576));
#192591=CARTESIAN_POINT('Ctrl Pts',(16.6733049262745,18.722243505688,21.479522065513));
#192592=CARTESIAN_POINT('Ctrl Pts',(16.69382332133,18.6455573540763,21.4750843617421));
#192593=CARTESIAN_POINT('Ctrl Pts',(16.698953221487,18.6273640674337,21.4740349431003));
#192594=CARTESIAN_POINT('Ctrl Pts',(16.7159623154871,18.5699940119783,21.4707298273629));
#192595=CARTESIAN_POINT('Ctrl Pts',(16.7287346785616,18.5310912410399,21.4684945740175));
#192596=CARTESIAN_POINT('Ctrl Pts',(16.7545783257699,18.4594555531082,21.4643518724571));
#192597=CARTESIAN_POINT('Ctrl Pts',(16.7673541440347,18.4266319018062,21.4624429597118));
#192598=CARTESIAN_POINT('Ctrl Pts',(16.8090251671684,18.3269990333951,21.4565793428602));
#192599=CARTESIAN_POINT('Ctrl Pts',(16.8405503212018,18.2613508689022,21.4526165738847));
#192600=CARTESIAN_POINT('Ctrl Pts',(16.901831238818,18.1489753810926,21.4455036084311));
#192601=CARTESIAN_POINT('Ctrl Pts',(16.9301556402399,18.1015480928942,21.4423912319948));
#192602=CARTESIAN_POINT('Ctrl Pts',(16.9790290475463,18.0265410883997,21.4372424455897));
#192603=CARTESIAN_POINT('Ctrl Pts',(16.9984529420148,17.9982584079703,21.4352459079393));
#192604=CARTESIAN_POINT('Ctrl Pts',(17.0248610484141,17.9617406739852,21.4325885592976));
#192605=CARTESIAN_POINT('Ctrl Pts',(17.0312337451873,17.9530684063029,21.4319514421578));
#192606=CARTESIAN_POINT('Ctrl Pts',(17.0417740500905,17.9389515180439,21.4309041982852));
#192607=CARTESIAN_POINT('Ctrl Pts',(17.0459025254163,17.9334778199235,21.4304956127586));
#192608=CARTESIAN_POINT('Ctrl Pts',(17.0539413443128,17.9229266386452,21.4297030642932));
#192609=CARTESIAN_POINT('Ctrl Pts',(17.0578483025536,17.9178466616372,21.4293192384062));
#192610=CARTESIAN_POINT('Ctrl Pts',(17.066916242911,17.9061663144368,21.4284314703004));
#192611=CARTESIAN_POINT('Ctrl Pts',(17.0720934375547,17.8995787196105,21.4279268822287));
#192612=CARTESIAN_POINT('Ctrl Pts',(17.0861067058682,17.8819641238223,21.426567050121));
#192613=CARTESIAN_POINT('Ctrl Pts',(17.095014187257,17.8709947166758,21.4257089298295));
#192614=CARTESIAN_POINT('Ctrl Pts',(17.1997103751384,17.7446689066322,21.415692898114));
#192615=CARTESIAN_POINT('Ctrl Pts',(17.3073653772947,17.6397364542029,21.4060185248015));
#192616=CARTESIAN_POINT('Ctrl Pts',(17.4998881917639,17.4883007393238,21.3898623514561));
#192617=CARTESIAN_POINT('Ctrl Pts',(17.5784750964082,17.4346308209117,21.3835372371883));
#192618=CARTESIAN_POINT('Ctrl Pts',(17.6991993323576,17.3635956643708,21.3744154557351));
#192619=CARTESIAN_POINT('Ctrl Pts',(17.738715759255,17.3420096294588,21.3715176022211));
#192620=CARTESIAN_POINT('Ctrl Pts',(17.800914836807,17.3105658415141,21.3671223586442));
#192621=CARTESIAN_POINT('Ctrl Pts',(17.8231310027739,17.2998182434774,21.3655842077384));
#192622=CARTESIAN_POINT('Ctrl Pts',(17.8514871251667,17.2867071210671,21.3636655049593));
#192623=CARTESIAN_POINT('Ctrl Pts',(17.8574560074017,17.283980879744,21.3632640922076));
#192624=CARTESIAN_POINT('Ctrl Pts',(17.8664996722272,17.2799009693489,21.362659730934));
#192625=CARTESIAN_POINT('Ctrl Pts',(17.8695650933016,17.2785268236494,21.3624555410055));
#192626=CARTESIAN_POINT('Ctrl Pts',(17.8758766949369,17.2757155257917,21.3620365029449));
#192627=CARTESIAN_POINT('Ctrl Pts',(17.8791231719923,17.2742792633185,21.3618217173134));
#192628=CARTESIAN_POINT('Ctrl Pts',(17.8864141131182,17.2710756084496,21.3613410179091));
#192629=CARTESIAN_POINT('Ctrl Pts',(17.8904604959507,17.2693126960055,21.3610753803063));
#192630=CARTESIAN_POINT('Ctrl Pts',(17.9007717155665,17.2648586599681,21.3604013040124));
#192631=CARTESIAN_POINT('Ctrl Pts',(17.9070441483551,17.262185100722,21.3599939118205));
#192632=CARTESIAN_POINT('Ctrl Pts',(17.9427390879267,17.2471738720776,21.3576899943043));
#192633=CARTESIAN_POINT('Ctrl Pts',(17.9724263216596,17.2354715465259,21.3558294456741));
#192634=CARTESIAN_POINT('Ctrl Pts',(18.1885431807815,17.1558775597884,21.3426052557944));
#192635=CARTESIAN_POINT('Ctrl Pts',(18.3834491892948,17.1138150096998,21.3322947095244));
#192636=CARTESIAN_POINT('Ctrl Pts',(18.6371249752938,17.0954792997304,21.3181606270837));
#192637=CARTESIAN_POINT('Ctrl Pts',(18.6930030125068,17.093659408102,21.31501078714));
#192638=CARTESIAN_POINT('Ctrl Pts',(18.7835678678964,17.0942961952381,21.3098016666273));
#192639=CARTESIAN_POINT('Ctrl Pts',(18.8182380614379,17.0953923527782,21.3077829835726));
#192640=CARTESIAN_POINT('Ctrl Pts',(18.8637157581176,17.097949847093,21.3050967408519));
#192641=CARTESIAN_POINT('Ctrl Pts',(18.8745622019997,17.0986436410209,21.3044532160136));
#192642=CARTESIAN_POINT('Ctrl Pts',(18.8923074836142,17.0999159983177,21.3033955234311));
#192643=CARTESIAN_POINT('Ctrl Pts',(18.8992097611708,17.1004449415865,21.302982915038));
#192644=CARTESIAN_POINT('Ctrl Pts',(18.9125579805265,17.1015337380506,21.3021825985309));
#192645=CARTESIAN_POINT('Ctrl Pts',(18.9190042014731,17.1020893080285,21.3017950291851));
#192646=CARTESIAN_POINT('Ctrl Pts',(18.9338717259933,17.1034393621586,21.3008986184457));
#192647=CARTESIAN_POINT('Ctrl Pts',(18.9422909751693,17.1042547815511,21.3003891248679));
#192648=CARTESIAN_POINT('Ctrl Pts',(18.9648973958348,17.1065810899074,21.299015965141));
#192649=CARTESIAN_POINT('Ctrl Pts',(18.9790743668384,17.1081849592323,21.298149394373));
#192650=CARTESIAN_POINT('Ctrl Pts',(19.1068141531769,17.1239457375089,21.2902909631835));
#192651=CARTESIAN_POINT('Ctrl Pts',(19.2190528723219,17.1471438329611,21.2830110919086));
#192652=CARTESIAN_POINT('Ctrl Pts',(19.485928557976,17.2252809449586,21.2648702335341));
#192653=CARTESIAN_POINT('Ctrl Pts',(19.637136158265,17.2893284635313,21.2538526756614));
#192654=CARTESIAN_POINT('Ctrl Pts',(19.8079500251652,17.3863372344162,21.2413706015328));
#192655=CARTESIAN_POINT('Ctrl Pts',(19.8360674661234,17.4031807507792,21.2393166943286));
#192656=CARTESIAN_POINT('Ctrl Pts',(19.8699388353069,17.4245552270992,21.2368538794387));
#192657=CARTESIAN_POINT('Ctrl Pts',(19.8760735153067,17.4284708828906,21.236408290736));
#192658=CARTESIAN_POINT('Ctrl Pts',(19.8856566304435,17.4346573947448,21.2357131167827));
#192659=CARTESIAN_POINT('Ctrl Pts',(19.8891187550593,17.4369067927334,21.2354621522318));
#192660=CARTESIAN_POINT('Ctrl Pts',(19.895571236487,17.4411259693614,21.2349947972675));
#192661=CARTESIAN_POINT('Ctrl Pts',(19.8985631502955,17.4430931893779,21.234778247877));
#192662=CARTESIAN_POINT('Ctrl Pts',(19.9053763775538,17.4475977708323,21.2342854623733));
#192663=CARTESIAN_POINT('Ctrl Pts',(19.9091944350792,17.4501399600222,21.2340095540906));
#192664=CARTESIAN_POINT('Ctrl Pts',(19.9209018395014,17.4579901771666,21.2331641804027));
#192665=CARTESIAN_POINT('Ctrl Pts',(19.9287638362217,17.463339049233,21.2325973896085));
#192666=CARTESIAN_POINT('Ctrl Pts',(19.9989653003663,17.5117954202825,21.2275420480878));
#192667=CARTESIAN_POINT('Ctrl Pts',(20.0589911033888,17.5581737594304,21.2232589859039));
#192668=CARTESIAN_POINT('Ctrl Pts',(20.2235805178994,17.7000848672498,21.2112288497494));
#192669=CARTESIAN_POINT('Ctrl Pts',(20.3212210737501,17.8030063055925,21.2037065280896));
#192670=CARTESIAN_POINT('Ctrl Pts',(20.4457142238262,17.9637849230438,21.1924562739161));
#192671=CARTESIAN_POINT('Ctrl Pts',(20.4814021715165,18.0142979381967,21.1889868950583));
#192672=CARTESIAN_POINT('Ctrl Pts',(20.534976655748,18.0976443868653,21.1833006114781));
#192673=CARTESIAN_POINT('Ctrl Pts',(20.5542940631699,18.1295163386221,21.1811348534304));
#192674=CARTESIAN_POINT('Ctrl Pts',(20.5782796385727,18.1715551038524,21.1782817014748));
#192675=CARTESIAN_POINT('Ctrl Pts',(20.5837232566918,18.1812733644952,21.1776223762077));
#192676=CARTESIAN_POINT('Ctrl Pts',(20.5924495240457,18.1971444914772,21.1765458225672));
#192677=CARTESIAN_POINT('Ctrl Pts',(20.5957789560666,18.2032714936313,21.1761302720609));
#192678=CARTESIAN_POINT('Ctrl Pts',(20.6021221885369,18.2150833926388,21.1753292011754));
#192679=CARTESIAN_POINT('Ctrl Pts',(20.6051404656764,18.2207658072893,21.1749438456728));
#192680=CARTESIAN_POINT('Ctrl Pts',(20.6119901938784,18.2338047128863,21.1740596096595));
#192681=CARTESIAN_POINT('Ctrl Pts',(20.6158043914032,18.2411701041421,21.1735601263266));
#192682=CARTESIAN_POINT('Ctrl Pts',(20.6258186637318,18.260789630425,21.1722295424782));
#192683=CARTESIAN_POINT('Ctrl Pts',(20.6319428699606,18.2730818525524,21.1713957996083));
#192684=CARTESIAN_POINT('Ctrl Pts',(20.6774819003258,18.3667583305714,21.1650403574053));
#192685=CARTESIAN_POINT('Ctrl Pts',(20.7117604860588,18.4505227738403,21.1593418085756));
#192686=CARTESIAN_POINT('Ctrl Pts',(20.7851815471082,18.6688508430694,21.1444683312998));
#192687=CARTESIAN_POINT('Ctrl Pts',(20.8165229424175,18.8055808664268,21.1351170671379));
#192688=CARTESIAN_POINT('Ctrl Pts',(20.8410811064594,18.9990281702302,21.1223461872799));
#192689=CARTESIAN_POINT('Ctrl Pts',(20.8458832238423,19.053923819165,21.1187767409162));
#192690=CARTESIAN_POINT('Ctrl Pts',(20.8499084724558,19.1373275542845,21.1134918611606));
#192691=CARTESIAN_POINT('Ctrl Pts',(20.8507067453712,19.1657337773155,21.1117162147408));
#192692=CARTESIAN_POINT('Ctrl Pts',(20.8509881545861,19.2010862737162,21.1095435926542));
#192693=CARTESIAN_POINT('Ctrl Pts',(20.8510092759326,19.2080238748373,21.1091190200358));
#192694=CARTESIAN_POINT('Ctrl Pts',(20.8509887283658,19.2190041639062,21.108449997686));
#192695=CARTESIAN_POINT('Ctrl Pts',(20.8509695837611,19.2230467726219,21.1082043185368));
#192696=CARTESIAN_POINT('Ctrl Pts',(20.8509116410095,19.2306705320514,21.1077422325926));
#192697=CARTESIAN_POINT('Ctrl Pts',(20.8508753362383,19.23425159541,21.1075256948778));
#192698=CARTESIAN_POINT('Ctrl Pts',(20.8507715511013,19.242439219687,21.107031768043));
#192699=CARTESIAN_POINT('Ctrl Pts',(20.850698121036,19.2470456572814,21.1067547148771));
#192700=CARTESIAN_POINT('Ctrl Pts',(20.8504631980617,19.2592773272236,21.1060211746422));
#192701=CARTESIAN_POINT('Ctrl Pts',(20.8502755330337,19.2669020690511,21.1055661137596));
#192702=CARTESIAN_POINT('Ctrl Pts',(20.8486704995668,19.3203658250186,21.1023896725936));
#192703=CARTESIAN_POINT('Ctrl Pts',(20.8458050291108,19.3661528295392,21.0997434624873));
#192704=CARTESIAN_POINT('Ctrl Pts',(20.8378766748003,19.4493573627226,21.0950121637234));
#192705=CARTESIAN_POINT('Ctrl Pts',(20.8332965336635,19.4867999089902,21.0929118339656));
#192706=CARTESIAN_POINT('Ctrl Pts',(20.8083604781842,19.6535479897378,21.0836115746201));
#192707=CARTESIAN_POINT('Ctrl Pts',(20.777039847047,19.7809208510916,21.0766341036281));
#192708=CARTESIAN_POINT('Ctrl Pts',(20.7052145667264,19.9880492344194,21.0645333293891));
#192709=CARTESIAN_POINT('Ctrl Pts',(20.6710806061883,20.069608490702,21.05956122565));
#192710=CARTESIAN_POINT('Ctrl Pts',(20.6228634555686,20.1671930277235,21.0532176312391));
#192711=CARTESIAN_POINT('Ctrl Pts',(20.6135045550156,20.185460283434,21.0520126115572));
#192712=CARTESIAN_POINT('Ctrl Pts',(20.5997293509222,20.2114106273785,21.0502742603882));
#192713=CARTESIAN_POINT('Ctrl Pts',(20.5955279349911,20.2192069122344,21.0497485338322));
#192714=CARTESIAN_POINT('Ctrl Pts',(20.5881610574298,20.2326740915707,21.0488342642214));
#192715=CARTESIAN_POINT('Ctrl Pts',(20.5850181696237,20.2383572458244,21.0484465314966));
#192716=CARTESIAN_POINT('Ctrl Pts',(20.5789259099609,20.2492549186532,21.0476993172978));
#192717=CARTESIAN_POINT('Ctrl Pts',(20.5759804522534,20.254471562488,21.0473399793536));
#192718=CARTESIAN_POINT('Ctrl Pts',(20.5682085306612,20.2681008147428,21.0463967827888));
#192719=CARTESIAN_POINT('Ctrl Pts',(20.5633463682453,20.2764928092513,21.0458116367754));
#192720=CARTESIAN_POINT('Ctrl Pts',(20.5462830669485,20.3054826263244,21.043774809955));
#192721=CARTESIAN_POINT('Ctrl Pts',(20.5337906762122,20.325906086627,21.0423125560804));
#192722=CARTESIAN_POINT('Ctrl Pts',(20.437687778471,20.477196403204,21.0312701560227));
#192723=CARTESIAN_POINT('Ctrl Pts',(20.3402647137796,20.5986968239619,21.0211538266253));
#192724=CARTESIAN_POINT('Ctrl Pts',(20.1778790644151,20.7609766117255,21.0059869580296));
#192725=CARTESIAN_POINT('Ctrl Pts',(20.1225691328863,20.8107157759639,21.0010639088933));
#192726=CARTESIAN_POINT('Ctrl Pts',(20.0289987656021,20.8863450692377,20.9932278344425));
#192727=CARTESIAN_POINT('Ctrl Pts',(19.9923066925104,20.9140759575389,20.9902670127103));
#192728=CARTESIAN_POINT('Ctrl Pts',(19.9410819425929,20.9502301708068,20.986312332158));
#192729=CARTESIAN_POINT('Ctrl Pts',(19.92731134,20.959707089788,20.9852661621551));
#192730=CARTESIAN_POINT('Ctrl Pts',(19.9035328193865,20.9756597439225,20.9834904436081));
#192731=CARTESIAN_POINT('Ctrl Pts',(19.893579995448,20.9822157622976,20.9827562488977));
#192732=CARTESIAN_POINT('Ctrl Pts',(19.8793558083444,20.9914140763217,20.9817203715126));
#192733=CARTESIAN_POINT('Ctrl Pts',(19.875129800612,20.9941256237914,20.9814142770875));
#192734=CARTESIAN_POINT('Ctrl Pts',(19.8678311471682,20.9987721090739,20.9808885453356));
#192735=CARTESIAN_POINT('Ctrl Pts',(19.8647631118735,21.0007142145842,20.9806684349348));
#192736=CARTESIAN_POINT('Ctrl Pts',(19.8588032234887,21.0044654564925,20.9802425849374));
#192737=CARTESIAN_POINT('Ctrl Pts',(19.8559119978918,21.0062754954517,20.9800367823656));
#192738=CARTESIAN_POINT('Ctrl Pts',(19.8481023485937,21.011138457909,20.9794829514067));
#192739=CARTESIAN_POINT('Ctrl Pts',(19.8431757149041,21.0141782346854,20.9791357841421));
#192740=CARTESIAN_POINT('Ctrl Pts',(19.8248600813388,21.0253756755394,20.9778530679902));
#192741=CARTESIAN_POINT('Ctrl Pts',(19.8113926771083,21.0334049661969,20.9769255568403));
#192742=CARTESIAN_POINT('Ctrl Pts',(19.6817603879085,21.1087526156303,20.9681342432055));
#192743=CARTESIAN_POINT('Ctrl Pts',(19.5595120547503,21.1650354409874,20.9608717268428));
#192744=CARTESIAN_POINT('Ctrl Pts',(19.2810476021562,21.2624024974086,20.9448519793377));
#192745=CARTESIAN_POINT('Ctrl Pts',(19.1238298381548,21.2979925293925,20.9361046021643));
#192746=CARTESIAN_POINT('Ctrl Pts',(18.9455576821849,21.3174853595901,20.925631613753));
#192747=CARTESIAN_POINT('Ctrl Pts',(18.9269819602058,21.3192682829984,20.9245344899101));
#192748=CARTESIAN_POINT('Ctrl Pts',(18.8998852282073,21.3215079577503,20.9229246643101));
#192749=CARTESIAN_POINT('Ctrl Pts',(18.8913808605586,21.3221591626752,20.9224180679968));
#192750=CARTESIAN_POINT('Ctrl Pts',(18.8764413407627,21.3232123555081,20.9215256795755));
#192751=CARTESIAN_POINT('Ctrl Pts',(18.8700078158853,21.3236363726203,20.9211405841363));
#192752=CARTESIAN_POINT('Ctrl Pts',(18.8574952526817,21.3244036515734,20.9203900205283));
#192753=CARTESIAN_POINT('Ctrl Pts',(18.8514164671774,21.3247500902306,20.9200246560614));
#192754=CARTESIAN_POINT('Ctrl Pts',(18.8368546841907,21.3255169783241,20.9191476392207));
#192755=CARTESIAN_POINT('Ctrl Pts',(18.8283705349422,21.3259126073027,20.9186352131181));
#192756=CARTESIAN_POINT('Ctrl Pts',(18.7975861841148,21.3271625231008,20.9167705151548));
#192757=CARTESIAN_POINT('Ctrl Pts',(18.7752758197653,21.3277152084991,20.915408848518));
#192758=CARTESIAN_POINT('Ctrl Pts',(18.5696370345954,21.3295571469673,20.9027594061675));
#192759=CARTESIAN_POINT('Ctrl Pts',(18.386908382201,21.3073779179333,20.8906947602941));
#192760=CARTESIAN_POINT('Ctrl Pts',(18.1303749379129,21.2417569008552,20.8732106831505));
#192761=CARTESIAN_POINT('Ctrl Pts',(18.0526120479145,21.2170032458207,20.8678505622162));
#192762=CARTESIAN_POINT('Ctrl Pts',(17.9424737730587,21.1747974520506,20.8603296315121));
#192763=CARTESIAN_POINT('Ctrl Pts',(17.9088201110924,21.1608955664088,20.8580419950872));
#192764=CARTESIAN_POINT('Ctrl Pts',(17.868691236688,21.143093650157,20.8553410489813));
#192765=CARTESIAN_POINT('Ctrl Pts',(17.8618589949675,21.1400192326766,20.8548821489732));
#192766=CARTESIAN_POINT('Ctrl Pts',(17.8512527076488,21.1351786760659,20.8541714152479));
#192767=CARTESIAN_POINT('Ctrl Pts',(17.8474673905208,21.1334375913408,20.8539180889712));
#192768=CARTESIAN_POINT('Ctrl Pts',(17.8404512609386,21.1301853407585,20.8534491934583));
#192769=CARTESIAN_POINT('Ctrl Pts',(17.8372191560386,21.1286771989723,20.8532334482913));
#192770=CARTESIAN_POINT('Ctrl Pts',(17.8299130095227,21.1252455460227,20.852746334506));
#192771=CARTESIAN_POINT('Ctrl Pts',(17.8258412984364,21.1233171992257,20.8524752689658));
#192772=CARTESIAN_POINT('Ctrl Pts',(17.8135516410723,21.1174487604509,20.8516582382603));
#192773=CARTESIAN_POINT('Ctrl Pts',(17.8053528288313,21.1134685269139,20.8511146998513));
#192774=CARTESIAN_POINT('Ctrl Pts',(17.7424061816535,21.0824062688924,20.8469515340594));
#192775=CARTESIAN_POINT('Ctrl Pts',(17.6888224192078,21.0530165623255,20.8434650796795));
#192776=CARTESIAN_POINT('Ctrl Pts',(17.4971412875124,20.9368208088771,20.8309358219835));
#192777=CARTESIAN_POINT('Ctrl Pts',(17.3679309893915,20.8364655076265,20.8223347994012));
#192778=CARTESIAN_POINT('Ctrl Pts',(17.1948920375277,20.6667222325276,20.8088862591062));
#192779=CARTESIAN_POINT('Ctrl Pts',(17.1414400752061,20.608043829206,20.8043989483772));
#192780=CARTESIAN_POINT('Ctrl Pts',(17.0791842625823,20.5314731773872,20.7986403046093));
#192781=CARTESIAN_POINT('Ctrl Pts',(17.0671665107565,20.5162703242046,20.7975015757591));
#192782=CARTESIAN_POINT('Ctrl Pts',(17.0500837117325,20.494039323221,20.7958420189092));
#192783=CARTESIAN_POINT('Ctrl Pts',(17.0448502079753,20.4871414292824,20.7953278534071));
#192784=CARTESIAN_POINT('Ctrl Pts',(17.0357826740992,20.4750366776844,20.794426810133));
#192785=CARTESIAN_POINT('Ctrl Pts',(17.0319298852444,20.469843966322,20.794040673272));
#192786=CARTESIAN_POINT('Ctrl Pts',(17.0245192153108,20.4597597971696,20.7932915220662));
#192787=CARTESIAN_POINT('Ctrl Pts',(17.0209583857795,20.4548705764736,20.7929286275567));
#192788=CARTESIAN_POINT('Ctrl Pts',(17.0125342137011,20.4431989286185,20.7920630537975));
#192789=CARTESIAN_POINT('Ctrl Pts',(17.007689957473,20.4364029080416,20.7915596447327));
#192790=CARTESIAN_POINT('Ctrl Pts',(16.9905653835099,20.412075719693,20.7897595896725));
#192791=CARTESIAN_POINT('Ctrl Pts',(16.9785112285648,20.3943876233003,20.7884543683578));
#192792=CARTESIAN_POINT('Ctrl Pts',(16.8760651329884,20.2390491443778,20.7770190350146));
#192793=CARTESIAN_POINT('Ctrl Pts',(16.801817613528,20.0915667584953,20.7662792900608));
#192794=CARTESIAN_POINT('Ctrl Pts',(16.7454193572565,19.9371102032791,20.755413683557));
#192795=CARTESIAN_POINT('',(16.6170002905218,19.2098909150927,21.2890562789773));
#192796=CARTESIAN_POINT('Ctrl Pts',(16.6170002905218,19.2098909150927,21.2890562789773));
#192797=CARTESIAN_POINT('Ctrl Pts',(16.6170426459466,19.1290437037364,21.2842160179537));
#192798=CARTESIAN_POINT('Ctrl Pts',(16.6217204203657,19.0483585462384,21.2793757569302));
#192799=CARTESIAN_POINT('Ctrl Pts',(16.6309534063534,18.9683396922623,21.2745354959067));
#192800=CARTESIAN_POINT('Ctrl Pts',(16.6402204417599,18.888025744643,21.2696773849617));
#192801=CARTESIAN_POINT('Ctrl Pts',(16.6540762126097,18.8083833014798,21.2648192740168));
#192802=CARTESIAN_POINT('Ctrl Pts',(16.6723897133774,18.7299053875882,21.2599611630718));
#192803=CARTESIAN_POINT('Ctrl Pts',(16.6907932588013,18.6510416099083,21.2550791655452));
#192804=CARTESIAN_POINT('Ctrl Pts',(16.7136983382303,18.5733541106456,21.2501971680187));
#192805=CARTESIAN_POINT('Ctrl Pts',(16.7409237582267,18.4973221353589,21.2453151704921));
#192806=CARTESIAN_POINT('Ctrl Pts',(16.7538532455414,18.4612141722819,21.2429966855946));
#192807=CARTESIAN_POINT('Ctrl Pts',(16.7677564325119,18.4254792559445,21.2406782006971));
#192808=CARTESIAN_POINT('Ctrl Pts',(16.7826102744629,18.3901668019212,21.2383597157996));
#192809=CARTESIAN_POINT('Ctrl Pts',(16.8107255793529,18.3233275010485,21.2339712949458));
#192810=CARTESIAN_POINT('Ctrl Pts',(16.8423337821689,18.2578040117701,21.229582874092));
#192811=CARTESIAN_POINT('Ctrl Pts',(16.8772900899987,18.1939860816573,21.2251944532382));
#192812=CARTESIAN_POINT('Ctrl Pts',(16.9121945317766,18.130262840723,21.2208125436574));
#192813=CARTESIAN_POINT('Ctrl Pts',(16.9504369871457,18.068240554869,21.2164306340766));
#192814=CARTESIAN_POINT('Ctrl Pts',(16.9918247580849,18.0082887185787,21.2120487244958));
#192815=CARTESIAN_POINT('Ctrl Pts',(17.0331639095237,17.9484073095731,21.2076719624803));
#192816=CARTESIAN_POINT('Ctrl Pts',(17.077640763908,17.8905919134513,21.2032952004649));
#192817=CARTESIAN_POINT('Ctrl Pts',(17.1250177563768,17.8351856448978,21.1989184384494));
#192818=CARTESIAN_POINT('Ctrl Pts',(17.1723647117999,17.7798145039565,21.194544451304));
#192819=CARTESIAN_POINT('Ctrl Pts',(17.2226078444088,17.7268498257148,21.1901704641587));
#192820=CARTESIAN_POINT('Ctrl Pts',(17.2754683616743,17.6766029001582,21.1857964770133));
#192821=CARTESIAN_POINT('Ctrl Pts',(17.3283127983901,17.6263712600779,21.1814238204663));
#192822=CARTESIAN_POINT('Ctrl Pts',(17.3837726896225,17.5788560634065,21.1770511639194));
#192823=CARTESIAN_POINT('Ctrl Pts',(17.4415325011772,17.5343316474368,21.1726785073724));
#192824=CARTESIAN_POINT('Ctrl Pts',(17.4992937900869,17.4898060926414,21.1683057389835));
#192825=CARTESIAN_POINT('Ctrl Pts',(17.5593547328911,17.4482717633095,21.1639329705946));
#192826=CARTESIAN_POINT('Ctrl Pts',(17.6213681875234,17.4099615634682,21.1595602022058));
#192827=CARTESIAN_POINT('Ctrl Pts',(17.6834459783432,17.3716116185067,21.1551828972651));
#192828=CARTESIAN_POINT('Ctrl Pts',(17.7474799141124,17.3364927353749,21.1508055923245));
#192829=CARTESIAN_POINT('Ctrl Pts',(17.8130961612385,17.3047930018609,21.1464282873839));
#192830=CARTESIAN_POINT('Ctrl Pts',(17.8787482349071,17.2730759602579,21.14204859243));
#192831=CARTESIAN_POINT('Ctrl Pts',(17.9459838951715,17.2447819724004,21.1376688974761));
#192832=CARTESIAN_POINT('Ctrl Pts',(18.0144096407929,17.2200508005134,21.1332892025222));
#192833=CARTESIAN_POINT('Ctrl Pts',(18.0829566152675,17.1952758127853,21.1289017481293));
#192834=CARTESIAN_POINT('Ctrl Pts',(18.1526974237226,17.1740763866221,21.1245142937365));
#192835=CARTESIAN_POINT('Ctrl Pts',(18.2232243074044,17.1565421172841,21.1201268393436));
#192836=CARTESIAN_POINT('Ctrl Pts',(18.271142526286,17.1446287742835,21.1171458626018));
#192837=CARTESIAN_POINT('Ctrl Pts',(18.3194233700504,17.1344063045172,21.1141648858599));
#192838=CARTESIAN_POINT('Ctrl Pts',(18.3679374553786,17.1258891603981,21.1111839091181));
#192839=CARTESIAN_POINT('Ctrl Pts',(18.4393551977364,17.1133510449166,21.1067956035882));
#192840=CARTESIAN_POINT('Ctrl Pts',(18.511557184181,17.1044619384225,21.1024072980583));
#192841=CARTESIAN_POINT('Ctrl Pts',(18.584137344166,17.0993110588,21.0980189925284));
#192842=CARTESIAN_POINT('Ctrl Pts',(18.6566098256394,17.0941678209222,21.0936371974031));
#192843=CARTESIAN_POINT('Ctrl Pts',(18.7294588897195,17.0927518342718,21.0892554022779));
#192844=CARTESIAN_POINT('Ctrl Pts',(18.8022695645398,17.0951010736433,21.0848736071526));
#192845=CARTESIAN_POINT('Ctrl Pts',(18.874994735323,17.0974475542235,21.0804969577174));
#192846=CARTESIAN_POINT('Ctrl Pts',(18.9476811266901,17.1035504617408,21.0761203082823));
#192847=CARTESIAN_POINT('Ctrl Pts',(19.0199116617327,17.113395766193,21.0717436588472));
#192848=CARTESIAN_POINT('Ctrl Pts',(19.0920964214468,17.1232348312887,21.0673697830668));
#192849=CARTESIAN_POINT('Ctrl Pts',(19.1638254212813,17.1368115225586,21.0629959072864));
#192850=CARTESIAN_POINT('Ctrl Pts',(19.2346860280265,17.1540599179026,21.058622031506));
#192851=CARTESIAN_POINT('Ctrl Pts',(19.3055251003311,17.171303071483,21.0542494849405));
#192852=CARTESIAN_POINT('Ctrl Pts',(19.3754958350899,17.1922155998631,21.0498769383749));
#192853=CARTESIAN_POINT('Ctrl Pts',(19.4441967831924,17.2166806852605,21.0455043918093));
#192854=CARTESIAN_POINT('Ctrl Pts',(19.5128995129431,17.2411464051203,21.0411317318488));
#192855=CARTESIAN_POINT('Ctrl Pts',(19.5803319369287,17.2691647012125,21.0367590718883));
#192856=CARTESIAN_POINT('Ctrl Pts',(19.6461103367674,17.3005697517151,21.0323864119278));
#192857=CARTESIAN_POINT('Ctrl Pts',(19.7119570281094,17.332007407117,21.0280092122472));
#192858=CARTESIAN_POINT('Ctrl Pts',(19.7761458305496,17.3668386288833,21.0236320125666));
#192859=CARTESIAN_POINT('Ctrl Pts',(19.8383162620759,17.4048508939418,21.019254812886));
#192860=CARTESIAN_POINT('Ctrl Pts',(19.9005206624135,17.4428839282218,21.0148752215819));
#192861=CARTESIAN_POINT('Ctrl Pts',(19.9607040979254,17.4841011935237,21.0104956302777));
#192862=CARTESIAN_POINT('Ctrl Pts',(20.0185360763143,17.5282474725477,21.0061160389735));
#192863=CARTESIAN_POINT('Ctrl Pts',(20.0764705669914,17.5724720047493,21.0017286844571));
#192864=CARTESIAN_POINT('Ctrl Pts',(20.1320449087986,17.6196356063735,20.9973413299406));
#192865=CARTESIAN_POINT('Ctrl Pts',(20.1849630756626,17.6694439182878,20.9929539754242));
#192866=CARTESIAN_POINT('Ctrl Pts',(20.2209300194265,17.7032971838063,20.9899720177616));
#192867=CARTESIAN_POINT('Ctrl Pts',(20.2556706966756,17.7383713940979,20.9869900600991));
#192868=CARTESIAN_POINT('Ctrl Pts',(20.2891028445139,17.7745654755664,20.9840081024366));
#192869=CARTESIAN_POINT('Ctrl Pts',(20.3382998967395,17.8278268491664,20.9796200048616));
#192870=CARTESIAN_POINT('Ctrl Pts',(20.3848536073391,17.8837226211078,20.9752319072866));
#192871=CARTESIAN_POINT('Ctrl Pts',(20.4284691550635,17.9419597001914,20.9708438097116));
#192872=CARTESIAN_POINT('Ctrl Pts',(20.4720199507418,18.000110319968,20.9664622267469));
#192873=CARTESIAN_POINT('Ctrl Pts',(20.5126409559541,18.0605949637829,20.9620806437822));
#192874=CARTESIAN_POINT('Ctrl Pts',(20.5500756142482,18.1230853143131,20.9576990608175));
#192875=CARTESIAN_POINT('Ctrl Pts',(20.5874662646494,18.1855022016739,20.9533226288076));
#192876=CARTESIAN_POINT('Ctrl Pts',(20.6216777625938,18.2499197000074,20.9489461967977));
#192877=CARTESIAN_POINT('Ctrl Pts',(20.6524961368915,18.3159795685391,20.9445697647878));
#192878=CARTESIAN_POINT('Ctrl Pts',(20.6832949573685,18.3819975230225,20.9401961095618));
#192879=CARTESIAN_POINT('Ctrl Pts',(20.7107047223526,18.449655344029,20.9358224543359));
#192880=CARTESIAN_POINT('Ctrl Pts',(20.7345574965437,18.5185704346126,20.9314487991099));
#192881=CARTESIAN_POINT('Ctrl Pts',(20.7584030062156,18.587464536652,20.9270764759094));
#192882=CARTESIAN_POINT('Ctrl Pts',(20.7786935180933,18.6576146924788,20.922704152709));
#192883=CARTESIAN_POINT('Ctrl Pts',(20.7953099442832,18.7286201563092,20.9183318295085));
#192884=CARTESIAN_POINT('Ctrl Pts',(20.8119267919329,18.7996274211253,20.9139593954082));
#192885=CARTESIAN_POINT('Ctrl Pts',(20.8248692609018,18.871489566845,20.9095869613079));
#192886=CARTESIAN_POINT('Ctrl Pts',(20.8340690644341,18.9437942279684,20.9052145272077));
#192887=CARTESIAN_POINT('Ctrl Pts',(20.8432784149155,19.0161739220992,20.9008375556837));
#192888=CARTESIAN_POINT('Ctrl Pts',(20.8487372844885,19.0889965689121,20.8964605841598));
#192889=CARTESIAN_POINT('Ctrl Pts',(20.8504292318751,19.161844059721,20.8920836126359));
#192890=CARTESIAN_POINT('Ctrl Pts',(20.8521221031259,19.2347313278874,20.8877042511276));
#192891=CARTESIAN_POINT('Ctrl Pts',(20.8500439707311,19.3076429845142,20.8833248896193));
#192892=CARTESIAN_POINT('Ctrl Pts',(20.8442305254939,19.3801630257289,20.8789455281111));
#192893=CARTESIAN_POINT('Ctrl Pts',(20.8384067750087,19.4528116201468,20.8745584034943));
#192894=CARTESIAN_POINT('Ctrl Pts',(20.8288345523668,19.5250667342145,20.8701712788775));
#192895=CARTESIAN_POINT('Ctrl Pts',(20.8156011167307,19.5965201561856,20.8657841542607));
#192896=CARTESIAN_POINT('Ctrl Pts',(20.8066002445799,19.6451200159337,20.8628002014256));
#192897=CARTESIAN_POINT('Ctrl Pts',(20.7959066968999,19.6933492110076,20.8598162485904));
#192898=CARTESIAN_POINT('Ctrl Pts',(20.7835610193857,19.7410836045517,20.8568322957552));
#192899=CARTESIAN_POINT('Ctrl Pts',(20.7654052821597,19.8112825146428,20.8524440502735));
#192900=CARTESIAN_POINT('Ctrl Pts',(20.7436033946027,19.8806845840498,20.8480558047918));
#192901=CARTESIAN_POINT('Ctrl Pts',(20.7182422505467,19.9488832503489,20.8436675593101));
#192902=CARTESIAN_POINT('Ctrl Pts',(20.6929187443098,20.0169807047679,20.8392858263103));
#192903=CARTESIAN_POINT('Ctrl Pts',(20.6640466342099,20.0838778530322,20.8349040933104));
#192904=CARTESIAN_POINT('Ctrl Pts',(20.6317631447894,20.1491812438324,20.8305223603105));
#192905=CARTESIAN_POINT('Ctrl Pts',(20.5995175882209,20.2144079036502,20.8261457758132));
#192906=CARTESIAN_POINT('Ctrl Pts',(20.5638688276462,20.2780440957741,20.821769191316));
#192907=CARTESIAN_POINT('Ctrl Pts',(20.52500229796,20.3397159823012,20.8173926068187));
#192908=CARTESIAN_POINT('Ctrl Pts',(20.4861604149721,20.401348760413,20.8130187976749));
#192909=CARTESIAN_POINT('Ctrl Pts',(20.4441050680544,20.4610192973534,20.8086449885311));
#192910=CARTESIAN_POINT('Ctrl Pts',(20.3990670887796,20.5183792830939,20.8042711793873));
#192911=CARTESIAN_POINT('Ctrl Pts',(20.3540428132133,20.5757218159082,20.7998987010627));
#192912=CARTESIAN_POINT('Ctrl Pts',(20.3060380047229,20.6307548140923,20.7955262227381));
#192913=CARTESIAN_POINT('Ctrl Pts',(20.2553251939663,20.6831612188219,20.7911537444134));
#192914=CARTESIAN_POINT('Ctrl Pts',(20.2046110855668,20.7355689645303,20.7867811542055));
#192915=CARTESIAN_POINT('Ctrl Pts',(20.1511891742029,20.7853496380956,20.7824085639976));
#192916=CARTESIAN_POINT('Ctrl Pts',(20.0953692572892,20.8322226081905,20.7780359737897));
#192917=CARTESIAN_POINT('Ctrl Pts',(20.039491410639,20.8791442229081,20.7736588457212));
#192918=CARTESIAN_POINT('Ctrl Pts',(19.9812109598893,20.9231517984441,20.7692817176527));
#192919=CARTESIAN_POINT('Ctrl Pts',(19.9208705934444,20.9640051895009,20.7649045895843));
#192920=CARTESIAN_POINT('Ctrl Pts',(19.8604972734422,21.004880891734,20.7605250710441));
#192921=CARTESIAN_POINT('Ctrl Pts',(19.7980622110869,21.0425987302322,20.7561455525039));
#192922=CARTESIAN_POINT('Ctrl Pts',(19.7339345423434,21.0769635342173,20.7517660339637));
#192923=CARTESIAN_POINT('Ctrl Pts',(19.6696932153011,21.1113892455334,20.7473787532728));
#192924=CARTESIAN_POINT('Ctrl Pts',(19.6037537278872,21.1424498489971,20.742991472582));
#192925=CARTESIAN_POINT('Ctrl Pts',(19.5365065764868,21.1699977526009,20.7386041918911));
#192926=CARTESIAN_POINT('Ctrl Pts',(19.4907905192111,21.1887254089068,20.7356216242854));
#192927=CARTESIAN_POINT('Ctrl Pts',(19.444470516459,21.2058306634918,20.7326390566796));
#192928=CARTESIAN_POINT('Ctrl Pts',(19.3976727117749,21.221280460942,20.7296564890738));
#192929=CARTESIAN_POINT('Ctrl Pts',(19.3288196246099,21.2440115753118,20.7252682706793));
#192930=CARTESIAN_POINT('Ctrl Pts',(19.258662966693,21.2632455878281,20.7208800522848));
#192931=CARTESIAN_POINT('Ctrl Pts',(19.1875916213885,21.2788354966017,20.7164918338903));
#192932=CARTESIAN_POINT('Ctrl Pts',(19.1166257529093,21.2944022684265,20.712110128041));
#192933=CARTESIAN_POINT('Ctrl Pts',(19.0447483591154,21.3063355700378,20.7077284221917));
#192934=CARTESIAN_POINT('Ctrl Pts',(18.9723645424585,21.31453781637,20.7033467163423));
#192935=CARTESIAN_POINT('Ctrl Pts',(18.9000657760964,21.3227304251408,20.6989701589556));
#192936=CARTESIAN_POINT('Ctrl Pts',(18.8272622458552,21.3272006333429,20.6945936015689));
#192937=CARTESIAN_POINT('Ctrl Pts',(18.7543686581099,21.3279020094862,20.6902170441822));
#192938=CARTESIAN_POINT('Ctrl Pts',(18.6815212945107,21.3286029408646,20.6858432621099));
#192939=CARTESIAN_POINT('Ctrl Pts',(18.6085844678842,21.3255397774992,20.6814694800377));
#192940=CARTESIAN_POINT('Ctrl Pts',(18.5359759923093,21.318718077063,20.6770956979654));
#192941=CARTESIAN_POINT('Ctrl Pts',(18.4633896081417,21.3118984521553,20.6727232466332));
#192942=CARTESIAN_POINT('Ctrl Pts',(18.3911318566611,21.3013226055695,20.6683507953009));
#192943=CARTESIAN_POINT('Ctrl Pts',(18.3196168457075,21.2870480730076,20.6639783439686));
#192944=CARTESIAN_POINT('Ctrl Pts',(18.2481000028579,21.2727731747958,20.6596057806336));
#192945=CARTESIAN_POINT('Ctrl Pts',(18.1773264109616,21.2547994988843,20.6552332172986));
#192946=CARTESIAN_POINT('Ctrl Pts',(18.1076997199475,21.2332356339473,20.6508606539636));
#192947=CARTESIAN_POINT('Ctrl Pts',(18.0380007641851,21.2116493881209,20.646483552395));
#192948=CARTESIAN_POINT('Ctrl Pts',(17.9694515476975,21.1864656566405,20.6421064508264));
#192949=CARTESIAN_POINT('Ctrl Pts',(17.9024394813628,21.1578425986309,20.6377293492578));
#192950=CARTESIAN_POINT('Ctrl Pts',(17.8353908150804,21.1292039075796,20.6333498570497));
#192951=CARTESIAN_POINT('Ctrl Pts',(17.7698814039915,21.0971223623162,20.6289703648416));
#192952=CARTESIAN_POINT('Ctrl Pts',(17.706275157963,21.0618027039801,20.6245908726336));
#192953=CARTESIAN_POINT('Ctrl Pts',(17.6425561688916,21.0264204410099,20.6202036177087));
#192954=CARTESIAN_POINT('Ctrl Pts',(17.5807474908118,20.9877888590985,20.6158163627838));
#192955=CARTESIAN_POINT('Ctrl Pts',(17.5211845892524,20.9461564135412,20.6114291078589));
#192956=CARTESIAN_POINT('Ctrl Pts',(17.4806889418755,20.9178513311731,20.60844629937));
#192957=CARTESIAN_POINT('Ctrl Pts',(17.4412307372919,20.8881600257597,20.6054634908812));
#192958=CARTESIAN_POINT('Ctrl Pts',(17.4029060721845,20.8571706944702,20.6024806823924));
#192959=CARTESIAN_POINT('Ctrl Pts',(17.3472665724937,20.8121805847363,20.5981502604166));
#192960=CARTESIAN_POINT('Ctrl Pts',(17.2937883055549,20.764267267587,20.5938198384409));
#192961=CARTESIAN_POINT('Ctrl Pts',(17.2428007358364,20.7136688772175,20.5894894164652));
#192962=CARTESIAN_POINT('Ctrl Pts',(17.1918849324429,20.6631417053928,20.5851650896706));
#192963=CARTESIAN_POINT('Ctrl Pts',(17.1434532240215,20.6099373000743,20.580840762876));
#192964=CARTESIAN_POINT('Ctrl Pts',(17.0978028464019,20.5543346100498,20.5765164360814));
#192965=CARTESIAN_POINT('Ctrl Pts',(17.0522038395386,20.4987944902028,20.5721969754883));
#192966=CARTESIAN_POINT('Ctrl Pts',(17.009380264264,20.4408618239644,20.5678775148952));
#192967=CARTESIAN_POINT('Ctrl Pts',(16.9695918503724,20.3808516493675,20.5635580543021));
#192968=CARTESIAN_POINT('Ctrl Pts',(16.9298290256535,20.3208800691895,20.5592413716891));
#192969=CARTESIAN_POINT('Ctrl Pts',(16.8930977626164,20.2588340443183,20.5549246890762));
#192970=CARTESIAN_POINT('Ctrl Pts',(16.8596158552161,20.1950594889451,20.5506080064632));
#192971=CARTESIAN_POINT('Ctrl Pts',(16.826139467696,20.1312954475459,20.5462920355053));
#192972=CARTESIAN_POINT('Ctrl Pts',(16.7959116071781,20.0658038781863,20.5419760645475));
#192973=CARTESIAN_POINT('Ctrl Pts',(16.7691044221986,19.9989558162336,20.5376600935896));
#192974=CARTESIAN_POINT('Ctrl Pts',(16.7608869589861,19.9784642394291,20.5363370776669));
#192975=CARTESIAN_POINT('Ctrl Pts',(16.752990588142,19.9578453517266,20.5350140617441));
#192976=CARTESIAN_POINT('Ctrl Pts',(16.7454193623258,19.9371102171621,20.5336910458214));
#192977=CARTESIAN_POINT('Ctrl Pts',(16.7454193623258,19.9371102171621,21.3335535344094));
#192978=CARTESIAN_POINT('Ctrl Pts',(16.7201109592649,19.8677987006626,21.3291191840504));
#192979=CARTESIAN_POINT('Ctrl Pts',(16.6984027907146,19.7970869511725,21.3246848336914));
#192980=CARTESIAN_POINT('Ctrl Pts',(16.6804408812102,19.7253772405883,21.3202504833324));
#192981=CARTESIAN_POINT('Ctrl Pts',(16.6624933564997,19.6537249587208,21.3158196842226));
#192982=CARTESIAN_POINT('Ctrl Pts',(16.6482862433426,19.5810767527722,21.3113888851128));
#192983=CARTESIAN_POINT('Ctrl Pts',(16.6379158001016,19.5078501759078,21.306958086003));
#192984=CARTESIAN_POINT('Ctrl Pts',(16.6275504545434,19.434659594212,21.3025294648915));
#192985=CARTESIAN_POINT('Ctrl Pts',(16.6210180961611,19.3608916660175,21.29810084378));
#192986=CARTESIAN_POINT('Ctrl Pts',(16.6183636592833,19.2869728493529,21.2936722226685));
#192987=CARTESIAN_POINT('Ctrl Pts',(16.6174414210567,19.2612910337636,21.2921335747865));
#192988=CARTESIAN_POINT('Ctrl Pts',(16.6169868263632,19.2355910567946,21.2905949269045));
#192989=CARTESIAN_POINT('Ctrl Pts',(16.6170002905214,19.2098909158485,21.2890562790225));
#192990=CARTESIAN_POINT('Origin',(-18.734,19.211,0.));
#192991=CARTESIAN_POINT('',(-20.7225806064498,19.9371103026755,0.755484067882562));
#192992=CARTESIAN_POINT('',(-20.7225806064217,19.9371103027527,0.534177455193947));
#192993=CARTESIAN_POINT('',(-20.7225806064498,19.9371103026755,0.));
#192994=CARTESIAN_POINT('',(-20.8509997094734,19.2121090940372,0.710943721022757));
#192995=CARTESIAN_POINT('Ctrl Pts',(-20.8509997094734,19.2121090940372,
0.710943721022757));
#192996=CARTESIAN_POINT('Ctrl Pts',(-20.8509573780607,19.2929098065566,
0.715781198363344));
#192997=CARTESIAN_POINT('Ctrl Pts',(-20.8462849630088,19.3735486530339,
0.720618675703931));
#192998=CARTESIAN_POINT('Ctrl Pts',(-20.8370625189587,19.4535222491878,
0.725456153044519));
#192999=CARTESIAN_POINT('Ctrl Pts',(-20.827521362655,19.5362595991716,0.730460805517526));
#193000=CARTESIAN_POINT('Ctrl Pts',(-20.8131101367243,19.6182845242239,
0.735465457990533));
#193001=CARTESIAN_POINT('Ctrl Pts',(-20.7939728312899,19.6990583308864,
0.74047011046354));
#193002=CARTESIAN_POINT('Ctrl Pts',(-20.7748355258554,19.7798321375489,
0.745474762936547));
#193003=CARTESIAN_POINT('Ctrl Pts',(-20.7509723452674,19.859354538864,0.750479415409554));
#193004=CARTESIAN_POINT('Ctrl Pts',(-20.7225806064499,19.9371103026755,
0.755484067882561));
#193005=CARTESIAN_POINT('',(-20.3539402423909,20.5738949376539,2.19221145944165E-7));
#193006=CARTESIAN_POINT('Ctrl Pts',(-20.3539402423909,20.5738949376539,
2.19221145944165E-7));
#193007=CARTESIAN_POINT('Ctrl Pts',(-20.307293457224,20.6293394201171,0.00438523054252758));
#193008=CARTESIAN_POINT('Ctrl Pts',(-20.2577052453278,20.6824952398002,
0.00877024186390921));
#193009=CARTESIAN_POINT('Ctrl Pts',(-20.2054289850318,20.7330334234203,
0.0131552531852908));
#193010=CARTESIAN_POINT('Ctrl Pts',(-20.1532303457041,20.7834965668073,
0.0175337535431212));
#193011=CARTESIAN_POINT('Ctrl Pts',(-20.0983519254293,20.8313494565077,
0.0219122539009516));
#193012=CARTESIAN_POINT('Ctrl Pts',(-20.0410868627425,20.8762966502236,
0.026290754258782));
#193013=CARTESIAN_POINT('Ctrl Pts',(-19.9838891952345,20.9211909456449,
0.030664101565157));
#193014=CARTESIAN_POINT('Ctrl Pts',(-19.9243108432097,20.963186041445,0.035037448871532));
#193015=CARTESIAN_POINT('Ctrl Pts',(-19.8626799780617,21.0020249878554,
0.039410796177907));
#193016=CARTESIAN_POINT('Ctrl Pts',(-19.8010881104921,21.040839358514,0.0437813762027675));
#193017=CARTESIAN_POINT('Ctrl Pts',(-19.7374467144134,21.0765012852423,
0.0481519562276279));
#193018=CARTESIAN_POINT('Ctrl Pts',(-19.6721138966915,21.1087964371434,
0.0525225362524884));
#193019=CARTESIAN_POINT('Ctrl Pts',(-19.6068007822918,21.1410818493485,
0.0568917981810319));
#193020=CARTESIAN_POINT('Ctrl Pts',(-19.5397976918714,21.1700022886331,
0.0612610601095754));
#193021=CARTESIAN_POINT('Ctrl Pts',(-19.47148685249,21.1953896145678,0.0656303220381189));
#193022=CARTESIAN_POINT('Ctrl Pts',(-19.4031739921599,21.2207776915762,
0.0699997132295205));
#193023=CARTESIAN_POINT('Ctrl Pts',(-19.3335537597038,21.2426322814668,
0.0743691044209222));
#193024=CARTESIAN_POINT('Ctrl Pts',(-19.2630262593487,21.2608341925433,
0.0787384956123238));
#193025=CARTESIAN_POINT('Ctrl Pts',(-19.1924269638886,21.2790546326773,
0.0831123347268408));
#193026=CARTESIAN_POINT('Ctrl Pts',(-19.1209190256057,21.2936148503494,
0.0874861738413579));
#193027=CARTESIAN_POINT('Ctrl Pts',(-19.048914683673,21.3044463790618,0.0918600129558749));
#193028=CARTESIAN_POINT('Ctrl Pts',(-18.9768705191299,21.3152838982429,
0.0962362710591149));
#193029=CARTESIAN_POINT('Ctrl Pts',(-18.9043298854534,21.3223885760892,
0.100612529162355));
#193030=CARTESIAN_POINT('Ctrl Pts',(-18.8317094286013,21.3257439248198,
0.104988787265595));
#193031=CARTESIAN_POINT('Ctrl Pts',(-18.7589648320255,21.3291050092906,
0.109372526283929));
#193032=CARTESIAN_POINT('Ctrl Pts',(-18.6861406230801,21.3287039714963,
0.113756265302264));
#193033=CARTESIAN_POINT('Ctrl Pts',(-18.6136520423459,21.324576440323,0.118140004320598));
#193034=CARTESIAN_POINT('Ctrl Pts',(-18.5716442693831,21.3221844995419,
0.1206804198115));
#193035=CARTESIAN_POINT('Ctrl Pts',(-18.5297491060651,21.3185420587999,
0.123220835302401));
#193036=CARTESIAN_POINT('Ctrl Pts',(-18.4880458562809,21.3136639196951,
0.125761250793303));
#193037=CARTESIAN_POINT('Ctrl Pts',(-18.415885212538,21.3052230988983,0.13015702374017));
#193038=CARTESIAN_POINT('Ctrl Pts',(-18.3440242467257,21.2930474771355,
0.134552796687038));
#193039=CARTESIAN_POINT('Ctrl Pts',(-18.2728788054798,21.2771694615796,
0.138948569633906));
#193040=CARTESIAN_POINT('Ctrl Pts',(-18.201836191067,21.2613143945926,0.143337989349937));
#193041=CARTESIAN_POINT('Ctrl Pts',(-18.1315075132681,21.2417676616992,
0.147727409065968));
#193042=CARTESIAN_POINT('Ctrl Pts',(-18.0623022558513,21.2186132945629,
0.152116828781999));
#193043=CARTESIAN_POINT('Ctrl Pts',(-17.9931750162606,21.1954850302611,
0.156501300131437));
#193044=CARTESIAN_POINT('Ctrl Pts',(-17.9251691345193,21.168757363137,0.160885771480875));
#193045=CARTESIAN_POINT('Ctrl Pts',(-17.8586810464524,21.1385647147529,
0.165270242830314));
#193046=CARTESIAN_POINT('Ctrl Pts',(-17.7922332423912,21.1083903595827,
0.169652057702872));
#193047=CARTESIAN_POINT('Ctrl Pts',(-17.7273018435918,21.0747553873414,
0.17403387257543));
#193048=CARTESIAN_POINT('Ctrl Pts',(-17.6642640090405,21.0378426066976,
0.178415687447987));
#193049=CARTESIAN_POINT('Ctrl Pts',(-17.6012437811927,21.0009401359319,
0.182796278463219));
#193050=CARTESIAN_POINT('Ctrl Pts',(-17.5401164818004,20.9607619172419,
0.187176869478451));
#193051=CARTESIAN_POINT('Ctrl Pts',(-17.4812338530683,20.9175362525015,
0.191557460493683));
#193052=CARTESIAN_POINT('Ctrl Pts',(-17.4223484413191,20.8743085447517,
0.195938258552312));
#193053=CARTESIAN_POINT('Ctrl Pts',(-17.3657082969835,20.8280333908516,
0.20031905661094));
#193054=CARTESIAN_POINT('Ctrl Pts',(-17.3116340465775,20.7789808973787,
0.204699854669569));
#193055=CARTESIAN_POINT('Ctrl Pts',(-17.2575026772116,20.7298765894583,
0.209085280191852));
#193056=CARTESIAN_POINT('Ctrl Pts',(-17.2059429696119,20.6779894082537,
0.213470705714135));
#193057=CARTESIAN_POINT('Ctrl Pts',(-17.157239849178,20.6236274904517,0.217856131236418));
#193058=CARTESIAN_POINT('Ctrl Pts',(-17.1085094838156,20.569235162143,0.222244010002027));
#193059=CARTESIAN_POINT('Ctrl Pts',(-17.0626391892086,20.5123657149587,
0.226631888767637));
#193060=CARTESIAN_POINT('Ctrl Pts',(-17.0198728898628,20.4533595495237,
0.231019767533247));
#193061=CARTESIAN_POINT('Ctrl Pts',(-16.9770308541579,20.3942488879738,
0.235415416949269));
#193062=CARTESIAN_POINT('Ctrl Pts',(-16.9373040526505,20.3329943550553,
0.23981106636529));
#193063=CARTESIAN_POINT('Ctrl Pts',(-16.9008921528455,20.2699639373937,
0.244206715781312));
#193064=CARTESIAN_POINT('Ctrl Pts',(-16.876785868281,20.2282350193065,0.247116829679121));
#193065=CARTESIAN_POINT('Ctrl Pts',(-16.8541315650652,20.1857282478032,
0.250026943576929));
#193066=CARTESIAN_POINT('Ctrl Pts',(-16.8329755574333,20.1425551882545,
0.252937057474737));
#193067=CARTESIAN_POINT('Ctrl Pts',(-16.8011149178839,20.077537188996,0.257319646645566));
#193068=CARTESIAN_POINT('Ctrl Pts',(-16.7725299917263,20.0107527148536,
0.261702235816396));
#193069=CARTESIAN_POINT('Ctrl Pts',(-16.7474198406578,19.9425656296656,
0.266084824987225));
#193070=CARTESIAN_POINT('Ctrl Pts',(-16.7223474688912,19.8744811348787,
0.270460820364237));
#193071=CARTESIAN_POINT('Ctrl Pts',(-16.7007396607462,19.8049986679621,
0.27483681574125));
#193072=CARTESIAN_POINT('Ctrl Pts',(-16.6827487993224,19.7345050254953,
0.279212811118263));
#193073=CARTESIAN_POINT('Ctrl Pts',(-16.6647794915184,19.6640958366371,
0.2835835639147));
#193074=CARTESIAN_POINT('Ctrl Pts',(-16.6504186420449,19.5926783449244,
0.287954316711137));
#193075=CARTESIAN_POINT('Ctrl Pts',(-16.6397693071744,19.5206559465392,
0.292325069507573));
#193076=CARTESIAN_POINT('Ctrl Pts',(-16.6291268685744,19.4486801882447,
0.296692991902476));
#193077=CARTESIAN_POINT('Ctrl Pts',(-16.6221912467961,19.3761007777964,
0.30106091429738));
#193078=CARTESIAN_POINT('Ctrl Pts',(-16.6190144407725,19.3033313828499,
0.305428836692283));
#193079=CARTESIAN_POINT('Ctrl Pts',(-16.6158386365901,19.2305849365468,
0.309795381613953));
#193080=CARTESIAN_POINT('Ctrl Pts',(-16.6164193161497,19.1576491077124,
0.314161926535623));
#193081=CARTESIAN_POINT('Ctrl Pts',(-16.6207564869952,19.0849410663897,
0.318528471457294));
#193082=CARTESIAN_POINT('Ctrl Pts',(-16.6250937309155,19.0122318000446,
0.322895089948759));
#193083=CARTESIAN_POINT('Ctrl Pts',(-16.6331875609615,18.9397508116577,
0.327261708440224));
#193084=CARTESIAN_POINT('Ctrl Pts',(-16.6449859783168,18.867911939568,0.33162832693169));
#193085=CARTESIAN_POINT('Ctrl Pts',(-16.6567966078099,18.7959987095218,
0.335999465160437));
#193086=CARTESIAN_POINT('Ctrl Pts',(-16.6723194019262,18.7247294012091,
0.340370603389185));
#193087=CARTESIAN_POINT('Ctrl Pts',(-16.6914510303897,18.6545085744202,
0.344741741617932));
#193088=CARTESIAN_POINT('Ctrl Pts',(-16.7105930357156,18.5842496603426,
0.349115250721684));
#193089=CARTESIAN_POINT('Ctrl Pts',(-16.7333476210311,18.5150408198693,
0.353488759825437));
#193090=CARTESIAN_POINT('Ctrl Pts',(-16.7595620940046,18.447269710324,0.357862268929189));
#193091=CARTESIAN_POINT('Ctrl Pts',(-16.7858233028863,18.3793777765168,
0.362243575249379));
#193092=CARTESIAN_POINT('Ctrl Pts',(-16.8155565194801,18.3129291342219,
0.366624881569569));
#193093=CARTESIAN_POINT('Ctrl Pts',(-16.8485618556777,18.2482892418101,
0.371006187889759));
#193094=CARTESIAN_POINT('Ctrl Pts',(-16.8714293819244,18.2035039250522,
0.37404174664523));
#193095=CARTESIAN_POINT('Ctrl Pts',(-16.8958666541819,18.1595863577281,
0.3770773054007));
#193096=CARTESIAN_POINT('Ctrl Pts',(-16.9217951530525,18.1166496937908,
0.380112864156171));
#193097=CARTESIAN_POINT('Ctrl Pts',(-16.9592870771133,18.0545644125798,
0.384502201884909));
#193098=CARTESIAN_POINT('Ctrl Pts',(-17.000046146169,17.9942872611045,0.388891539613646));
#193099=CARTESIAN_POINT('Ctrl Pts',(-17.0438725732189,17.9361830401024,
0.393280877342384));
#193100=CARTESIAN_POINT('Ctrl Pts',(-17.0876340137246,17.8781649769917,
0.397663706489195));
#193101=CARTESIAN_POINT('Ctrl Pts',(-17.1344534950993,17.8223138297407,
0.402046535636006));
#193102=CARTESIAN_POINT('Ctrl Pts',(-17.184086764136,17.7689674201692,0.406429364782818));
#193103=CARTESIAN_POINT('Ctrl Pts',(-17.2336617334565,17.7156836718045,
0.410807045816273));
#193104=CARTESIAN_POINT('Ctrl Pts',(-17.2860435979522,17.6648991677451,
0.415184726849729));
#193105=CARTESIAN_POINT('Ctrl Pts',(-17.3409475304283,17.616919130966,0.419562407883185));
#193106=CARTESIAN_POINT('Ctrl Pts',(-17.3958166506481,17.5689695162945,
0.423937313214657));
#193107=CARTESIAN_POINT('Ctrl Pts',(-17.4532043037707,17.5238211571201,
0.428312218546129));
#193108=CARTESIAN_POINT('Ctrl Pts',(-17.512789475476,17.4817418195099,0.4326871238776));
#193109=CARTESIAN_POINT('Ctrl Pts',(-17.5723564947758,17.4396753012166,
0.4370606964101));
#193110=CARTESIAN_POINT('Ctrl Pts',(-17.6341193099785,17.4006762261876,
0.4414342689426));
#193111=CARTESIAN_POINT('Ctrl Pts',(-17.6977258981411,17.3649704807841,
0.445807841475099));
#193112=CARTESIAN_POINT('Ctrl Pts',(-17.7613340609317,17.3292638514585,
0.450181522278617));
#193113=CARTESIAN_POINT('Ctrl Pts',(-17.8267856659412,17.29685094787,0.454555203082135));
#193114=CARTESIAN_POINT('Ctrl Pts',(-17.8937034068913,17.2679120875241,
0.458928883885652));
#193115=CARTESIAN_POINT('Ctrl Pts',(-17.9606903750842,17.238943289564,0.463307089316848));
#193116=CARTESIAN_POINT('Ctrl Pts',(-18.0291460640642,17.2134559021899,
0.467685294748045));
#193117=CARTESIAN_POINT('Ctrl Pts',(-18.0986732370017,17.191582038255,0.472063500179241));
#193118=CARTESIAN_POINT('Ctrl Pts',(-18.1682382801082,17.1696962600299,
0.476444090338191));
#193119=CARTESIAN_POINT('Ctrl Pts',(-18.2388755021192,17.1514280448653,
0.48082468049714));
#193120=CARTESIAN_POINT('Ctrl Pts',(-18.3101751880181,17.1368588455102,
0.48520527065609));
#193121=CARTESIAN_POINT('Ctrl Pts',(-18.3816008664645,17.1222639011532,
0.489593601686642));
#193122=CARTESIAN_POINT('Ctrl Pts',(-18.4536908693965,17.1113810977932,
0.493981932717194));
#193123=CARTESIAN_POINT('Ctrl Pts',(-18.5260286230796,17.1042401877808,
0.498370263747746));
#193124=CARTESIAN_POINT('Ctrl Pts',(-18.5750326393233,17.0994026962577,
0.501343066111033));
#193125=CARTESIAN_POINT('Ctrl Pts',(-18.624150260615,17.0962813311373,0.504315868474319));
#193126=CARTESIAN_POINT('Ctrl Pts',(-18.6732524681258,17.0948717578154,
0.507288670837606));
#193127=CARTESIAN_POINT('Ctrl Pts',(-18.7457477325718,17.0927906417942,
0.511677762579041));
#193128=CARTESIAN_POINT('Ctrl Pts',(-18.818490899314,17.0944351534906,0.516066854320476));
#193129=CARTESIAN_POINT('Ctrl Pts',(-18.8910671105736,17.0998347002719,
0.520455946061912));
#193130=CARTESIAN_POINT('Ctrl Pts',(-18.9635359557305,17.1052262591976,
0.524838544771176));
#193131=CARTESIAN_POINT('Ctrl Pts',(-19.035837858837,17.1143617900503,0.52922114348044));
#193132=CARTESIAN_POINT('Ctrl Pts',(-19.1075565880863,17.1272187073742,
0.533603742189705));
#193133=CARTESIAN_POINT('Ctrl Pts',(-19.1791914726444,17.1400605939763,
0.537981217305188));
#193134=CARTESIAN_POINT('Ctrl Pts',(-19.2502440654555,17.1566151398615,
0.542358692420671));
#193135=CARTESIAN_POINT('Ctrl Pts',(-19.320303591177,17.1768079984984,0.546736167536153));
#193136=CARTESIAN_POINT('Ctrl Pts',(-19.3903189366747,17.1969881233207,
0.551110882172916));
#193137=CARTESIAN_POINT('Ctrl Pts',(-19.4593419954754,17.2208018753163,
0.555485596809679));
#193138=CARTESIAN_POINT('Ctrl Pts',(-19.5269739113633,17.2481242077255,
0.559860311446443));
#193139=CARTESIAN_POINT('Ctrl Pts',(-19.5945854628883,17.2754383132217,
0.564233708831213));
#193140=CARTESIAN_POINT('Ctrl Pts',(-19.6608062563391,17.3062587212116,
0.568607106215984));
#193141=CARTESIAN_POINT('Ctrl Pts',(-19.7252558767888,17.3404116469058,
0.572980503600755));
#193142=CARTESIAN_POINT('Ctrl Pts',(-19.7897073269136,17.3745655421752,
0.577354025142908));
#193143=CARTESIAN_POINT('Ctrl Pts',(-19.8523870791113,17.4120519154596,
0.581727546685062));
#193144=CARTESIAN_POINT('Ctrl Pts',(-19.9129393606855,17.4526510631202,
0.586101068227215));
#193145=CARTESIAN_POINT('Ctrl Pts',(-19.9735546434687,17.4932924518874,
0.590479140170077));
#193146=CARTESIAN_POINT('Ctrl Pts',(-20.0320376349006,17.537052812133,0.594857212112939));
#193147=CARTESIAN_POINT('Ctrl Pts',(-20.0880623158585,17.5836695956961,
0.599235284055801));
#193148=CARTESIAN_POINT('Ctrl Pts',(-20.1441176953744,17.6303119227877,
0.603615754950226));
#193149=CARTESIAN_POINT('Ctrl Pts',(-20.1977117280627,17.6798134620822,
0.607996225844651));
#193150=CARTESIAN_POINT('Ctrl Pts',(-20.2485542488444,17.7318737622139,
0.612376696739076));
#193151=CARTESIAN_POINT('Ctrl Pts',(-20.2994868988123,17.7840263503048,
0.616764932950222));
#193152=CARTESIAN_POINT('Ctrl Pts',(-20.3476579775569,17.8387463951232,
0.621153169161368));
#193153=CARTESIAN_POINT('Ctrl Pts',(-20.3928170879059,17.8956997039188,
0.625541405372514));
#193154=CARTESIAN_POINT('Ctrl Pts',(-20.4234260448481,17.9343027978054,
0.628515762754689));
#193155=CARTESIAN_POINT('Ctrl Pts',(-20.4526521208593,17.9739312228937,
0.631490120136864));
#193156=CARTESIAN_POINT('Ctrl Pts',(-20.4804290546179,18.0144739630136,
0.634464477519039));
#193157=CARTESIAN_POINT('Ctrl Pts',(-20.5219871907903,18.0751315118038,
0.638914527700529));
#193158=CARTESIAN_POINT('Ctrl Pts',(-20.5604590132257,18.1380695894107,
0.643364577882019));
#193159=CARTESIAN_POINT('Ctrl Pts',(-20.5955899392305,18.2029464805101,
0.647814628063508));
#193160=CARTESIAN_POINT('Ctrl Pts',(-20.6306645724414,18.2677194147297,
0.652257547611509));
#193161=CARTESIAN_POINT('Ctrl Pts',(-20.6624087216052,18.3344245877164,
0.65670046715951));
#193162=CARTESIAN_POINT('Ctrl Pts',(-20.6906107187659,18.4026909655271,
0.661143386707512));
#193163=CARTESIAN_POINT('Ctrl Pts',(-20.7187694104787,18.4708525172134,
0.665579483950703));
#193164=CARTESIAN_POINT('Ctrl Pts',(-20.7433965899229,18.5405700796876,
0.670015581193894));
#193165=CARTESIAN_POINT('Ctrl Pts',(-20.7643270288141,18.6114492047649,
0.674451678437085));
#193166=CARTESIAN_POINT('Ctrl Pts',(-20.7852384786614,18.6822640250841,
0.678883751051583));
#193167=CARTESIAN_POINT('Ctrl Pts',(-20.8024597179405,18.7542378712037,
0.68331582366608));
#193168=CARTESIAN_POINT('Ctrl Pts',(-20.8158744295843,18.8269585185907,
0.687747896280578));
#193169=CARTESIAN_POINT('Ctrl Pts',(-20.8292815989961,18.8996382798217,
0.692177477024898));
#193170=CARTESIAN_POINT('Ctrl Pts',(-20.8388864061313,18.9730635524855,
0.696607057769218));
#193171=CARTESIAN_POINT('Ctrl Pts',(-20.8446233280938,19.0468105761441,
0.701036638513538));
#193172=CARTESIAN_POINT('Ctrl Pts',(-20.8489003437794,19.1017907866147,
0.704338999334862));
#193173=CARTESIAN_POINT('Ctrl Pts',(-20.851028607491,19.156949536228,0.707641360156185));
#193174=CARTESIAN_POINT('Ctrl Pts',(-20.8509997094738,19.2121090932814,
0.710943720977509));
#193175=CARTESIAN_POINT('',(-17.1140743056112,20.5739122292573,0.));
#193176=CARTESIAN_POINT('Origin',(-18.734,19.211,0.));
#193177=CARTESIAN_POINT('',(-20.8509993841467,19.2126147825168,0.48905627896718));
#193178=CARTESIAN_POINT('Ctrl Pts',(-20.8509993841467,19.2126147825168,
0.48905627896718));
#193179=CARTESIAN_POINT('Ctrl Pts',(-20.8510560155281,19.1383703573979,
0.484575909845393));
#193180=CARTESIAN_POINT('Ctrl Pts',(-20.8472020813435,19.0639814494018,
0.480095540723607));
#193181=CARTESIAN_POINT('Ctrl Pts',(-20.8394225379869,18.9899006184163,
0.47561517160182));
#193182=CARTESIAN_POINT('Ctrl Pts',(-20.8319236734385,18.9184925560489,
0.471296450099625));
#193183=CARTESIAN_POINT('Ctrl Pts',(-20.8207776608864,18.8473712681642,
0.466977728597429));
#193184=CARTESIAN_POINT('Ctrl Pts',(-20.806023944847,18.7769426627958,0.462659007095234));
#193185=CARTESIAN_POINT('Ctrl Pts',(-20.791280057372,18.7065609752404,0.458343162619601));
#193186=CARTESIAN_POINT('Ctrl Pts',(-20.7729333325562,18.6368715401201,
0.454027318143968));
#193187=CARTESIAN_POINT('Ctrl Pts',(-20.7510747141467,18.5682725324448,
0.449711473668335));
#193188=CARTESIAN_POINT('Ctrl Pts',(-20.7292229865185,18.4996951501417,
0.445396989733422));
#193189=CARTESIAN_POINT('Ctrl Pts',(-20.7038617126699,18.4322079861377,
0.441082505798508));
#193190=CARTESIAN_POINT('Ctrl Pts',(-20.6751318568351,18.3661946292903,
0.436768021863595));
#193191=CARTESIAN_POINT('Ctrl Pts',(-20.6464009762914,18.3001789179419,
0.432453384043816));
#193192=CARTESIAN_POINT('Ctrl Pts',(-20.6143014765397,18.2356375721218,
0.428138746224037));
#193193=CARTESIAN_POINT('Ctrl Pts',(-20.5790219308427,18.1729330104904,
0.423824108404258));
#193194=CARTESIAN_POINT('Ctrl Pts',(-20.5437074960946,18.1101664383482,
0.419505203703596));
#193195=CARTESIAN_POINT('Ctrl Pts',(-20.5052069868332,18.0492407068168,
0.415186299002933));
#193196=CARTESIAN_POINT('Ctrl Pts',(-20.4637537219139,17.9904914742105,
0.410867394302271));
#193197=CARTESIAN_POINT('Ctrl Pts',(-20.4222758014217,17.9317072987355,
0.406545920803466));
#193198=CARTESIAN_POINT('Ctrl Pts',(-20.377841940606,17.8751025856419,0.402224447304661));
#193199=CARTESIAN_POINT('Ctrl Pts',(-20.3307256272438,17.8209797586716,
0.397902973805856));
#193200=CARTESIAN_POINT('Ctrl Pts',(-20.2835347249498,17.7667712508921,
0.393574659065255));
#193201=CARTESIAN_POINT('Ctrl Pts',(-20.233653247686,17.7150528185668,0.389246344324653));
#193202=CARTESIAN_POINT('Ctrl Pts',(-20.1813905470417,17.6660891273817,
0.384918029584051));
#193203=CARTESIAN_POINT('Ctrl Pts',(-20.1677437875061,17.6533038003446,
0.383787826404133));
#193204=CARTESIAN_POINT('Ctrl Pts',(-20.1539348347408,17.6407060782365,
0.382657623224215));
#193205=CARTESIAN_POINT('Ctrl Pts',(-20.139969531998,17.6283001942588,0.381527420044297));
#193206=CARTESIAN_POINT('Ctrl Pts',(-20.0856806361701,17.5800734028086,
0.377133853801673));
#193207=CARTESIAN_POINT('Ctrl Pts',(-20.028804456646,17.534551575879,0.372740287559048));
#193208=CARTESIAN_POINT('Ctrl Pts',(-19.9696413059749,17.4920236874905,
0.368346721316423));
#193209=CARTESIAN_POINT('Ctrl Pts',(-19.9105644543722,17.4495578329374,
0.363959563804056));
#193210=CARTESIAN_POINT('Ctrl Pts',(-19.8492076419245,17.410077525157,0.359572406291689));
#193211=CARTESIAN_POINT('Ctrl Pts',(-19.7859055363077,17.3738326851685,
0.355185248779322));
#193212=CARTESIAN_POINT('Ctrl Pts',(-19.7226758978492,17.3376293376474,
0.350803113609178));
#193213=CARTESIAN_POINT('Ctrl Pts',(-19.6575058056516,17.3046543374869,
0.346420978439034));
#193214=CARTESIAN_POINT('Ctrl Pts',(-19.5907589079216,17.2751143696755,
0.342038843268889));
#193215=CARTESIAN_POINT('Ctrl Pts',(-19.52405315142,17.2455926096101,0.337659409144484));
#193216=CARTESIAN_POINT('Ctrl Pts',(-19.4557729567064,17.219501874687,0.333279975020079));
#193217=CARTESIAN_POINT('Ctrl Pts',(-19.3863053176005,17.1970022908081,
0.328900540895673));
#193218=CARTESIAN_POINT('Ctrl Pts',(-19.3168577535507,17.1745092089554,
0.324522372358903));
#193219=CARTESIAN_POINT('Ctrl Pts',(-19.2462238836977,17.1556053656812,
0.320144203822133));
#193220=CARTESIAN_POINT('Ctrl Pts',(-19.1748077989579,17.1404016602977,
0.315766035285362));
#193221=CARTESIAN_POINT('Ctrl Pts',(-19.1033889720518,17.1251973711369,
0.31138769863987));
#193222=CARTESIAN_POINT('Ctrl Pts',(-19.0311883413905,17.1136936001516,
0.307009361994378));
#193223=CARTESIAN_POINT('Ctrl Pts',(-18.9586205452229,17.1059502118326,
0.302631025348886));
#193224=CARTESIAN_POINT('Ctrl Pts',(-18.8859767969382,17.0981987189993,
0.298248106175672));
#193225=CARTESIAN_POINT('Ctrl Pts',(-18.8129655950943,17.0942155178377,
0.293865187002457));
#193226=CARTESIAN_POINT('Ctrl Pts',(-18.7400062483051,17.0940085203333,
0.289482267829242));
#193227=CARTESIAN_POINT('Ctrl Pts',(-18.667006546944,17.0938014083365,0.285096924417947));
#193228=CARTESIAN_POINT('Ctrl Pts',(-18.5940592383891,17.0973746352134,
0.280711581006652));
#193229=CARTESIAN_POINT('Ctrl Pts',(-18.5215804684088,17.1046840354309,
0.276326237595358));
#193230=CARTESIAN_POINT('Ctrl Pts',(-18.4489736078897,17.1120063534313,
0.27193314403874));
#193231=CARTESIAN_POINT('Ctrl Pts',(-18.3768374152679,17.1230779575914,
0.267540050482122));
#193232=CARTESIAN_POINT('Ctrl Pts',(-18.3055792094826,17.1378032832718,
0.263146956925504));
#193233=CARTESIAN_POINT('Ctrl Pts',(-18.2580242315412,17.1476303976399,
0.260215175737957));
#193234=CARTESIAN_POINT('Ctrl Pts',(-18.2108600441032,17.159083715391,0.257283394550411));
#193235=CARTESIAN_POINT('Ctrl Pts',(-18.1642034381997,17.1721226426878,
0.254351613362864));
#193236=CARTESIAN_POINT('Ctrl Pts',(-18.0951058972849,17.1914330446111,
0.250009701502008));
#193237=CARTESIAN_POINT('Ctrl Pts',(-18.0268399854881,17.2143024101294,
0.245667789641151));
#193238=CARTESIAN_POINT('Ctrl Pts',(-17.9598043906284,17.2406421242755,
0.241325877780295));
#193239=CARTESIAN_POINT('Ctrl Pts',(-17.8928697395248,17.266942175468,0.236990504071199));
#193240=CARTESIAN_POINT('Ctrl Pts',(-17.8271621848896,17.29670202984,0.232655130362104));
#193241=CARTESIAN_POINT('Ctrl Pts',(-17.7630669345953,17.3297828454684,
0.228319756653008));
#193242=CARTESIAN_POINT('Ctrl Pts',(-17.6990453506667,17.3628256404409,
0.223989365703531));
#193243=CARTESIAN_POINT('Ctrl Pts',(-17.6366328289127,17.3991815955315,
0.219658974754055));
#193244=CARTESIAN_POINT('Ctrl Pts',(-17.5761945067699,17.4386638468264,
0.215328583804578));
#193245=CARTESIAN_POINT('Ctrl Pts',(-17.5157933283169,17.4781218334421,
0.211000854191369));
#193246=CARTESIAN_POINT('Ctrl Pts',(-17.4573643561353,17.5207020380533,
0.206673124578159));
#193247=CARTESIAN_POINT('Ctrl Pts',(-17.4012466091922,17.5661725320599,
0.20234539496495));
#193248=CARTESIAN_POINT('Ctrl Pts',(-17.3451439091012,17.6116308340625,
0.198018825745928));
#193249=CARTESIAN_POINT('Ctrl Pts',(-17.2913515880727,17.6599775776502,
0.193692256526906));
#193250=CARTESIAN_POINT('Ctrl Pts',(-17.2401767514859,17.7109396338151,
0.189365687307884));
#193251=CARTESIAN_POINT('Ctrl Pts',(-17.1889979072007,17.7619056810148,
0.185038779258574));
#193252=CARTESIAN_POINT('Ctrl Pts',(-17.140437302276,17.8154870975617,0.180711871209265));
#193253=CARTESIAN_POINT('Ctrl Pts',(-17.09476491744,17.8713741775763,0.176384963159955));
#193254=CARTESIAN_POINT('Ctrl Pts',(-17.049037723187,17.9273283252134,0.172052862578918));
#193255=CARTESIAN_POINT('Ctrl Pts',(-17.0062059805784,17.9855932764929,
0.167720761997882));
#193256=CARTESIAN_POINT('Ctrl Pts',(-16.9664985330236,18.0458272384593,
0.163388661416845));
#193257=CARTESIAN_POINT('Ctrl Pts',(-16.9267665792057,18.1060983750469,
0.159053887191356));
#193258=CARTESIAN_POINT('Ctrl Pts',(-16.890163004568,18.1683405133194,0.154719112965868));
#193259=CARTESIAN_POINT('Ctrl Pts',(-16.8568710208892,18.2321865367791,
0.150384338740379));
#193260=CARTESIAN_POINT('Ctrl Pts',(-16.8235119906462,18.2961611394354,
0.146040834734134));
#193261=CARTESIAN_POINT('Ctrl Pts',(-16.7934780711976,18.3617456271073,
0.141697330727888));
#193262=CARTESIAN_POINT('Ctrl Pts',(-16.7669043702655,18.4285526960368,
0.137353826721643));
#193263=CARTESIAN_POINT('Ctrl Pts',(-16.7461478827045,18.4807351187546,
0.133961153374905));
#193264=CARTESIAN_POINT('Ctrl Pts',(-16.7275015133356,18.5336630097783,
0.130568480028167));
#193265=CARTESIAN_POINT('Ctrl Pts',(-16.7110080390405,18.5871470318309,
0.127175806681429));
#193266=CARTESIAN_POINT('Ctrl Pts',(-16.6890808417458,18.6582511959801,
0.122665427818863));
#193267=CARTESIAN_POINT('Ctrl Pts',(-16.6708715522275,18.7306260888239,
0.118155048956298));
#193268=CARTESIAN_POINT('Ctrl Pts',(-16.6565194459451,18.8038593025457,
0.113644670093733));
#193269=CARTESIAN_POINT('Ctrl Pts',(-16.6414519720022,18.8807427590775,
0.108909475506494));
#193270=CARTESIAN_POINT('Ctrl Pts',(-16.6306364414031,18.9585718864235,
0.104174280919254));
#193271=CARTESIAN_POINT('Ctrl Pts',(-16.624175177866,19.0368500074442,0.0994390863320154));
#193272=CARTESIAN_POINT('Ctrl Pts',(-16.6180411415214,19.1111637754199,
0.0949437031101447));
#193273=CARTESIAN_POINT('Ctrl Pts',(-16.6158311470803,19.18588164953,0.090448319888274));
#193274=CARTESIAN_POINT('Ctrl Pts',(-16.6175803959886,19.2605687376906,
0.0859529366664034));
#193275=CARTESIAN_POINT('Ctrl Pts',(-16.6193280001048,19.3351855987192,
0.0814617803849421));
#193276=CARTESIAN_POINT('Ctrl Pts',(-16.6250274372589,19.4097712832384,
0.0769706241034808));
#193277=CARTESIAN_POINT('Ctrl Pts',(-16.6346618981062,19.4838892338239,
0.0724794678220195));
#193278=CARTESIAN_POINT('Ctrl Pts',(-16.6442898170097,19.5579568572063,
0.0679913611032202));
#193279=CARTESIAN_POINT('Ctrl Pts',(-16.6578473889511,19.6315569329051,
0.0635032543844209));
#193280=CARTESIAN_POINT('Ctrl Pts',(-16.6752659458499,19.7042576347942,
0.0590151476656216));
#193281=CARTESIAN_POINT('Ctrl Pts',(-16.6926772219334,19.7769279483805,
0.0545289169389693));
#193282=CARTESIAN_POINT('Ctrl Pts',(-16.7139461674509,19.848699198966,0.0500426862123171));
#193283=CARTESIAN_POINT('Ctrl Pts',(-16.7389532085404,19.9191506194919,
0.0455564554856648));
#193284=CARTESIAN_POINT('Ctrl Pts',(-16.7639633583527,19.9896107981087,
0.0410696670581777));
#193285=CARTESIAN_POINT('Ctrl Pts',(-16.7927123885947,20.0587503922127,
0.0365828786306905));
#193286=CARTESIAN_POINT('Ctrl Pts',(-16.8250314087852,20.1261655138582,
0.0320960902032033));
#193287=CARTESIAN_POINT('Ctrl Pts',(-16.8573519842582,20.1935838797096,
0.0276090858587915));
#193288=CARTESIAN_POINT('Ctrl Pts',(-16.8932426902262,20.2592772053157,
0.0231220815143796));
#193289=CARTESIAN_POINT('Ctrl Pts',(-16.932487950158,20.3228648003575,0.0186350771699677));
#193290=CARTESIAN_POINT('Ctrl Pts',(-16.9717602972259,20.3864962836509,
0.0141449758885641));
#193291=CARTESIAN_POINT('Ctrl Pts',(-17.0143915779344,20.4480187554704,
0.00965487460716038));
#193292=CARTESIAN_POINT('Ctrl Pts',(-17.0601224600125,20.5070798513692,
0.0051647733257567));
#193293=CARTESIAN_POINT('Ctrl Pts',(-17.0776565589201,20.5297250103958,
0.00344318221716946));
#193294=CARTESIAN_POINT('Ctrl Pts',(-17.0956458992255,20.5520086551532,
0.00172159110858221));
#193295=CARTESIAN_POINT('Ctrl Pts',(-17.1140743056112,20.5739122292573,
-5.04250086090388E-15));
#193296=CARTESIAN_POINT('Ctrl Pts',(-20.8509994310879,19.2125520223715,
0.490010528127495));
#193297=CARTESIAN_POINT('Ctrl Pts',(-20.8509485244656,19.2819899972947,
0.494577406431818));
#193298=CARTESIAN_POINT('Ctrl Pts',(-20.8474812586126,19.3513903947451,
0.499099088403655));
#193299=CARTESIAN_POINT('Ctrl Pts',(-20.8382973967345,19.4437375097343,
0.504962354973714));
#193300=CARTESIAN_POINT('Ctrl Pts',(-20.835602110511,19.466935447343,0.506422052247473));
#193301=CARTESIAN_POINT('Ctrl Pts',(-20.8317146529006,19.4961663924751,
0.508240780883106));
#193302=CARTESIAN_POINT('Ctrl Pts',(-20.8308794508201,19.5022442397664,
0.508617812016216));
#193303=CARTESIAN_POINT('Ctrl Pts',(-20.8294395919533,19.5123948705701,
0.509245509884849));
#193304=CARTESIAN_POINT('Ctrl Pts',(-20.8288494591845,19.5164696311213,
0.50949695144284));
#193305=CARTESIAN_POINT('Ctrl Pts',(-20.8277537164569,19.5238830074484,
0.509953403504262));
#193306=CARTESIAN_POINT('Ctrl Pts',(-20.8272520009022,19.5272221728698,
0.510158628848267));
#193307=CARTESIAN_POINT('Ctrl Pts',(-20.8262053588598,19.5340764444855,
0.510579109141992));
#193308=CARTESIAN_POINT('Ctrl Pts',(-20.8256595644637,19.5375913647262,
0.510794307785923));
#193309=CARTESIAN_POINT('Ctrl Pts',(-20.8244066116742,19.5455284026313,
0.51127928381383));
#193310=CARTESIAN_POINT('Ctrl Pts',(-20.8236942817571,19.5499496480936,
0.511548763855699));
#193311=CARTESIAN_POINT('Ctrl Pts',(-20.8214988308291,19.5633062157398,
0.512360924113693));
#193312=CARTESIAN_POINT('Ctrl Pts',(-20.8199723679794,19.5722344461074,
0.512901190399044));
#193313=CARTESIAN_POINT('Ctrl Pts',(-20.8078159804437,19.6406889785574,
0.517025262324955));
#193314=CARTESIAN_POINT('Ctrl Pts',(-20.7946963208786,19.69975090938,0.52047760042993));
#193315=CARTESIAN_POINT('Ctrl Pts',(-20.7741781413724,19.7764374678371,
0.52491533155393));
#193316=CARTESIAN_POINT('Ctrl Pts',(-20.7690474666048,19.7946336297256,
0.525964916091698));
#193317=CARTESIAN_POINT('Ctrl Pts',(-20.7520374606963,19.8520067038969,
0.529270205287377));
#193318=CARTESIAN_POINT('Ctrl Pts',(-20.7392650272457,19.8909096372322,
0.531505467687245));
#193319=CARTESIAN_POINT('Ctrl Pts',(-20.724446703344,19.9319843000659,0.533880820955069));
#193320=CARTESIAN_POINT('Ctrl Pts',(-20.7235161259709,19.9345482181418,
0.534029156379));
#193321=CARTESIAN_POINT('Ctrl Pts',(-20.7225806064217,19.9371103027527,
0.534177455193948));
#193322=CARTESIAN_POINT('Origin',(-18.734,19.211,0.));
#193323=CARTESIAN_POINT('',(-20.7225807924205,19.937109793362,1.55576067791234));
#193324=CARTESIAN_POINT('',(-20.7225806064482,19.93711030268,1.33163204998037));
#193325=CARTESIAN_POINT('',(-20.7225806064498,19.9371103026755,0.));
#193326=CARTESIAN_POINT('',(-20.8509996091576,19.212286400548,1.51094372094299));
#193327=CARTESIAN_POINT('Ctrl Pts',(-20.7225807924205,19.937109793362,1.55576067791233));
#193328=CARTESIAN_POINT('Ctrl Pts',(-20.7518560701808,19.8569342392254,
1.55013149406959));
#193329=CARTESIAN_POINT('Ctrl Pts',(-20.776275590636,19.7750071948395,1.54446141602598));
#193330=CARTESIAN_POINT('Ctrl Pts',(-20.8019773243859,19.664791125207,1.53708125042421));
#193331=CARTESIAN_POINT('Ctrl Pts',(-20.80773922883,19.6376876057867,1.53528611986878));
#193332=CARTESIAN_POINT('Ctrl Pts',(-20.8211288695143,19.5680050856512,
1.53073311432502));
#193333=CARTESIAN_POINT('Ctrl Pts',(-20.8279872948907,19.5252886365728,
1.52800095498755));
#193334=CARTESIAN_POINT('Ctrl Pts',(-20.8344943181864,19.4749486713284,
1.52487275427425));
#193335=CARTESIAN_POINT('Ctrl Pts',(-20.8354165131656,19.4675032628571,
1.52441242682007));
#193336=CARTESIAN_POINT('Ctrl Pts',(-20.8368427997025,19.4554637325832,
1.52367201175446));
#193337=CARTESIAN_POINT('Ctrl Pts',(-20.8373714515695,19.4508726630248,
1.52339059474849));
#193338=CARTESIAN_POINT('Ctrl Pts',(-20.8382824843403,19.4427261589683,
1.52289293101392));
#193339=CARTESIAN_POINT('Ctrl Pts',(-20.8386708947665,19.4391714532004,
1.52267634874263));
#193340=CARTESIAN_POINT('Ctrl Pts',(-20.8394063456645,19.4322789646659,
1.52225751842798));
#193341=CARTESIAN_POINT('Ctrl Pts',(-20.8397544548719,19.4289413607279,
1.52205520894178));
#193342=CARTESIAN_POINT('Ctrl Pts',(-20.840503712184,19.4215882136833,1.52161057875839));
#193343=CARTESIAN_POINT('Ctrl Pts',(-20.8409013184691,19.4175723118643,
1.52136845553285));
#193344=CARTESIAN_POINT('Ctrl Pts',(-20.8418560173667,19.407640084005,1.52077133229358));
#193345=CARTESIAN_POINT('Ctrl Pts',(-20.842399690987,19.4017224619594,1.52041705831759));
#193346=CARTESIAN_POINT('Ctrl Pts',(-20.844583902401,19.3767968117948,1.51893080522986));
#193347=CARTESIAN_POINT('Ctrl Pts',(-20.8459924230598,19.3577687024684,
1.51781085531585));
#193348=CARTESIAN_POINT('Ctrl Pts',(-20.8496863092788,19.2966545343023,
1.51425338537026));
#193349=CARTESIAN_POINT('Ctrl Pts',(-20.8509723412249,19.2545169002474,
1.51186058233845));
#193350=CARTESIAN_POINT('Ctrl Pts',(-20.8509995586414,19.2123670084621,
1.50950273727475));
#193351=CARTESIAN_POINT('Ctrl Pts',(-20.7225806064499,19.9371103026755,
0.755484067882561));
#193352=CARTESIAN_POINT('Ctrl Pts',(-20.7109390597927,19.9689927230547,
0.757536139988532));
#193353=CARTESIAN_POINT('Ctrl Pts',(-20.6985367444623,20.0005784216913,
0.759588212094503));
#193354=CARTESIAN_POINT('Ctrl Pts',(-20.685389730172,20.0318331870602,0.761640284200474));
#193355=CARTESIAN_POINT('Ctrl Pts',(-20.6572744289615,20.0986724802413,
0.766028704574177));
#193356=CARTESIAN_POINT('Ctrl Pts',(-20.625666230531,20.1641959624094,0.770417124947881));
#193357=CARTESIAN_POINT('Ctrl Pts',(-20.5907099276933,20.2280138860434,
0.774805545321584));
#193358=CARTESIAN_POINT('Ctrl Pts',(-20.5558054909444,20.2917371204276,
0.779187454417423));
#193359=CARTESIAN_POINT('Ctrl Pts',(-20.5175630412173,20.3537594003653,
0.783569363513262));
#193360=CARTESIAN_POINT('Ctrl Pts',(-20.4761752764379,20.4137112314137,
0.787951272609101));
#193361=CARTESIAN_POINT('Ctrl Pts',(-20.4348361312034,20.4735926351085,
0.79232803413471));
#193362=CARTESIAN_POINT('Ctrl Pts',(-20.3903592835476,20.5314080265974,
0.796704795660318));
#193363=CARTESIAN_POINT('Ctrl Pts',(-20.3429822982407,20.5868142912284,
0.801081557185927));
#193364=CARTESIAN_POINT('Ctrl Pts',(-20.2956353500081,20.6421854282108,
0.805455543838661));
#193365=CARTESIAN_POINT('Ctrl Pts',(-20.2453922250265,20.6951501032064,
0.809829530491395));
#193366=CARTESIAN_POINT('Ctrl Pts',(-20.1925317157385,20.7453970262565,
0.814203517144128));
#193367=CARTESIAN_POINT('Ctrl Pts',(-20.1396872870245,20.7956286638058,
0.818576173196446));
#193368=CARTESIAN_POINT('Ctrl Pts',(-20.0842274041465,20.8431438586879,
0.822948829248764));
#193369=CARTESIAN_POINT('Ctrl Pts',(-20.0264676012165,20.8876682736325,
0.827321485301082));
#193370=CARTESIAN_POINT('Ctrl Pts',(-19.9687063209491,20.9321938273895,
0.831694253193947));
#193371=CARTESIAN_POINT('Ctrl Pts',(-19.908645387059,20.973728156449,0.836067021086812));
#193372=CARTESIAN_POINT('Ctrl Pts',(-19.8466319415337,21.0120383568039,
0.840439788979677));
#193373=CARTESIAN_POINT('Ctrl Pts',(-19.7845541598035,21.050388302296,0.844817093425684));
#193374=CARTESIAN_POINT('Ctrl Pts',(-19.7205202333155,21.0855071867432,
0.84919439787169));
#193375=CARTESIAN_POINT('Ctrl Pts',(-19.6549039955861,21.1172069223759,
0.853571702317697));
#193376=CARTESIAN_POINT('Ctrl Pts',(-19.5892519313151,21.1489239661007,
0.857951396776985));
#193377=CARTESIAN_POINT('Ctrl Pts',(-19.5220162805637,21.1772179568835,
0.862331091236272));
#193378=CARTESIAN_POINT('Ctrl Pts',(-19.4535905444954,21.2019491325176,
0.86671078569556));
#193379=CARTESIAN_POINT('Ctrl Pts',(-19.3850435794912,21.2267241240356,
0.871098239599312));
#193380=CARTESIAN_POINT('Ctrl Pts',(-19.3153027805434,21.2479235548028,
0.875485693503064));
#193381=CARTESIAN_POINT('Ctrl Pts',(-19.2447759063311,21.2654578295773,
0.879873147406816));
#193382=CARTESIAN_POINT('Ctrl Pts',(-19.1968576175474,21.2773711952502,
0.88285412856518));
#193383=CARTESIAN_POINT('Ctrl Pts',(-19.148576702708,21.2875936826828,0.885835109723544));
#193384=CARTESIAN_POINT('Ctrl Pts',(-19.1000625457264,21.2961108394079,
0.888816090881908));
#193385=CARTESIAN_POINT('Ctrl Pts',(-19.0286448051689,21.3086489546123,
0.893204396321412));
#193386=CARTESIAN_POINT('Ctrl Pts',(-18.9564428204743,21.3175380610284,
0.897592701760916));
#193387=CARTESIAN_POINT('Ctrl Pts',(-18.8838626621671,21.3226889407506,
0.90198100720042));
#193388=CARTESIAN_POINT('Ctrl Pts',(-18.8113901824199,21.3278321787243,
0.906362802232374));
#193389=CARTESIAN_POINT('Ctrl Pts',(-18.7385411199947,21.3292481656531,
0.910744597264328));
#193390=CARTESIAN_POINT('Ctrl Pts',(-18.6657304467397,21.3268989267207,
0.915126392296281));
#193391=CARTESIAN_POINT('Ctrl Pts',(-18.5930052775877,21.3245524465811,
0.919503041634105));
#193392=CARTESIAN_POINT('Ctrl Pts',(-18.5203188877622,21.3184495396718,
0.923879690971928));
#193393=CARTESIAN_POINT('Ctrl Pts',(-18.4480883541564,21.3086042359728,
0.928256340309752));
#193394=CARTESIAN_POINT('Ctrl Pts',(-18.3759035959188,21.2987651716352,
0.932630215990441));
#193395=CARTESIAN_POINT('Ctrl Pts',(-18.3041745974556,21.2851884812727,
0.937004091671129));
#193396=CARTESIAN_POINT('Ctrl Pts',(-18.2333139919643,21.2679400869635,
0.941377967351818));
#193397=CARTESIAN_POINT('Ctrl Pts',(-18.1624749209504,21.2506969344265,
0.945750513815436));
#193398=CARTESIAN_POINT('Ctrl Pts',(-18.0925041873641,21.2297844072208,
0.950123060279053));
#193399=CARTESIAN_POINT('Ctrl Pts',(-18.0238032403067,21.2053193231078,
0.954495606742671));
#193400=CARTESIAN_POINT('Ctrl Pts',(-17.9551005116343,21.1808536045441,
0.958868266599101));
#193401=CARTESIAN_POINT('Ctrl Pts',(-17.8876680885983,21.1528353098613,
0.963240926455532));
#193402=CARTESIAN_POINT('Ctrl Pts',(-17.8218896895733,21.121430260861,0.967613586311963));
#193403=CARTESIAN_POINT('Ctrl Pts',(-17.7560429990831,21.0899926069806,
0.971990785885884));
#193404=CARTESIAN_POINT('Ctrl Pts',(-17.6918541973568,21.0551613868326,
0.976367985459805));
#193405=CARTESIAN_POINT('Ctrl Pts',(-17.6296837664011,21.0171491234696,
0.980745185033726));
#193406=CARTESIAN_POINT('Ctrl Pts',(-17.5674793666564,20.9791160908995,
0.985124776229623));
#193407=CARTESIAN_POINT('Ctrl Pts',(-17.5072959315927,20.9378988273871,
0.98950436742552));
#193408=CARTESIAN_POINT('Ctrl Pts',(-17.4494639535034,20.8937525502138,
0.993883958621417));
#193409=CARTESIAN_POINT('Ctrl Pts',(-17.3915294631427,20.8495280198785,
0.998271313028188));
#193410=CARTESIAN_POINT('Ctrl Pts',(-17.3359551215016,20.8023644201836,
1.00265866743496));
#193411=CARTESIAN_POINT('Ctrl Pts',(-17.283036954651,20.7525561102443,1.00704602184173));
#193412=CARTESIAN_POINT('Ctrl Pts',(-17.2470699990045,20.7187028348753,
1.0100279804156));
#193413=CARTESIAN_POINT('Ctrl Pts',(-17.2123293106136,20.6836286139468,
1.01300993898947));
#193414=CARTESIAN_POINT('Ctrl Pts',(-17.1788971524539,20.6474345211509,
1.01599189756334));
#193415=CARTESIAN_POINT('Ctrl Pts',(-17.1297000977299,20.5941731446206,
1.0203799953476));
#193416=CARTESIAN_POINT('Ctrl Pts',(-17.0831463850142,20.5382773695794,
1.02476809313186));
#193417=CARTESIAN_POINT('Ctrl Pts',(-17.039530835554,20.4800402872808,1.02915619091612));
#193418=CARTESIAN_POINT('Ctrl Pts',(-16.9959800381062,20.4218896642455,
1.03353777409341));
#193419=CARTESIAN_POINT('Ctrl Pts',(-16.9553590315084,20.3614050170529,
1.0379193572707));
#193420=CARTESIAN_POINT('Ctrl Pts',(-16.9179243722069,20.298914663076,1.04230094044799));
#193421=CARTESIAN_POINT('Ctrl Pts',(-16.8805337207632,20.2364977722124,
1.04667737267444));
#193422=CARTESIAN_POINT('Ctrl Pts',(-16.8463222221597,20.1720802703032,
1.05105380490089));
#193423=CARTESIAN_POINT('Ctrl Pts',(-16.8155038475772,20.1060203981691,
1.05543023712734));
#193424=CARTESIAN_POINT('Ctrl Pts',(-16.7847050267982,20.0400024400483,
1.05980389257218));
#193425=CARTESIAN_POINT('Ctrl Pts',(-16.7572952618898,19.9723446153759,
1.06417754801702));
#193426=CARTESIAN_POINT('Ctrl Pts',(-16.7334424881414,19.90342952114,1.06855120346186));
#193427=CARTESIAN_POINT('Ctrl Pts',(-16.7095969789008,19.8345354154166,
1.07292352688325));
#193428=CARTESIAN_POINT('Ctrl Pts',(-16.6893064678243,19.7643852559182,
1.07729585030464));
#193429=CARTESIAN_POINT('Ctrl Pts',(-16.6726900427937,19.6933797884677,
1.08166817372603));
#193430=CARTESIAN_POINT('Ctrl Pts',(-16.6560731962969,19.6223725200037,
1.08604060804893));
#193431=CARTESIAN_POINT('Ctrl Pts',(-16.6431307288416,19.5505103706869,
1.09041304237183));
#193432=CARTESIAN_POINT('Ctrl Pts',(-16.6339309271711,19.4782057060532,
1.09478547669473));
#193433=CARTESIAN_POINT('Ctrl Pts',(-16.6247215785514,19.4058260083939,
1.09916244844239));
#193434=CARTESIAN_POINT('Ctrl Pts',(-16.6192627111906,19.3330033581393,
1.10353942019006));
#193435=CARTESIAN_POINT('Ctrl Pts',(-16.6175707663535,19.2601558640094,
1.10791639193772));
#193436=CARTESIAN_POINT('Ctrl Pts',(-16.6158778976532,19.1872685925062,
1.11229575367068));
#193437=CARTESIAN_POINT('Ctrl Pts',(-16.6179560329377,19.1143569326632,
1.11667511540364));
#193438=CARTESIAN_POINT('Ctrl Pts',(-16.623769481391,19.0418368883857,1.1210544771366));
#193439=CARTESIAN_POINT('Ctrl Pts',(-16.6295932350961,18.9691882909213,
1.12544160197716));
#193440=CARTESIAN_POINT('Ctrl Pts',(-16.6391654612832,18.8969331739607,
1.12982872681773));
#193441=CARTESIAN_POINT('Ctrl Pts',(-16.6523989007771,18.8254797492814,
1.13421585165829));
#193442=CARTESIAN_POINT('Ctrl Pts',(-16.6613997691414,18.7768799223047,
1.13719980252045));
#193443=CARTESIAN_POINT('Ctrl Pts',(-16.6720933107671,18.7286507595593,
1.14018375338261));
#193444=CARTESIAN_POINT('Ctrl Pts',(-16.6844389800457,18.6809163976466,
1.14316770424478));
#193445=CARTESIAN_POINT('Ctrl Pts',(-16.7025947167718,18.610717489178,1.14755594963142));
#193446=CARTESIAN_POINT('Ctrl Pts',(-16.7243966036732,18.5413154212983,
1.15194419501807));
#193447=CARTESIAN_POINT('Ctrl Pts',(-16.7497577469366,18.4731167564189,
1.15633244040472));
#193448=CARTESIAN_POINT('Ctrl Pts',(-16.7750812523751,18.4050193034357,
1.1607141733085));
#193449=CARTESIAN_POINT('Ctrl Pts',(-16.803953361538,18.3381221564993,1.16509590621228));
#193450=CARTESIAN_POINT('Ctrl Pts',(-16.8362368499008,18.2728187669083,
1.16947763911606));
#193451=CARTESIAN_POINT('Ctrl Pts',(-16.8684824054041,18.207592108316,1.17385422351616));
#193452=CARTESIAN_POINT('Ctrl Pts',(-16.9041311647913,18.1439559172984,
1.17823080791626));
#193453=CARTESIAN_POINT('Ctrl Pts',(-16.942997693185,18.0822840317496,1.18260739231636));
#193454=CARTESIAN_POINT('Ctrl Pts',(-16.9818395748752,18.020651254625,1.18698120136238));
#193455=CARTESIAN_POINT('Ctrl Pts',(-17.0238949203893,17.9609807185433,
1.1913550104084));
#193456=CARTESIAN_POINT('Ctrl Pts',(-17.0689328981712,17.9036207335254,
1.19572881945443));
#193457=CARTESIAN_POINT('Ctrl Pts',(-17.1139571722399,17.8462782014402,
1.20010129768081));
#193458=CARTESIAN_POINT('Ctrl Pts',(-17.1619619791427,17.7912452038486,
1.2044737759072));
#193459=CARTESIAN_POINT('Ctrl Pts',(-17.2126747882375,17.7388387995685,
1.20884625413359));
#193460=CARTESIAN_POINT('Ctrl Pts',(-17.2633888949715,17.6864310543136,
1.21321884424293));
#193461=CARTESIAN_POINT('Ctrl Pts',(-17.3168108045951,17.6366503810584,
1.21759143435227));
#193462=CARTESIAN_POINT('Ctrl Pts',(-17.3726307197092,17.5897774111244,
1.22196402446161));
#193463=CARTESIAN_POINT('Ctrl Pts',(-17.4285085645615,17.5428557965647,
1.22634115243167));
#193464=CARTESIAN_POINT('Ctrl Pts',(-17.4867890134539,17.4988482210374,
1.23071828040173));
#193465=CARTESIAN_POINT('Ctrl Pts',(-17.547129377997,17.4579948298347,1.23509540837179));
#193466=CARTESIAN_POINT('Ctrl Pts',(-17.6075026960962,17.4171191274556,
1.23947492681353));
#193467=CARTESIAN_POINT('Ctrl Pts',(-17.669937756504,17.3794012886564,1.24385444525527));
#193468=CARTESIAN_POINT('Ctrl Pts',(-17.7340654232695,17.3450364842101,
1.248233963697));
#193469=CARTESIAN_POINT('Ctrl Pts',(-17.7983067483476,17.3106107724227,
1.25262124429041));
#193470=CARTESIAN_POINT('Ctrl Pts',(-17.8642462337679,17.2795501683287,
1.25700852488382));
#193471=CARTESIAN_POINT('Ctrl Pts',(-17.9314933831593,17.2520022639301,
1.26139580547722));
#193472=CARTESIAN_POINT('Ctrl Pts',(-17.9772094535304,17.2332746011599,
1.26437837396022));
#193473=CARTESIAN_POINT('Ctrl Pts',(-18.0235294697532,17.2161693410616,
1.26736094244321));
#193474=CARTESIAN_POINT('Ctrl Pts',(-18.0703272881676,17.2007195390769,
1.27034351092621));
#193475=CARTESIAN_POINT('Ctrl Pts',(-18.1391803751295,17.1779884247721,
1.2747317293109));
#193476=CARTESIAN_POINT('Ctrl Pts',(-18.2093370328472,17.1587544122963,
1.27911994769558));
#193477=CARTESIAN_POINT('Ctrl Pts',(-18.2804083779596,17.1431645035413,
1.28350816608027));
#193478=CARTESIAN_POINT('Ctrl Pts',(-18.3513742462393,17.1275977317368,
1.28788987191936));
#193479=CARTESIAN_POINT('Ctrl Pts',(-18.4232516398406,17.1156644301232,
1.29227157775844));
#193480=CARTESIAN_POINT('Ctrl Pts',(-18.4956354563143,17.1074621837691,
1.29665328359752));
#193481=CARTESIAN_POINT('Ctrl Pts',(-18.5679342224827,17.0992695749775,
1.30102984097336));
#193482=CARTESIAN_POINT('Ctrl Pts',(-18.6407377525394,17.0947993667338,
1.3054063983492));
#193483=CARTESIAN_POINT('Ctrl Pts',(-18.7136313401116,17.0940979905309,
1.30978295572503));
#193484=CARTESIAN_POINT('Ctrl Pts',(-18.7864787035313,17.0933970590931,
1.31415673778602));
#193485=CARTESIAN_POINT('Ctrl Pts',(-18.8594155299897,17.0964602223804,
1.31853051984701));
#193486=CARTESIAN_POINT('Ctrl Pts',(-18.9320240054094,17.1032819227227,
1.322904301908));
#193487=CARTESIAN_POINT('Ctrl Pts',(-19.0046103894158,17.1101015475359,
1.32727675322865));
#193488=CARTESIAN_POINT('Ctrl Pts',(-19.0768681407482,17.120677394011,1.3316492045493));
#193489=CARTESIAN_POINT('Ctrl Pts',(-19.148383151568,17.1349519264486,1.33602165586994));
#193490=CARTESIAN_POINT('Ctrl Pts',(-19.219899994278,17.149226824535,1.34039421919296));
#193491=CARTESIAN_POINT('Ctrl Pts',(-19.2906735860492,17.1672005003068,
1.34476678251598));
#193492=CARTESIAN_POINT('Ctrl Pts',(-19.3603002769535,17.1887643650929,
1.349139345839));
#193493=CARTESIAN_POINT('Ctrl Pts',(-19.4299992325989,17.2103506107661,
1.35351644739516));
#193494=CARTESIAN_POINT('Ctrl Pts',(-19.4985484489852,17.235534342081,1.35789354895132));
#193495=CARTESIAN_POINT('Ctrl Pts',(-19.5655605152348,17.2641573999158,
1.36227065050748));
#193496=CARTESIAN_POINT('Ctrl Pts',(-19.632609181428,17.2927960907905,1.3666501427028));
#193497=CARTESIAN_POINT('Ctrl Pts',(-19.6981185924442,17.3248776358673,
1.37102963489813));
#193498=CARTESIAN_POINT('Ctrl Pts',(-19.7617248384167,17.3601972940096,
1.37540912709345));
#193499=CARTESIAN_POINT('Ctrl Pts',(-19.8254438274278,17.3955795567832,
1.37979638200532));
#193500=CARTESIAN_POINT('Ctrl Pts',(-19.8872525054644,17.4342111384903,
1.38418363691718));
#193501=CARTESIAN_POINT('Ctrl Pts',(-19.9468154069978,17.4758435838379,
1.38857089182904));
#193502=CARTESIAN_POINT('Ctrl Pts',(-19.9873110558898,17.5041486671347,
1.39155370042191));
#193503=CARTESIAN_POINT('Ctrl Pts',(-20.0267692619178,17.5338399735792,
1.39453650901478));
#193504=CARTESIAN_POINT('Ctrl Pts',(-20.0650939283882,17.5648293059928,
1.39751931760765));
#193505=CARTESIAN_POINT('Ctrl Pts',(-20.1207402998965,17.6098249723118,
1.4018502744139));
#193506=CARTESIAN_POINT('Ctrl Pts',(-20.1742249041617,17.6577445690432,
1.40618123122015));
#193507=CARTESIAN_POINT('Ctrl Pts',(-20.2252181563952,17.7083498710487,
1.4105121880264));
#193508=CARTESIAN_POINT('Ctrl Pts',(-20.2761246600306,17.7588690844285,
1.41483577710427));
#193509=CARTESIAN_POINT('Ctrl Pts',(-20.3245478783115,17.8120645847693,
1.41915936618215));
#193510=CARTESIAN_POINT('Ctrl Pts',(-20.3701907287601,17.8676575644611,
1.42348295526002));
#193511=CARTESIAN_POINT('Ctrl Pts',(-20.415790130129,17.9231976231856,1.42780242855714));
#193512=CARTESIAN_POINT('Ctrl Pts',(-20.4586140966688,17.9811302563624,
1.43212190185425));
#193513=CARTESIAN_POINT('Ctrl Pts',(-20.4984028945192,18.0411404247464,
1.43644137515136));
#193514=CARTESIAN_POINT('Ctrl Pts',(-20.5381677566161,18.101114492804,1.44075824998224));
#193515=CARTESIAN_POINT('Ctrl Pts',(-20.5749007972635,18.1631632051077,
1.44507512481312));
#193516=CARTESIAN_POINT('Ctrl Pts',(-20.6083841924735,18.2269406018916,
1.44939199964401));
#193517=CARTESIAN_POINT('Ctrl Pts',(-20.6418591738518,18.2907019724546,
1.45370778971456));
#193518=CARTESIAN_POINT('Ctrl Pts',(-20.672085900762,18.3561907258456,1.45802357978511));
#193519=CARTESIAN_POINT('Ctrl Pts',(-20.6988922453411,18.423035873787,1.46233936985566));
#193520=CARTESIAN_POINT('Ctrl Pts',(-20.7257171930929,18.489927411188,1.46665815501524));
#193521=CARTESIAN_POINT('Ctrl Pts',(-20.7491168291636,18.5581767631563,
1.47097694017482));
#193522=CARTESIAN_POINT('Ctrl Pts',(-20.7689674532606,18.6273935708287,
1.47529572533439));
#193523=CARTESIAN_POINT('Ctrl Pts',(-20.7888248459354,18.6966339797413,
1.47961598309418));
#193524=CARTESIAN_POINT('Ctrl Pts',(-20.8051307022979,18.7668420178477,
1.48393624085397));
#193525=CARTESIAN_POINT('Ctrl Pts',(-20.8178121286519,18.8376154629832,
1.48825649861375));
#193526=CARTESIAN_POINT('Ctrl Pts',(-20.8305133213042,18.908499221343,1.49258349027723));
#193527=CARTESIAN_POINT('Ctrl Pts',(-20.8395787385446,18.9799496538715,
1.49691048194071));
#193528=CARTESIAN_POINT('Ctrl Pts',(-20.8449873102489,19.0515585500307,
1.50123747360419));
#193529=CARTESIAN_POINT('Ctrl Pts',(-20.8490314544484,19.1051025756753,
1.50447288938379));
#193530=CARTESIAN_POINT('Ctrl Pts',(-20.8510321497683,19.1587350706587,
1.50770830516339));
#193531=CARTESIAN_POINT('Ctrl Pts',(-20.8509996091576,19.212286400548,1.51094372094299));
#193532=CARTESIAN_POINT('Ctrl Pts',(-20.7225806064217,19.9371103027527,
0.534177455193948));
#193533=CARTESIAN_POINT('Ctrl Pts',(-20.7114374698477,19.9676277395686,
0.535943868253035));
#193534=CARTESIAN_POINT('Ctrl Pts',(-20.6995931583947,19.9978850480326,
0.537705158541846));
#193535=CARTESIAN_POINT('Ctrl Pts',(-20.6589746514824,20.0950013681374,
0.543420670497742));
#193536=CARTESIAN_POINT('Ctrl Pts',(-20.6274494476113,20.1606495982188,
0.547383443423855));
#193537=CARTESIAN_POINT('Ctrl Pts',(-20.5661685037545,20.2730250582085,
0.554496407985185));
#193538=CARTESIAN_POINT('Ctrl Pts',(-20.5378441393874,20.3204522608092,
0.557608779156871));
#193539=CARTESIAN_POINT('Ctrl Pts',(-20.4889707980559,20.3954591389319,
0.562757557262939));
#193540=CARTESIAN_POINT('Ctrl Pts',(-20.4695469282906,20.4237417762343,
0.564754091976727));
#193541=CARTESIAN_POINT('Ctrl Pts',(-20.4431388558086,20.4602594569332,
0.567411436815425));
#193542=CARTESIAN_POINT('Ctrl Pts',(-20.4367661664181,20.4689317132342,
0.56804855313285));
#193543=CARTESIAN_POINT('Ctrl Pts',(-20.426225873687,20.4830485833113,0.569095795672003));
#193544=CARTESIAN_POINT('Ctrl Pts',(-20.422097403048,20.4885222745581,0.569504380689825));
#193545=CARTESIAN_POINT('Ctrl Pts',(-20.4140585932407,20.4990734427671,
0.570296928178457));
#193546=CARTESIAN_POINT('Ctrl Pts',(-20.4101516393926,20.504153413573,0.570680753597797));
#193547=CARTESIAN_POINT('Ctrl Pts',(-20.401083709184,20.5158337467052,0.5715685206328));
#193548=CARTESIAN_POINT('Ctrl Pts',(-20.3959065203337,20.5224213336935,
0.572073108100753));
#193549=CARTESIAN_POINT('Ctrl Pts',(-20.3818932677003,20.540035908778,0.573432938593689));
#193550=CARTESIAN_POINT('Ctrl Pts',(-20.3729857963623,20.5510053031887,
0.574291057870885));
#193551=CARTESIAN_POINT('Ctrl Pts',(-20.2682894327803,20.6773313240747,
0.58430710600086));
#193552=CARTESIAN_POINT('Ctrl Pts',(-20.1606341987796,20.7822639584046,
0.593981499501864));
#193553=CARTESIAN_POINT('Ctrl Pts',(-19.9681110289533,20.9336998234509,
0.610137699571716));
#193554=CARTESIAN_POINT('Ctrl Pts',(-19.8895240311662,20.9873697509775,
0.616462819861445));
#193555=CARTESIAN_POINT('Ctrl Pts',(-19.7687998424279,21.0584047934686,
0.625584594307354));
#193556=CARTESIAN_POINT('Ctrl Pts',(-19.729283565231,21.0799907259246,0.628482435959696));
#193557=CARTESIAN_POINT('Ctrl Pts',(-19.6670847064776,21.111434381759,0.632877663235488));
#193558=CARTESIAN_POINT('Ctrl Pts',(-19.6448686052041,21.122181942398,0.634415809433181));
#193559=CARTESIAN_POINT('Ctrl Pts',(-19.6165125588766,21.1352930237958,
0.636334506882315));
#193560=CARTESIAN_POINT('Ctrl Pts',(-19.6105436868814,21.1380192592776,
0.636735918909718));
#193561=CARTESIAN_POINT('Ctrl Pts',(-19.6015000360848,21.1420991616775,
0.637340279196587));
#193562=CARTESIAN_POINT('Ctrl Pts',(-19.5984346187612,21.1434733051433,
0.637544468859004));
#193563=CARTESIAN_POINT('Ctrl Pts',(-19.5921230212518,21.1462846000517,
0.637963506613385));
#193564=CARTESIAN_POINT('Ctrl Pts',(-19.5888765445637,21.1477208617937,
0.638178292203626));
#193565=CARTESIAN_POINT('Ctrl Pts',(-19.581585601535,21.1509245162282,0.63865899169706));
#193566=CARTESIAN_POINT('Ctrl Pts',(-19.5775392164236,21.1526874289545,
0.638924629429125));
#193567=CARTESIAN_POINT('Ctrl Pts',(-19.5672279888454,21.1571414666062,
0.639598706191506));
#193568=CARTESIAN_POINT('Ctrl Pts',(-19.5609555503574,21.1598150271458,
0.640006098720852));
#193569=CARTESIAN_POINT('Ctrl Pts',(-19.5252605404774,21.174826278749,0.642310020582687));
#193570=CARTESIAN_POINT('Ctrl Pts',(-19.495573241086,21.1865286231352,0.644170573075016));
#193571=CARTESIAN_POINT('Ctrl Pts',(-19.2794566774673,21.2661224387947,
0.657394742669097));
#193572=CARTESIAN_POINT('Ctrl Pts',(-19.0845510714179,21.3081849084335,
0.667705270028045));
#193573=CARTESIAN_POINT('Ctrl Pts',(-18.8308754209566,21.3265206893776,
0.681839342496874));
#193574=CARTESIAN_POINT('Ctrl Pts',(-18.7749971092634,21.3283405967854,
0.684989197358653));
#193575=CARTESIAN_POINT('Ctrl Pts',(-18.6844318490127,21.3277038002695,
0.690198340708285));
#193576=CARTESIAN_POINT('Ctrl Pts',(-18.649761525261,21.3266076329026,0.692217031247737));
#193577=CARTESIAN_POINT('Ctrl Pts',(-18.6042836795442,21.3240501184867,
0.694903282787265));
#193578=CARTESIAN_POINT('Ctrl Pts',(-18.5934372163466,21.3233563203746,
0.695546808780345));
#193579=CARTESIAN_POINT('Ctrl Pts',(-18.5756919081778,21.3220839560979,
0.696604502968437));
#193580=CARTESIAN_POINT('Ctrl Pts',(-18.5687896233513,21.3215550102596,
0.697017111806223));
#193581=CARTESIAN_POINT('Ctrl Pts',(-18.5554413934161,21.3204662089668,
0.697817428969723));
#193582=CARTESIAN_POINT('Ctrl Pts',(-18.5489951691573,21.3199106367706,
0.698204998525948));
#193583=CARTESIAN_POINT('Ctrl Pts',(-18.5341276419443,21.3185605778978,
0.699101409454807));
#193584=CARTESIAN_POINT('Ctrl Pts',(-18.5257083933891,21.3177451560176,
0.699610903010173));
#193585=CARTESIAN_POINT('Ctrl Pts',(-18.5031019851936,21.3154188421011,
0.700984062019599));
#193586=CARTESIAN_POINT('Ctrl Pts',(-18.4889250260433,21.3138149699328,
0.701850632083286));
#193587=CARTESIAN_POINT('Ctrl Pts',(-18.3611862263606,21.2980542766511,
0.709709002707594));
#193588=CARTESIAN_POINT('Ctrl Pts',(-18.248948460074,21.2748564259868,0.716988808719096));
#193589=CARTESIAN_POINT('Ctrl Pts',(-17.9820744672696,21.1967201284121,
0.735129537826583));
#193590=CARTESIAN_POINT('Ctrl Pts',(-17.8308675718973,21.132673214878,0.746147032977224));
#193591=CARTESIAN_POINT('Ctrl Pts',(-17.6600530146194,21.0356645800402,
0.758629156568118));
#193592=CARTESIAN_POINT('Ctrl Pts',(-17.6319343410552,21.0188203764615,
0.76068315406141));
#193593=CARTESIAN_POINT('Ctrl Pts',(-17.5980616863358,20.9974451050083,
0.76314606236294));
#193594=CARTESIAN_POINT('Ctrl Pts',(-17.5919269198305,20.9935293963174,
0.76359165733612));
#193595=CARTESIAN_POINT('Ctrl Pts',(-17.5823436971568,20.9873428177069,
0.76428683906326));
#193596=CARTESIAN_POINT('Ctrl Pts',(-17.5788815510295,20.9850934066207,
0.764537805163716));
#193597=CARTESIAN_POINT('Ctrl Pts',(-17.5724290481779,20.9808742174639,
0.765005161661114));
#193598=CARTESIAN_POINT('Ctrl Pts',(-17.5694371343737,20.9789069981398,
0.765221711043567));
#193599=CARTESIAN_POINT('Ctrl Pts',(-17.5626239308124,20.9744024339311,
0.765714494814857));
#193600=CARTESIAN_POINT('Ctrl Pts',(-17.5588058968779,20.97186026145,0.765990401383822));
#193601=CARTESIAN_POINT('Ctrl Pts',(-17.547098640409,20.964010146944,0.766835764363602));
#193602=CARTESIAN_POINT('Ctrl Pts',(-17.5392367670136,20.9586613623376,
0.767402546263394));
#193603=CARTESIAN_POINT('Ctrl Pts',(-17.4690404166341,20.9102085642016,
0.772457519535672));
#193604=CARTESIAN_POINT('Ctrl Pts',(-17.4090192225959,20.8638342390826,
0.776740255607443));
#193605=CARTESIAN_POINT('Ctrl Pts',(-17.2444280988522,20.7219242508775,
0.788770466806824));
#193606=CARTESIAN_POINT('Ctrl Pts',(-17.1467824827809,20.618998372626,0.796293125138248));
#193607=CARTESIAN_POINT('Ctrl Pts',(-17.022285476647,20.4582146529618,0.807543735498695));
#193608=CARTESIAN_POINT('Ctrl Pts',(-16.9865976887691,20.4077018443386,
0.811013100431889));
#193609=CARTESIAN_POINT('Ctrl Pts',(-16.9330234067257,20.3243557103918,
0.81669936314064));
#193610=CARTESIAN_POINT('Ctrl Pts',(-16.9137060555985,20.2924838573702,
0.818865114738588));
#193611=CARTESIAN_POINT('Ctrl Pts',(-16.8897205357709,20.250445205352,0.821718259343063));
#193612=CARTESIAN_POINT('Ctrl Pts',(-16.8842769220177,20.2407269563917,
0.822377583893358));
#193613=CARTESIAN_POINT('Ctrl Pts',(-16.8755506591457,20.2248558443021,
0.823454136645717));
#193614=CARTESIAN_POINT('Ctrl Pts',(-16.87222122739,20.2187288452848,0.823869686985817));
#193615=CARTESIAN_POINT('Ctrl Pts',(-16.8658779938211,20.2069169494291,
0.824670757746429));
#193616=CARTESIAN_POINT('Ctrl Pts',(-16.8628597153497,20.2012345347806,
0.825056113291186));
#193617=CARTESIAN_POINT('Ctrl Pts',(-16.8560099819751,20.1881956251176,
0.825940349676464));
#193618=CARTESIAN_POINT('Ctrl Pts',(-16.8521957806587,20.1808302297633,
0.826439833340899));
#193619=CARTESIAN_POINT('Ctrl Pts',(-16.842181493918,20.1612106837186,0.827770418671016));
#193620=CARTESIAN_POINT('Ctrl Pts',(-16.8360572773322,20.1489184457796,
0.828604162700456));
#193621=CARTESIAN_POINT('Ctrl Pts',(-16.7905179108019,20.0552413115783,
0.834959650078114));
#193622=CARTESIAN_POINT('Ctrl Pts',(-16.7562390824143,19.9714761892541,
0.840658245854226));
#193623=CARTESIAN_POINT('Ctrl Pts',(-16.6828174720997,19.7531458591501,
0.855531878553615));
#193624=CARTESIAN_POINT('Ctrl Pts',(-16.6514759899623,19.6164142017218,
0.864883255525189));
#193625=CARTESIAN_POINT('Ctrl Pts',(-16.6269184297165,19.4229668070138,
0.877654126274579));
#193626=CARTESIAN_POINT('Ctrl Pts',(-16.6221165608976,19.368072730332,0.881223466303394));
#193627=CARTESIAN_POINT('Ctrl Pts',(-16.618091488661,19.2846711192318,0.8865082084408));
#193628=CARTESIAN_POINT('Ctrl Pts',(-16.6172932451848,19.256265439619,0.888283820194297));
#193629=CARTESIAN_POINT('Ctrl Pts',(-16.6170118446478,19.2209135315712,
0.890456405932284));
#193630=CARTESIAN_POINT('Ctrl Pts',(-16.616990724002,19.2139759749343,0.890880975800615));
#193631=CARTESIAN_POINT('Ctrl Pts',(-16.6170112720142,19.2029957409646,
0.891549994766704));
#193632=CARTESIAN_POINT('Ctrl Pts',(-16.6170304167401,19.1989531428592,
0.891795673262578));
#193633=CARTESIAN_POINT('Ctrl Pts',(-16.6170883596838,19.1913293931787,
0.892257758602559));
#193634=CARTESIAN_POINT('Ctrl Pts',(-16.617124664591,19.1877483289616,0.892474296362578));
#193635=CARTESIAN_POINT('Ctrl Pts',(-16.617228450216,19.179560689524,0.892968224096466));
#193636=CARTESIAN_POINT('Ctrl Pts',(-16.6173018807224,19.1749542376282,
0.89324527811114));
#193637=CARTESIAN_POINT('Ctrl Pts',(-16.6175368056402,19.1627225024376,
0.893978822222175));
#193638=CARTESIAN_POINT('Ctrl Pts',(-16.6177244726278,19.1550977096705,
0.89443388610738));
#193639=CARTESIAN_POINT('Ctrl Pts',(-16.6193295470784,19.1016328178291,
0.897610394406912));
#193640=CARTESIAN_POINT('Ctrl Pts',(-16.6221951265029,19.0558447313641,
0.900256665027179));
#193641=CARTESIAN_POINT('Ctrl Pts',(-16.6301237549122,18.9726387903883,
0.904988039765976));
#193642=CARTESIAN_POINT('Ctrl Pts',(-16.63470400901,18.9351959136889,0.907088386485106));
#193643=CARTESIAN_POINT('Ctrl Pts',(-16.6596402980374,18.768448723022,0.916388591586645));
#193644=CARTESIAN_POINT('Ctrl Pts',(-16.690960810843,18.6410770633278,0.92336600192118));
#193645=CARTESIAN_POINT('Ctrl Pts',(-16.762785710537,18.4339500931436,0.93546669699205));
#193646=CARTESIAN_POINT('Ctrl Pts',(-16.7969195885184,18.3523910980012,
0.940438786075902));
#193647=CARTESIAN_POINT('Ctrl Pts',(-16.8451366111527,18.2548068412481,
0.946782362698708));
#193648=CARTESIAN_POINT('Ctrl Pts',(-16.8544954963979,18.2365396181598,
0.947987380284465));
#193649=CARTESIAN_POINT('Ctrl Pts',(-16.8682706809051,18.2105893133332,
0.949725728871437));
#193650=CARTESIAN_POINT('Ctrl Pts',(-16.8724720934033,18.2027930354066,
0.950251454969338));
#193651=CARTESIAN_POINT('Ctrl Pts',(-16.8798389662669,18.1893258654414,
0.951165723955367));
#193652=CARTESIAN_POINT('Ctrl Pts',(-16.8829818528705,18.1836427136646,
0.951553456515558));
#193653=CARTESIAN_POINT('Ctrl Pts',(-16.8890741111731,18.1727450437957,
0.952300670518855));
#193654=CARTESIAN_POINT('Ctrl Pts',(-16.8920195687416,18.1675284004536,
0.952660008432743));
#193655=CARTESIAN_POINT('Ctrl Pts',(-16.8997914922062,18.1538991455451,
0.953603205191064));
#193656=CARTESIAN_POINT('Ctrl Pts',(-16.9046536566807,18.1455071479193,
0.954188351430258));
#193657=CARTESIAN_POINT('Ctrl Pts',(-16.9217169765652,18.1165173009355,
0.956225180389785));
#193658=CARTESIAN_POINT('Ctrl Pts',(-16.9342093846982,18.0960938143696,
0.95768743621197));
#193659=CARTESIAN_POINT('Ctrl Pts',(-17.0303114782358,17.9448047871347,
0.968729742983238));
#193660=CARTESIAN_POINT('Ctrl Pts',(-17.127733439411,17.8233054871346,0.978845965486544));
#193661=CARTESIAN_POINT('Ctrl Pts',(-17.290118875248,17.661025224386,0.994012844950908));
#193662=CARTESIAN_POINT('Ctrl Pts',(-17.3454300549669,17.6112848483738,
0.998936010626699));
#193663=CARTESIAN_POINT('Ctrl Pts',(-17.4390016825733,17.5356545883667,
1.00677218781032));
#193664=CARTESIAN_POINT('Ctrl Pts',(-17.4756936447651,17.5079237972352,
1.0097329997917));
#193665=CARTESIAN_POINT('Ctrl Pts',(-17.5269182487629,17.4717696967445,
1.01368766850648));
#193666=CARTESIAN_POINT('Ctrl Pts',(-17.5406888215884,17.4622928003012,
1.01473383612806));
#193667=CARTESIAN_POINT('Ctrl Pts',(-17.5644672947668,17.4463401805657,
1.01650955099053));
#193668=CARTESIAN_POINT('Ctrl Pts',(-17.5744201013412,17.4397841744795,
1.01724374437526));
#193669=CARTESIAN_POINT('Ctrl Pts',(-17.5886442672696,17.4305858750477,
1.01827962017682));
#193670=CARTESIAN_POINT('Ctrl Pts',(-17.5928702713742,17.4278743301528,
1.01858571432806));
#193671=CARTESIAN_POINT('Ctrl Pts',(-17.6001689201298,17.4232278482474,
1.01911144572552));
#193672=CARTESIAN_POINT('Ctrl Pts',(-17.6032369543778,17.4212857435601,
1.01933155604431));
#193673=CARTESIAN_POINT('Ctrl Pts',(-17.6091968425474,17.4175345020901,
1.01975740601362));
#193674=CARTESIAN_POINT('Ctrl Pts',(-17.612088068981,17.4157244627561,1.01996320863873));
#193675=CARTESIAN_POINT('Ctrl Pts',(-17.6198977229054,17.4108614978265,
1.02051703990849));
#193676=CARTESIAN_POINT('Ctrl Pts',(-17.6248243603994,17.4078217189798,
1.02086420742884));
#193677=CARTESIAN_POINT('Ctrl Pts',(-17.643140021943,17.3966242621233,1.02214692548973));
#193678=CARTESIAN_POINT('Ctrl Pts',(-17.6566074506474,17.3885949580349,
1.02307443826268));
#193679=CARTESIAN_POINT('Ctrl Pts',(-17.7862402628644,17.3132470190554,
1.03186578656901));
#193680=CARTESIAN_POINT('Ctrl Pts',(-17.9084891445359,17.2569640131818,
1.03912833110805));
#193681=CARTESIAN_POINT('Ctrl Pts',(-18.1869536715711,17.1595972085844,
1.05514807789573));
#193682=CARTESIAN_POINT('Ctrl Pts',(-18.3441708786778,17.1240073815863,
1.06389542625938));
#193683=CARTESIAN_POINT('Ctrl Pts',(-18.5224424529483,17.1045146268698,
1.07436838051043));
#193684=CARTESIAN_POINT('Ctrl Pts',(-18.5410181714938,17.1027317049779,
1.07546550415108));
#193685=CARTESIAN_POINT('Ctrl Pts',(-18.5681149000296,17.1004920321706,
1.07707532954445));
#193686=CARTESIAN_POINT('Ctrl Pts',(-18.5766192676691,17.099840827766,1.07758192585691));
#193687=CARTESIAN_POINT('Ctrl Pts',(-18.5915587880994,17.0987876357999,
1.07847431431548));
#193688=CARTESIAN_POINT('Ctrl Pts',(-18.597992313621,17.0983636190404,1.07885940979307));
#193689=CARTESIAN_POINT('Ctrl Pts',(-18.6105048785615,17.0975963407544,
1.07960997350512));
#193690=CARTESIAN_POINT('Ctrl Pts',(-18.6165836651595,17.0972499024151,
1.07997533803777));
#193691=CARTESIAN_POINT('Ctrl Pts',(-18.6311454515579,17.0964830150636,
1.08085235508423));
#193692=CARTESIAN_POINT('Ctrl Pts',(-18.6396296031234,17.0960873865274,
1.08136478132736));
#193693=CARTESIAN_POINT('Ctrl Pts',(-18.6704139673352,17.0948374722322,
1.08322948010482));
#193694=CARTESIAN_POINT('Ctrl Pts',(-18.6927243427418,17.0942847882159,
1.08459114742374));
#193695=CARTESIAN_POINT('Ctrl Pts',(-18.8983629639602,17.0924428680754,
1.09724057980109));
#193696=CARTESIAN_POINT('Ctrl Pts',(-19.0810914412825,17.1146220681367,
1.10930521320479));
#193697=CARTESIAN_POINT('Ctrl Pts',(-19.3376248031391,17.1802430190148,
1.12678928365928));
#193698=CARTESIAN_POINT('Ctrl Pts',(-19.4153877710262,17.2049966894788,
1.13214940984021));
#193699=CARTESIAN_POINT('Ctrl Pts',(-19.5255261418308,17.247202513244,1.13967034698697));
#193700=CARTESIAN_POINT('Ctrl Pts',(-19.5591798243294,17.2611044058583,
1.14195798478512));
#193701=CARTESIAN_POINT('Ctrl Pts',(-19.5993087210326,17.2789063308987,
1.14465893236394));
#193702=CARTESIAN_POINT('Ctrl Pts',(-19.6061409649305,17.2819807491836,
1.14511783251375));
#193703=CARTESIAN_POINT('Ctrl Pts',(-19.6167472553775,17.2868213069696,
1.14582856644189));
#193704=CARTESIAN_POINT('Ctrl Pts',(-19.6205325734649,17.288562392049,1.14608189278049));
#193705=CARTESIAN_POINT('Ctrl Pts',(-19.6275487043413,17.2918146430756,
1.14655078837561));
#193706=CARTESIAN_POINT('Ctrl Pts',(-19.6307808095771,17.2933227849476,
1.14676653356323));
#193707=CARTESIAN_POINT('Ctrl Pts',(-19.6380869564188,17.2967544378917,
1.14725364736596));
#193708=CARTESIAN_POINT('Ctrl Pts',(-19.6421586674959,17.2986827845956,
1.14752471290317));
#193709=CARTESIAN_POINT('Ctrl Pts',(-19.6544483244028,17.3045512228829,
1.14834174357124));
#193710=CARTESIAN_POINT('Ctrl Pts',(-19.6626471361992,17.3085314560192,
1.14888528194622));
#193711=CARTESIAN_POINT('Ctrl Pts',(-19.7255937638177,17.3395937029289,
1.15304844641102));
#193712=CARTESIAN_POINT('Ctrl Pts',(-19.7791775080496,17.3689833971257,
1.15653489960124));
#193713=CARTESIAN_POINT('Ctrl Pts',(-19.9708586361236,17.4851791353637,
1.16906415693261));
#193714=CARTESIAN_POINT('Ctrl Pts',(-20.100068947161,17.5855344379555,1.1776651801176));
#193715=CARTESIAN_POINT('Ctrl Pts',(-20.2731079113415,17.7552777135112,
1.19111372097631));
#193716=CARTESIAN_POINT('Ctrl Pts',(-20.3265598745273,17.8139561135951,
1.1956010316147));
#193717=CARTESIAN_POINT('Ctrl Pts',(-20.3888156884265,17.8905267612264,
1.20135967524924));
#193718=CARTESIAN_POINT('Ctrl Pts',(-20.4008334404232,17.9057296134612,
1.20249840406351));
#193719=CARTESIAN_POINT('Ctrl Pts',(-20.4179162397091,17.9279606130509,
1.20415796085933));
#193720=CARTESIAN_POINT('Ctrl Pts',(-20.4231497435415,17.9348585065455,
1.20467212634369));
#193721=CARTESIAN_POINT('Ctrl Pts',(-20.4322172775493,17.9469632573573,
1.20557316958583));
#193722=CARTESIAN_POINT('Ctrl Pts',(-20.4360700664591,17.9521559683779,
1.20595930643275));
#193723=CARTESIAN_POINT('Ctrl Pts',(-20.4434807364971,17.9622401368593,
1.2067084576106));
#193724=CARTESIAN_POINT('Ctrl Pts',(-20.4470415660781,17.9671293572265,
1.20707135210618));
#193725=CARTESIAN_POINT('Ctrl Pts',(-20.4554657382686,17.9788010042822,
1.207936925831));
#193726=CARTESIAN_POINT('Ctrl Pts',(-20.4603099945613,17.9855970243881,
1.20844033487524));
#193727=CARTESIAN_POINT('Ctrl Pts',(-20.4774345686988,18.009924210953,1.21024038985446));
#193728=CARTESIAN_POINT('Ctrl Pts',(-20.4894887237817,18.0276123060267,
1.21154561110807));
#193729=CARTESIAN_POINT('Ctrl Pts',(-20.6070117123993,18.2058117832186,
1.22466387062213));
#193730=CARTESIAN_POINT('Ctrl Pts',(-20.6904215902378,18.3797598360829,
1.23734178450062));
#193731=CARTESIAN_POINT('Ctrl Pts',(-20.7725200131164,18.6348873195065,
1.25502398947527));
#193732=CARTESIAN_POINT('Ctrl Pts',(-20.7918958078666,18.7084703105442,
1.26000962831794));
#193733=CARTESIAN_POINT('Ctrl Pts',(-20.8143280450851,18.8171190742397,
1.26707459920589));
#193734=CARTESIAN_POINT('Ctrl Pts',(-20.820538957625,18.8514691043632,1.2692655558093));
#193735=CARTESIAN_POINT('Ctrl Pts',(-20.8270336481075,18.8932676428165,
1.27186758279374));
#193736=CARTESIAN_POINT('Ctrl Pts',(-20.8281309513188,18.9005821117358,
1.2723205554791));
#193737=CARTESIAN_POINT('Ctrl Pts',(-20.8297832003394,18.9120034307894,
1.2730240118857));
#193738=CARTESIAN_POINT('Ctrl Pts',(-20.8303644473172,18.9161063311484,
1.27327594252214));
#193739=CARTESIAN_POINT('Ctrl Pts',(-20.8314236226128,18.9237442402589,
1.27374346151841));
#193740=CARTESIAN_POINT('Ctrl Pts',(-20.8319046586926,18.9272787151129,
1.27395921812063));
#193741=CARTESIAN_POINT('Ctrl Pts',(-20.8329764096804,18.9353053158722,
1.27444786561784));
#193742=CARTESIAN_POINT('Ctrl Pts',(-20.8335616374145,18.9397981216413,
1.27472044424227));
#193743=CARTESIAN_POINT('Ctrl Pts',(-20.8352591883987,18.953165147939,1.27552872938973));
#193744=CARTESIAN_POINT('Ctrl Pts',(-20.8363297207846,18.9620447043229,
1.27606213717881));
#193745=CARTESIAN_POINT('Ctrl Pts',(-20.8440773401224,19.0299247942671,
1.28011469178529));
#193746=CARTESIAN_POINT('Ctrl Pts',(-20.8483264336687,19.0891816749318,
1.28350793907857));
#193747=CARTESIAN_POINT('Ctrl Pts',(-20.8506770365375,19.1688228885189,
1.28796720666029));
#193748=CARTESIAN_POINT('Ctrl Pts',(-20.8509840406832,19.1891096026186,
1.28909428040348));
#193749=CARTESIAN_POINT('Ctrl Pts',(-20.8511051845503,19.3491947094905,
1.29793919539568));
#193750=CARTESIAN_POINT('Ctrl Pts',(-20.8373639130496,19.4886586124641,
1.3053742556948));
#193751=CARTESIAN_POINT('Ctrl Pts',(-20.7922498000778,19.714469502803,1.31812049820498));
#193752=CARTESIAN_POINT('Ctrl Pts',(-20.7688588159742,19.8019488125389,
1.32323618964279));
#193753=CARTESIAN_POINT('Ctrl Pts',(-20.735559598103,19.9006641156182,1.32934395282682));
#193754=CARTESIAN_POINT('Ctrl Pts',(-20.7310458706774,19.913627350948,1.33015272451101));
#193755=CARTESIAN_POINT('Ctrl Pts',(-20.7251405246782,19.9300705383681,
1.33118747866683));
#193756=CARTESIAN_POINT('Ctrl Pts',(-20.7238652303846,19.9335921343837,
1.33140960977109));
#193757=CARTESIAN_POINT('Ctrl Pts',(-20.7225806064482,19.93711030268,1.33163204998037));
#193758=CARTESIAN_POINT('Origin',(-18.734,19.211,0.));
#193759=CARTESIAN_POINT('',(-20.7225806064941,19.9371103025544,2.35747633162257));
#193760=CARTESIAN_POINT('',(-20.7227695185423,19.9371792543491,2.1335156684528));
#193761=CARTESIAN_POINT('',(-20.7225806064498,19.9371103026755,0.));
#193762=CARTESIAN_POINT('Ctrl Pts',(-20.7225806064941,19.9371103025544,
2.35747633162257));
#193763=CARTESIAN_POINT('Ctrl Pts',(-20.7258083370006,19.9282705956041,
2.35692307432503));
#193764=CARTESIAN_POINT('Ctrl Pts',(-20.7289770874423,19.9194094713397,
2.35636790109843));
#193765=CARTESIAN_POINT('Ctrl Pts',(-20.7349196690319,19.9024354529302,
2.35530318962104));
#193766=CARTESIAN_POINT('Ctrl Pts',(-20.7377034729521,19.8943263471203,
2.35479399943749));
#193767=CARTESIAN_POINT('Ctrl Pts',(-20.7424958166832,19.8800853356252,
2.35389873934373));
#193768=CARTESIAN_POINT('Ctrl Pts',(-20.744525736348,19.8739607032413,2.35351338181118));
#193769=CARTESIAN_POINT('Ctrl Pts',(-20.7484115459079,19.8620545243679,
2.35276356970637));
#193770=CARTESIAN_POINT('Ctrl Pts',(-20.7502706246368,19.8562740789923,
2.35239922471625));
#193771=CARTESIAN_POINT('Ctrl Pts',(-20.7546531726338,19.8424435269296,
2.35152669771869));
#193772=CARTESIAN_POINT('Ctrl Pts',(-20.7571534259374,19.8343862235171,
2.35101775858528));
#193773=CARTESIAN_POINT('Ctrl Pts',(-20.7659891992941,19.8052989895712,
2.34917807743202));
#193774=CARTESIAN_POINT('Ctrl Pts',(-20.7720453452344,19.7841862775621,
2.34783825951628));
#193775=CARTESIAN_POINT('Ctrl Pts',(-20.8265422866132,19.5824062340106,
2.33498643421796));
#193776=CARTESIAN_POINT('Ctrl Pts',(-20.851156347104,19.3961933090496,2.32266067027536));
#193777=CARTESIAN_POINT('Ctrl Pts',(-20.8509463100805,19.1462094374975,
2.30615866168918));
#193778=CARTESIAN_POINT('Ctrl Pts',(-20.8480800911786,19.0832283197751,
2.30201616600222));
#193779=CARTESIAN_POINT('Ctrl Pts',(-20.837918860491,18.9707861185551,2.29473641728172));
#193780=CARTESIAN_POINT('Ctrl Pts',(-20.8316744047912,18.9212755815429,
2.29157206213904));
#193781=CARTESIAN_POINT('Ctrl Pts',(-20.8224344768722,18.8643135220372,
2.28801331259313));
#193782=CARTESIAN_POINT('Ctrl Pts',(-20.8211403746173,18.8566059549827,
2.28753352859736));
#193783=CARTESIAN_POINT('Ctrl Pts',(-20.8190058160593,18.844310073383,2.28677112202291));
#193784=CARTESIAN_POINT('Ctrl Pts',(-20.818192841526,18.8397171488273,2.28648700577087));
#193785=CARTESIAN_POINT('Ctrl Pts',(-20.8167271896738,18.8315934302223,
2.28598570510313));
#193786=CARTESIAN_POINT('Ctrl Pts',(-20.8160807012362,18.8280615635935,
2.28576817293963));
#193787=CARTESIAN_POINT('Ctrl Pts',(-20.8146926431108,18.8205858247794,
2.28530862225324));
#193788=CARTESIAN_POINT('Ctrl Pts',(-20.8139488460956,18.8166424191797,
2.28506673215675));
#193789=CARTESIAN_POINT('Ctrl Pts',(-20.8119140363715,18.8060203361484,
2.28441651366059));
#193790=CARTESIAN_POINT('Ctrl Pts',(-20.810602027063,18.7993456610807,2.28400936519241));
#193791=CARTESIAN_POINT('Ctrl Pts',(-20.803970729535,18.7664484432482,2.28200923301305));
#193792=CARTESIAN_POINT('Ctrl Pts',(-20.7981865505351,18.7403207641232,
2.28044128843594));
#193793=CARTESIAN_POINT('Ctrl Pts',(-20.7800922310083,18.6653518059024,
2.27598366438792));
#193794=CARTESIAN_POINT('Ctrl Pts',(-20.7665321461988,18.6168290476827,
2.27314937726003));
#193795=CARTESIAN_POINT('Ctrl Pts',(-20.7111897277366,18.4429806428975,
2.26303185761288));
#193796=CARTESIAN_POINT('Ctrl Pts',(-20.6594360217855,18.3211508442493,
2.25599591422191));
#193797=CARTESIAN_POINT('Ctrl Pts',(-20.547245161614,18.1134367048173,2.24300921728127));
#193798=CARTESIAN_POINT('Ctrl Pts',(-20.4911568897142,18.0257157213685,
2.23716710359459));
#193799=CARTESIAN_POINT('Ctrl Pts',(-20.4204318607925,17.931221022007,2.23025035766843));
#193800=CARTESIAN_POINT('Ctrl Pts',(-20.4118958788883,17.9200499393819,
2.22942226593358));
#193801=CARTESIAN_POINT('Ctrl Pts',(-20.398090742884,17.9023513264738,2.22809315366176));
#193802=CARTESIAN_POINT('Ctrl Pts',(-20.3928928708287,17.8957685407889,
2.22759495475064));
#193803=CARTESIAN_POINT('Ctrl Pts',(-20.3836314072036,17.8841817112644,
2.22671111081189));
#193804=CARTESIAN_POINT('Ctrl Pts',(-20.3795837997856,17.8791649849098,
2.22632610981205));
#193805=CARTESIAN_POINT('Ctrl Pts',(-20.3711396549156,17.86879631854,2.22552550100565));
#193806=CARTESIAN_POINT('Ctrl Pts',(-20.3667396432207,17.8634473190618,
2.2251097551417));
#193807=CARTESIAN_POINT('Ctrl Pts',(-20.3553245529637,17.849708224409,2.22403477989301));
#193808=CARTESIAN_POINT('Ctrl Pts',(-20.3482706313711,17.8413508018482,
2.22337396825025));
#193809=CARTESIAN_POINT('Ctrl Pts',(-20.3180882580626,17.8061480577944,
2.22056073146907));
#193810=CARTESIAN_POINT('Ctrl Pts',(-20.2943535738347,17.7798322686497,
2.21838329754759));
#193811=CARTESIAN_POINT('Ctrl Pts',(-20.2303134845433,17.7123153230627,
2.2125935812829));
#193812=CARTESIAN_POINT('Ctrl Pts',(-20.188968672702,17.672144894414,2.20893873669524));
#193813=CARTESIAN_POINT('Ctrl Pts',(-20.0462318762339,17.5443621398683,
2.19660000518597));
#193814=CARTESIAN_POINT('Ctrl Pts',(-19.9381729687711,17.4646905791544,
2.18767359816132));
#193815=CARTESIAN_POINT('Ctrl Pts',(-19.746372921014,17.3495908055372,2.17297280290509));
#193816=CARTESIAN_POINT('Ctrl Pts',(-19.6665527342797,17.3083459893408,
2.16715227537536));
#193817=CARTESIAN_POINT('Ctrl Pts',(-19.5755079983687,17.2684124357765,
2.16101027401375));
#193818=CARTESIAN_POINT('Ctrl Pts',(-19.5666425089598,17.2645959781263,
2.16041727244592));
#193819=CARTESIAN_POINT('Ctrl Pts',(-19.5535033404576,17.2590459694984,
2.159546224005));
#193820=CARTESIAN_POINT('Ctrl Pts',(-19.54924974574,17.2572655975766,2.15926543943138));
#193821=CARTESIAN_POINT('Ctrl Pts',(-19.5416882442493,17.2541296723596,
2.15876847387096));
#193822=CARTESIAN_POINT('Ctrl Pts',(-19.5383826912116,17.2527685872574,
2.15855196085396));
#193823=CARTESIAN_POINT('Ctrl Pts',(-19.5312874481935,17.2498680677301,
2.1580888148879));
#193824=CARTESIAN_POINT('Ctrl Pts',(-19.5274967503697,17.2483312458238,
2.15784234010848));
#193825=CARTESIAN_POINT('Ctrl Pts',(-19.5170660112718,17.244137582312,2.15716671059019));
#193826=CARTESIAN_POINT('Ctrl Pts',(-19.5104168530839,17.2415033582937,
2.15673889927245));
#193827=CARTESIAN_POINT('Ctrl Pts',(-19.474642028307,17.227539630704,2.15445187227512));
#193828=CARTESIAN_POINT('Ctrl Pts',(-19.4452798811727,17.216821769449,2.15262712912745));
#193829=CARTESIAN_POINT('Ctrl Pts',(-19.2606290852214,17.1540177449465,
2.14141264561027));
#193830=CARTESIAN_POINT('Ctrl Pts',(-19.0999557970955,17.1194448667353,
2.1327577596003));
#193831=CARTESIAN_POINT('Ctrl Pts',(-18.8202504340664,17.0925146077549,
2.11737625119989));
#193832=CARTESIAN_POINT('Ctrl Pts',(-18.7028972266081,17.0909889580431,
2.11083589061962));
#193833=CARTESIAN_POINT('Ctrl Pts',(-18.5717696855549,17.1001767824266,
2.10313521104301));
#193834=CARTESIAN_POINT('Ctrl Pts',(-18.5575209690726,17.1013202926768,
2.10229343993255));
#193835=CARTESIAN_POINT('Ctrl Pts',(-18.5348635434246,17.1033697724834,
2.10094651766514));
#193836=CARTESIAN_POINT('Ctrl Pts',(-18.5264466412293,17.1041819954307,
2.10044431007719));
#193837=CARTESIAN_POINT('Ctrl Pts',(-18.511611565799,17.1057033278525,2.09955580802749));
#193838=CARTESIAN_POINT('Ctrl Pts',(-18.5051913115994,17.106391419739,2.09917018002476));
#193839=CARTESIAN_POINT('Ctrl Pts',(-18.4919194249586,17.1078752836032,
2.09837068351477));
#193840=CARTESIAN_POINT('Ctrl Pts',(-18.4850683404699,17.1086751904943,
2.0979566888701));
#193841=CARTESIAN_POINT('Ctrl Pts',(-18.4674939994984,17.1108142147692,
2.09689135437236));
#193842=CARTESIAN_POINT('Ctrl Pts',(-18.4567769632541,17.1122019721029,
2.09623848599041));
#193843=CARTESIAN_POINT('Ctrl Pts',(-18.4121029017266,17.1183349890723,
2.09350327361417));
#193844=CARTESIAN_POINT('Ctrl Pts',(-18.3782546107007,17.123822577768,2.09139761636602));
#193845=CARTESIAN_POINT('Ctrl Pts',(-18.2904310993027,17.1402591315567,
2.08584401235039));
#193846=CARTESIAN_POINT('Ctrl Pts',(-18.2367260837093,17.1524959444146,
2.08235769518531));
#193847=CARTESIAN_POINT('Ctrl Pts',(-18.0779619843425,17.1952462599452,
2.07178963441209));
#193848=CARTESIAN_POINT('Ctrl Pts',(-17.9747307892796,17.2318194075763,
2.06455949505509));
#193849=CARTESIAN_POINT('Ctrl Pts',(-17.8336072438721,17.2944893896417,
2.0543593205525));
#193850=CARTESIAN_POINT('Ctrl Pts',(-17.7930125337472,17.3140912502936,
2.05138771895395));
#193851=CARTESIAN_POINT('Ctrl Pts',(-17.7315241471326,17.3462419712409,
2.04685423655292));
#193852=CARTESIAN_POINT('Ctrl Pts',(-17.7101698028667,17.3578804322822,
2.04527363202804));
#193853=CARTESIAN_POINT('Ctrl Pts',(-17.6764698715496,17.3770078301368,
2.04277421216629));
#193854=CARTESIAN_POINT('Ctrl Pts',(-17.6639924591252,17.3842594241168,
2.04184768595572));
#193855=CARTESIAN_POINT('Ctrl Pts',(-17.619633958912,17.4106500449378,2.03855222127833));
#193856=CARTESIAN_POINT('Ctrl Pts',(-17.5881821264162,17.4305019170751,
2.03621261754915));
#193857=CARTESIAN_POINT('Ctrl Pts',(-17.5513103956448,17.4551567114566,
2.03348106413737));
#193858=CARTESIAN_POINT('Ctrl Pts',(-17.545373434595,17.4591703149171,2.03304159686524));
#193859=CARTESIAN_POINT('Ctrl Pts',(-17.5357254037224,17.465764365517,2.03232816526987));
#193860=CARTESIAN_POINT('Ctrl Pts',(-17.5320020716161,17.4683266487978,
2.03205302092957));
#193861=CARTESIAN_POINT('Ctrl Pts',(-17.5253553732641,17.4729321398766,
2.03156221327305));
#193862=CARTESIAN_POINT('Ctrl Pts',(-17.5224289481114,17.4749708219706,
2.03134624923917));
#193863=CARTESIAN_POINT('Ctrl Pts',(-17.5161064391476,17.4793991460541,
2.03087994899954));
#193864=CARTESIAN_POINT('Ctrl Pts',(-17.5127122405319,17.4817913797909,
2.03062979391265));
#193865=CARTESIAN_POINT('Ctrl Pts',(-17.5032605254076,17.4884946666344,
2.02993361865172));
#193866=CARTESIAN_POINT('Ctrl Pts',(-17.4972185795621,17.4928277153981,
2.02948908081139));
#193867=CARTESIAN_POINT('Ctrl Pts',(-17.4624473827256,17.5180427195761,
2.0269328177355));
#193868=CARTESIAN_POINT('Ctrl Pts',(-17.4342225954955,17.5396145131729,
2.02486588513897));
#193869=CARTESIAN_POINT('Ctrl Pts',(-17.3455905585501,17.6109585959089,
2.01835413227576));
#193870=CARTESIAN_POINT('Ctrl Pts',(-17.2873918049756,17.6633760446575,
2.01404431440661));
#193871=CARTESIAN_POINT('Ctrl Pts',(-17.0993857698685,17.8526010146753,
1.99949369086041));
#193872=CARTESIAN_POINT('Ctrl Pts',(-16.9850088288275,18.0034257238715,
1.98942786273719));
#193873=CARTESIAN_POINT('Ctrl Pts',(-16.8813546360488,18.1863684794536,
1.97719494500122));
#193874=CARTESIAN_POINT('Ctrl Pts',(-16.8708981147763,18.2055071305123,
1.97591627478501));
#193875=CARTESIAN_POINT('Ctrl Pts',(-16.8568209136995,18.2322464906009,
1.97412983086024));
#193876=CARTESIAN_POINT('Ctrl Pts',(-16.8529468629093,18.2397127888505,
1.97363101752833));
#193877=CARTESIAN_POINT('Ctrl Pts',(-16.8463560133552,18.2526023942967,
1.97276980516306));
#193878=CARTESIAN_POINT('Ctrl Pts',(-16.8436178184557,18.2580146918992,
1.97240816274895));
#193879=CARTESIAN_POINT('Ctrl Pts',(-16.8380133321823,18.2692116833683,
1.97165991337662));
#193880=CARTESIAN_POINT('Ctrl Pts',(-16.8351501694008,18.2749978646993,
1.97127320176178));
#193881=CARTESIAN_POINT('Ctrl Pts',(-16.8285363522481,18.2885190063735,
1.97036938717927));
#193882=CARTESIAN_POINT('Ctrl Pts',(-16.824806275711,18.2962638543073,1.96985157431136));
#193883=CARTESIAN_POINT('Ctrl Pts',(-16.8129678213732,18.321232187129,1.9681817330836));
#193884=CARTESIAN_POINT('Ctrl Pts',(-16.8050447309268,18.3385420211256,
1.96702333482139));
#193885=CARTESIAN_POINT('Ctrl Pts',(-16.7663604989393,18.4261603951531,
1.96115449531175));
#193886=CARTESIAN_POINT('Ctrl Pts',(-16.7392083718904,18.4979905446274,
1.95632311388193));
#193887=CARTESIAN_POINT('Ctrl Pts',(-16.6826152379122,18.6764703364228,
1.94428019424811));
#193888=CARTESIAN_POINT('Ctrl Pts',(-16.6575151682528,18.7842580782506,
1.93696891770298));
#193889=CARTESIAN_POINT('Ctrl Pts',(-16.6298780378241,18.9664517725166,
1.92479845314424));
#193890=CARTESIAN_POINT('Ctrl Pts',(-16.6226329904922,19.03993392899,1.91994307867057));
#193891=CARTESIAN_POINT('Ctrl Pts',(-16.6172136150019,19.1576578260206,
1.91237655293546));
#193892=CARTESIAN_POINT('Ctrl Pts',(-16.6165617923873,19.2017240223307,
1.90959198699267));
#193893=CARTESIAN_POINT('Ctrl Pts',(-16.6174096716781,19.2533234549422,
1.90641127088156));
#193894=CARTESIAN_POINT('Ctrl Pts',(-16.6175739039016,19.2608645809207,
1.90594842080259));
#193895=CARTESIAN_POINT('Ctrl Pts',(-16.6179027442007,19.2729872428002,
1.90520776627002));
#193896=CARTESIAN_POINT('Ctrl Pts',(-16.618041933233,19.2775693237704,1.90492859644079));
#193897=CARTESIAN_POINT('Ctrl Pts',(-16.6183163360682,19.2857291935196,
1.90443287796156));
#193898=CARTESIAN_POINT('Ctrl Pts',(-16.6184457434308,19.2893071287099,
1.90421600834757));
#193899=CARTESIAN_POINT('Ctrl Pts',(-16.6187412494184,19.2969412444764,
1.90375434411372));
#193900=CARTESIAN_POINT('Ctrl Pts',(-16.6189099377581,19.3009972702751,
1.90350969598839));
#193901=CARTESIAN_POINT('Ctrl Pts',(-16.6194018272902,19.3120580964329,
1.90284421015918));
#193902=CARTESIAN_POINT('Ctrl Pts',(-16.6197481696241,19.319061888617,1.90242464952712));
#193903=CARTESIAN_POINT('Ctrl Pts',(-16.621725355079,19.3553852954967,1.90025760287986));
#193904=CARTESIAN_POINT('Ctrl Pts',(-16.6239313900089,19.3846719507194,
1.8985404494388));
#193905=CARTESIAN_POINT('Ctrl Pts',(-16.6322961696378,19.471543772585,1.89351153264984));
#193906=CARTESIAN_POINT('Ctrl Pts',(-16.6402090956601,19.5289349739786,
1.89027357571878));
#193907=CARTESIAN_POINT('Ctrl Pts',(-16.6798591510338,19.7492735420975,
1.87793081563257));
#193908=CARTESIAN_POINT('Ctrl Pts',(-16.7283560757306,19.9085865619674,
1.86914773812102));
#193909=CARTESIAN_POINT('Ctrl Pts',(-16.8200857739345,20.1179398975091,
1.85628654995288));
#193910=CARTESIAN_POINT('Ctrl Pts',(-16.8477370071711,20.1741295246211,
1.85269839702926));
#193911=CARTESIAN_POINT('Ctrl Pts',(-16.8838245483546,20.239929024275,1.8482909681105));
#193912=CARTESIAN_POINT('Ctrl Pts',(-16.8899102150147,20.2507966117704,
1.84755612672559));
#193913=CARTESIAN_POINT('Ctrl Pts',(-16.9000594582229,20.2685514280333,
1.84634390960961));
#193914=CARTESIAN_POINT('Ctrl Pts',(-16.9040668384881,20.2754705516952,
1.84586855853382));
#193915=CARTESIAN_POINT('Ctrl Pts',(-16.9113411678317,20.2878678951228,
1.84501146244165));
#193916=CARTESIAN_POINT('Ctrl Pts',(-16.9145938740788,20.2933543918753,
1.84463023834275));
#193917=CARTESIAN_POINT('Ctrl Pts',(-16.9215732617618,20.3050064994763,
1.84381647882346));
#193918=CARTESIAN_POINT('Ctrl Pts',(-16.9253067145432,20.3111679415082,
1.84338369887726));
#193919=CARTESIAN_POINT('Ctrl Pts',(-16.9354432966271,20.3277056238536,
1.84221533561125));
#193920=CARTESIAN_POINT('Ctrl Pts',(-16.9419046666353,20.3380456831811,
1.84147761428908));
#193921=CARTESIAN_POINT('Ctrl Pts',(-16.9746227203249,20.3894112522024,
1.83777619086537));
#193922=CARTESIAN_POINT('Ctrl Pts',(-17.0021987043686,20.4295750494239,
1.83476357395853));
#193923=CARTESIAN_POINT('Ctrl Pts',(-17.0856179040998,20.5425162462129,
1.82593647662104));
#193924=CARTESIAN_POINT('Ctrl Pts',(-17.1448321631763,20.6126566642694,
1.82000152537663));
#193925=CARTESIAN_POINT('Ctrl Pts',(-17.2753410281926,20.7483110795851,
1.80763880285383));
#193926=CARTESIAN_POINT('Ctrl Pts',(-17.3469621728779,20.8132288390426,
1.80121568213012));
#193927=CARTESIAN_POINT('Ctrl Pts',(-17.4836221018539,20.9210447851366,
1.78982360829918));
#193928=CARTESIAN_POINT('Ctrl Pts',(-17.5470790787152,20.9656850037643,
1.78482798822033));
#193929=CARTESIAN_POINT('Ctrl Pts',(-17.620917434964,21.0117850201804,1.77945151558655));
#193930=CARTESIAN_POINT('Ctrl Pts',(-17.6290203626898,21.0167683944472,
1.77886718027165));
#193931=CARTESIAN_POINT('Ctrl Pts',(-17.6410774151889,21.0240720436402,
1.77800638864554));
#193932=CARTESIAN_POINT('Ctrl Pts',(-17.6450057994789,21.0264342852233,
1.77772728505667));
#193933=CARTESIAN_POINT('Ctrl Pts',(-17.6520090689725,21.0306146253844,
1.77723216947439));
#193934=CARTESIAN_POINT('Ctrl Pts',(-17.6550809077026,21.0324377158368,
1.77701583476367));
#193935=CARTESIAN_POINT('Ctrl Pts',(-17.6616953844734,21.036340704356,1.77655181559128));
#193936=CARTESIAN_POINT('Ctrl Pts',(-17.6652394558983,21.0384180625925,
1.77630429589092));
#193937=CARTESIAN_POINT('Ctrl Pts',(-17.6750393388708,21.0441240053895,
1.77562284658762));
#193938=CARTESIAN_POINT('Ctrl Pts',(-17.6813077994382,21.0477309098678,
1.77519029914606));
#193939=CARTESIAN_POINT('Ctrl Pts',(-17.7157565007453,21.0673185812155,
1.77283076321627));
#193940=CARTESIAN_POINT('Ctrl Pts',(-17.744283887119,21.0826839405927,1.77094088613304));
#193941=CARTESIAN_POINT('Ctrl Pts',(-17.9182188363299,21.1712789194842,
1.7597315590692));
#193942=CARTESIAN_POINT('Ctrl Pts',(-18.07133709615,21.2281965990321,1.75112687495386));
#193943=CARTESIAN_POINT('Ctrl Pts',(-18.3429908796731,21.2948573269123,
1.73581422361014));
#193944=CARTESIAN_POINT('Ctrl Pts',(-18.4585978772053,21.3132601876843,
1.72928959262602));
#193945=CARTESIAN_POINT('Ctrl Pts',(-18.5893741822905,21.3231024106734,
1.72160661815243));
#193946=CARTESIAN_POINT('Ctrl Pts',(-18.6036346747824,21.3240305457778,
1.72076507144283));
#193947=CARTESIAN_POINT('Ctrl Pts',(-18.6263453904664,21.3252778838986,
1.71941844131572));
#193948=CARTESIAN_POINT('Ctrl Pts',(-18.634790171541,21.3256909684562,1.71891629945182));
#193949=CARTESIAN_POINT('Ctrl Pts',(-18.6496880282078,21.3263302773831,
1.71802787415162));
#193950=CARTESIAN_POINT('Ctrl Pts',(-18.6561401248943,21.3265775876635,
1.71764225680737));
#193951=CARTESIAN_POINT('Ctrl Pts',(-18.6694873680134,21.3270280489729,
1.71684274358255));
#193952=CARTESIAN_POINT('Ctrl Pts',(-18.6763825702282,21.3272270232091,
1.71642872137321));
#193953=CARTESIAN_POINT('Ctrl Pts',(-18.6940840311506,21.3276512562827,
1.71536323420402));
#193954=CARTESIAN_POINT('Ctrl Pts',(-18.7048911673507,21.3278274597541,
1.71471023986695));
#193955=CARTESIAN_POINT('Ctrl Pts',(-18.7500025742677,21.328217452008,1.71197380483497));
#193956=CARTESIAN_POINT('Ctrl Pts',(-18.7843065669613,21.3276801493136,
1.70986702479858));
#193957=CARTESIAN_POINT('Ctrl Pts',(-18.8736412130645,21.3241080950453,
1.70430975168817));
#193958=CARTESIAN_POINT('Ctrl Pts',(-18.9285905010767,21.3197577399365,
1.70082082497084));
#193959=CARTESIAN_POINT('Ctrl Pts',(-19.0871715552301,21.3009519218248,
1.69055625303314));
#193960=CARTESIAN_POINT('Ctrl Pts',(-19.1899762856936,21.2809545168195,
1.68365003757954));
#193961=CARTESIAN_POINT('Ctrl Pts',(-19.4098718339464,21.2209998733261,
1.66858985106));
#193962=CARTESIAN_POINT('Ctrl Pts',(-19.5258210272218,21.17821342418,1.66046083813723));
#193963=CARTESIAN_POINT('Ctrl Pts',(-19.6459306174739,21.1215393591917,
1.65225901090985));
#193964=CARTESIAN_POINT('Ctrl Pts',(-19.6544401566968,21.117454305677,1.65167924091008));
#193965=CARTESIAN_POINT('Ctrl Pts',(-19.6670283199641,21.1113073525025,
1.65082385770607));
#193966=CARTESIAN_POINT('Ctrl Pts',(-19.6711279142617,21.1092890067232,
1.65054564431789));
#193967=CARTESIAN_POINT('Ctrl Pts',(-19.6784194143644,21.1056698182203,
1.65005150168731));
#193968=CARTESIAN_POINT('Ctrl Pts',(-19.6816138289532,21.104074161814,1.64983525468109));
#193969=CARTESIAN_POINT('Ctrl Pts',(-19.6884093605998,21.1006581842282,
1.64937574297494));
#193970=CARTESIAN_POINT('Ctrl Pts',(-19.692009302844,21.0988356541581,1.64913261959681));
#193971=CARTESIAN_POINT('Ctrl Pts',(-19.7018354092485,21.0938256809191,
1.64846978133991));
#193972=CARTESIAN_POINT('Ctrl Pts',(-19.7080510864723,21.0906176228627,
1.64805134043633));
#193973=CARTESIAN_POINT('Ctrl Pts',(-19.7219080525441,21.083378517952,1.6471201345054));
#193974=CARTESIAN_POINT('Ctrl Pts',(-19.7295408395043,21.0793313617043,
1.64660832929403));
#193975=CARTESIAN_POINT('Ctrl Pts',(-19.752995588107,21.0667103291821,1.64503843378264));
#193976=CARTESIAN_POINT('Ctrl Pts',(-19.7687335679533,21.0579811373214,
1.64398903592947));
#193977=CARTESIAN_POINT('Ctrl Pts',(-19.828886429719,21.0236066531205,1.6399861360298));
#193978=CARTESIAN_POINT('Ctrl Pts',(-19.8724777658955,20.9965498472194,
1.63710225204504));
#193979=CARTESIAN_POINT('Ctrl Pts',(-20.0283803324946,20.8917490819468,
1.62669288391142));
#193980=CARTESIAN_POINT('Ctrl Pts',(-20.1340789811193,20.804775142282,1.61942670334326));
#193981=CARTESIAN_POINT('Ctrl Pts',(-20.3002696004928,20.6386463557276,
1.60646865982797));
#193982=CARTESIAN_POINT('Ctrl Pts',(-20.3649281372122,20.5643087019784,
1.60092488104402));
#193983=CARTESIAN_POINT('Ctrl Pts',(-20.43257196273,20.4746204378556,1.5943407417292));
#193984=CARTESIAN_POINT('Ctrl Pts',(-20.4408556345718,20.4634085405383,
1.59351955992391));
#193985=CARTESIAN_POINT('Ctrl Pts',(-20.4539248015979,20.4453489974257,
1.5921994494648));
#193986=CARTESIAN_POINT('Ctrl Pts',(-20.4587816277087,20.4385532999689,
1.59170328170978));
#193987=CARTESIAN_POINT('Ctrl Pts',(-20.4673119154711,20.4264671057377,
1.59082178566523));
#193988=CARTESIAN_POINT('Ctrl Pts',(-20.4710017095797,20.4211882254205,
1.59043709005023));
#193989=CARTESIAN_POINT('Ctrl Pts',(-20.4786180162605,20.4101852067226,
1.58963586225675));
#193990=CARTESIAN_POINT('Ctrl Pts',(-20.482540574539,20.4044584366823,1.58921918581006));
#193991=CARTESIAN_POINT('Ctrl Pts',(-20.4926090908109,20.3896026374459,
1.58813910720564));
#193992=CARTESIAN_POINT('Ctrl Pts',(-20.4987120973301,20.3804448758496,
1.58747409412736));
#193993=CARTESIAN_POINT('Ctrl Pts',(-20.5245036292371,20.3410821749285,
1.584618735998));
#193994=CARTESIAN_POINT('Ctrl Pts',(-20.5434892339324,20.3104259546805,
1.58240244054529));
#193995=CARTESIAN_POINT('Ctrl Pts',(-20.5914724005276,20.2283349139736,
1.57648346236878));
#193996=CARTESIAN_POINT('Ctrl Pts',(-20.619115622545,20.1761487659913,1.57273581705888));
#193997=CARTESIAN_POINT('Ctrl Pts',(-20.6735090116571,20.0621854787197,
1.5645939701441));
#193998=CARTESIAN_POINT('Ctrl Pts',(-20.6995477912786,20.0001897629222,
1.56018956835498));
#193999=CARTESIAN_POINT('Ctrl Pts',(-20.7225807924205,19.937109793362,1.55576067791233));
#194000=CARTESIAN_POINT('',(-20.8479202339018,19.2101717420009,2.08900081873324));
#194001=CARTESIAN_POINT('Ctrl Pts',(-20.7225806064482,19.93711030268,1.33163204998037));
#194002=CARTESIAN_POINT('Ctrl Pts',(-20.7210219801323,19.9413788746215,
1.33190193531729));
#194003=CARTESIAN_POINT('Ctrl Pts',(-20.7194496198182,19.9456424006789,
1.33217227569476));
#194004=CARTESIAN_POINT('Ctrl Pts',(-20.7156191794292,19.9559266917663,
1.33282626855238));
#194005=CARTESIAN_POINT('Ctrl Pts',(-20.7133473849464,19.9619422592217,
1.33321037582342));
#194006=CARTESIAN_POINT('Ctrl Pts',(-20.7085566179748,19.9744551210761,
1.33401266450812));
#194007=CARTESIAN_POINT('Ctrl Pts',(-20.7060329042928,19.9809505062436,
1.33443100152553));
#194008=CARTESIAN_POINT('Ctrl Pts',(-20.6993949396819,19.9977881672302,
1.33552036370451));
#194009=CARTESIAN_POINT('Ctrl Pts',(-20.69523115058,20.0081105667363,1.33619305310805));
#194010=CARTESIAN_POINT('Ctrl Pts',(-20.6767885689131,20.0528119545002,
1.33912762571572));
#194011=CARTESIAN_POINT('Ctrl Pts',(-20.6616864783648,20.086842083609,1.34141728728153));
#194012=CARTESIAN_POINT('Ctrl Pts',(-20.619174301263,20.1762037026226,1.34758328748549));
#194013=CARTESIAN_POINT('Ctrl Pts',(-20.5902290357626,20.2307612337437,
1.35150939858986));
#194014=CARTESIAN_POINT('Ctrl Pts',(-20.4847193863011,20.4102152056578,
1.36495843768551));
#194015=CARTESIAN_POINT('Ctrl Pts',(-20.3975968400093,20.528412548849,1.37476366490735));
#194016=CARTESIAN_POINT('Ctrl Pts',(-20.2858390406964,20.6510922783274,
1.38559624225933));
#194017=CARTESIAN_POINT('Ctrl Pts',(-20.2724917414562,20.66534293502,1.3868651468458));
#194018=CARTESIAN_POINT('Ctrl Pts',(-20.2223171049878,20.7174495703338,
1.39153861523857));
#194019=CARTESIAN_POINT('Ctrl Pts',(-20.1842710771645,20.7541114429139,
1.39489478220167));
#194020=CARTESIAN_POINT('Ctrl Pts',(-20.1384093776391,20.7951082242178,
1.39868927155921));
#194021=CARTESIAN_POINT('Ctrl Pts',(-20.1318927159941,20.8008617947951,
1.39922279338419));
#194022=CARTESIAN_POINT('Ctrl Pts',(-20.1219663922015,20.8095175436712,
1.40002669898881));
#194023=CARTESIAN_POINT('Ctrl Pts',(-20.1185827513091,20.8124492339549,
1.40029920425877));
#194024=CARTESIAN_POINT('Ctrl Pts',(-20.1124893449964,20.8176949999569,
1.40078716852804));
#194025=CARTESIAN_POINT('Ctrl Pts',(-20.1097830276927,20.8200129764682,
1.40100291356046));
#194026=CARTESIAN_POINT('Ctrl Pts',(-20.1038860843768,20.8250379868895,
1.40147088500487));
#194027=CARTESIAN_POINT('Ctrl Pts',(-20.1006932920077,20.8277423893645,
1.4017229187453));
#194028=CARTESIAN_POINT('Ctrl Pts',(-20.0916937734164,20.8353195740922,
1.40242963365348));
#194029=CARTESIAN_POINT('Ctrl Pts',(-20.0858687956632,20.8401707167768,
1.40288275892046));
#194030=CARTESIAN_POINT('Ctrl Pts',(-20.0507099584497,20.8691331977841,
1.4055929180279));
#194031=CARTESIAN_POINT('Ctrl Pts',(-20.0207558051386,20.8924846766865,
1.40779861654323));
#194032=CARTESIAN_POINT('Ctrl Pts',(-19.919679264397,20.9669973916801,1.4149670293758));
#194033=CARTESIAN_POINT('Ctrl Pts',(-19.8460068841176,21.0145535140239,
1.4197614569395));
#194034=CARTESIAN_POINT('Ctrl Pts',(-19.6172786138434,21.1428401094856,
1.43402871201116));
#194035=CARTESIAN_POINT('Ctrl Pts',(-19.4549968073101,21.209085129227,1.44342161132237));
#194036=CARTESIAN_POINT('Ctrl Pts',(-19.2641710281374,21.2606680886938,
1.45490747645002));
#194037=CARTESIAN_POINT('Ctrl Pts',(-19.2418174444265,21.2663204067987,
1.45625818626721));
#194038=CARTESIAN_POINT('Ctrl Pts',(-19.2100739958543,21.2737975884584,
1.45818542731543));
#194039=CARTESIAN_POINT('Ctrl Pts',(-19.2007567509785,21.2759257786522,
1.45875220920406));
#194040=CARTESIAN_POINT('Ctrl Pts',(-19.1855974111556,21.2792805440006,
1.45967628392139));
#194041=CARTESIAN_POINT('Ctrl Pts',(-19.1797639105687,21.2805456422521,
1.46003233689495));
#194042=CARTESIAN_POINT('Ctrl Pts',(-19.167544176819,21.2831416461357,1.4607791698737));
#194043=CARTESIAN_POINT('Ctrl Pts',(-19.1611569949902,21.2844677366808,
1.46117009979784));
#194044=CARTESIAN_POINT('Ctrl Pts',(-19.1459516656235,21.2875513895421,
1.4621021350298));
#194045=CARTESIAN_POINT('Ctrl Pts',(-19.1371283024604,21.2892823234767,
1.46264408471871));
#194046=CARTESIAN_POINT('Ctrl Pts',(-19.1073848532958,21.2949207439661,
1.46447486056438));
#194047=CARTESIAN_POINT('Ctrl Pts',(-19.086417467998,21.298568871237,1.46577189765452));
#194048=CARTESIAN_POINT('Ctrl Pts',(-18.9080304550596,21.3268424920729,
1.47686494062663));
#194049=CARTESIAN_POINT('Ctrl Pts',(-18.7483780016142,21.3339345607675,
1.48723402128144));
#194050=CARTESIAN_POINT('Ctrl Pts',(-18.4581190095075,21.3140723894634,
1.50645220289788));
#194051=CARTESIAN_POINT('Ctrl Pts',(-18.3278779539579,21.2928488882342,
1.51519416249287));
#194052=CARTESIAN_POINT('Ctrl Pts',(-18.1852095922554,21.255692133338,1.52439164038815));
#194053=CARTESIAN_POINT('Ctrl Pts',(-18.1700193264239,21.2515544994403,
1.52536571578161));
#194054=CARTESIAN_POINT('Ctrl Pts',(-18.1492987512426,21.2456614148295,
1.52668594932913));
#194055=CARTESIAN_POINT('Ctrl Pts',(-18.1437278409085,21.2440522382159,
1.52704006298472));
#194056=CARTESIAN_POINT('Ctrl Pts',(-18.1348885921039,21.2414595954865,
1.5276005088182));
#194057=CARTESIAN_POINT('Ctrl Pts',(-18.1316159471186,21.2404910941394,
1.52780769856876));
#194058=CARTESIAN_POINT('Ctrl Pts',(-18.1248643571976,21.238475269468,1.52823447783236));
#194059=CARTESIAN_POINT('Ctrl Pts',(-18.1213857646962,21.2374269043043,
1.52845399909992));
#194060=CARTESIAN_POINT('Ctrl Pts',(-18.1131072948803,21.2349087053527,
1.52897558268967));
#194061=CARTESIAN_POINT('Ctrl Pts',(-18.1083098767027,21.2334307329704,
1.52927717034093));
#194062=CARTESIAN_POINT('Ctrl Pts',(-18.0921655107758,21.2283940873623,
1.530289951387));
#194063=CARTESIAN_POINT('Ctrl Pts',(-18.0808430656785,21.2247567998778,
1.53099669198937));
#194064=CARTESIAN_POINT('Ctrl Pts',(-17.9457581876221,21.1801021467023,
1.53939274105539));
#194065=CARTESIAN_POINT('Ctrl Pts',(-17.8259909109847,21.1278249250091,
1.54648533894591));
#194066=CARTESIAN_POINT('Ctrl Pts',(-17.5697567012959,20.9865368072029,
1.56238143050949));
#194067=CARTESIAN_POINT('Ctrl Pts',(-17.4372178433931,20.892172943223,1.5711604336109));
#194068=CARTESIAN_POINT('Ctrl Pts',(-17.2991282904203,20.7677257801433,
1.58195444034238));
#194069=CARTESIAN_POINT('Ctrl Pts',(-17.2817714598471,20.7515467139499,
1.58334382814564));
#194070=CARTESIAN_POINT('Ctrl Pts',(-17.2577302603234,20.7283694778242,
1.58531689758181));
#194071=CARTESIAN_POINT('Ctrl Pts',(-17.2508159379729,20.7216116343901,
1.58589018191496));
#194072=CARTESIAN_POINT('Ctrl Pts',(-17.2396938405766,20.710591268333,1.58682196063981));
#194073=CARTESIAN_POINT('Ctrl Pts',(-17.2354573881051,20.7063577864015,
1.58717917308321));
#194074=CARTESIAN_POINT('Ctrl Pts',(-17.226656353439,20.6974879622328,1.58792610575059));
#194075=CARTESIAN_POINT('Ctrl Pts',(-17.2220950719861,20.6928484463236,
1.5883159655961));
#194076=CARTESIAN_POINT('Ctrl Pts',(-17.2113471488286,20.6818148940398,
1.5892411921529));
#194077=CARTESIAN_POINT('Ctrl Pts',(-17.2051793219487,20.6754027752964,
1.58977737082846));
#194078=CARTESIAN_POINT('Ctrl Pts',(-17.1847748553258,20.6539207300488,
1.59156881988248));
#194079=CARTESIAN_POINT('Ctrl Pts',(-17.1707195237632,20.6386809471077,
1.59283182937378));
#194080=CARTESIAN_POINT('Ctrl Pts',(-17.0968888195151,20.5562308746983,
1.59962552830862));
#194081=CARTESIAN_POINT('Ctrl Pts',(-17.0412259293054,20.4854769397015,
1.60532414920766));
#194082=CARTESIAN_POINT('Ctrl Pts',(-16.9134494572044,20.2998630129998,
1.61992773361721));
#194083=CARTESIAN_POINT('Ctrl Pts',(-16.8475448694516,20.1812114728228,
1.62897837382845));
#194084=CARTESIAN_POINT('Ctrl Pts',(-16.7632447013434,19.9878630755169,
1.64277153526155));
#194085=CARTESIAN_POINT('Ctrl Pts',(-16.7367835348864,19.9170606157419,
1.64763344815371));
#194086=CARTESIAN_POINT('Ctrl Pts',(-16.7113186000928,19.8359312469652,
1.65288523437605));
#194087=CARTESIAN_POINT('Ctrl Pts',(-16.7085367006307,19.8268551287328,
1.653468338077));
#194088=CARTESIAN_POINT('Ctrl Pts',(-16.7045032143848,19.8133726197446,
1.6543276685691));
#194089=CARTESIAN_POINT('Ctrl Pts',(-16.703204770918,19.808980530025,1.65460652995822));
#194090=CARTESIAN_POINT('Ctrl Pts',(-16.7009191219284,19.801155826853,1.65510137735914));
#194091=CARTESIAN_POINT('Ctrl Pts',(-16.6999263418062,19.7977249018458,
1.65531768476355));
#194092=CARTESIAN_POINT('Ctrl Pts',(-16.6978096797043,19.7903400344377,
1.6557818254181));
#194093=CARTESIAN_POINT('Ctrl Pts',(-16.6966886322303,19.7863853381737,
1.65602949295948));
#194094=CARTESIAN_POINT('Ctrl Pts',(-16.6936239227215,19.7754527712034,
1.6567117762454));
#194095=CARTESIAN_POINT('Ctrl Pts',(-16.6917045229514,19.7684680757904,
1.65714500418878));
#194096=CARTESIAN_POINT('Ctrl Pts',(-16.6813531719808,19.7300284188622,
1.65951524848396));
#194097=CARTESIAN_POINT('Ctrl Pts',(-16.673611532173,19.6983901152728,1.66141475411808));
#194098=CARTESIAN_POINT('Ctrl Pts',(-16.631599073941,19.5077414685826,1.67262337897791));
#194099=CARTESIAN_POINT('Ctrl Pts',(-16.6150144979466,19.3453779231829,
1.68122065938082));
#194100=CARTESIAN_POINT('Ctrl Pts',(-16.6187508090477,19.0658798490546,
1.69652311335512));
#194101=CARTESIAN_POINT('Ctrl Pts',(-16.6299799312674,18.9494024320638,
1.70304537510243));
#194102=CARTESIAN_POINT('Ctrl Pts',(-16.6532984614773,18.8203923877595,
1.71072567854626));
#194103=CARTESIAN_POINT('Ctrl Pts',(-16.6559824232015,18.8063567809064,
1.71156718170344));
#194104=CARTESIAN_POINT('Ctrl Pts',(-16.6604801797896,18.7840620235293,
1.71291375121977));
#194105=CARTESIAN_POINT('Ctrl Pts',(-16.6622017480682,18.7757845583075,
1.71341587634892));
#194106=CARTESIAN_POINT('Ctrl Pts',(-16.6653254310486,18.7612042494906,
1.71430427736137));
#194107=CARTESIAN_POINT('Ctrl Pts',(-16.6667068923005,18.7548970567565,
1.71468988721356));
#194108=CARTESIAN_POINT('Ctrl Pts',(-16.6696238737885,18.7418648460967,
1.71548939009626));
#194109=CARTESIAN_POINT('Ctrl Pts',(-16.6711634515581,18.7351408236042,
1.71590340947901));
#194110=CARTESIAN_POINT('Ctrl Pts',(-16.6751997173664,18.7179003915304,
1.71696890022436));
#194111=CARTESIAN_POINT('Ctrl Pts',(-16.6777441101175,18.7073954565501,
1.71762190105234));
#194112=CARTESIAN_POINT('Ctrl Pts',(-16.6886997835749,18.6636308631386,
1.72035845384063));
#194113=CARTESIAN_POINT('Ctrl Pts',(-16.6978380839052,18.6305601819208,
1.72246534820482));
#194114=CARTESIAN_POINT('Ctrl Pts',(-16.7237398248229,18.5449819924262,
1.72802300836551));
#194115=CARTESIAN_POINT('Ctrl Pts',(-16.7417564684323,18.4928838198673,
1.73151221538506));
#194116=CARTESIAN_POINT('Ctrl Pts',(-16.8015456967986,18.3396347969966,
1.74208581381004));
#194117=CARTESIAN_POINT('Ctrl Pts',(-16.8491452091636,18.2409608757493,
1.74931858449843));
#194118=CARTESIAN_POINT('Ctrl Pts',(-16.9285005074288,18.1045619344368,
1.75974265669016));
#194119=CARTESIAN_POINT('Ctrl Pts',(-16.9542796738513,18.0635552702121,
1.76293490421929));
#194120=CARTESIAN_POINT('Ctrl Pts',(-16.9913642549095,18.0088259373301,
1.76724780316153));
#194121=CARTESIAN_POINT('Ctrl Pts',(-17.0014688803577,17.9943086829254,
1.7683970128548));
#194122=CARTESIAN_POINT('Ctrl Pts',(-17.0427753808773,17.9365220989961,
1.77298776232825));
#194123=CARTESIAN_POINT('Ctrl Pts',(-17.0754285061932,17.8943085900685,
1.77637885811053));
#194124=CARTESIAN_POINT('Ctrl Pts',(-17.1152365163026,17.8466797224422,
1.78020805360985));
#194125=CARTESIAN_POINT('Ctrl Pts',(-17.1208699462202,17.8400235335685,
1.78074325128853));
#194126=CARTESIAN_POINT('Ctrl Pts',(-17.1294617383259,17.8299981662177,
1.7815491945669));
#194127=CARTESIAN_POINT('Ctrl Pts',(-17.1323898605233,17.8266033588356,
1.78182207696204));
#194128=CARTESIAN_POINT('Ctrl Pts',(-17.1376650503803,17.8205265447025,
1.78231045455654));
#194129=CARTESIAN_POINT('Ctrl Pts',(-17.1400081157676,17.8178411523271,
1.78252623786829));
#194130=CARTESIAN_POINT('Ctrl Pts',(-17.1451139404862,17.8120190992982,
1.7829939863762));
#194131=CARTESIAN_POINT('Ctrl Pts',(-17.1478792022982,17.8088847100052,
1.78324576054905));
#194132=CARTESIAN_POINT('Ctrl Pts',(-17.155672242294,17.8001039555202,1.78395102770169));
#194133=CARTESIAN_POINT('Ctrl Pts',(-17.1607210687068,17.7944762383457,
1.78440297492255));
#194134=CARTESIAN_POINT('Ctrl Pts',(-17.1910744505373,17.761005064852,1.78709140166385));
#194135=CARTESIAN_POINT('Ctrl Pts',(-17.2170891566877,17.7338113017969,
1.78927749713153));
#194136=CARTESIAN_POINT('Ctrl Pts',(-17.3050623907025,17.6466274838278,
1.79635040381578));
#194137=CARTESIAN_POINT('Ctrl Pts',(-17.3699642977016,17.5897248801626,
1.80107399952186));
#194138=CARTESIAN_POINT('Ctrl Pts',(-17.5778061456249,17.428841162142,1.81537759309751));
#194139=CARTESIAN_POINT('Ctrl Pts',(-17.7304096845272,17.3386554312784,
1.82486619265082));
#194140=CARTESIAN_POINT('Ctrl Pts',(-17.9134545786712,17.2593547823782,
1.83645888797792));
#194141=CARTESIAN_POINT('Ctrl Pts',(-17.934621891721,17.2505897307822,1.8378011256653));
#194142=CARTESIAN_POINT('Ctrl Pts',(-17.9647922760009,17.2386665212445,
1.83971832511273));
#194143=CARTESIAN_POINT('Ctrl Pts',(-17.973681311151,17.235222846334,1.84028367620528));
#194144=CARTESIAN_POINT('Ctrl Pts',(-17.9881693161024,17.2297223400254,
1.84120604127702));
#194145=CARTESIAN_POINT('Ctrl Pts',(-17.9937543169603,17.2276289044716,
1.84156182445295));
#194146=CARTESIAN_POINT('Ctrl Pts',(-18.0054692936836,17.2232941339921,
1.84230859983847));
#194147=CARTESIAN_POINT('Ctrl Pts',(-18.0116009288726,17.221057493202,1.84269974420532));
#194148=CARTESIAN_POINT('Ctrl Pts',(-18.0262232058863,17.2158002043669,
1.84363323022021));
#194149=CARTESIAN_POINT('Ctrl Pts',(-18.0347229338106,17.2128053659475,
1.84417642341575));
#194150=CARTESIAN_POINT('Ctrl Pts',(-18.0634738043621,17.2028810431611,
1.84601587832944));
#194151=CARTESIAN_POINT('Ctrl Pts',(-18.0838103256414,17.196204611278,1.84732045807473));
#194152=CARTESIAN_POINT('Ctrl Pts',(-18.1954197622506,17.1614292166487,
1.85450128670511));
#194153=CARTESIAN_POINT('Ctrl Pts',(-18.2884010228921,17.139226277544,1.86056765281151));
#194154=CARTESIAN_POINT('Ctrl Pts',(-18.5505639581331,17.0950916987946,
1.87784520501006));
#194155=CARTESIAN_POINT('Ctrl Pts',(-18.7213642528363,17.0871935141841,
1.88934038074912));
#194156=CARTESIAN_POINT('Ctrl Pts',(-18.9278551191995,17.10257503266,1.90255504073256));
#194157=CARTESIAN_POINT('Ctrl Pts',(-18.9643760218696,17.1062522922644,
1.9048632364457));
#194158=CARTESIAN_POINT('Ctrl Pts',(-19.007864637526,17.1117767896868,1.90756276575745));
#194159=CARTESIAN_POINT('Ctrl Pts',(-19.0149395416,17.1127119111806,1.90800037641221));
#194160=CARTESIAN_POINT('Ctrl Pts',(-19.0264784023802,17.1142964610959,
1.90871140342267));
#194161=CARTESIAN_POINT('Ctrl Pts',(-19.0309451842789,17.1149244039595,
1.9089859868437));
#194162=CARTESIAN_POINT('Ctrl Pts',(-19.0389395101046,17.1160743186059,
1.90947619136222));
#194163=CARTESIAN_POINT('Ctrl Pts',(-19.0424677604797,17.1165909289878,
1.90969211004854));
#194164=CARTESIAN_POINT('Ctrl Pts',(-19.0501085124337,17.1177294233781,
1.91015876390807));
#194165=CARTESIAN_POINT('Ctrl Pts',(-19.0542204787161,17.1183545106066,
1.91040931553867));
#194166=CARTESIAN_POINT('Ctrl Pts',(-19.0657080617744,17.1201354667003,
1.91110771447887));
#194167=CARTESIAN_POINT('Ctrl Pts',(-19.0730795298178,17.1213182512444,
1.91155406405324));
#194168=CARTESIAN_POINT('Ctrl Pts',(-19.1159773692034,17.1284343701754,
1.91414184735344));
#194169=CARTESIAN_POINT('Ctrl Pts',(-19.1513562307166,17.1352349751963,
1.91623718646327));
#194170=CARTESIAN_POINT('Ctrl Pts',(-19.2647982224745,17.1600590509605,
1.92287977136236));
#194171=CARTESIAN_POINT('Ctrl Pts',(-19.3420213067432,17.181611514481,1.92728568404138));
#194172=CARTESIAN_POINT('Ctrl Pts',(-19.5935406000503,17.2674606282222,
1.94177388425946));
#194173=CARTESIAN_POINT('Ctrl Pts',(-19.7605673945307,17.3502719959322,
1.95170323443065));
#194174=CARTESIAN_POINT('Ctrl Pts',(-19.9329942577577,17.4661246233785,
1.96378511893577));
#194175=CARTESIAN_POINT('Ctrl Pts',(-19.9511416933849,17.4787346178818,
1.96508050629727));
#194176=CARTESIAN_POINT('Ctrl Pts',(-19.9759568881357,17.4965602614094,
1.96688661928272));
#194177=CARTESIAN_POINT('Ctrl Pts',(-19.9827961457548,17.5015355480619,
1.96738812047849));
#194178=CARTESIAN_POINT('Ctrl Pts',(-19.9944985900138,17.5101563145602,
1.96825273673944));
#194179=CARTESIAN_POINT('Ctrl Pts',(-19.9993762622033,17.513782025904,1.96861508126713));
#194180=CARTESIAN_POINT('Ctrl Pts',(-20.0092317980577,17.5211740252801,
1.96935124480031));
#194181=CARTESIAN_POINT('Ctrl Pts',(-20.0142087493364,17.5249414243735,
1.9697251051651));
#194182=CARTESIAN_POINT('Ctrl Pts',(-20.0257363123027,17.5337479015135,
1.97059598368412));
#194183=CARTESIAN_POINT('Ctrl Pts',(-20.0322741895855,17.5388034122657,
1.97109364834265));
#194184=CARTESIAN_POINT('Ctrl Pts',(-20.0459552464992,17.5495110890584,
1.9721430325731));
#194185=CARTESIAN_POINT('Ctrl Pts',(-20.0530918697995,17.5551713237902,
1.97269506840962));
#194186=CARTESIAN_POINT('Ctrl Pts',(-20.0719930252715,17.5703620461178,
1.97416961822842));
#194187=CARTESIAN_POINT('Ctrl Pts',(-20.0836920576686,17.5799728505687,
1.97509534458661));
#194188=CARTESIAN_POINT('Ctrl Pts',(-20.1190530954181,17.6096630706265,
1.9779339251842));
#194189=CARTESIAN_POINT('Ctrl Pts',(-20.142376745457,17.6301373164522,1.97986259971846));
#194190=CARTESIAN_POINT('Ctrl Pts',(-20.2893723186999,17.7650102287499,
1.99238949493841));
#194191=CARTESIAN_POINT('Ctrl Pts',(-20.3994497338085,17.8933013198049,
2.00357762924864));
#194192=CARTESIAN_POINT('Ctrl Pts',(-20.5482373928072,18.1155372990444,
2.02119561177938));
#194193=CARTESIAN_POINT('Ctrl Pts',(-20.5974955279141,18.2016017037933,
2.02764827953092));
#194194=CARTESIAN_POINT('Ctrl Pts',(-20.64476467428,18.2995388947264,2.03436721312591));
#194195=CARTESIAN_POINT('Ctrl Pts',(-20.6489187114157,18.3082988735037,
2.03496288620485));
#194196=CARTESIAN_POINT('Ctrl Pts',(-20.6549630915623,18.3212746828114,
2.03583709280972));
#194197=CARTESIAN_POINT('Ctrl Pts',(-20.6568999795341,18.3254685161823,
2.03611839220426));
#194198=CARTESIAN_POINT('Ctrl Pts',(-20.6603117270552,18.3329197556956,
2.03661592599245));
#194199=CARTESIAN_POINT('Ctrl Pts',(-20.6617920753978,18.3361745888801,
2.03683249527066));
#194200=CARTESIAN_POINT('Ctrl Pts',(-20.6649460109766,18.3431560104152,
2.03729538221783));
#194201=CARTESIAN_POINT('Ctrl Pts',(-20.6666170559021,18.3468836863881,
2.03754154370137));
#194202=CARTESIAN_POINT('Ctrl Pts',(-20.6711741840977,18.3571288232929,
2.03821543231835));
#194203=CARTESIAN_POINT('Ctrl Pts',(-20.674038188588,18.3636561288024,2.0386418275163));
#194204=CARTESIAN_POINT('Ctrl Pts',(-20.6891489412836,18.3985730439408,
2.04090771294289));
#194205=CARTESIAN_POINT('Ctrl Pts',(-20.7008063082492,18.4272155179464,
2.04271348048651));
#194206=CARTESIAN_POINT('Ctrl Pts',(-20.7341848426354,18.5146675928256,
2.04809769033837));
#194207=CARTESIAN_POINT('Ctrl Pts',(-20.7539266266334,18.5741987773712,
2.05158943073611));
#194208=CARTESIAN_POINT('Ctrl Pts',(-20.824016430556,18.8218628606598,2.06573534679006));
#194209=CARTESIAN_POINT('Ctrl Pts',(-20.850932996752,19.0155969878599,2.07601666321669));
#194210=CARTESIAN_POINT('Ctrl Pts',(-20.8509998750783,19.2102727321581,
2.08722602201617));
#194211=CARTESIAN_POINT('Ctrl Pts',(-20.7227695185423,19.9371792543491,
2.1335156684528));
#194212=CARTESIAN_POINT('Ctrl Pts',(-20.8048848906457,19.7049845745767,
2.11869587197603));
#194213=CARTESIAN_POINT('Ctrl Pts',(-20.8469525718855,19.4574404677657,
2.10387607549926));
#194214=CARTESIAN_POINT('Ctrl Pts',(-20.8478239987731,19.2101685861784,
2.0890562790225));
#194215=CARTESIAN_POINT('Origin',(-18.734,19.211,0.));
#194216=CARTESIAN_POINT('',(-20.7225806782364,19.9371101060755,3.15472451729439));
#194217=CARTESIAN_POINT('',(-20.722580576248,19.9371103853886,2.93545682861291));
#194218=CARTESIAN_POINT('',(-20.7225806064498,19.9371103026755,0.));
#194219=CARTESIAN_POINT('',(-20.850999955063,19.2105638083985,3.11292714750027));
#194220=CARTESIAN_POINT('Ctrl Pts',(-20.7225806782367,19.9371101060747,
3.15472451729435));
#194221=CARTESIAN_POINT('Ctrl Pts',(-20.785411417517,19.7650370374217,3.14472561691515));
#194222=CARTESIAN_POINT('Ctrl Pts',(-20.825700349719,19.5853831201472,3.13494347122732));
#194223=CARTESIAN_POINT('Ctrl Pts',(-20.8447697707137,19.3755532461302,
3.12275001213983));
#194224=CARTESIAN_POINT('Ctrl Pts',(-20.846707234681,19.3484584918627,3.12116300122428));
#194225=CARTESIAN_POINT('Ctrl Pts',(-20.8486554029297,19.31112969335,3.11895645481964));
#194226=CARTESIAN_POINT('Ctrl Pts',(-20.849114096932,19.3009209655022,3.1183509463616));
#194227=CARTESIAN_POINT('Ctrl Pts',(-20.849728275587,19.2846205866491,3.11738069348166));
#194228=CARTESIAN_POINT('Ctrl Pts',(-20.8499314061084,19.2785308103528,
3.11701744584967));
#194229=CARTESIAN_POINT('Ctrl Pts',(-20.8502862993193,19.2663076837636,
3.11628678408661));
#194230=CARTESIAN_POINT('Ctrl Pts',(-20.8504376956161,19.2601743827262,
3.11591936206823));
#194231=CARTESIAN_POINT('Ctrl Pts',(-20.8507174560956,19.2464168823187,
3.11509339266041));
#194232=CARTESIAN_POINT('Ctrl Pts',(-20.850831292037,19.2387925020608,3.11463439433882));
#194233=CARTESIAN_POINT('Ctrl Pts',(-20.8509693632007,19.2242998895109,
3.11375949559301));
#194234=CARTESIAN_POINT('Ctrl Pts',(-20.8510013701658,19.217431828255,3.1133438460819));
#194235=CARTESIAN_POINT('Ctrl Pts',(-20.850999955063,19.2105638083985,3.11292714750027));
#194236=CARTESIAN_POINT('Ctrl Pts',(-20.85099995523,19.2105646193066,3.11292719669993));
#194237=CARTESIAN_POINT('Ctrl Pts',(-20.8509977754103,19.1999654398095,
3.11228412019782));
#194238=CARTESIAN_POINT('Ctrl Pts',(-20.850915995346,19.1893665416074,3.11163855555496));
#194239=CARTESIAN_POINT('Ctrl Pts',(-20.8504276815245,19.1572969635354,
3.10967750172564));
#194240=CARTESIAN_POINT('Ctrl Pts',(-20.8497740575474,19.1358319766212,
3.10835440386201));
#194241=CARTESIAN_POINT('Ctrl Pts',(-20.8411283414657,18.9465942990346,
3.0965948009523));
#194242=CARTESIAN_POINT('Ctrl Pts',(-20.8135227192111,18.7803420861453,
3.08553279276271));
#194243=CARTESIAN_POINT('Ctrl Pts',(-20.7432715722678,18.5390867304095,
3.06893612399543));
#194244=CARTESIAN_POINT('Ctrl Pts',(-20.7152531445003,18.4604818545801,
3.06345029913019));
#194245=CARTESIAN_POINT('Ctrl Pts',(-20.6682556445442,18.3497772264329,
3.05577794756062));
#194246=CARTESIAN_POINT('Ctrl Pts',(-20.6529556395076,18.3162043807657,
3.05345918018755));
#194247=CARTESIAN_POINT('Ctrl Pts',(-20.6334899111243,18.2762895695352,
3.05072678385532));
#194248=CARTESIAN_POINT('Ctrl Pts',(-20.6301587543699,18.2695503234881,
3.05026629891224));
#194249=CARTESIAN_POINT('Ctrl Pts',(-20.6249238390602,18.2591000958969,
3.04955374629547));
#194250=CARTESIAN_POINT('Ctrl Pts',(-20.6230449320338,18.2553768326334,
3.049300171825));
#194251=CARTESIAN_POINT('Ctrl Pts',(-20.6195396037895,18.2484813715494,
3.04883114050058));
#194252=CARTESIAN_POINT('Ctrl Pts',(-20.6179161876382,18.2453077582299,
3.04861550580104));
#194253=CARTESIAN_POINT('Ctrl Pts',(-20.6142273568779,18.2381411740061,
3.04812908442373));
#194254=CARTESIAN_POINT('Ctrl Pts',(-20.6121572409978,18.2341506831601,
3.04785859798749));
#194255=CARTESIAN_POINT('Ctrl Pts',(-20.6060078864863,18.2223885952509,
3.04706231348817));
#194256=CARTESIAN_POINT('Ctrl Pts',(-20.6018929525113,18.2146356285688,
3.04653871361708));
#194257=CARTESIAN_POINT('Ctrl Pts',(-20.5717301719462,18.1586494315956,
3.04276526587493));
#194258=CARTESIAN_POINT('Ctrl Pts',(-20.5438634644742,18.1114140592089,
3.03962253504811));
#194259=CARTESIAN_POINT('Ctrl Pts',(-20.4242378302051,17.9255378147647,
3.02720652788796));
#194260=CARTESIAN_POINT('Ctrl Pts',(-20.3181325530796,17.7968400739698,
3.01845185057355));
#194261=CARTESIAN_POINT('Ctrl Pts',(-20.154583678917,17.6402506638012,3.00591103511555));
#194262=CARTESIAN_POINT('Ctrl Pts',(-20.1093577520868,17.6005026498559,
3.00252978065241));
#194263=CARTESIAN_POINT('Ctrl Pts',(-20.0340386336047,17.5397953261327,
2.99697490314731));
#194264=CARTESIAN_POINT('Ctrl Pts',(-20.0049867810244,17.5175957727333,
2.99484944804649));
#194265=CARTESIAN_POINT('Ctrl Pts',(-19.9687427363683,17.4913586327558,
2.99221161301274));
#194266=CARTESIAN_POINT('Ctrl Pts',(-19.9620817807088,17.4865954088437,
2.9917273929548));
#194267=CARTESIAN_POINT('Ctrl Pts',(-19.9491828825018,17.4774840993406,
2.990790691494));
#194268=CARTESIAN_POINT('Ctrl Pts',(-19.9429488114991,17.4731307343099,
2.99033842102202));
#194269=CARTESIAN_POINT('Ctrl Pts',(-19.9366515568343,17.4687835280316,
2.98988197227961));
#194270=CARTESIAN_POINT('Ctrl Pts',(-19.9366116282065,17.4687559659863,
2.9898790781186));
#194271=CARTESIAN_POINT('Ctrl Pts',(-19.9365301425433,17.4686997219697,
2.9898731717975));
#194272=CARTESIAN_POINT('Ctrl Pts',(-19.9364885854512,17.4686710401278,
2.98987015963466));
#194273=CARTESIAN_POINT('Ctrl Pts',(-19.9364037345947,17.4686124823107,
2.98986400946673));
#194274=CARTESIAN_POINT('Ctrl Pts',(-19.9363604407185,17.4685826064453,
2.98986087145505));
#194275=CARTESIAN_POINT('Ctrl Pts',(-19.936271997837,17.4685215794089,2.98985446100809));
#194276=CARTESIAN_POINT('Ctrl Pts',(-19.9362268486726,17.4684904283363,
2.98985118856294));
#194277=CARTESIAN_POINT('Ctrl Pts',(-19.9361345647791,17.468426761527,2.98984449980009));
#194278=CARTESIAN_POINT('Ctrl Pts',(-19.9360874300691,17.4683942460359,
2.98984108348563));
#194279=CARTESIAN_POINT('Ctrl Pts',(-19.9359910322673,17.4683277525793,
2.98983409663849));
#194280=CARTESIAN_POINT('Ctrl Pts',(-19.9359417689632,17.4682937747276,
2.98983052609251));
#194281=CARTESIAN_POINT('Ctrl Pts',(-19.9358409559903,17.4682242483827,
2.9898232193383));
#194282=CARTESIAN_POINT('Ctrl Pts',(-19.9357894061808,17.4681887000846,
2.98981948312222));
#194283=CARTESIAN_POINT('Ctrl Pts',(-19.9356838453768,17.4681159131875,
2.98981183236436));
#194284=CARTESIAN_POINT('Ctrl Pts',(-19.9356298343095,17.4680786748676,
2.98980791781996));
#194285=CARTESIAN_POINT('Ctrl Pts',(-19.9355191572701,17.4680023753746,
2.98979989637337));
#194286=CARTESIAN_POINT('Ctrl Pts',(-19.9354624911111,17.4679633144452,
2.98979578946063));
#194287=CARTESIAN_POINT('Ctrl Pts',(-19.9353462882075,17.4678832222028,
2.98978736765489));
#194288=CARTESIAN_POINT('Ctrl Pts',(-19.9352867512011,17.4678421911321,
2.9897830527463));
#194289=CARTESIAN_POINT('Ctrl Pts',(-19.9351645654217,17.4677579936901,
2.98977419747979));
#194290=CARTESIAN_POINT('Ctrl Pts',(-19.9351019164488,17.4677148276627,
2.98976965711124));
#194291=CARTESIAN_POINT('Ctrl Pts',(-19.9349732364898,17.4676261755824,
2.98976033135096));
#194292=CARTESIAN_POINT('Ctrl Pts',(-19.9349072052411,17.4675806899001,
2.98975554594462));
#194293=CARTESIAN_POINT('Ctrl Pts',(-19.9347714564812,17.4674871906218,
2.98974570807275));
#194294=CARTESIAN_POINT('Ctrl Pts',(-19.9347017386606,17.4674391774465,
2.98974065558987));
#194295=CARTESIAN_POINT('Ctrl Pts',(-19.9345582726968,17.4673403881846,
2.98973025864625));
#194296=CARTESIAN_POINT('Ctrl Pts',(-19.9344845242288,17.4672896126064,
2.98972491416782));
#194297=CARTESIAN_POINT('Ctrl Pts',(-19.9343326063573,17.4671850318566,
2.9897139049437));
#194298=CARTESIAN_POINT('Ctrl Pts',(-19.9342544365194,17.4671312272361,
2.98970824017331));
#194299=CARTESIAN_POINT('Ctrl Pts',(-19.9340932297034,17.4670202838966,
2.98969655805073));
#194300=CARTESIAN_POINT('Ctrl Pts',(-19.9340101923363,17.4669631459029,
2.98969054067828));
#194301=CARTESIAN_POINT('Ctrl Pts',(-19.9338387387249,17.4668451867533,
2.98967811629242));
#194302=CARTESIAN_POINT('Ctrl Pts',(-19.9337503218969,17.4667843663627,
2.98967170924602));
#194303=CARTESIAN_POINT('Ctrl Pts',(-19.9335675181791,17.4666586393566,
2.98965846270114));
#194304=CARTESIAN_POINT('Ctrl Pts',(-19.9334731306912,17.4665937337101,
2.98965162317032));
#194305=CARTESIAN_POINT('Ctrl Pts',(-19.9332776976403,17.4664593673469,
2.98963746183536));
#194306=CARTESIAN_POINT('Ctrl Pts',(-19.9331766513016,17.4663899077427,
2.98963013998798));
#194307=CARTESIAN_POINT('Ctrl Pts',(-19.9329671029273,17.4662458902671,
2.98961495626448));
#194308=CARTESIAN_POINT('Ctrl Pts',(-19.9328585963718,17.4661713312655,
2.98960709407647));
#194309=CARTESIAN_POINT('Ctrl Pts',(-19.9326331730472,17.4660164652386,
2.98959076055715));
#194310=CARTESIAN_POINT('Ctrl Pts',(-19.9325162562616,17.4659361605959,
2.98958228924378));
#194311=CARTESIAN_POINT('Ctrl Pts',(-19.9272497752479,17.4623196413682,
2.98920070767884));
#194312=CARTESIAN_POINT('Ctrl Pts',(-19.9220846377868,17.4588062564452,
2.98882673450909));
#194313=CARTESIAN_POINT('Ctrl Pts',(-19.9101877430885,17.4507906433636,
2.98796592842409));
#194314=CARTESIAN_POINT('Ctrl Pts',(-19.903445581029,17.4463041008862,2.9874785105995));
#194315=CARTESIAN_POINT('Ctrl Pts',(-19.8836695874574,17.4333073543324,
2.9860499362193));
#194316=CARTESIAN_POINT('Ctrl Pts',(-19.8705676486739,17.4249022248315,
2.98510487651262));
#194317=CARTESIAN_POINT('Ctrl Pts',(-19.758331169233,17.3546355149255,2.9770193353589));
#194318=CARTESIAN_POINT('Ctrl Pts',(-19.6543404957147,17.3009452859684,
2.96957791062179));
#194319=CARTESIAN_POINT('Ctrl Pts',(-19.3961388602265,17.1936345862814,
2.95131355151301));
#194320=CARTESIAN_POINT('Ctrl Pts',(-19.2391098901707,17.148706333767,2.94035030369415));
#194321=CARTESIAN_POINT('Ctrl Pts',(-19.0464926728137,17.1169396705471,
2.92794662346129));
#194322=CARTESIAN_POINT('Ctrl Pts',(-19.0143814710994,17.1123988394046,
2.92591453207428));
#194323=CARTESIAN_POINT('Ctrl Pts',(-18.9749926611102,17.1077492145261,
2.92347561768575));
#194324=CARTESIAN_POINT('Ctrl Pts',(-18.9678042213774,17.1069379954831,
2.92303269851357));
#194325=CARTESIAN_POINT('Ctrl Pts',(-18.9565268377359,17.1057238457736,
2.92234140580566));
#194326=CARTESIAN_POINT('Ctrl Pts',(-18.9524407174705,17.1052959532069,
2.92209166429393));
#194327=CARTESIAN_POINT('Ctrl Pts',(-18.9447996294934,17.1045182707032,
2.92162604928551));
#194328=CARTESIAN_POINT('Ctrl Pts',(-18.9412450614059,17.104165586856,2.92141002079775));
#194329=CARTESIAN_POINT('Ctrl Pts',(-18.9331275660419,17.1033809123853,
2.92091796865442));
#194330=CARTESIAN_POINT('Ctrl Pts',(-18.9285641266738,17.1029547425271,
2.92064227481427));
#194331=CARTESIAN_POINT('Ctrl Pts',(-18.914528527399,17.1016899529705,2.9197970777449));
#194332=CARTESIAN_POINT('Ctrl Pts',(-18.9050519220118,17.1009003172099,
2.91923025507764));
#194333=CARTESIAN_POINT('Ctrl Pts',(-18.7766113584994,17.0910690177648,
2.91159598309741));
#194334=CARTESIAN_POINT('Ctrl Pts',(-18.6570773640448,17.092034620886,2.90504371645033));
#194335=CARTESIAN_POINT('Ctrl Pts',(-18.4296594082806,17.1131537684383,
2.8926109792909));
#194336=CARTESIAN_POINT('Ctrl Pts',(-18.3220142797846,17.1316133462094,
2.8867373085778));
#194337=CARTESIAN_POINT('Ctrl Pts',(-18.143322514997,17.1766820108722,2.87648730374147));
#194338=CARTESIAN_POINT('Ctrl Pts',(-18.0714096980329,17.1989557787946,
2.87222125854008));
#194339=CARTESIAN_POINT('Ctrl Pts',(-17.9831708519841,17.2315305461036,
2.8667293547082));
#194340=CARTESIAN_POINT('Ctrl Pts',(-17.9655904226102,17.2382885624412,
2.86562218317031));
#194341=CARTESIAN_POINT('Ctrl Pts',(-17.9401553053867,17.2484575516588,
2.86400042499205));
#194342=CARTESIAN_POINT('Ctrl Pts',(-17.9322271334331,17.2516831476604,
2.86349207839713));
#194343=CARTESIAN_POINT('Ctrl Pts',(-17.9183591816658,17.2574236235625,
2.86259779381244));
#194344=CARTESIAN_POINT('Ctrl Pts',(-17.9124108923423,17.2599177516402,
2.86221256336359));
#194345=CARTESIAN_POINT('Ctrl Pts',(-17.9008813289732,17.2648141915301,
2.86146262116881));
#194346=CARTESIAN_POINT('Ctrl Pts',(-17.895298811504,17.2672134282999,2.86109801723052));
#194347=CARTESIAN_POINT('Ctrl Pts',(-17.8819756874295,17.2730074788069,
2.8602242601708));
#194348=CARTESIAN_POINT('Ctrl Pts',(-17.874244976147,17.2764246623278,2.85971434508585));
#194349=CARTESIAN_POINT('Ctrl Pts',(-17.8464078225822,17.2889292482502,
2.85786751990641));
#194350=CARTESIAN_POINT('Ctrl Pts',(-17.8264238299025,17.2982843165305,
2.85652144180748));
#194351=CARTESIAN_POINT('Ctrl Pts',(-17.6393416843702,17.3894546890769,
2.84372334794477));
#194352=CARTESIAN_POINT('Ctrl Pts',(-17.4835971715653,17.4926376674441,
2.83146747950523));
#194353=CARTESIAN_POINT('Ctrl Pts',(-17.2831655959475,17.6672562575808,
2.81391777144383));
#194354=CARTESIAN_POINT('Ctrl Pts',(-17.2259703466318,17.7230774609551,
2.80867204112289));
#194355=CARTESIAN_POINT('Ctrl Pts',(-17.1477960780451,17.8085241501172,
2.80129000096494));
#194356=CARTESIAN_POINT('Ctrl Pts',(-17.1242073511821,17.8356639045859,
2.7990314943008));
#194357=CARTESIAN_POINT('Ctrl Pts',(-17.0965701300872,17.8691475140997,
2.79636045805782));
#194358=CARTESIAN_POINT('Ctrl Pts',(-17.0918508289035,17.8749271066005,
2.79590344222051));
#194359=CARTESIAN_POINT('Ctrl Pts',(-17.084549169472,17.8839663724423,2.79519508429811));
#194360=CARTESIAN_POINT('Ctrl Pts',(-17.0819457457191,17.8872088410185,
2.79494226328094));
#194361=CARTESIAN_POINT('Ctrl Pts',(-17.0771274978094,17.8932461430462,
2.79447391830848));
#194362=CARTESIAN_POINT('Ctrl Pts',(-17.0749102024703,17.896038875084,2.79425822096408));
#194363=CARTESIAN_POINT('Ctrl Pts',(-17.0699034054958,17.9023778694491,
2.79377076000355));
#194364=CARTESIAN_POINT('Ctrl Pts',(-17.0671181849839,17.9059274456788,
2.793499302157));
#194365=CARTESIAN_POINT('Ctrl Pts',(-17.0589012460277,17.9164685987238,
2.79269749824917));
#194366=CARTESIAN_POINT('Ctrl Pts',(-17.0535019373629,17.9234854749911,
2.79216939607174));
#194367=CARTESIAN_POINT('Ctrl Pts',(-17.0137761000571,17.9757883448498,
2.78827284917072));
#194368=CARTESIAN_POINT('Ctrl Pts',(-16.9812381365477,18.0224104331941,
2.7850195988906));
#194369=CARTESIAN_POINT('Ctrl Pts',(-16.9357152036213,18.0935809974637,
2.78028178135635));
#194370=CARTESIAN_POINT('Ctrl Pts',(-16.9212746062238,18.1171626424178,
2.77874739362743));
#194371=CARTESIAN_POINT('Ctrl Pts',(-16.8895811214755,18.1712707107043,
2.77529118226473));
#194372=CARTESIAN_POINT('Ctrl Pts',(-16.8726163054525,18.2019564782933,
2.77337620346514));
#194373=CARTESIAN_POINT('Ctrl Pts',(-16.805948584421,18.3299526913423,2.76551935850843));
#194374=CARTESIAN_POINT('Ctrl Pts',(-16.7630542108576,18.4306164895672,
2.75963568995538));
#194375=CARTESIAN_POINT('Ctrl Pts',(-16.7105369056274,18.586251065365,2.75050163253197));
#194376=CARTESIAN_POINT('Ctrl Pts',(-16.6949902021556,18.6390275113436,
2.74740000704839));
#194377=CARTESIAN_POINT('Ctrl Pts',(-16.6731235544017,18.725561115507,2.74226487875214));
#194378=CARTESIAN_POINT('Ctrl Pts',(-16.6655382976033,18.7589727612832,
2.74027058544756));
#194379=CARTESIAN_POINT('Ctrl Pts',(-16.6566319574282,18.8031425176688,
2.73761316136558));
#194380=CARTESIAN_POINT('Ctrl Pts',(-16.6545777056313,18.8137486622724,
2.73697348621668));
#194381=CARTESIAN_POINT('Ctrl Pts',(-16.6513451572067,18.8311508543501,
2.73592118537163));
#194382=CARTESIAN_POINT('Ctrl Pts',(-16.6501187192852,18.8379378418858,
2.73551009862636));
#194383=CARTESIAN_POINT('Ctrl Pts',(-16.6478082738142,18.8510905964199,
2.73471207155915));
#194384=CARTESIAN_POINT('Ctrl Pts',(-16.6467201827165,18.8574555754656,
2.73432526608893));
#194385=CARTESIAN_POINT('Ctrl Pts',(-16.6442742142628,18.872168663406,2.73342966864509));
#194386=CARTESIAN_POINT('Ctrl Pts',(-16.6429372177709,18.8805200887094,
2.73292021953313));
#194387=CARTESIAN_POINT('Ctrl Pts',(-16.6394743591176,18.9030132384448,
2.73154507240444));
#194388=CARTESIAN_POINT('Ctrl Pts',(-16.6374417152992,18.9171686730325,
2.73067644075851));
#194389=CARTESIAN_POINT('Ctrl Pts',(-16.6200061350573,19.0479992694939,
2.72261719298556));
#194390=CARTESIAN_POINT('Ctrl Pts',(-16.6142165511034,19.165729025055,2.71512023312754));
#194391=CARTESIAN_POINT('Ctrl Pts',(-16.6238232368497,19.4468024093604,
2.69674435040332));
#194392=CARTESIAN_POINT('Ctrl Pts',(-16.6483407182322,19.6090885168231,
2.68572645352123));
#194393=CARTESIAN_POINT('Ctrl Pts',(-16.6994365607521,19.7968335156138,
2.67338067920544));
#194394=CARTESIAN_POINT('Ctrl Pts',(-16.7082303693405,19.8265541686603,
2.67144052449234));
#194395=CARTESIAN_POINT('Ctrl Pts',(-16.7198475785932,19.8628664755711,
2.6690966282912));
#194396=CARTESIAN_POINT('Ctrl Pts',(-16.7220554157931,19.8696492784876,
2.66865996345441));
#194397=CARTESIAN_POINT('Ctrl Pts',(-16.7255819053651,19.8802999730684,
2.66797625184641));
#194398=CARTESIAN_POINT('Ctrl Pts',(-16.726877522471,19.8841753543147,2.66772788516232));
#194399=CARTESIAN_POINT('Ctrl Pts',(-16.7293278647538,19.891434724609,2.66726344615056));
#194400=CARTESIAN_POINT('Ctrl Pts',(-16.7304799288485,19.894819500299,2.66704722715218));
#194401=CARTESIAN_POINT('Ctrl Pts',(-16.7331395357272,19.9025690315533,
2.66655293051639));
#194402=CARTESIAN_POINT('Ctrl Pts',(-16.7346527851077,19.9069317769167,
2.66627519426601));
#194403=CARTESIAN_POINT('Ctrl Pts',(-16.7393842309852,19.920429872482,2.6654174585691));
#194404=CARTESIAN_POINT('Ctrl Pts',(-16.7426509064998,19.9295482627064,
2.66484025636619));
#194405=CARTESIAN_POINT('Ctrl Pts',(-16.7824124744682,20.0381821222546,
2.65798667197639));
#194406=CARTESIAN_POINT('Ctrl Pts',(-16.826274378671,20.1348577946083,2.65211547231414));
#194407=CARTESIAN_POINT('Ctrl Pts',(-16.88333536993,20.239052788475,2.64562755017659));
#194408=CARTESIAN_POINT('Ctrl Pts',(-16.8895710858579,20.2501987743916,
2.64493143250745));
#194409=CARTESIAN_POINT('Ctrl Pts',(-16.9500544790224,20.3560498500362,
2.63829480520645));
#194410=CARTESIAN_POINT('Ctrl Pts',(-17.0114482111197,20.4464817715604,
2.63241692555868));
#194411=CARTESIAN_POINT('Ctrl Pts',(-17.126560946372,20.5906773261895,2.62215551166551));
#194412=CARTESIAN_POINT('Ctrl Pts',(-17.1766920750684,20.6470223322504,
2.61788215953077));
#194413=CARTESIAN_POINT('Ctrl Pts',(-17.2429820636454,20.7139670412145,
2.61238144921584));
#194414=CARTESIAN_POINT('Ctrl Pts',(-17.2564250843209,20.727184932008,2.61127322406143));
#194415=CARTESIAN_POINT('Ctrl Pts',(-17.2762277387244,20.7461424533672,
2.60965020281947));
#194416=CARTESIAN_POINT('Ctrl Pts',(-17.2824487445255,20.7520260436863,
2.60914166067777));
#194417=CARTESIAN_POINT('Ctrl Pts',(-17.293418569446,20.7622755241157,2.60824715007469));
#194418=CARTESIAN_POINT('Ctrl Pts',(-17.2981519975476,20.7666577779864,
2.60786189027519));
#194419=CARTESIAN_POINT('Ctrl Pts',(-17.3073822266992,20.7751251989829,
2.60711197864455));
#194420=CARTESIAN_POINT('Ctrl Pts',(-17.3118767345711,20.7792127808178,
2.6067474350332));
#194421=CARTESIAN_POINT('Ctrl Pts',(-17.3226634440892,20.7889383715966,
2.60587396433251));
#194422=CARTESIAN_POINT('Ctrl Pts',(-17.3289718873195,20.7945581384804,
2.60536427640623));
#194423=CARTESIAN_POINT('Ctrl Pts',(-17.3518589644793,20.8147022680002,
2.60351911870323));
#194424=CARTESIAN_POINT('Ctrl Pts',(-17.3686300963038,20.8290048748068,
2.60217450247361));
#194425=CARTESIAN_POINT('Ctrl Pts',(-17.5292434351453,20.961702178104,2.58936291310832));
#194426=CARTESIAN_POINT('Ctrl Pts',(-17.6878756334158,21.0608628026699,
2.57708963256288));
#194427=CARTESIAN_POINT('Ctrl Pts',(-17.9299184228805,21.1709723982243,
2.55953486186786));
#194428=CARTESIAN_POINT('Ctrl Pts',(-18.0042627360628,21.1998499722629,
2.55430033562526));
#194429=CARTESIAN_POINT('Ctrl Pts',(-18.1142120499929,21.2355594814582,
2.54693189779709));
#194430=CARTESIAN_POINT('Ctrl Pts',(-18.1486405530848,21.2457807915411,
2.54467625192697));
#194431=CARTESIAN_POINT('Ctrl Pts',(-18.1905166143594,21.2570621794086,
2.54200813289057));
#194432=CARTESIAN_POINT('Ctrl Pts',(-18.1977288921983,21.2589643393422,
2.5415512845431));
#194433=CARTESIAN_POINT('Ctrl Pts',(-18.2089769290744,21.2618673923712,
2.54084312920023));
#194434=CARTESIAN_POINT('Ctrl Pts',(-18.2130057554708,21.2628945596569,
2.54059034461245));
#194435=CARTESIAN_POINT('Ctrl Pts',(-18.2204956783852,21.2647806669998,
2.54012203267311));
#194436=CARTESIAN_POINT('Ctrl Pts',(-18.2239558860916,21.26564272286,2.53990633214794));
#194437=CARTESIAN_POINT('Ctrl Pts',(-18.2317998435727,21.2675758839695,
2.53941882020694));
#194438=CARTESIAN_POINT('Ctrl Pts',(-18.2361848385281,21.2686417155364,
2.53914731483113));
#194439=CARTESIAN_POINT('Ctrl Pts',(-18.2475193459509,21.2713583652125,
2.53844809037181));
#194440=CARTESIAN_POINT('Ctrl Pts',(-18.2544739301075,21.2729880628731,
2.53802155703353));
#194441=CARTESIAN_POINT('Ctrl Pts',(-18.2973116080084,21.2827979503608,
2.53540885043659));
#194442=CARTESIAN_POINT('Ctrl Pts',(-18.3333970779269,21.2900769983733,
2.53327078911107));
#194443=CARTESIAN_POINT('Ctrl Pts',(-18.5372529005305,21.3256927790929,
2.52145104972034));
#194444=CARTESIAN_POINT('Ctrl Pts',(-18.7077826973774,21.334666545312,2.5124978338181));
#194445=CARTESIAN_POINT('Ctrl Pts',(-18.9729231896225,21.3166449397461,
2.49788064924861));
#194446=CARTESIAN_POINT('Ctrl Pts',(-19.0677262227037,21.3037132206297,
2.49252200499758));
#194447=CARTESIAN_POINT('Ctrl Pts',(-19.18229797623,21.2801004038947,2.48571044509213));
#194448=CARTESIAN_POINT('Ctrl Pts',(-19.2032037384758,21.2754600648055,
2.48445395424378));
#194449=CARTESIAN_POINT('Ctrl Pts',(-19.2328037468124,21.2684170862731,
2.48265414763837));
#194450=CARTESIAN_POINT('Ctrl Pts',(-19.2415590085599,21.266274700308,2.4821191940547));
#194451=CARTESIAN_POINT('Ctrl Pts',(-19.2566302414693,21.2624846413908,
2.48119374149794));
#194452=CARTESIAN_POINT('Ctrl Pts',(-19.2629528116407,21.2608635380793,
2.48080410506403));
#194453=CARTESIAN_POINT('Ctrl Pts',(-19.275038000158,21.2577052675881,2.48005662277461));
#194454=CARTESIAN_POINT('Ctrl Pts',(-19.2808018258988,21.2561729345095,
2.47969893689682));
#194455=CARTESIAN_POINT('Ctrl Pts',(-19.2957593893355,21.2521286639712,
2.47876759098365));
#194456=CARTESIAN_POINT('Ctrl Pts',(-19.304942700576,21.2495789811543,2.47819270922806));
#194457=CARTESIAN_POINT('Ctrl Pts',(-19.3361290817075,21.2406930429304,
2.47622976620224));
#194458=CARTESIAN_POINT('Ctrl Pts',(-19.3580458404042,21.2340620366225,
2.47483214555194));
#194459=CARTESIAN_POINT('Ctrl Pts',(-19.5482025801118,21.1731453441004,
2.46254288034587));
#194460=CARTESIAN_POINT('Ctrl Pts',(-19.7091066967145,21.0983481876638,
2.45093578208277));
#194461=CARTESIAN_POINT('Ctrl Pts',(-19.9317626182106,20.95870387719,2.43357188735246));
#194462=CARTESIAN_POINT('Ctrl Pts',(-20.0018586109472,20.9085395630027,
2.42789886920743));
#194463=CARTESIAN_POINT('Ctrl Pts',(-20.097888640167,20.8305400845952,2.42000168768567));
#194464=CARTESIAN_POINT('Ctrl Pts',(-20.126435187597,20.8060633090678,2.41763728485151));
#194465=CARTESIAN_POINT('Ctrl Pts',(-20.159921574675,20.7757663709232,2.414858530903));
#194466=CARTESIAN_POINT('Ctrl Pts',(-20.1654994803408,20.7706651481769,
2.41439549131404));
#194467=CARTESIAN_POINT('Ctrl Pts',(-20.1741190148305,20.7626970356697,
2.41367985103559));
#194468=CARTESIAN_POINT('Ctrl Pts',(-20.1771796121016,20.7598508886571,
2.41342572288789));
#194469=CARTESIAN_POINT('Ctrl Pts',(-20.1828344744696,20.754560937399,2.41295618287214));
#194470=CARTESIAN_POINT('Ctrl Pts',(-20.185430974356,20.7521196672717,2.41274058989437));
#194471=CARTESIAN_POINT('Ctrl Pts',(-20.1912801487014,20.7465922868005,
2.41225491288289));
#194472=CARTESIAN_POINT('Ctrl Pts',(-20.1945291821626,20.7435024019499,
2.41198512511031));
#194473=CARTESIAN_POINT('Ctrl Pts',(-20.2040697009577,20.7343713112875,
2.41119279953939));
#194474=CARTESIAN_POINT('Ctrl Pts',(-20.2103337839112,20.7283014341696,
2.41067242744472));
#194475=CARTESIAN_POINT('Ctrl Pts',(-20.2546652361281,20.684809930901,2.40698706660287));
#194476=CARTESIAN_POINT('Ctrl Pts',(-20.2913461219772,20.6459956622131,
2.40392359083267));
#194477=CARTESIAN_POINT('Ctrl Pts',(-20.3355350676358,20.5955437882601,
2.40015196205096));
#194478=CARTESIAN_POINT('Ctrl Pts',(-20.3444470216982,20.5851675575748,
2.39938689808646));
#194479=CARTESIAN_POINT('Ctrl Pts',(-20.3868880904001,20.5347732200816,
2.39571808119312));
#194480=CARTESIAN_POINT('Ctrl Pts',(-20.4190308258731,20.4936090895913,
2.3928615197817));
#194481=CARTESIAN_POINT('Ctrl Pts',(-20.5137301795037,20.3626178607048,
2.38406090155473));
#194482=CARTESIAN_POINT('Ctrl Pts',(-20.5708676911869,20.2691018000445,
2.37816904471015));
#194483=CARTESIAN_POINT('Ctrl Pts',(-20.6549212208048,20.1040280606797,
2.36786973125037));
#194484=CARTESIAN_POINT('Ctrl Pts',(-20.6856664530823,20.0346709047926,
2.36357209760958));
#194485=CARTESIAN_POINT('Ctrl Pts',(-20.7160027946319,19.954938307128,2.35859155954439));
#194486=CARTESIAN_POINT('Ctrl Pts',(-20.719321761882,19.9460352209481,2.35803492211194));
#194487=CARTESIAN_POINT('Ctrl Pts',(-20.7225806064941,19.9371103025544,
2.35747633162257));
#194488=CARTESIAN_POINT('',(-20.8499621049652,19.2128841874121,2.8890562790225));
#194489=CARTESIAN_POINT('Ctrl Pts',(-20.8499621049652,19.2128841874121,
2.8890562790225));
#194490=CARTESIAN_POINT('Ctrl Pts',(-20.845633252063,18.7070050108363,2.85866010167885));
#194491=CARTESIAN_POINT('Ctrl Pts',(-20.4101935901701,17.4889118801332,
2.78587198877473));
#194492=CARTESIAN_POINT('Ctrl Pts',(-18.3741968228298,16.7337288824509,
2.6706919403101));
#194493=CARTESIAN_POINT('Ctrl Pts',(-16.4562523864159,18.1726376448454,
2.54351613362869));
#194494=CARTESIAN_POINT('Ctrl Pts',(-16.6280000106062,20.564179464316,2.41634032694724));
#194495=CARTESIAN_POINT('Ctrl Pts',(-18.731871915622,21.7142630277803,2.28916452026582));
#194496=CARTESIAN_POINT('Ctrl Pts',(-20.2929105264368,20.8643639334257,
2.194889634101));
#194497=CARTESIAN_POINT('Ctrl Pts',(-20.6701805215755,20.085883266734,2.14300668349666));
#194498=CARTESIAN_POINT('Ctrl Pts',(-20.7227695185423,19.9371792543491,
2.1335156684528));
#194499=CARTESIAN_POINT('Ctrl Pts',(-20.8509991255307,19.2129241887627,
2.88845980109392));
#194500=CARTESIAN_POINT('Ctrl Pts',(-20.850855388126,19.3710645780658,2.8988202813796));
#194501=CARTESIAN_POINT('Ctrl Pts',(-20.832993119571,19.5286963706424,2.90945375295789));
#194502=CARTESIAN_POINT('Ctrl Pts',(-20.7934894773314,19.7014647873359,
2.92067365423454));
#194503=CARTESIAN_POINT('Ctrl Pts',(-20.7889879759962,19.7199961557791,
2.92187071866517));
#194504=CARTESIAN_POINT('Ctrl Pts',(-20.7809486400232,19.7512447612192,
2.92387556393314));
#194505=CARTESIAN_POINT('Ctrl Pts',(-20.7775412260559,19.763994045634,2.92468963664369));
#194506=CARTESIAN_POINT('Ctrl Pts',(-20.7726159275808,19.7817552018483,
2.92581747267831));
#194507=CARTESIAN_POINT('Ctrl Pts',(-20.7711984117392,19.7867942628903,
2.92613674703618));
#194508=CARTESIAN_POINT('Ctrl Pts',(-20.7687546217206,19.7953595777528,
2.92667817863929));
#194509=CARTESIAN_POINT('Ctrl Pts',(-20.7677378406046,19.7988884954982,
2.92690088220672));
#194510=CARTESIAN_POINT('Ctrl Pts',(-20.7657731499416,19.8056412010862,
2.92732630744239));
#194511=CARTESIAN_POINT('Ctrl Pts',(-20.7648267450337,19.8088653885898,
2.92752911793041));
#194512=CARTESIAN_POINT('Ctrl Pts',(-20.7623032579457,19.8173872075475,
2.92806436237892));
#194513=CARTESIAN_POINT('Ctrl Pts',(-20.7607130854098,19.8226809811204,
2.92839603643779));
#194514=CARTESIAN_POINT('Ctrl Pts',(-20.7550185535674,19.841372386282,2.92956441330896));
#194515=CARTESIAN_POINT('Ctrl Pts',(-20.7508018310205,19.854735766525,2.93039481478052));
#194516=CARTESIAN_POINT('Ctrl Pts',(-20.7388900140446,19.8912196309275,
2.93265089211074));
#194517=CARTESIAN_POINT('Ctrl Pts',(-20.7309311654813,19.9142408329297,
2.93406225781276));
#194518=CARTESIAN_POINT('Ctrl Pts',(-20.722580576248,19.9371103853886,2.93545682861291));
#194519=CARTESIAN_POINT('Origin',(-18.734,19.211,0.));
#194520=CARTESIAN_POINT('',(-20.7225806759744,19.9371101122702,3.95421657486109));
#194521=CARTESIAN_POINT('',(-20.7225806064494,19.9371103026767,3.73234504707874));
#194522=CARTESIAN_POINT('',(-20.7225806064498,19.9371103026755,0.));
#194523=CARTESIAN_POINT('Ctrl Pts',(-20.7225806759744,19.9371101122702,
3.95421657486109));
#194524=CARTESIAN_POINT('Ctrl Pts',(-20.7432514903791,19.8804994393335,
3.95029631842219));
#194525=CARTESIAN_POINT('Ctrl Pts',(-20.7615069746506,19.8230005145436,
3.94643459043925));
#194526=CARTESIAN_POINT('Ctrl Pts',(-20.7804090216855,19.7532558144153,
3.94195341122591));
#194527=CARTESIAN_POINT('Ctrl Pts',(-20.7834316339718,19.7417176697722,
3.94121863712442));
#194528=CARTESIAN_POINT('Ctrl Pts',(-20.7875891289675,19.725281973163,3.94018189259722));
#194529=CARTESIAN_POINT('Ctrl Pts',(-20.788804268635,19.7204052191809,3.9398755087063));
#194530=CARTESIAN_POINT('Ctrl Pts',(-20.7908681039204,19.7119948194786,
3.93934930571094));
#194531=CARTESIAN_POINT('Ctrl Pts',(-20.7917250850485,19.7084632460899,
3.93912901274259));
#194532=CARTESIAN_POINT('Ctrl Pts',(-20.7933688049833,19.7016126368667,
3.93870298798722));
#194533=CARTESIAN_POINT('Ctrl Pts',(-20.7941566161855,19.6982939067538,
3.9384971923441));
#194534=CARTESIAN_POINT('Ctrl Pts',(-20.796259960111,19.6893370935663,3.93794332966228));
#194535=CARTESIAN_POINT('Ctrl Pts',(-20.7975604025928,19.6836954461399,
3.93759612417221));
#194536=CARTESIAN_POINT('Ctrl Pts',(-20.8022980768524,19.66275002125,3.93631297583456));
#194537=CARTESIAN_POINT('Ctrl Pts',(-20.8055884394275,19.6474130916265,
3.93538507921685));
#194538=CARTESIAN_POINT('Ctrl Pts',(-20.8354454541131,19.5002904502564,
3.9265831659023));
#194539=CARTESIAN_POINT('Ctrl Pts',(-20.8495760163056,19.3662740352944,
3.91931203515023));
#194540=CARTESIAN_POINT('Ctrl Pts',(-20.8509595375063,19.2255206442362,
3.91166810814775));
#194541=CARTESIAN_POINT('Ctrl Pts',(-20.8509933270378,19.2192332133599,
3.91132667341362));
#194542=CARTESIAN_POINT('Ctrl Pts',(-20.8511331455132,19.0671072341399,
3.90306444324088));
#194543=CARTESIAN_POINT('Ctrl Pts',(-20.8361978950863,18.9216640281003,
3.89510372735859));
#194544=CARTESIAN_POINT('Ctrl Pts',(-20.8015323055344,18.7553942923716,
3.8852444687199));
#194545=CARTESIAN_POINT('Ctrl Pts',(-20.7962279556996,18.7319570117017,
3.88383768620377));
#194546=CARTESIAN_POINT('Ctrl Pts',(-20.7882195562543,18.6991743711183,
3.88184395681023));
#194547=CARTESIAN_POINT('Ctrl Pts',(-20.7858481761669,18.6897490845538,
3.88126770468889));
#194548=CARTESIAN_POINT('Ctrl Pts',(-20.781908381504,18.6745335580391,3.8803323966953));
#194549=CARTESIAN_POINT('Ctrl Pts',(-20.7803800924634,18.6687330008068,
3.87997464207438));
#194550=CARTESIAN_POINT('Ctrl Pts',(-20.7771446742841,18.6566615857626,
3.87922760908645));
#194551=CARTESIAN_POINT('Ctrl Pts',(-20.7754332819468,18.6503919448913,
3.87883819566093));
#194552=CARTESIAN_POINT('Ctrl Pts',(-20.7713216375678,18.6355975519863,
3.87791589776476));
#194553=CARTESIAN_POINT('Ctrl Pts',(-20.7688967218961,18.6270798345886,
3.87738221533758));
#194554=CARTESIAN_POINT('Ctrl Pts',(-20.7606830626322,18.5989013000478,
3.87560764047356));
#194555=CARTESIAN_POINT('Ctrl Pts',(-20.7546623949245,18.5793098115203,
3.87435920727821));
#194556=CARTESIAN_POINT('Ctrl Pts',(-20.7212770023923,18.4760372207133,
3.86769851033935));
#194557=CARTESIAN_POINT('Ctrl Pts',(-20.6889996910731,18.3940465179559,
3.86212559133135));
#194558=CARTESIAN_POINT('Ctrl Pts',(-20.5968951046246,18.1970657457696,
3.84804782489255));
#194559=CARTESIAN_POINT('Ctrl Pts',(-20.5314380705507,18.0850987712143,
3.8394138991219));
#194560=CARTESIAN_POINT('Ctrl Pts',(-20.4404261756852,17.9577913240164,
3.82914906247664));
#194561=CARTESIAN_POINT('Ctrl Pts',(-20.4242561905604,17.9360661334745,
3.82738107538567));
#194562=CARTESIAN_POINT('Ctrl Pts',(-20.3724974459434,17.8692418342402,
3.82190424442907));
#194563=CARTESIAN_POINT('Ctrl Pts',(-20.3354839864957,17.8252730584197,
3.81824361855776));
#194564=CARTESIAN_POINT('Ctrl Pts',(-20.2907363631564,17.7763085059287,
3.81415058119492));
#194565=CARTESIAN_POINT('Ctrl Pts',(-20.2847071386254,17.7697938509429,
3.81360566751355));
#194566=CARTESIAN_POINT('Ctrl Pts',(-20.2755483343229,17.7600216634201,
3.81278802704059));
#194567=CARTESIAN_POINT('Ctrl Pts',(-20.2724490988911,17.7567360035834,
3.81251307176792));
#194568=CARTESIAN_POINT('Ctrl Pts',(-20.2668839722237,17.7508738252702,
3.81202246825166));
#194569=CARTESIAN_POINT('Ctrl Pts',(-20.2644220727579,17.7482936049031,
3.81180652034107));
#194570=CARTESIAN_POINT('Ctrl Pts',(-20.2590779441154,17.7427208964985,
3.81134010380499));
#194571=CARTESIAN_POINT('Ctrl Pts',(-20.256193431545,17.7397306775953,3.81108981710817));
#194572=CARTESIAN_POINT('Ctrl Pts',(-20.2481154338852,17.7314058386046,
3.81039290268273));
#194573=CARTESIAN_POINT('Ctrl Pts',(-20.2429025240412,17.7260900342973,
3.80994776240585));
#194574=CARTESIAN_POINT('Ctrl Pts',(-20.2125439966636,17.6954572297961,
3.80738106408755));
#194575=CARTESIAN_POINT('Ctrl Pts',(-20.1867879389767,17.6707500910073,
3.8053047276702));
#194576=CARTESIAN_POINT('Ctrl Pts',(-20.1021428189004,17.5935656325941,
3.79874985702829));
#194577=CARTESIAN_POINT('Ctrl Pts',(-20.0409390952215,17.5437205258226,
3.79440839539127));
#194578=CARTESIAN_POINT('Ctrl Pts',(-19.9033622252448,17.4439182753741,
3.78513898159681));
#194579=CARTESIAN_POINT('Ctrl Pts',(-19.8262581557949,17.3952473096775,
3.78023202309352));
#194580=CARTESIAN_POINT('Ctrl Pts',(-19.6529388749741,17.3008873441964,
3.76938626865495));
#194581=CARTESIAN_POINT('Ctrl Pts',(-19.555937582257,17.2571849194045,3.76342359210836));
#194582=CARTESIAN_POINT('Ctrl Pts',(-19.4428144227744,17.2161390854988,
3.75637198242424));
#194583=CARTESIAN_POINT('Ctrl Pts',(-19.4295076493934,17.2114607907256,
3.75554120807912));
#194584=CARTESIAN_POINT('Ctrl Pts',(-19.4082024232918,17.2042088624856,
3.75420860148586));
#194585=CARTESIAN_POINT('Ctrl Pts',(-19.4002335378382,17.2015492175387,
3.7537096145858));
#194586=CARTESIAN_POINT('Ctrl Pts',(-19.3861206020294,17.1969321513491,
3.75282485681574));
#194587=CARTESIAN_POINT('Ctrl Pts',(-19.3799830095107,17.1949552265478,
3.75243973437528));
#194588=CARTESIAN_POINT('Ctrl Pts',(-19.3672397192858,17.1909147664626,
3.75163935334847));
#194589=CARTESIAN_POINT('Ctrl Pts',(-19.3606327510181,17.1888555228621,
3.7512239590788));
#194590=CARTESIAN_POINT('Ctrl Pts',(-19.3435839467035,17.1836333713012,
3.75015091805408));
#194591=CARTESIAN_POINT('Ctrl Pts',(-19.3331276393709,17.180518751625,3.74949169987412));
#194592=CARTESIAN_POINT('Ctrl Pts',(-19.2888347996529,17.1676971654686,
3.74669429028345));
#194593=CARTESIAN_POINT('Ctrl Pts',(-19.2547845747077,17.1587545659254,
3.74453143921429));
#194594=CARTESIAN_POINT('Ctrl Pts',(-19.1649553149611,17.1375422254497,
3.73878997100111));
#194595=CARTESIAN_POINT('Ctrl Pts',(-19.1088779416,17.1266739102755,3.73516966847652));
#194596=CARTESIAN_POINT('Ctrl Pts',(-18.9020441647172,17.095204476871,3.72170059516301));
#194597=CARTESIAN_POINT('Ctrl Pts',(-18.7496309251215,17.0886007852889,
3.71151325108821));
#194598=CARTESIAN_POINT('Ctrl Pts',(-18.5753891062997,17.0998301631692,
3.70010896947933));
#194599=CARTESIAN_POINT('Ctrl Pts',(-18.5529541797568,17.1016356510266,
3.6986461573074));
#194600=CARTESIAN_POINT('Ctrl Pts',(-18.4794302653382,17.1087343124674,
3.69387852895901));
#194601=CARTESIAN_POINT('Ctrl Pts',(-18.4285005517896,17.1155292187516,
3.69061756279996));
#194602=CARTESIAN_POINT('Ctrl Pts',(-18.3701007822128,17.1254956517456,
3.68696353540444));
#194603=CARTESIAN_POINT('Ctrl Pts',(-18.3623445992239,17.1268638972527,
3.68647999166459));
#194604=CARTESIAN_POINT('Ctrl Pts',(-18.3499899916602,17.1291145003275,
3.68571276483803));
#194605=CARTESIAN_POINT('Ctrl Pts',(-18.3453866325855,17.1299688681116,
3.68542755890813));
#194606=CARTESIAN_POINT('Ctrl Pts',(-18.3372556552558,17.1315058705807,
3.68492501749278));
#194607=CARTESIAN_POINT('Ctrl Pts',(-18.3337268924935,17.1321822231061,
3.68470732836511));
#194608=CARTESIAN_POINT('Ctrl Pts',(-18.3262699935258,17.1336311670206,
3.68424819218868));
#194609=CARTESIAN_POINT('Ctrl Pts',(-18.3223423291099,17.1344059161639,
3.68400686977246));
#194610=CARTESIAN_POINT('Ctrl Pts',(-18.3117892200099,17.1365186808967,
3.68335978788533));
#194611=CARTESIAN_POINT('Ctrl Pts',(-18.3051678819098,17.1378773062455,
3.68295518879082));
#194612=CARTESIAN_POINT('Ctrl Pts',(-18.2728625195408,17.1446674068323,
3.68098749916396));
#194613=CARTESIAN_POINT('Ctrl Pts',(-18.2472732977086,17.1505448508723,
3.67944848146252));
#194614=CARTESIAN_POINT('Ctrl Pts',(-18.1742854569501,17.1687447493238,
3.67509796353542));
#194615=CARTESIAN_POINT('Ctrl Pts',(-18.1271943317503,17.1822382124924,
3.67233871987648));
#194616=CARTESIAN_POINT('Ctrl Pts',(-17.988708883323,17.2271740611538,3.66425503086561));
#194617=CARTESIAN_POINT('Ctrl Pts',(-17.8989529657018,17.263252042426,3.65905221383546));
#194618=CARTESIAN_POINT('Ctrl Pts',(-17.6850100182676,17.3667651877693,
3.64611957534623));
#194619=CARTESIAN_POINT('Ctrl Pts',(-17.5645222591219,17.4407185800776,
3.63833998948033));
#194620=CARTESIAN_POINT('Ctrl Pts',(-17.440920997773,17.5347423537324,3.62924197715143));
#194621=CARTESIAN_POINT('Ctrl Pts',(-17.4296413193198,17.5435044468074,
3.62840087284816));
#194622=CARTESIAN_POINT('Ctrl Pts',(-17.411828880737,17.5576325334598,3.62705481820785));
#194623=CARTESIAN_POINT('Ctrl Pts',(-17.4052379856689,17.5629247729135,
3.62655280543829));
#194624=CARTESIAN_POINT('Ctrl Pts',(-17.3936689366269,17.5723287922984,
3.6256645302439));
#194625=CARTESIAN_POINT('Ctrl Pts',(-17.3886775402258,17.5764241638287,
3.62527893318531));
#194626=CARTESIAN_POINT('Ctrl Pts',(-17.3783915692997,17.5849426889457,
3.62447938510047));
#194627=CARTESIAN_POINT('Ctrl Pts',(-17.3730997318831,17.5893690140154,
3.62406530736619));
#194628=CARTESIAN_POINT('Ctrl Pts',(-17.3595698527088,17.6007988683725,
3.62299951522317));
#194629=CARTESIAN_POINT('Ctrl Pts',(-17.3513637353089,17.6078397251536,
3.62234626975066));
#194630=CARTESIAN_POINT('Ctrl Pts',(-17.3173218762173,17.6375034583948,
3.61960740266274));
#194631=CARTESIAN_POINT('Ctrl Pts',(-17.2919857721781,17.660689378659,3.61749838980813));
#194632=CARTESIAN_POINT('Ctrl Pts',(-17.2274344851288,17.7227142261806,
3.61193382348519));
#194633=CARTESIAN_POINT('Ctrl Pts',(-17.1891562244276,17.7624865965264,
3.60843971050327));
#194634=CARTESIAN_POINT('Ctrl Pts',(-17.0797128785038,17.8854794597193,
3.59785667723224));
#194635=CARTESIAN_POINT('Ctrl Pts',(-17.013404858041,17.9727675999785,3.59061941136421));
#194636=CARTESIAN_POINT('Ctrl Pts',(-16.9252733487927,18.1096186290764,
3.57986716272942));
#194637=CARTESIAN_POINT('Ctrl Pts',(-16.8981025949038,18.1555313458928,
3.57635221990293));
#194638=CARTESIAN_POINT('Ctrl Pts',(-16.8666875789495,18.213507007949,3.57206079716307));
#194639=CARTESIAN_POINT('Ctrl Pts',(-16.8607802235557,18.2246452841926,
3.57124286633408));
#194640=CARTESIAN_POINT('Ctrl Pts',(-16.830403543619,18.2831775952021,3.56698088221409));
#194641=CARTESIAN_POINT('Ctrl Pts',(-16.8076300467672,18.331435492361,3.5635902492921));
#194642=CARTESIAN_POINT('Ctrl Pts',(-16.7832814460662,18.3885268069515,
3.55976151111705));
#194643=CARTESIAN_POINT('Ctrl Pts',(-16.7799103196028,18.396568568314,3.55922633472176));
#194644=CARTESIAN_POINT('Ctrl Pts',(-16.7748813066296,18.4087761889134,
3.55842041456937));
#194645=CARTESIAN_POINT('Ctrl Pts',(-16.773186855971,18.4129267496989,3.55814753426138));
#194646=CARTESIAN_POINT('Ctrl Pts',(-16.7701690500042,18.4203865032507,
3.55765915757875));
#194647=CARTESIAN_POINT('Ctrl Pts',(-16.7688408608608,18.4236936683568,
3.55744337310531));
#194648=CARTESIAN_POINT('Ctrl Pts',(-16.7659730596671,18.4308869099378,
3.55697561975071));
#194649=CARTESIAN_POINT('Ctrl Pts',(-16.7644366080456,18.4347741843195,
3.55672384190667));
#194650=CARTESIAN_POINT('Ctrl Pts',(-16.760153333913,18.445705610263,3.55601855091234));
#194651=CARTESIAN_POINT('Ctrl Pts',(-16.757432688094,18.4527600448411,3.55556658370545));
#194652=CARTESIAN_POINT('Ctrl Pts',(-16.7413975721506,18.4950107529676,
3.55287776383636));
#194653=CARTESIAN_POINT('Ctrl Pts',(-16.7289847772557,18.5305447203492,
3.55069131272691));
#194654=CARTESIAN_POINT('Ctrl Pts',(-16.6912622741091,18.6485491686528,
3.543616671411));
#194655=CARTESIAN_POINT('Ctrl Pts',(-16.6700426742774,18.7322402854818,
3.53889178941334));
#194656=CARTESIAN_POINT('Ctrl Pts',(-16.6211280727965,18.990470157116,3.52458895915509));
#194657=CARTESIAN_POINT('Ctrl Pts',(-16.6101004765044,19.1673495945278,
3.51510219294579));
#194658=CARTESIAN_POINT('Ctrl Pts',(-16.6225876545883,19.3664088391931,
3.50351150892648));
#194659=CARTESIAN_POINT('Ctrl Pts',(-16.6243933011252,19.3892512704385,
3.50216907549365));
#194660=CARTESIAN_POINT('Ctrl Pts',(-16.6274747076475,19.4215494630727,
3.5002516475308));
#194661=CARTESIAN_POINT('Ctrl Pts',(-16.628444202406,19.4310333211593,3.49968626697525));
#194662=CARTESIAN_POINT('Ctrl Pts',(-16.6301243411273,19.4464395624773,
3.4987638693762));
#194663=CARTESIAN_POINT('Ctrl Pts',(-16.6307960234147,19.4523661271407,
3.49840808334582));
#194664=CARTESIAN_POINT('Ctrl Pts',(-16.6322551296475,19.4647717433327,
3.49766131468196));
#194665=CARTESIAN_POINT('Ctrl Pts',(-16.6330474873899,19.4712501412938,
3.4972701799488));
#194666=CARTESIAN_POINT('Ctrl Pts',(-16.6350051359181,19.4866642239923,
3.49633674048221));
#194667=CARTESIAN_POINT('Ctrl Pts',(-16.6361975411364,19.4955962815855,
3.4957935843909));
#194668=CARTESIAN_POINT('Ctrl Pts',(-16.6404140880412,19.5257141744831,
3.49395436811252));
#194669=CARTESIAN_POINT('Ctrl Pts',(-16.6437023615917,19.5468611505771,
3.49264999269345));
#194670=CARTESIAN_POINT('Ctrl Pts',(-16.6634083595606,19.6620588842719,
3.48547106622526));
#194671=CARTESIAN_POINT('Ctrl Pts',(-16.6858512622676,19.7549543611588,
3.47940650833344));
#194672=CARTESIAN_POINT('Ctrl Pts',(-16.7656092587515,20.0086087244211,
3.46212616343468));
#194673=CARTESIAN_POINT('Ctrl Pts',(-16.8361823793679,20.1644290686028,
3.45062579842278));
#194674=CARTESIAN_POINT('Ctrl Pts',(-16.943705152627,20.3414324383234,3.43740901693797));
#194675=CARTESIAN_POINT('Ctrl Pts',(-16.9635516135627,20.37226914308,3.43510302750022));
#194676=CARTESIAN_POINT('Ctrl Pts',(-16.9882058697753,20.4084734861957,
3.43240575397968));
#194677=CARTESIAN_POINT('Ctrl Pts',(-16.9922512190136,20.4143499418328,
3.43196827865283));
#194678=CARTESIAN_POINT('Ctrl Pts',(-16.9989022926969,20.4239077812208,
3.43125742895086));
#194679=CARTESIAN_POINT('Ctrl Pts',(-17.0014901734997,20.4276014308657,
3.43098288842408));
#194680=CARTESIAN_POINT('Ctrl Pts',(-17.0061452649811,20.4342006088516,
3.4304927317174));
#194681=CARTESIAN_POINT('Ctrl Pts',(-17.0082080233292,20.4371091993318,
3.43027681818018));
#194682=CARTESIAN_POINT('Ctrl Pts',(-17.0126930098357,20.4433995082745,
3.42981014222676));
#194683=CARTESIAN_POINT('Ctrl Pts',(-17.015117851103,20.4467792931065,3.42955956353027));
#194684=CARTESIAN_POINT('Ctrl Pts',(-17.0219237596647,20.4562066952139,
3.42886101118834));
#194685=CARTESIAN_POINT('Ctrl Pts',(-17.0263269376507,20.4622383795355,
3.42841453635099));
#194686=CARTESIAN_POINT('Ctrl Pts',(-17.0521734736523,20.4972536239808,
3.4258245441598));
#194687=CARTESIAN_POINT('Ctrl Pts',(-17.0743238979072,20.5257107801461,
3.42372721356036));
#194688=CARTESIAN_POINT('Ctrl Pts',(-17.1480757792327,20.6156248061067,
3.41707538730218));
#194689=CARTESIAN_POINT('Ctrl Pts',(-17.2024494011681,20.6747217138211,
3.41266267814509));
#194690=CARTESIAN_POINT('Ctrl Pts',(-17.3931628851355,20.8597067959543,
3.39817929573788));
#194691=CARTESIAN_POINT('Ctrl Pts',(-17.5426454244653,20.9707575157078,
3.3882600528732));
#194692=CARTESIAN_POINT('Ctrl Pts',(-17.724012075889,21.0716726984023,3.37618901940036));
#194693=CARTESIAN_POINT('Ctrl Pts',(-17.7435122676712,21.0821259965933,
3.37489208203068));
#194694=CARTESIAN_POINT('Ctrl Pts',(-17.7706916734237,21.0961518952964,
3.37308414836764));
#194695=CARTESIAN_POINT('Ctrl Pts',(-17.7782342751361,21.0999871562315,
3.37258240119048));
#194696=CARTESIAN_POINT('Ctrl Pts',(-17.7912345063099,21.1064997164791,
3.37171747298293));
#194697=CARTESIAN_POINT('Ctrl Pts',(-17.796681084978,21.1091989362607,3.37135506376575));
#194698=CARTESIAN_POINT('Ctrl Pts',(-17.8079295628955,21.1147132483312,
3.37060648763457));
#194699=CARTESIAN_POINT('Ctrl Pts',(-17.8137328453446,21.1175253601738,
3.37022022166074));
#194700=CARTESIAN_POINT('Ctrl Pts',(-17.8272607880999,21.1240044742167,
3.36931961415898));
#194701=CARTESIAN_POINT('Ctrl Pts',(-17.8349949570232,21.1276512583466,
3.36880457797297));
#194702=CARTESIAN_POINT('Ctrl Pts',(-17.8597932596405,21.1391609328035,
3.36715262518793));
#194703=CARTESIAN_POINT('Ctrl Pts',(-17.8769396957805,21.1468433838744,
3.36600952837221));
#194704=CARTESIAN_POINT('Ctrl Pts',(-17.962940013082,21.1840092514451,3.36027031371747));
#194705=CARTESIAN_POINT('Ctrl Pts',(-18.0332152737659,21.2100491847617,
3.35555917983213));
#194706=CARTESIAN_POINT('Ctrl Pts',(-18.2086822873976,21.2646764370667,
3.34375254227823));
#194707=CARTESIAN_POINT('Ctrl Pts',(-18.3149835358247,21.2889719274676,
3.33655667270851));
#194708=CARTESIAN_POINT('Ctrl Pts',(-18.5412481554534,21.3226123840721,
3.32144440415869));
#194709=CARTESIAN_POINT('Ctrl Pts',(-18.6611220247945,21.3301402961569,
3.313555838931));
#194710=CARTESIAN_POINT('Ctrl Pts',(-18.7905135122365,21.3272669435106,
3.30556200239142));
#194711=CARTESIAN_POINT('Ctrl Pts',(-18.8000257874368,21.326991530329,3.3049774456643));
#194712=CARTESIAN_POINT('Ctrl Pts',(-18.814117734892,21.3264883991271,3.30411639140283));
#194713=CARTESIAN_POINT('Ctrl Pts',(-18.8186988924786,21.3263099339841,
3.30383724430556));
#194714=CARTESIAN_POINT('Ctrl Pts',(-18.826848459626,21.3259659391652,3.30334208047868));
#194715=CARTESIAN_POINT('Ctrl Pts',(-18.8304170587594,21.3258062586729,
3.30312574079422));
#194716=CARTESIAN_POINT('Ctrl Pts',(-18.8380882652773,21.325443544964,3.3026617431343));
#194717=CARTESIAN_POINT('Ctrl Pts',(-18.8421906789341,21.3252376047784,
3.3024142497511));
#194718=CARTESIAN_POINT('Ctrl Pts',(-18.8535122121464,21.3246362275369,
3.30173294931598));
#194719=CARTESIAN_POINT('Ctrl Pts',(-18.8607300236011,21.3242157428328,
3.30130052341879));
#194720=CARTESIAN_POINT('Ctrl Pts',(-18.9002465976868,21.3217104522226,
3.29894289595577));
#194721=CARTESIAN_POINT('Ctrl Pts',(-18.932498340221,21.3189220126568,3.29705473484988));
#194722=CARTESIAN_POINT('Ctrl Pts',(-19.1265309786929,21.2976529281723,
3.28584523796555));
#194723=CARTESIAN_POINT('Ctrl Pts',(-19.2858160989885,21.2612955665585,
3.27723919543386));
#194724=CARTESIAN_POINT('Ctrl Pts',(-19.5495590289864,21.1680922258782,
3.26192580803239));
#194725=CARTESIAN_POINT('Ctrl Pts',(-19.6563184295678,21.1201018730927,
3.2554019306277));
#194726=CARTESIAN_POINT('Ctrl Pts',(-19.7721865477171,21.0560203156677,
3.24764514155896));
#194727=CARTESIAN_POINT('Ctrl Pts',(-19.7857235678568,21.0483374188237,
3.24672812929792));
#194728=CARTESIAN_POINT('Ctrl Pts',(-19.8061729231246,21.0364314026384,
3.24532584619987));
#194729=CARTESIAN_POINT('Ctrl Pts',(-19.8131479585771,21.0323166291268,
3.24484449444167));
#194730=CARTESIAN_POINT('Ctrl Pts',(-19.8254396220627,21.0249700275085,
3.24399075270369));
#194731=CARTESIAN_POINT('Ctrl Pts',(-19.8307659624935,21.0217545751831,
3.24361896378203));
#194732=CARTESIAN_POINT('Ctrl Pts',(-19.8420026163977,21.0149033655167,
3.24283068947592));
#194733=CARTESIAN_POINT('Ctrl Pts',(-19.8479093728519,21.0112619413171,
3.24241399870618));
#194734=CARTESIAN_POINT('Ctrl Pts',(-19.8599605117035,21.0037505836147,
3.2415590477976));
#194735=CARTESIAN_POINT('Ctrl Pts',(-19.866103093518,20.9998779479206,3.24112069126428));
#194736=CARTESIAN_POINT('Ctrl Pts',(-19.8812445575404,20.9902226794257,
3.24003368758007));
#194737=CARTESIAN_POINT('Ctrl Pts',(-19.8902196935948,20.9844033470528,
3.23938368072231));
#194738=CARTESIAN_POINT('Ctrl Pts',(-19.9967259000512,20.9141942478109,
3.23160138067261));
#194739=CARTESIAN_POINT('Ctrl Pts',(-20.0887916533393,20.841913572239,3.22416485619098));
#194740=CARTESIAN_POINT('Ctrl Pts',(-20.3104130479253,20.6361493847985,
3.20441973838464));
#194741=CARTESIAN_POINT('Ctrl Pts',(-20.4292177876253,20.4925488607579,
3.19185582995532));
#194742=CARTESIAN_POINT('Ctrl Pts',(-20.5353383515891,20.3232372822493,
3.17941620880226));
#194743=CARTESIAN_POINT('Ctrl Pts',(-20.5427765658817,20.3110995358283,
3.17853674385243));
#194744=CARTESIAN_POINT('Ctrl Pts',(-20.5529509485145,20.294114674696,3.1773240990047));
#194745=CARTESIAN_POINT('Ctrl Pts',(-20.5557911003333,20.289330719214,3.17698451330051));
#194746=CARTESIAN_POINT('Ctrl Pts',(-20.5603198446551,20.2816335330842,
3.17644135553094));
#194747=CARTESIAN_POINT('Ctrl Pts',(-20.5620203804379,20.2787274119442,
3.17623701625981));
#194748=CARTESIAN_POINT('Ctrl Pts',(-20.565558136712,20.2726483572403,3.17581112739224));
#194749=CARTESIAN_POINT('Ctrl Pts',(-20.5673940540597,20.2694746975455,
3.1755896669461));
#194750=CARTESIAN_POINT('Ctrl Pts',(-20.5718153760083,20.2617857609393,
3.17505521769718));
#194751=CARTESIAN_POINT('Ctrl Pts',(-20.574392419023,20.2572656531684,3.17474276745335));
#194752=CARTESIAN_POINT('Ctrl Pts',(-20.583349174217,20.2414201063898,3.17365335283475));
#194753=CARTESIAN_POINT('Ctrl Pts',(-20.5896413683298,20.2300451878635,
3.17288180901761));
#194754=CARTESIAN_POINT('Ctrl Pts',(-20.626171071982,20.1625469869171,3.1683609097762));
#194755=CARTESIAN_POINT('Ctrl Pts',(-20.6539686038732,20.1051337403328,
3.16474776973187));
#194756=CARTESIAN_POINT('Ctrl Pts',(-20.6946425036429,20.0104459608017,
3.15901977670304));
#194757=CARTESIAN_POINT('Ctrl Pts',(-20.7091282699385,19.973951900444,3.15686533709011));
#194758=CARTESIAN_POINT('Ctrl Pts',(-20.7225806782367,19.9371101060747,
3.15472451729435));
#194759=CARTESIAN_POINT('Ctrl Pts',(-20.722580576248,19.9371103853886,2.93545682861291));
#194760=CARTESIAN_POINT('Ctrl Pts',(-20.674294176734,20.0693511549778,2.94352078684689));
#194761=CARTESIAN_POINT('Ctrl Pts',(-20.6129098886537,20.1965203883229,
2.95104140375662));
#194762=CARTESIAN_POINT('Ctrl Pts',(-20.4906188222878,20.3961859327918,
2.96379346074783));
#194763=CARTESIAN_POINT('Ctrl Pts',(-20.436747863976,20.4723576225925,2.96891787851721));
#194764=CARTESIAN_POINT('Ctrl Pts',(-20.3470885818636,20.5828773470361,
2.97700806590996));
#194765=CARTESIAN_POINT('Ctrl Pts',(-20.3148231570149,20.6199357057277,
2.97984502488194));
#194766=CARTESIAN_POINT('Ctrl Pts',(-20.2731171368074,20.6645993893865,
2.98344130758929));
#194767=CARTESIAN_POINT('Ctrl Pts',(-20.2648603003467,20.6732925417145,
2.98414999872162));
#194768=CARTESIAN_POINT('Ctrl Pts',(-20.2514581381414,20.6871649933568,
2.98529531847376));
#194769=CARTESIAN_POINT('Ctrl Pts',(-20.2463590115715,20.6923887088454,
2.98572993655263));
#194770=CARTESIAN_POINT('Ctrl Pts',(-20.23676208271,20.7021189289957,2.98654584958489));
#194771=CARTESIAN_POINT('Ctrl Pts',(-20.2322707588035,20.7066317292645,
2.98692685684658));
#194772=CARTESIAN_POINT('Ctrl Pts',(-20.2221914699005,20.7166682520657,
2.98778008146402));
#194773=CARTESIAN_POINT('Ctrl Pts',(-20.216592993948,20.7221812426254,2.98825276457139));
#194774=CARTESIAN_POINT('Ctrl Pts',(-20.2023627094792,20.7360390473774,
2.98945120931347));
#194775=CARTESIAN_POINT('Ctrl Pts',(-20.1936904475494,20.7443417527191,
2.99017878883542));
#194776=CARTESIAN_POINT('Ctrl Pts',(-20.1444074798519,20.7907275974345,
2.99429845813934));
#194777=CARTESIAN_POINT('Ctrl Pts',(-20.1023806877526,20.8272679005677,
2.99775552007251));
#194778=CARTESIAN_POINT('Ctrl Pts',(-20.0362234156259,20.8803571973296,
3.00311869446364));
#194779=CARTESIAN_POINT('Ctrl Pts',(-20.0131072879826,20.8981347627081,
3.00497872929123));
#194780=CARTESIAN_POINT('Ctrl Pts',(-19.8632098503749,21.0085624056929,
3.01694731135086));
#194781=CARTESIAN_POINT('Ctrl Pts',(-19.7268213345117,21.087337798399,3.02747187506542));
#194782=CARTESIAN_POINT('Ctrl Pts',(-19.5380931236786,21.1699605503791,
3.04091643176587));
#194783=CARTESIAN_POINT('Ctrl Pts',(-19.4925132432654,21.1880560144762,
3.04408012381068));
#194784=CARTESIAN_POINT('Ctrl Pts',(-19.4216037413538,21.21339364062,3.04883525114068));
#194785=CARTESIAN_POINT('Ctrl Pts',(-19.396700328173,21.2217728909936,3.05047441617128));
#194786=CARTESIAN_POINT('Ctrl Pts',(-19.3651992312652,21.2317231971571,
3.05250371074648));
#194787=CARTESIAN_POINT('Ctrl Pts',(-19.3587425359735,21.2337287202385,
3.05291733842175));
#194788=CARTESIAN_POINT('Ctrl Pts',(-19.3484471159471,21.236872594996,3.05357308254486));
#194789=CARTESIAN_POINT('Ctrl Pts',(-19.3446146419496,21.238031028155,3.05381634801302));
#194790=CARTESIAN_POINT('Ctrl Pts',(-19.3373366954821,21.2402084025413,
3.05427669907735));
#194791=CARTESIAN_POINT('Ctrl Pts',(-19.3338919591473,21.2412294320012,
3.05449389977425));
#194792=CARTESIAN_POINT('Ctrl Pts',(-19.3259529986308,21.2435605922227,
3.05499291352776));
#194793=CARTESIAN_POINT('Ctrl Pts',(-19.3214570183267,21.2448645889602,
3.0552743670054));
#194794=CARTESIAN_POINT('Ctrl Pts',(-19.3093877749042,21.2483217462275,
3.05602693294367));
#194795=CARTESIAN_POINT('Ctrl Pts',(-19.3018066807179,21.2504476131665,
3.0564965020632));
#194796=CARTESIAN_POINT('Ctrl Pts',(-19.2447447455184,21.26610590057,3.06000852757599));
#194797=CARTESIAN_POINT('Ctrl Pts',(-19.1947942449952,21.2778792994095,
3.0629568649243));
#194798=CARTESIAN_POINT('Ctrl Pts',(-19.1224217189075,21.2921829039909,
3.06711287204316));
#194799=CARTESIAN_POINT('Ctrl Pts',(-19.1003137572517,21.296187759523,3.06836708465605));
#194800=CARTESIAN_POINT('Ctrl Pts',(-18.9306983870196,21.3241326484922,
3.0778999644202));
#194801=CARTESIAN_POINT('Ctrl Pts',(-18.7810920699222,21.3327457862096,
3.08582264540635));
#194802=CARTESIAN_POINT('Ctrl Pts',(-18.5729911334362,21.3226898906018,
3.09737307806423));
#194803=CARTESIAN_POINT('Ctrl Pts',(-18.5143091689989,21.3173934164892,
3.1006850253826));
#194804=CARTESIAN_POINT('Ctrl Pts',(-18.4202434092413,21.3049296775668,
3.10613622209162));
#194805=CARTESIAN_POINT('Ctrl Pts',(-18.3846876387832,21.2992924462735,
3.1082296202063));
#194806=CARTESIAN_POINT('Ctrl Pts',(-18.3384789537933,21.2907531269146,
3.11100018952998));
#194807=CARTESIAN_POINT('Ctrl Pts',(-18.327679482196,21.2886702329314,3.11165127876057));
#194808=CARTESIAN_POINT('Ctrl Pts',(-18.3100930298703,21.2851359749784,
3.11271757899035));
#194809=CARTESIAN_POINT('Ctrl Pts',(-18.3032960045519,21.283735204643,3.11313116986443));
#194810=CARTESIAN_POINT('Ctrl Pts',(-18.2902040403987,21.2809699595375,
3.11393069502366));
#194811=CARTESIAN_POINT('Ctrl Pts',(-18.2839081919858,21.2796101252007,
3.11431647658929));
#194812=CARTESIAN_POINT('Ctrl Pts',(-18.2694591468087,21.2764202039866,
3.11520486932457));
#194813=CARTESIAN_POINT('Ctrl Pts',(-18.261310422863,21.2745705424964,3.11570810438923));
#194814=CARTESIAN_POINT('Ctrl Pts',(-18.2395866276593,21.2695040795906,
3.11705570048035));
#194815=CARTESIAN_POINT('Ctrl Pts',(-18.2260322191464,21.2662012912196,
3.11790281510485));
#194816=CARTESIAN_POINT('Ctrl Pts',(-18.1175031400767,21.238616918699,3.12473726981985));
#194817=CARTESIAN_POINT('Ctrl Pts',(-18.0243000911508,21.2079026180012,
3.13093375870797));
#194818=CARTESIAN_POINT('Ctrl Pts',(-17.8056468900667,21.1186014984214,
3.14624081667651));
#194819=CARTESIAN_POINT('Ctrl Pts',(-17.6831482769317,21.0539568216178,
3.15548273967279));
#194820=CARTESIAN_POINT('Ctrl Pts',(-17.5257609959178,20.9500769915515,
3.16779961637272));
#194821=CARTESIAN_POINT('Ctrl Pts',(-17.484690354188,20.9208117909914,3.17105608982906));
#194822=CARTESIAN_POINT('Ctrl Pts',(-17.4234655035585,20.87380040142,3.17593322307956));
#194823=CARTESIAN_POINT('Ctrl Pts',(-17.4025397620007,20.8570922304318,
3.17760435836788));
#194824=CARTESIAN_POINT('Ctrl Pts',(-17.3767001964428,20.8356453563956,
3.17966734726269));
#194825=CARTESIAN_POINT('Ctrl Pts',(-17.3714857501643,20.831274733709,3.18008362940935));
#194826=CARTESIAN_POINT('Ctrl Pts',(-17.3632291431778,20.8242862002877,
3.18074259907813));
#194827=CARTESIAN_POINT('Ctrl Pts',(-17.3601732515484,20.8216846903756,
3.18098645482183));
#194828=CARTESIAN_POINT('Ctrl Pts',(-17.3543974108886,20.8167392651717,
3.18144725404704));
#194829=CARTESIAN_POINT('Ctrl Pts',(-17.351676061376,20.8143971499484,3.18166431634587));
#194830=CARTESIAN_POINT('Ctrl Pts',(-17.3454335868465,20.8089968917271,
3.18216214558974));
#194831=CARTESIAN_POINT('Ctrl Pts',(-17.3419166016,20.8059340307859,3.18244255872497));
#194832=CARTESIAN_POINT('Ctrl Pts',(-17.3325346538488,20.797708835855,3.18319051609213));
#194833=CARTESIAN_POINT('Ctrl Pts',(-17.3266880368958,20.7925255574938,
3.18365654647553));
#194834=CARTESIAN_POINT('Ctrl Pts',(-17.2837642380047,20.7540452434154,
3.18707855710478));
#194835=CARTESIAN_POINT('Ctrl Pts',(-17.2478412208922,20.7194778153257,
3.18994575535038));
#194836=CARTESIAN_POINT('Ctrl Pts',(-17.1654590508402,20.634401587934,3.19662582273113));
#194837=CARTESIAN_POINT('Ctrl Pts',(-17.1201687782878,20.5828391432208,
3.20038544235283));
#194838=CARTESIAN_POINT('Ctrl Pts',(-17.0090836959537,20.443238452875,3.21010125503683));
#194839=CARTESIAN_POINT('Ctrl Pts',(-16.9474996018098,20.3521237263023,
3.21601186210985));
#194840=CARTESIAN_POINT('Ctrl Pts',(-16.8555144959244,20.1901944028768,
3.22636238890177));
#194841=CARTESIAN_POINT('Ctrl Pts',(-16.8213964512187,20.1217553714144,
3.23069281713936));
#194842=CARTESIAN_POINT('Ctrl Pts',(-16.7835125838982,20.0341941506857,
3.23626232229619));
#194843=CARTESIAN_POINT('Ctrl Pts',(-16.7762055319999,20.0166615644226,
3.23737875004261));
#194844=CARTESIAN_POINT('Ctrl Pts',(-16.7659385590013,19.9910621302361,
3.23901160114075));
#194845=CARTESIAN_POINT('Ctrl Pts',(-16.7627901397617,19.9830715291721,
3.23952166181124));
#194846=CARTESIAN_POINT('Ctrl Pts',(-16.7573608850013,19.9690425258735,
3.24041792940939));
#194847=CARTESIAN_POINT('Ctrl Pts',(-16.7550588668143,19.9630124014517,
3.24080341896293));
#194848=CARTESIAN_POINT('Ctrl Pts',(-16.75064636719,19.951293310164,3.24155310059979));
#194849=CARTESIAN_POINT('Ctrl Pts',(-16.7485326947236,19.9456056059824,
3.24191718127886));
#194850=CARTESIAN_POINT('Ctrl Pts',(-16.7435444058367,19.9320037616824,
3.24278845134586));
#194851=CARTESIAN_POINT('Ctrl Pts',(-16.7406925124986,19.9240814495994,
3.24329639292468));
#194852=CARTESIAN_POINT('Ctrl Pts',(-16.7306063846141,19.8955297126004,
3.24512882906657));
#194853=CARTESIAN_POINT('Ctrl Pts',(-16.7236447255072,19.8748060858997,
3.24646230673773));
#194854=CARTESIAN_POINT('Ctrl Pts',(-16.6599021177827,19.6748485423855,
3.25936579453176));
#194855=CARTESIAN_POINT('Ctrl Pts',(-16.6269267470173,19.4889408487993,
3.27175923197078));
#194856=CARTESIAN_POINT('Ctrl Pts',(-16.6155745605528,19.2226745827203,
3.28935021725087));
#194857=CARTESIAN_POINT('Ctrl Pts',(-16.6166004195378,19.1440423965755,
3.29450882005877));
#194858=CARTESIAN_POINT('Ctrl Pts',(-16.6244404954491,19.0301265169542,
3.30178495156751));
#194859=CARTESIAN_POINT('Ctrl Pts',(-16.6277807474953,18.9946731015927,
3.30402109499804));
#194860=CARTESIAN_POINT('Ctrl Pts',(-16.632898464929,18.9519310986414,3.30666931684317));
#194861=CARTESIAN_POINT('Ctrl Pts',(-16.6338219515318,18.9445482692111,
3.3071250166315));
#194862=CARTESIAN_POINT('Ctrl Pts',(-16.6353216182513,18.9330516190588,
3.30783178271872));
#194863=CARTESIAN_POINT('Ctrl Pts',(-16.6358710052018,18.9289344502446,
3.30808431743661));
#194864=CARTESIAN_POINT('Ctrl Pts',(-16.6369146307297,18.921285185992,3.308552403415));
#194865=CARTESIAN_POINT('Ctrl Pts',(-16.6374056725163,18.9177527567096,
3.30876812636692));
#194866=CARTESIAN_POINT('Ctrl Pts',(-16.6385390401514,18.9097479803668,
3.30925599056532));
#194867=CARTESIAN_POINT('Ctrl Pts',(-16.6391867564605,18.9052764498054,
3.30952782390702));
#194868=CARTESIAN_POINT('Ctrl Pts',(-16.6408980490523,18.8937233031635,
3.31022845412401));
#194869=CARTESIAN_POINT('Ctrl Pts',(-16.6419832600324,18.8866448822526,
3.3106560572816));
#194870=CARTESIAN_POINT('Ctrl Pts',(-16.6489123648876,18.8429309095058,
3.31328727076249));
#194871=CARTESIAN_POINT('Ctrl Pts',(-16.6556828986259,18.8064462910856,
3.3154419838569));
#194872=CARTESIAN_POINT('Ctrl Pts',(-16.6988858517993,18.6035272364578,
3.32728797625059));
#194873=CARTESIAN_POINT('Ctrl Pts',(-16.754348967805,18.4417754020813,3.3362519566324));
#194874=CARTESIAN_POINT('Ctrl Pts',(-16.8700557848137,18.202810555408,3.35085875138092));
#194875=CARTESIAN_POINT('Ctrl Pts',(-16.9172191154571,18.120111298474,3.35619207864221));
#194876=CARTESIAN_POINT('Ctrl Pts',(-16.9815825874255,18.0230697251581,
3.36297297135718));
#194877=CARTESIAN_POINT('Ctrl Pts',(-16.9936556466916,18.005451739431,3.36422617644362));
#194878=CARTESIAN_POINT('Ctrl Pts',(-17.0111944269801,17.9806703574607,
3.36602208509113));
#194879=CARTESIAN_POINT('Ctrl Pts',(-17.0164427559218,17.9733541777877,
3.36655647648905));
#194880=CARTESIAN_POINT('Ctrl Pts',(-17.0255748574342,17.9607939719363,
3.36748126313192));
#194881=CARTESIAN_POINT('Ctrl Pts',(-17.0294365262826,17.9555339737945,
3.3678707991702));
#194882=CARTESIAN_POINT('Ctrl Pts',(-17.0368752960774,17.9454991769957,
3.36861830277713));
#194883=CARTESIAN_POINT('Ctrl Pts',(-17.0404483887357,17.9407214744236,
3.36897611140026));
#194884=CARTESIAN_POINT('Ctrl Pts',(-17.0497884292747,17.9283420453147,
3.36990824636289));
#194885=CARTESIAN_POINT('Ctrl Pts',(-17.0555866127161,17.9207641531851,
3.3704837985326));
#194886=CARTESIAN_POINT('Ctrl Pts',(-17.0755132229462,17.8950828473311,
3.37245148539138));
#194887=CARTESIAN_POINT('Ctrl Pts',(-17.0898845081516,17.8771707280767,
3.37385324225886));
#194888=CARTESIAN_POINT('Ctrl Pts',(-17.2168421286309,17.7241027822618,
3.38609352168608));
#194889=CARTESIAN_POINT('Ctrl Pts',(-17.3455575527169,17.6032576965896,
3.39763949798531));
#194890=CARTESIAN_POINT('Ctrl Pts',(-17.5577942539594,17.4486863111455,
3.41498664519782));
#194891=CARTESIAN_POINT('Ctrl Pts',(-17.6309697273569,17.4019849027498,
3.42070133631461));
#194892=CARTESIAN_POINT('Ctrl Pts',(-17.7398154831848,17.3415853470848,
3.42864839395857));
#194893=CARTESIAN_POINT('Ctrl Pts',(-17.7733096664698,17.324153824787,3.43102279981182));
#194894=CARTESIAN_POINT('Ctrl Pts',(-17.8140582895227,17.304313471832,3.43381170260923));
#194895=CARTESIAN_POINT('Ctrl Pts',(-17.820880005455,17.3010371346785,3.43427529405046));
#194896=CARTESIAN_POINT('Ctrl Pts',(-17.8314980692211,17.2960073763876,
3.43499160117533));
#194897=CARTESIAN_POINT('Ctrl Pts',(-17.8352822107371,17.2942285427026,
3.43524584879597));
#194898=CARTESIAN_POINT('Ctrl Pts',(-17.8423013457109,17.2909543727722,
3.43571549900468));
#194899=CARTESIAN_POINT('Ctrl Pts',(-17.8455348165529,17.2894560065411,
3.43593108340598));
#194900=CARTESIAN_POINT('Ctrl Pts',(-17.8528426877208,17.2860919836153,
3.43641660178693));
#194901=CARTESIAN_POINT('Ctrl Pts',(-17.8569192255296,17.2842310993717,
3.43668624035576));
#194902=CARTESIAN_POINT('Ctrl Pts',(-17.8689371416884,17.2787911279314,
3.43747772186595));
#194903=CARTESIAN_POINT('Ctrl Pts',(-17.8768948473473,17.2752480434398,
3.43799740599801));
#194904=CARTESIAN_POINT('Ctrl Pts',(-17.9335931305573,17.250421915488,3.44167052638591));
#194905=CARTESIAN_POINT('Ctrl Pts',(-17.9831029613884,17.2309312560237,
3.44472319528746));
#194906=CARTESIAN_POINT('Ctrl Pts',(-18.0354590603296,17.2125669144527,
3.44784390083105));
#194907=CARTESIAN_POINT('Ctrl Pts',(-18.0376207455991,17.2118126211102,
3.44797256035732));
#194908=CARTESIAN_POINT('Ctrl Pts',(-18.1790518309796,17.1627192178655,
3.45637820594238));
#194909=CARTESIAN_POINT('Ctrl Pts',(-18.3229953469071,17.1290532342067,
3.46419526710065));
#194910=CARTESIAN_POINT('Ctrl Pts',(-18.5662418109367,17.0983955015415,
3.4776670819938));
#194911=CARTESIAN_POINT('Ctrl Pts',(-18.6639259919915,17.0929048740995,
3.48313974083939));
#194912=CARTESIAN_POINT('Ctrl Pts',(-18.7832996905922,17.0944631927324,
3.49008947755054));
#194913=CARTESIAN_POINT('Ctrl Pts',(-18.8049599212159,17.0950786511952,
3.49136067086335));
#194914=CARTESIAN_POINT('Ctrl Pts',(-18.8356539834407,17.0964226226306,
3.49317790883942));
#194915=CARTESIAN_POINT('Ctrl Pts',(-18.8446989064189,17.0968768329473,
3.49371536572356));
#194916=CARTESIAN_POINT('Ctrl Pts',(-18.8602650117813,17.0977586857453,
3.49464378679632));
#194917=CARTESIAN_POINT('Ctrl Pts',(-18.8667876888746,17.0981585166701,
3.49503387357448));
#194918=CARTESIAN_POINT('Ctrl Pts',(-18.8792508340747,17.0989804305249,
3.49578127495249));
#194919=CARTESIAN_POINT('Ctrl Pts',(-18.8851915859044,17.0993973930044,
3.4961384250107));
#194920=CARTESIAN_POINT('Ctrl Pts',(-18.9005869113662,17.1005432435248,
3.49706631496793));
#194921=CARTESIAN_POINT('Ctrl Pts',(-18.9100384115632,17.1013105932226,
3.49763825862536));
#194922=CARTESIAN_POINT('Ctrl Pts',(-18.9420029627241,17.1041220301849,
3.49958048033892));
#194923=CARTESIAN_POINT('Ctrl Pts',(-18.9644877178414,17.1064631478775,
3.50096004589867));
#194924=CARTESIAN_POINT('Ctrl Pts',(-19.1659634924792,17.1307082673477,
3.51344597501258));
#194925=CARTESIAN_POINT('Ctrl Pts',(-19.3414786543945,17.1750357395059,
3.52530078801102));
#194926=CARTESIAN_POINT('Ctrl Pts',(-19.5870768084979,17.2716829728511,
3.5427338722436));
#194927=CARTESIAN_POINT('Ctrl Pts',(-19.6630604514825,17.3069151606001,
3.54824049257048));
#194928=CARTESIAN_POINT('Ctrl Pts',(-19.7693186012447,17.3640644743566,
3.55593788520325));
#194929=CARTESIAN_POINT('Ctrl Pts',(-19.8014122712448,17.3824249072294,
3.55826177967616));
#194930=CARTESIAN_POINT('Ctrl Pts',(-19.839439811248,17.4055226655027,3.5609993889357));
#194931=CARTESIAN_POINT('Ctrl Pts',(-19.845848123005,17.4094619524007,3.56146016395888));
#194932=CARTESIAN_POINT('Ctrl Pts',(-19.8557774347931,17.4156388140984,
3.56217306723734));
#194933=CARTESIAN_POINT('Ctrl Pts',(-19.859312973088,17.4178527348972,3.56242670462952));
#194934=CARTESIAN_POINT('Ctrl Pts',(-19.865857594475,17.421977894845,3.56289579358229));
#194935=CARTESIAN_POINT('Ctrl Pts',(-19.868868366988,17.4238862664055,3.56311142335979));
#194936=CARTESIAN_POINT('Ctrl Pts',(-19.8756640864316,17.4282178174308,
3.56359775932483));
#194937=CARTESIAN_POINT('Ctrl Pts',(-19.8794461357558,17.4306454432692,
3.56386816572663));
#194938=CARTESIAN_POINT('Ctrl Pts',(-19.8905863985753,17.4378463605746,
3.56466399626279));
#194939=CARTESIAN_POINT('Ctrl Pts',(-19.8979228154563,17.4426534242246,
3.56518722594247));
#194940=CARTESIAN_POINT('Ctrl Pts',(-19.9507592063296,17.4777448562216,
3.56895083887473));
#194941=CARTESIAN_POINT('Ctrl Pts',(-19.9951052480139,17.5097384087307,
3.5720847371227));
#194942=CARTESIAN_POINT('Ctrl Pts',(-20.1707478296543,17.6471031020045,
3.58461106230112));
#194943=CARTESIAN_POINT('Ctrl Pts',(-20.290496176468,17.7662353072659,3.59346952949677));
#194944=CARTESIAN_POINT('Ctrl Pts',(-20.4314204297724,17.944537890231,3.60606884571564));
#194945=CARTESIAN_POINT('Ctrl Pts',(-20.4660158001134,17.9922781716356,
3.6093827767193));
#194946=CARTESIAN_POINT('Ctrl Pts',(-20.5184688775535,18.0714138109634,
3.61483694415326));
#194947=CARTESIAN_POINT('Ctrl Pts',(-20.5375946862398,18.1019319954593,
3.61693126388929));
#194948=CARTESIAN_POINT('Ctrl Pts',(-20.5615339449738,18.1423888986536,
3.61970288369652));
#194949=CARTESIAN_POINT('Ctrl Pts',(-20.5670618559126,18.1518993289392,
3.62035407668547));
#194950=CARTESIAN_POINT('Ctrl Pts',(-20.5759561082204,18.1674795819698,
3.62142050424096));
#194951=CARTESIAN_POINT('Ctrl Pts',(-20.579367206134,18.1735237158283,3.62183411793738));
#194952=CARTESIAN_POINT('Ctrl Pts',(-20.5858865435777,18.185209224511,3.62263365735505));
#194953=CARTESIAN_POINT('Ctrl Pts',(-20.5889988830437,18.1908482329343,
3.62301943019648));
#194954=CARTESIAN_POINT('Ctrl Pts',(-20.5960893269204,18.2038345979843,
3.62390776015328));
#194955=CARTESIAN_POINT('Ctrl Pts',(-20.6000497457547,18.2111914424794,
3.62441094087385));
#194956=CARTESIAN_POINT('Ctrl Pts',(-20.6105050970159,18.2308917588406,
3.62575829686116));
#194957=CARTESIAN_POINT('Ctrl Pts',(-20.6169216820362,18.2432761405141,
3.62660522418123));
#194958=CARTESIAN_POINT('Ctrl Pts',(-20.6678619786731,18.3440188229043,
3.63349516759902));
#194959=CARTESIAN_POINT('Ctrl Pts',(-20.7062574655786,18.4353234214685,
3.63975142507013));
#194960=CARTESIAN_POINT('Ctrl Pts',(-20.7819939206222,18.6578717871092,
3.65499311512505));
#194961=CARTESIAN_POINT('Ctrl Pts',(-20.8133219835055,18.7907067361352,
3.66409682105377));
#194962=CARTESIAN_POINT('Ctrl Pts',(-20.8417530853864,18.9996855456632,
3.67787835293917));
#194963=CARTESIAN_POINT('Ctrl Pts',(-20.8479010431315,19.0742457273808,
3.68268516259665));
#194964=CARTESIAN_POINT('Ctrl Pts',(-20.8503509135253,19.1578371651599,
3.68784422392104));
#194965=CARTESIAN_POINT('Ctrl Pts',(-20.850554851592,19.1666937623867,3.68838793079842));
#194966=CARTESIAN_POINT('Ctrl Pts',(-20.8507777607909,19.1800041518406,
3.68920043427108));
#194967=CARTESIAN_POINT('Ctrl Pts',(-20.8508382796655,19.1844570204453,
3.68947147272052));
#194968=CARTESIAN_POINT('Ctrl Pts',(-20.8509183443664,19.1921296534542,
3.68993711501611));
#194969=CARTESIAN_POINT('Ctrl Pts',(-20.8509445959975,19.1953492924698,
3.6901320912159));
#194970=CARTESIAN_POINT('Ctrl Pts',(-20.850987402342,19.2026391165335,3.69057259526842));
#194971=CARTESIAN_POINT('Ctrl Pts',(-20.8509995645895,19.2067092871484,
3.69081787437903));
#194972=CARTESIAN_POINT('Ctrl Pts',(-20.8510007238771,19.2178398475239,
3.69148685974545));
#194973=CARTESIAN_POINT('Ctrl Pts',(-20.8509661391612,19.2249002609865,
3.6919092662087));
#194974=CARTESIAN_POINT('Ctrl Pts',(-20.8505991940585,19.2619597474054,
3.69411682418592));
#194975=CARTESIAN_POINT('Ctrl Pts',(-20.8496644767133,19.2919510627868,
3.69587027679547));
#194976=CARTESIAN_POINT('Ctrl Pts',(-20.8449576393496,19.3816663716478,
3.70104321441789));
#194977=CARTESIAN_POINT('Ctrl Pts',(-20.8392907084485,19.4412633856781,
3.7043837998999));
#194978=CARTESIAN_POINT('Ctrl Pts',(-20.8105321382441,19.6495555519041,
3.71596096917035));
#194979=CARTESIAN_POINT('Ctrl Pts',(-20.7741427280388,19.7958983757255,
3.72394896228244));
#194980=CARTESIAN_POINT('Ctrl Pts',(-20.7225806064494,19.9371103026766,
3.73234504707874));
#194981=CARTESIAN_POINT('Origin',(-18.734,19.211,0.));
#194982=CARTESIAN_POINT('',(-20.7225806084094,19.937110297309,4.75730094873459));
#194983=CARTESIAN_POINT('',(-20.7225805792317,19.9371103772171,4.53222349041431));
#194984=CARTESIAN_POINT('',(-20.7225806064498,19.9371103026755,0.));
#194985=CARTESIAN_POINT('',(-20.8509999221905,19.2104260266189,4.70909172043352));
#194986=CARTESIAN_POINT('Ctrl Pts',(-20.7225806084094,19.937110297309,4.75730094873459));
#194987=CARTESIAN_POINT('Ctrl Pts',(-20.7382263485064,19.8942616894923,
4.75443866810734));
#194988=CARTESIAN_POINT('Ctrl Pts',(-20.7524832949378,19.8509180613671,
4.75153426385756));
#194989=CARTESIAN_POINT('Ctrl Pts',(-20.8222129884855,19.6133189441214,
4.73557997940159));
#194990=CARTESIAN_POINT('Ctrl Pts',(-20.8510546775763,19.4123816420812,
4.72184240933827));
#194991=CARTESIAN_POINT('Ctrl Pts',(-20.8509999221905,19.2104260266189,
4.70909172043352));
#194992=CARTESIAN_POINT('Ctrl Pts',(-20.8509999215531,19.2104236806784,
4.70909157232004));
#194993=CARTESIAN_POINT('Ctrl Pts',(-20.8509956361906,19.1946822127091,
4.70809771821267));
#194994=CARTESIAN_POINT('Ctrl Pts',(-20.8508157764336,19.1789407168608,
4.70711098890863));
#194995=CARTESIAN_POINT('Ctrl Pts',(-20.8502148552955,19.1523322896803,
4.70545674230044));
#194996=CARTESIAN_POINT('Ctrl Pts',(-20.849885630565,19.1414642283405,4.704784929544));
#194997=CARTESIAN_POINT('Ctrl Pts',(-20.8492914997428,19.1258317551766,
4.70382461278879));
#194998=CARTESIAN_POINT('Ctrl Pts',(-20.8490942018603,19.1210651509873,
4.7035326004156));
#194999=CARTESIAN_POINT('Ctrl Pts',(-20.8487208813721,19.112728068835,4.70302330825673));
#195000=CARTESIAN_POINT('Ctrl Pts',(-20.8485519257395,19.1091573156752,
4.70280564676389));
#195001=CARTESIAN_POINT('Ctrl Pts',(-20.8482044716945,19.1021880840255,
4.70238175978817));
#195002=CARTESIAN_POINT('Ctrl Pts',(-20.8480268211227,19.0987895664123,
4.70217548757971));
#195003=CARTESIAN_POINT('Ctrl Pts',(-20.8476550551931,19.0919920245619,
4.70176379849832));
#195004=CARTESIAN_POINT('Ctrl Pts',(-20.8474609357335,19.0885930391345,
4.70155838161796));
#195005=CARTESIAN_POINT('Ctrl Pts',(-20.8469736811945,19.0804082226764,
4.70106476398547));
#195006=CARTESIAN_POINT('Ctrl Pts',(-20.8466724833825,19.0756228649065,
4.70077701234596));
#195007=CARTESIAN_POINT('Ctrl Pts',(-20.8455076186839,19.0580673441033,
4.69972434795524));
#195008=CARTESIAN_POINT('Ctrl Pts',(-20.8445443839743,19.0453037649106,
4.69896480349769));
#195009=CARTESIAN_POINT('Ctrl Pts',(-20.8412948240264,19.0068907097402,
4.69669422891624));
#195010=CARTESIAN_POINT('Ctrl Pts',(-20.8386561526834,18.9812725967026,
4.69520057613638));
#195011=CARTESIAN_POINT('Ctrl Pts',(-20.8271568183861,18.8866107253501,
4.68973698366177));
#195012=CARTESIAN_POINT('Ctrl Pts',(-20.815359701632,18.8179642595826,4.68588409709238));
#195013=CARTESIAN_POINT('Ctrl Pts',(-20.7628523866104,18.5826167235474,
4.67268986147537));
#195014=CARTESIAN_POINT('Ctrl Pts',(-20.7053025210351,18.420385130281,4.6635643276233));
#195015=CARTESIAN_POINT('Ctrl Pts',(-20.6094430852125,18.2280002287463,
4.65129081970063));
#195016=CARTESIAN_POINT('Ctrl Pts',(-20.5888830986371,18.1897343057494,
4.64877505454473));
#195017=CARTESIAN_POINT('Ctrl Pts',(-20.5612889500311,18.1419621330024,
4.64552585314126));
#195018=CARTESIAN_POINT('Ctrl Pts',(-20.5553316401202,18.1318438869678,
4.64483133656453));
#195019=CARTESIAN_POINT('Ctrl Pts',(-20.545635240889,18.1156839603565,4.64371168324615));
#195020=CARTESIAN_POINT('Ctrl Pts',(-20.5419493182459,18.1096105441325,
4.64328848994679));
#195021=CARTESIAN_POINT('Ctrl Pts',(-20.5348872058423,18.0981050467459,
4.64248217973361));
#195022=CARTESIAN_POINT('Ctrl Pts',(-20.5315168278889,18.0926694776544,
4.64209927979589));
#195023=CARTESIAN_POINT('Ctrl Pts',(-20.5237892059008,18.0803319583397,
4.64122563817267));
#195024=CARTESIAN_POINT('Ctrl Pts',(-20.5194165919564,18.0734397984084,
4.64073433061718));
#195025=CARTESIAN_POINT('Ctrl Pts',(-20.5079762063604,18.055635798028,4.63945659847115));
#195026=CARTESIAN_POINT('Ctrl Pts',(-20.5008476596439,18.0447635935634,
4.63866791487524));
#195027=CARTESIAN_POINT('Ctrl Pts',(-20.4535528492585,17.9740601968294,
4.63348284501959));
#195028=CARTESIAN_POINT('Ctrl Pts',(-20.4104582071831,17.9162536842956,
4.62897579343002));
#195029=CARTESIAN_POINT('Ctrl Pts',(-20.2374623580639,17.7073494951758,
4.61164117641781));
#195030=CARTESIAN_POINT('Ctrl Pts',(-20.0894289020334,17.5726593379008,
4.59813842911275));
#195031=CARTESIAN_POINT('Ctrl Pts',(-19.9014491080653,17.4447759395971,
4.58356919259272));
#195032=CARTESIAN_POINT('Ctrl Pts',(-19.8778080894437,17.4293748818869,
4.58178006681209));
#195033=CARTESIAN_POINT('Ctrl Pts',(-19.8437610561343,17.4081519307837,
4.57927156501528));
#195034=CARTESIAN_POINT('Ctrl Pts',(-19.8336037186753,17.4019387964087,
4.5785316279267));
#195035=CARTESIAN_POINT('Ctrl Pts',(-19.8178770363495,17.3925003509142,
4.57739954164229));
#195036=CARTESIAN_POINT('Ctrl Pts',(-19.8123446702371,17.3892142886145,
4.57700385241569));
#195037=CARTESIAN_POINT('Ctrl Pts',(-19.8031433772348,17.383805592284,4.57635009554928));
#195038=CARTESIAN_POINT('Ctrl Pts',(-19.7994829476587,17.3816686867517,
4.57609115314194));
#195039=CARTESIAN_POINT('Ctrl Pts',(-19.7923782198309,17.37754960923,4.575590786715));
#195040=CARTESIAN_POINT('Ctrl Pts',(-19.7889347124578,17.375566115416,4.57534927944021));
#195041=CARTESIAN_POINT('Ctrl Pts',(-19.7824724983168,17.3718680111772,
4.57489797617566));
#195042=CARTESIAN_POINT('Ctrl Pts',(-19.7794551945294,17.3701511500241,
4.57468803970332));
#195043=CARTESIAN_POINT('Ctrl Pts',(-19.7724408688373,17.3661827714855,
4.57420179984742));
#195044=CARTESIAN_POINT('Ctrl Pts',(-19.7684407476192,17.3639368215274,
4.57392585599385));
#195045=CARTESIAN_POINT('Ctrl Pts',(-19.7561078677403,17.3570649041168,
4.57307912973231));
#195046=CARTESIAN_POINT('Ctrl Pts',(-19.7477510133827,17.3524821164191,
4.57251104198148));
#195047=CARTESIAN_POINT('Ctrl Pts',(-19.6351305199465,17.291708188119,4.56492711157822));
#195048=CARTESIAN_POINT('Ctrl Pts',(-19.5263450888224,17.2442985344387,
4.55841883662445));
#195049=CARTESIAN_POINT('Ctrl Pts',(-19.3106039756828,17.171104675059,4.54601545495623));
#195050=CARTESIAN_POINT('Ctrl Pts',(-19.2044919573254,17.144050190448,4.54012765391835));
#195051=CARTESIAN_POINT('Ctrl Pts',(-19.0424815618063,17.1158712547053,
4.53098398998122));
#195052=CARTESIAN_POINT('Ctrl Pts',(-18.9878490398172,17.1085525326042,
4.52787685894774));
#195053=CARTESIAN_POINT('Ctrl Pts',(-18.8988433881107,17.1001488801067,
4.5227334288636));
#195054=CARTESIAN_POINT('Ctrl Pts',(-18.8646190761696,17.0977550417999,
4.5207365058017));
#195055=CARTESIAN_POINT('Ctrl Pts',(-18.8195557280447,17.0957019023244,
4.51807607455091));
#195056=CARTESIAN_POINT('Ctrl Pts',(-18.8087549307922,17.0952926671215,
4.51743608981436));
#195057=CARTESIAN_POINT('Ctrl Pts',(-18.7910566771901,17.094757783409,4.51638340946749));
#195058=CARTESIAN_POINT('Ctrl Pts',(-18.7841608183004,17.0945831048043,
4.51597225498933));
#195059=CARTESIAN_POINT('Ctrl Pts',(-18.7708087734838,17.0943101773493,
4.51517418921256));
#195060=CARTESIAN_POINT('Ctrl Pts',(-18.7643527423884,17.094207756837,4.51478741325659));
#195061=CARTESIAN_POINT('Ctrl Pts',(-18.7494420108875,17.09403943587,4.51389201933557));
#195062=CARTESIAN_POINT('Ctrl Pts',(-18.7409872248408,17.0939946478029,
4.51338274517082));
#195063=CARTESIAN_POINT('Ctrl Pts',(-18.7182418348187,17.0940104149501,
4.51200837633005));
#195064=CARTESIAN_POINT('Ctrl Pts',(-18.7039519283694,17.0941650228108,
4.51114035318679));
#195065=CARTESIAN_POINT('Ctrl Pts',(-18.5727877356283,17.0969125175869,
4.50312970998661));
#195066=CARTESIAN_POINT('Ctrl Pts',(-18.4563334254439,17.1090369333371,
4.49568501739993));
#195067=CARTESIAN_POINT('Ctrl Pts',(-18.1814277000123,17.1609061046711,
4.47741112914737));
#195068=CARTESIAN_POINT('Ctrl Pts',(-18.0253895151496,17.2094774780682,
4.46644146029023));
#195069=CARTESIAN_POINT('Ctrl Pts',(-17.8469187509254,17.2885484035777,
4.45404010779418));
#195070=CARTESIAN_POINT('Ctrl Pts',(-17.8176749663243,17.3023140698814,
4.45201499635562));
#195071=CARTESIAN_POINT('Ctrl Pts',(-17.782289997379,17.3199713666781,4.44958327965227));
#195072=CARTESIAN_POINT('Ctrl Pts',(-17.775840377276,17.3232311153155,4.44914082387328));
#195073=CARTESIAN_POINT('Ctrl Pts',(-17.7657517733806,17.3283950926444,
4.44845009266478));
#195074=CARTESIAN_POINT('Ctrl Pts',(-17.7621014943149,17.33027695796,4.44820045284476));
#195075=CARTESIAN_POINT('Ctrl Pts',(-17.7552862699309,17.3338156201542,
4.44773492577405));
#195076=CARTESIAN_POINT('Ctrl Pts',(-17.7521200771149,17.3354697873334,
4.44751888414557));
#195077=CARTESIAN_POINT('Ctrl Pts',(-17.7448989481459,17.3392657405255,
4.44702667033214));
#195078=CARTESIAN_POINT('Ctrl Pts',(-17.7408467821932,17.3414126883889,
4.44675082879972));
#195079=CARTESIAN_POINT('Ctrl Pts',(-17.7284022734093,17.348058004763,4.44590472857384));
#195080=CARTESIAN_POINT('Ctrl Pts',(-17.7200331443874,17.352599911558,4.44533715876251));
#195081=CARTESIAN_POINT('Ctrl Pts',(-17.6079266222893,17.414422640176,4.43775007482204));
#195082=CARTESIAN_POINT('Ctrl Pts',(-17.509130518653,17.4802676844073,4.43123870275612));
#195083=CARTESIAN_POINT('Ctrl Pts',(-17.3307843951688,17.622092341876,4.41883304774966));
#195084=CARTESIAN_POINT('Ctrl Pts',(-17.2506152416133,17.6966650462839,
4.41294603043153));
#195085=CARTESIAN_POINT('Ctrl Pts',(-17.1392571530733,17.8176161842848,
4.40380418848833));
#195086=CARTESIAN_POINT('Ctrl Pts',(-17.1035454617429,17.8595783190234,
4.40069810176586));
#195087=CARTESIAN_POINT('Ctrl Pts',(-17.0483206513809,17.9298480467366,
4.39555624627508));
#195088=CARTESIAN_POINT('Ctrl Pts',(-17.0277883227301,17.9573227250749,
4.393559821887));
#195089=CARTESIAN_POINT('Ctrl Pts',(-17.0016757672682,17.9940946809114,
4.39089996085846));
#195090=CARTESIAN_POINT('Ctrl Pts',(-16.9954859929765,18.0029541218301,
4.39026003480146));
#195091=CARTESIAN_POINT('Ctrl Pts',(-16.9854572266273,18.0175450363167,
4.38920742638816));
#195092=CARTESIAN_POINT('Ctrl Pts',(-16.9815778835294,18.0232486351817,
4.38879628475046));
#195093=CARTESIAN_POINT('Ctrl Pts',(-16.9741212726445,18.0343277613249,
4.3879982263231));
#195094=CARTESIAN_POINT('Ctrl Pts',(-16.9705405834183,18.0397009020307,
4.38761144478309));
#195095=CARTESIAN_POINT('Ctrl Pts',(-16.9623278246113,18.0521478964474,
4.38671601232906));
#195096=CARTESIAN_POINT('Ctrl Pts',(-16.9577134656275,18.0592332529884,
4.38620670503767));
#195097=CARTESIAN_POINT('Ctrl Pts',(-16.9454138097052,18.0783691173359,
4.38483218883365));
#195098=CARTESIAN_POINT('Ctrl Pts',(-16.9378080003604,18.0904699641766,
4.38396405047665));
#195099=CARTESIAN_POINT('Ctrl Pts',(-16.8690460597599,18.2023694451796,
4.37594452549632));
#195100=CARTESIAN_POINT('Ctrl Pts',(-16.8161523942463,18.3069858895769,
4.36849028879542));
#195101=CARTESIAN_POINT('Ctrl Pts',(-16.7107926865835,18.5667929340149,
4.35017616402295));
#195102=CARTESIAN_POINT('Ctrl Pts',(-16.6671333362167,18.7247562947737,
4.3391746047566));
#195103=CARTESIAN_POINT('Ctrl Pts',(-16.637193347888,18.9175706191703,4.32678446692435));
#195104=CARTESIAN_POINT('Ctrl Pts',(-16.6330245216234,18.9490816365276,
4.32479368431312));
#195105=CARTESIAN_POINT('Ctrl Pts',(-16.6287844060638,18.9878229682364,
4.32239740568799));
#195106=CARTESIAN_POINT('Ctrl Pts',(-16.6280386384158,18.994973540069,4.32195725595343));
#195107=CARTESIAN_POINT('Ctrl Pts',(-16.6269249166321,19.0062064664921,
4.32126931948258));
#195108=CARTESIAN_POINT('Ctrl Pts',(-16.6265323752652,19.0102862494254,
4.32102018614093));
#195109=CARTESIAN_POINT('Ctrl Pts',(-16.6258197612817,19.0179252704006,
4.32055509481909));
#195110=CARTESIAN_POINT('Ctrl Pts',(-16.6254968559095,19.0214841386238,
4.3203389855196));
#195111=CARTESIAN_POINT('Ctrl Pts',(-16.6247790474197,19.0296243754028,
4.31984595633227));
#195112=CARTESIAN_POINT('Ctrl Pts',(-16.6243900591065,19.034206215606,4.31956937131007));
#195113=CARTESIAN_POINT('Ctrl Pts',(-16.6234119662117,19.0461901445694,
4.31884828388752));
#195114=CARTESIAN_POINT('Ctrl Pts',(-16.6228468659472,19.0535942025803,
4.31840509402368));
#195115=CARTESIAN_POINT('Ctrl Pts',(-16.6193611045964,19.1026666628772,
4.3154822002857));
#195116=CARTESIAN_POINT('Ctrl Pts',(-16.6176350585818,19.1444137639373,
4.31306467071894));
#195117=CARTESIAN_POINT('Ctrl Pts',(-16.6170489590419,19.1944164593618,
4.31022283046059));
#195118=CARTESIAN_POINT('Ctrl Pts',(-16.61700048749,19.2026459166037,4.30975686326737));
#195119=CARTESIAN_POINT('Ctrl Pts',(-16.6169984731698,19.2369080501551,
4.30782338691925));
#195120=CARTESIAN_POINT('Ctrl Pts',(-16.6174771214944,19.2629391384073,
4.30637003367368));
#195121=CARTESIAN_POINT('Ctrl Pts',(-16.6200726497615,19.3333768594573,
4.30246461686822));
#195122=CARTESIAN_POINT('Ctrl Pts',(-16.6231082557594,19.3777369073968,
4.30003426143808));
#195123=CARTESIAN_POINT('Ctrl Pts',(-16.6384343473003,19.5307628983407,
4.29166126775283));
#195124=CARTESIAN_POINT('Ctrl Pts',(-16.6577423292433,19.6385475593011,
4.2857737723225));
#195125=CARTESIAN_POINT('Ctrl Pts',(-16.7043541571101,19.8175921656384,
4.27548628601285));
#195126=CARTESIAN_POINT('Ctrl Pts',(-16.72733223724,19.889748149863,4.27119623087738));
#195127=CARTESIAN_POINT('Ctrl Pts',(-16.7608112661022,19.9781845935418,
4.26567538912572));
#195128=CARTESIAN_POINT('Ctrl Pts',(-16.7677366613975,19.9957639321345,
4.26456475847457));
#195129=CARTESIAN_POINT('Ctrl Pts',(-16.7781439846533,20.0211788047035,
4.26293885389868));
#195130=CARTESIAN_POINT('Ctrl Pts',(-16.7814397989613,20.0290899133859,
4.26242986571197));
#195131=CARTESIAN_POINT('Ctrl Pts',(-16.7873007725456,20.0429211157723,
4.26153483933823));
#195132=CARTESIAN_POINT('Ctrl Pts',(-16.7898451435989,20.0488499376076,
4.26114951237064));
#195133=CARTESIAN_POINT('Ctrl Pts',(-16.7948370813972,20.060336833812,4.26039966959961));
#195134=CARTESIAN_POINT('Ctrl Pts',(-16.7972815440673,20.065896194522,4.26003526295441));
#195135=CARTESIAN_POINT('Ctrl Pts',(-16.8031803317689,20.0791564633059,
4.2591624428008));
#195136=CARTESIAN_POINT('Ctrl Pts',(-16.8066568357113,20.0868473382104,
4.2586532710136));
#195137=CARTESIAN_POINT('Ctrl Pts',(-16.8193555616691,20.1144982713477,
4.25681189124235));
#195138=CARTESIAN_POINT('Ctrl Pts',(-16.8288423736915,20.1343346160819,
4.25547058551369));
#195139=CARTESIAN_POINT('Ctrl Pts',(-16.9218540721198,20.3212778320708,
4.24263112929833));
#195140=CARTESIAN_POINT('Ctrl Pts',(-17.0268314031326,20.4767554904814,
4.23032151974281));
#195141=CARTESIAN_POINT('Ctrl Pts',(-17.203480495964,20.6757509026055,4.21275586767703));
#195142=CARTESIAN_POINT('Ctrl Pts',(-17.2594556963321,20.732087093671,4.20754440657923));
#195143=CARTESIAN_POINT('Ctrl Pts',(-17.3450953158364,20.8090974298502,
4.2002039866135));
#195144=CARTESIAN_POINT('Ctrl Pts',(-17.372330752474,20.8323663465069,4.19795424391827));
#195145=CARTESIAN_POINT('Ctrl Pts',(-17.4059329352687,20.8596304682066,
4.19529214563405));
#195146=CARTESIAN_POINT('Ctrl Pts',(-17.4117454433443,20.8642959324707,
4.19483564366738));
#195147=CARTESIAN_POINT('Ctrl Pts',(-17.4208376849063,20.8715152845359,
4.19412790726711));
#195148=CARTESIAN_POINT('Ctrl Pts',(-17.4241004390102,20.8740903212888,
4.1938751980102));
#195149=CARTESIAN_POINT('Ctrl Pts',(-17.4301766274713,20.878856807584,4.19340695426395));
#195150=CARTESIAN_POINT('Ctrl Pts',(-17.4329879882371,20.8810507366181,
4.19319124704778));
#195151=CARTESIAN_POINT('Ctrl Pts',(-17.4393708098283,20.8860058622604,
4.19270362923973));
#195152=CARTESIAN_POINT('Ctrl Pts',(-17.4429455577205,20.8887627384671,
4.1924320252486));
#195153=CARTESIAN_POINT('Ctrl Pts',(-17.4535663338135,20.8968995270186,
4.19162938938989));
#195154=CARTESIAN_POINT('Ctrl Pts',(-17.4606374673259,20.9022467162709,
4.1911006083338));
#195155=CARTESIAN_POINT('Ctrl Pts',(-17.5135319948742,20.9417257381824,
4.1871849170608));
#195156=CARTESIAN_POINT('Ctrl Pts',(-17.5606911631499,20.9740375302445,
4.18391448520274));
#195157=CARTESIAN_POINT('Ctrl Pts',(-17.7373501869243,21.0848452268982,
4.17222289170266));
#195158=CARTESIAN_POINT('Ctrl Pts',(-17.8738598788654,21.1513018608102,
4.16420749353028));
#195159=CARTESIAN_POINT('Ctrl Pts',(-18.1035156055683,21.2340603346366,
4.15076204402042));
#195160=CARTESIAN_POINT('Ctrl Pts',(-18.1926939348683,21.2597236409817,
4.14555624900042));
#195161=CARTESIAN_POINT('Ctrl Pts',(-18.3038463138748,21.2839449340748,
4.13892976063124));
#195162=CARTESIAN_POINT('Ctrl Pts',(-18.324497247321,21.288123092583,4.13769322565967));
#195163=CARTESIAN_POINT('Ctrl Pts',(-18.3540092600314,21.2936368453675,
4.13591710654804));
#195164=CARTESIAN_POINT('Ctrl Pts',(-18.3628221935975,21.2952255694682,
4.1353855831559));
#195165=CARTESIAN_POINT('Ctrl Pts',(-18.3780651898459,21.2978737086659,
4.13446418950468));
#195166=CARTESIAN_POINT('Ctrl Pts',(-18.3844905993502,21.2989594446238,
4.13407516149355));
#195167=CARTESIAN_POINT('Ctrl Pts',(-18.3968182685827,21.3009840184618,
4.13332753124733));
#195168=CARTESIAN_POINT('Ctrl Pts',(-18.4027196999227,21.3019275642809,
4.13296908265181));
#195169=CARTESIAN_POINT('Ctrl Pts',(-18.4181096159665,21.3043213799239,
4.13203284768305));
#195170=CARTESIAN_POINT('Ctrl Pts',(-18.4276040300351,21.305732116337,4.13145381406636));
#195171=CARTESIAN_POINT('Ctrl Pts',(-18.4601866293815,21.3103471762095,
4.12946157190856));
#195172=CARTESIAN_POINT('Ctrl Pts',(-18.4833173229155,21.3132346337751,
4.12803841341041));
#195173=CARTESIAN_POINT('Ctrl Pts',(-18.6762836344439,21.3340931355481,
4.11608808533391));
#195174=CARTESIAN_POINT('Ctrl Pts',(-18.8476436772053,21.3318298100536,
4.10489906855872));
#195175=CARTESIAN_POINT('Ctrl Pts',(-19.1063745545575,21.2969505592224,
4.08764697788675));
#195176=CARTESIAN_POINT('Ctrl Pts',(-19.1950578905991,21.2791586405268,
4.08168383185548));
#195177=CARTESIAN_POINT('Ctrl Pts',(-19.3196740187697,21.2457405765133,
4.07344070081578));
#195178=CARTESIAN_POINT('Ctrl Pts',(-19.3567321701541,21.2347065868923,
4.07100780714257));
#195179=CARTESIAN_POINT('Ctrl Pts',(-19.4007094674453,21.2202898073772,
4.0681596518496));
#195180=CARTESIAN_POINT('Ctrl Pts',(-19.407936305669,21.2178774013286,4.06769289049096));
#195181=CARTESIAN_POINT('Ctrl Pts',(-19.4191195770003,21.214077068325,4.0669727539404));
#195182=CARTESIAN_POINT('Ctrl Pts',(-19.4230850900762,21.2127163424863,
4.0667178209751));
#195183=CARTESIAN_POINT('Ctrl Pts',(-19.4304131528273,21.2101774345724,
4.06624753536373));
#195184=CARTESIAN_POINT('Ctrl Pts',(-19.433776742609,21.2090025538389,4.06603199687738));
#195185=CARTESIAN_POINT('Ctrl Pts',(-19.4413507359171,21.2063355330595,
4.06554737376713));
#195186=CARTESIAN_POINT('Ctrl Pts',(-19.44555937988,21.2048385598734,4.06527857973651));
#195187=CARTESIAN_POINT('Ctrl Pts',(-19.4578987970621,21.2004055042796,
4.06449186908883));
#195188=CARTESIAN_POINT('Ctrl Pts',(-19.4660164742409,21.1974328873808,
4.06397607251001));
#195189=CARTESIAN_POINT('Ctrl Pts',(-19.5224621650846,21.1763700009335,
4.06040026662786));
#195190=CARTESIAN_POINT('Ctrl Pts',(-19.5701370130605,21.1565661524418,
4.05743505377173));
#195191=CARTESIAN_POINT('Ctrl Pts',(-19.636925934135,21.1259131308532,4.05329619516721));
#195192=CARTESIAN_POINT('Ctrl Pts',(-19.6566654427852,21.1164805346011,
4.05207491840168));
#195193=CARTESIAN_POINT('Ctrl Pts',(-19.7995547650047,21.0454591781868,
4.04322471149285));
#195194=CARTESIAN_POINT('Ctrl Pts',(-19.916583212246,20.9722912961926,4.03590134546389));
#195195=CARTESIAN_POINT('Ctrl Pts',(-20.0975673974847,20.832914122616,4.0233071191621));
#195196=CARTESIAN_POINT('Ctrl Pts',(-20.1658131725678,20.7729954462517,
4.01820661662544));
#195197=CARTESIAN_POINT('Ctrl Pts',(-20.2447378791476,20.6941702107017,
4.01170751222547));
#195198=CARTESIAN_POINT('Ctrl Pts',(-20.2592564945129,20.6792354694394,
4.01048489129421));
#195199=CARTESIAN_POINT('Ctrl Pts',(-20.279670357033,20.6576069275721,4.00872530717446));
#195200=CARTESIAN_POINT('Ctrl Pts',(-20.2857476193548,20.6510860313311,
4.00819619783071));
#195201=CARTESIAN_POINT('Ctrl Pts',(-20.2961911308814,20.6397372885967,
4.00727765435714));
#195202=CARTESIAN_POINT('Ctrl Pts',(-20.3005766609677,20.6349272920634,
4.00688904825375));
#195203=CARTESIAN_POINT('Ctrl Pts',(-20.3089521401547,20.6256556406509,
4.00614128713957));
#195204=CARTESIAN_POINT('Ctrl Pts',(-20.3129454924414,20.6211971337934,
4.00578228124705));
#195205=CARTESIAN_POINT('Ctrl Pts',(-20.323326263625,20.6095078159399,4.0048424946448));
#195206=CARTESIAN_POINT('Ctrl Pts',(-20.3296832005953,20.602250229833,4.00426044806461));
#195207=CARTESIAN_POINT('Ctrl Pts',(-20.3514219070606,20.577086598985,4.00224712433017));
#195208=CARTESIAN_POINT('Ctrl Pts',(-20.3665532241883,20.5589674034557,
4.00080561241734));
#195209=CARTESIAN_POINT('Ctrl Pts',(-20.4850678695611,20.4121273915577,
3.98918380176066));
#195210=CARTESIAN_POINT('Ctrl Pts',(-20.5733549462891,20.2719898213501,
3.97838997625524));
#195211=CARTESIAN_POINT('Ctrl Pts',(-20.6734505473955,20.0623223155182,
3.963036326288));
#195212=CARTESIAN_POINT('Ctrl Pts',(-20.6995188410847,20.0002690167383,
3.95859029255549));
#195213=CARTESIAN_POINT('Ctrl Pts',(-20.7225806759744,19.9371101122702,
3.95421657486109));
#195214=CARTESIAN_POINT('',(-20.8509992439641,19.2092108506511,4.48828862659254));
#195215=CARTESIAN_POINT('Ctrl Pts',(-20.7225806064494,19.9371103026767,
3.73234504707874));
#195216=CARTESIAN_POINT('Ctrl Pts',(-20.7168696304283,19.9527508136538,
3.73327499017389));
#195217=CARTESIAN_POINT('Ctrl Pts',(-20.7109725058956,19.9683284018271,
3.73420949014154));
#195218=CARTESIAN_POINT('Ctrl Pts',(-20.6832634653051,20.0389917889889,
3.7384902088931));
#195219=CARTESIAN_POINT('Ctrl Pts',(-20.6593330525292,20.0932075531427,
3.74189155812553));
#195220=CARTESIAN_POINT('Ctrl Pts',(-20.6277538445489,20.1573272320699,
3.7460905102994));
#195221=CARTESIAN_POINT('Ctrl Pts',(-20.622250176804,20.168261779382,3.74681289219443));
#195222=CARTESIAN_POINT('Ctrl Pts',(-20.6130255007591,20.1862000066534,
3.74800870193385));
#195223=CARTESIAN_POINT('Ctrl Pts',(-20.6093593733053,20.1932316955886,
3.7484801987666));
#195224=CARTESIAN_POINT('Ctrl Pts',(-20.6026761015929,20.2058764927002,
3.74933311093481));
#195225=CARTESIAN_POINT('Ctrl Pts',(-20.5996729429309,20.2114969150553,
3.74971402699587));
#195226=CARTESIAN_POINT('Ctrl Pts',(-20.5931997764901,20.2234809763269,
3.75053014623025));
#195227=CARTESIAN_POINT('Ctrl Pts',(-20.5897223786286,20.2298405114377,
3.7509656096224));
#195228=CARTESIAN_POINT('Ctrl Pts',(-20.5802117563529,20.2470235020649,
3.75214872340126));
#195229=CARTESIAN_POINT('Ctrl Pts',(-20.5741161202903,20.2578119218562,
3.75289860566175));
#195230=CARTESIAN_POINT('Ctrl Pts',(-20.5423238334514,20.3129439982901,
3.7567676853936));
#195231=CARTESIAN_POINT('Ctrl Pts',(-20.5151195681332,20.3563942699004,
3.75994128189931));
#195232=CARTESIAN_POINT('Ctrl Pts',(-20.3905638624033,20.540150084319,3.77392327858955));
#195233=CARTESIAN_POINT('Ctrl Pts',(-20.278021974646,20.6693632296009,3.78529518480088));
#195234=CARTESIAN_POINT('Ctrl Pts',(-20.0828463791118,20.8452499981519,
3.80257347817695));
#195235=CARTESIAN_POINT('Ctrl Pts',(-20.0105227441864,20.9023465867342,
3.80854955411206));
#195236=CARTESIAN_POINT('Ctrl Pts',(-19.9267413411507,20.960042758568,3.81483435935799));
#195237=CARTESIAN_POINT('Ctrl Pts',(-19.9187407994087,20.9654719218458,
3.81542839819196));
#195238=CARTESIAN_POINT('Ctrl Pts',(-19.9068673040276,20.9734110131545,
3.81630067326625));
#195239=CARTESIAN_POINT('Ctrl Pts',(-19.9030230193468,20.9759633065063,
3.81658165812261));
#195240=CARTESIAN_POINT('Ctrl Pts',(-19.8961854756308,20.9804707405698,
3.81707884488073));
#195241=CARTESIAN_POINT('Ctrl Pts',(-19.8931955816986,20.9824308864719,
3.81729537992134));
#195242=CARTESIAN_POINT('Ctrl Pts',(-19.8867759724377,20.9866163074762,
3.81775842541092));
#195243=CARTESIAN_POINT('Ctrl Pts',(-19.8833447821085,20.9888392184039,
3.81800477846252));
#195244=CARTESIAN_POINT('Ctrl Pts',(-19.8739014914335,20.9949183290227,
3.81867973056067));
#195245=CARTESIAN_POINT('Ctrl Pts',(-19.8678762176468,20.9987541053402,
3.81910699066484));
#195246=CARTESIAN_POINT('Ctrl Pts',(-19.835494536006,21.019139185873,3.82138575513574));
#195247=CARTESIAN_POINT('Ctrl Pts',(-19.8087935372755,21.0351372239326,
3.82320308113566));
#195248=CARTESIAN_POINT('Ctrl Pts',(-19.6393305023987,21.1316583053444,
3.83441829111504));
#195249=CARTESIAN_POINT('Ctrl Pts',(-19.4879597995627,21.1959706914068,
3.84307899541137));
#195250=CARTESIAN_POINT('Ctrl Pts',(-19.2182120936925,21.2752106745866,
3.85846837068923));
#195251=CARTESIAN_POINT('Ctrl Pts',(-19.1032202626038,21.2988453394168,
3.86501042879958));
#195252=CARTESIAN_POINT('Ctrl Pts',(-18.972679902309,21.3145506285162,3.87271301899665));
#195253=CARTESIAN_POINT('Ctrl Pts',(-18.9584707434067,21.3161142992548,
3.87355481392854));
#195254=CARTESIAN_POINT('Ctrl Pts',(-18.9358327579793,21.3183737314754,
3.8749017672507));
#195255=CARTESIAN_POINT('Ctrl Pts',(-18.9274135621793,21.3191631097016,
3.87540398185882));
#195256=CARTESIAN_POINT('Ctrl Pts',(-18.9125575894412,21.3204662549907,
3.87629249215949));
#195257=CARTESIAN_POINT('Ctrl Pts',(-18.9061227318743,21.3210010562646,
3.8766781213542));
#195258=CARTESIAN_POINT('Ctrl Pts',(-18.892809139549,21.3220462415804,3.87747761624303));
#195259=CARTESIAN_POINT('Ctrl Pts',(-18.8859301633169,21.3225524621988,
3.87789160805452));
#195260=CARTESIAN_POINT('Ctrl Pts',(-18.8682679925928,21.3237654584227,
3.87895692664623));
#195261=CARTESIAN_POINT('Ctrl Pts',(-18.8574817358048,21.3244232965217,
3.87960978186614));
#195262=CARTESIAN_POINT('Ctrl Pts',(-18.8124546889602,21.3268235565145,
3.882344865898));
#195263=CARTESIAN_POINT('Ctrl Pts',(-18.7781807188865,21.3278165505495,
3.88445040522089));
#195264=CARTESIAN_POINT('Ctrl Pts',(-18.6888393957829,21.3282343219379,
3.89000362367824));
#195265=CARTESIAN_POINT('Ctrl Pts',(-18.6337945662457,21.3263436378429,
3.89348966655988));
#195266=CARTESIAN_POINT('Ctrl Pts',(-18.4698250632734,21.3142973777107,
3.90405719943152));
#195267=CARTESIAN_POINT('Ctrl Pts',(-18.3615528452754,21.2978464021971,
3.91128708690311));
#195268=CARTESIAN_POINT('Ctrl Pts',(-18.2114890425629,21.2629919115816,
3.92146384158483));
#195269=CARTESIAN_POINT('Ctrl Pts',(-18.1682631169347,21.2514976013884,
3.92441233777086));
#195270=CARTESIAN_POINT('Ctrl Pts',(-18.1012763192632,21.2313924980513,
3.92898260396063));
#195271=CARTESIAN_POINT('Ctrl Pts',(-18.0772506166834,21.2237109630246,
3.93062193163042));
#195272=CARTESIAN_POINT('Ctrl Pts',(-18.0061380222753,21.1995657388441,
3.9354643089776));
#195273=CARTESIAN_POINT('Ctrl Pts',(-17.9594859446093,21.1818641761618,
3.93862832067649));
#195274=CARTESIAN_POINT('Ctrl Pts',(-17.9062948955802,21.1595005349747,
3.94218673066462));
#195275=CARTESIAN_POINT('Ctrl Pts',(-17.8991074104856,21.1564316855042,
3.9426665007003));
#195276=CARTESIAN_POINT('Ctrl Pts',(-17.8876576180704,21.1514678114357,
3.9434288893544));
#195277=CARTESIAN_POINT('Ctrl Pts',(-17.883384373156,21.1495984140603,3.9437130015385));
#195278=CARTESIAN_POINT('Ctrl Pts',(-17.8758325585335,21.1462649777586,
3.94421429758045));
#195279=CARTESIAN_POINT('Ctrl Pts',(-17.8725514922228,21.1448067020571,
3.94443182916393));
#195280=CARTESIAN_POINT('Ctrl Pts',(-17.8656111889867,21.1417009029133,
3.94489138146119));
#195281=CARTESIAN_POINT('Ctrl Pts',(-17.8619529290507,21.1400513239073,
3.94513327373414));
#195282=CARTESIAN_POINT('Ctrl Pts',(-17.8521061852617,21.1355775049156,
3.94578350412289));
#195283=CARTESIAN_POINT('Ctrl Pts',(-17.8459265258999,21.1327337953971,
3.9461906622334));
#195284=CARTESIAN_POINT('Ctrl Pts',(-17.8155066540928,21.1185573343534,
3.94819091762249));
#195285=CARTESIAN_POINT('Ctrl Pts',(-17.7914679162794,21.1067949341273,
3.94975897206591));
#195286=CARTESIAN_POINT('Ctrl Pts',(-17.7228432581424,21.0715880656409,
3.95421700488871));
#195287=CARTESIAN_POINT('Ctrl Pts',(-17.6788607918092,21.0470032229055,
3.95705157878362));
#195288=CARTESIAN_POINT('Ctrl Pts',(-17.5228550937659,20.9523410686637,
3.96717097501148));
#195289=CARTESIAN_POINT('Ctrl Pts',(-17.4165757480954,20.8733887883335,
3.97420842372241));
#195290=CARTESIAN_POINT('Ctrl Pts',(-17.2410517516806,20.715526950815,3.98719497351883));
#195291=CARTESIAN_POINT('Ctrl Pts',(-17.1689926773416,20.6404208108032,
3.99303519302854));
#195292=CARTESIAN_POINT('Ctrl Pts',(-17.0937853362103,20.5495000894048,
3.9999498214986));
#195293=CARTESIAN_POINT('Ctrl Pts',(-17.0849332246235,20.5385787693355,
4.00077786993149));
#195294=CARTESIAN_POINT('Ctrl Pts',(-17.0709745739133,20.5210022060422,
4.00210692585956));
#195295=CARTESIAN_POINT('Ctrl Pts',(-17.065797586662,20.5144032578948,4.00260511211224));
#195296=CARTESIAN_POINT('Ctrl Pts',(-17.0567115108498,20.502678704127,4.00348894146171));
#195297=CARTESIAN_POINT('Ctrl Pts',(-17.0527863408113,20.4975656536958,
4.0038739406019));
#195298=CARTESIAN_POINT('Ctrl Pts',(-17.0446920832965,20.4869215242743,
4.00467455336182));
#195299=CARTESIAN_POINT('Ctrl Pts',(-17.0405266713653,20.4813877585102,
4.00509030507787));
#195300=CARTESIAN_POINT('Ctrl Pts',(-17.0298541693055,20.4670635339918,
4.00616531218814));
#195301=CARTESIAN_POINT('Ctrl Pts',(-17.02338796867,20.4582429935407,4.00682615001767));
#195302=CARTESIAN_POINT('Ctrl Pts',(-16.9962604088946,20.4206305111364,
4.00963964665945));
#195303=CARTESIAN_POINT('Ctrl Pts',(-16.976256356435,20.3913736294851,4.01181731999833));
#195304=CARTESIAN_POINT('Ctrl Pts',(-16.9256711461044,20.3132511307669,
4.01760782934577));
#195305=CARTESIAN_POINT('Ctrl Pts',(-16.8963365321344,20.2636171418002,
4.02126324208149));
#195306=CARTESIAN_POINT('Ctrl Pts',(-16.7931988145228,20.0716275062087,
4.03529985020796));
#195307=CARTESIAN_POINT('Ctrl Pts',(-16.7336272484179,19.9222597648831,
4.04606240769764));
#195308=CARTESIAN_POINT('Ctrl Pts',(-16.6877273811675,19.7538272705526,
4.05741698812309));
#195309=CARTESIAN_POINT('Ctrl Pts',(-16.6841109151314,19.7400064554014,
4.05834277012739));
#195310=CARTESIAN_POINT('Ctrl Pts',(-16.6786274231437,19.7181494897221,
4.05979653150733));
#195311=CARTESIAN_POINT('Ctrl Pts',(-16.6766670337921,19.7101373597414,
4.06032726254465));
#195312=CARTESIAN_POINT('Ctrl Pts',(-16.6647681487689,19.6602451900943,
4.06361787058717));
#195313=CARTESIAN_POINT('Ctrl Pts',(-16.6560612270731,19.6180782877685,
4.06633659837874));
#195314=CARTESIAN_POINT('Ctrl Pts',(-16.6473550468378,19.568292545095,4.06945132282921));
#195315=CARTESIAN_POINT('Ctrl Pts',(-16.6461037192063,19.5609060556804,
4.06991099376607));
#195316=CARTESIAN_POINT('Ctrl Pts',(-16.6441444281326,19.5489556422237,
4.07065056052939));
#195317=CARTESIAN_POINT('Ctrl Pts',(-16.6434121550079,19.5443958468252,
4.07093178094086));
#195318=CARTESIAN_POINT('Ctrl Pts',(-16.6421394154587,19.5363015204073,
4.07142922795462));
#195319=CARTESIAN_POINT('Ctrl Pts',(-16.641592977027,19.532767983536,4.07164578900032));
#195320=CARTESIAN_POINT('Ctrl Pts',(-16.6404412830981,19.5251935600743,
4.0721087168901));
#195321=CARTESIAN_POINT('Ctrl Pts',(-16.6398387745129,19.5211523119757,
4.07235492724245));
#195322=CARTESIAN_POINT('Ctrl Pts',(-16.6382167729572,19.5100527112808,
4.07302908587159));
#195323=CARTESIAN_POINT('Ctrl Pts',(-16.6372212292934,19.5029908369928,
4.07345570044128));
#195324=CARTESIAN_POINT('Ctrl Pts',(-16.6320932341326,19.4652362241726,
4.07572483700404));
#195325=CARTESIAN_POINT('Ctrl Pts',(-16.6285987401311,19.4344588844199,
4.0775335216847));
#195326=CARTESIAN_POINT('Ctrl Pts',(-16.6200627582494,19.3410300248442,
4.08292964150221));
#195327=CARTESIAN_POINT('Ctrl Pts',(-16.6171340551401,19.2782175275517,
4.08642992354793));
#195328=CARTESIAN_POINT('Ctrl Pts',(-16.616953707009,19.1907231919099,4.09123805107953));
#195329=CARTESIAN_POINT('Ctrl Pts',(-16.6173331192014,19.1660833855326,
4.09258457032675));
#195330=CARTESIAN_POINT('Ctrl Pts',(-16.624174195859,18.9579468847463,4.10393234758351));
#195331=CARTESIAN_POINT('Ctrl Pts',(-16.6540502841451,18.7760243720731,
4.11376258135185));
#195332=CARTESIAN_POINT('Ctrl Pts',(-16.7134517158726,18.578883608284,4.12573510593473));
#195333=CARTESIAN_POINT('Ctrl Pts',(-16.7202236136068,18.5576309534037,
4.12704244263184));
#195334=CARTESIAN_POINT('Ctrl Pts',(-16.7300347845924,18.5284426846403,
4.12886257430851));
#195335=CARTESIAN_POINT('Ctrl Pts',(-16.7327880585426,18.5204119639808,
4.12936595358267));
#195336=CARTESIAN_POINT('Ctrl Pts',(-16.7375979334902,18.5066529052532,
4.13023295115586));
#195337=CARTESIAN_POINT('Ctrl Pts',(-16.7396310843441,18.5009164358201,
4.13059578915481));
#195338=CARTESIAN_POINT('Ctrl Pts',(-16.7438681335245,18.4891234928006,
4.13134455932915));
#195339=CARTESIAN_POINT('Ctrl Pts',(-16.7460750074265,18.4830681624735,
4.13173058748616));
#195340=CARTESIAN_POINT('Ctrl Pts',(-16.7512655468315,18.4690257528709,
4.13262945798287));
#195341=CARTESIAN_POINT('Ctrl Pts',(-16.7542698664453,18.4610464746681,
4.13314298672208));
#195342=CARTESIAN_POINT('Ctrl Pts',(-16.7640008798335,18.4356675152782,
4.13478527875509));
#195343=CARTESIAN_POINT('Ctrl Pts',(-16.7709092494871,18.418338870885,4.13592012105316));
#195344=CARTESIAN_POINT('Ctrl Pts',(-16.8394972472511,18.2526941040955,
4.14690127404881));
#195345=CARTESIAN_POINT('Ctrl Pts',(-16.9176283329592,18.1117885085386,
4.15733620684613));
#195346=CARTESIAN_POINT('Ctrl Pts',(-17.0889479800298,17.8717711474586,
4.17681149319563));
#195347=CARTESIAN_POINT('Ctrl Pts',(-17.1772154353026,17.7701120455588,
4.18573912392085));
#195348=CARTESIAN_POINT('Ctrl Pts',(-17.2858831507387,17.6666903436825,
4.19509723160919));
#195349=CARTESIAN_POINT('Ctrl Pts',(-17.2973582224274,17.6560095949428,
4.19606709460667));
#195350=CARTESIAN_POINT('Ctrl Pts',(-17.3132315918932,17.641560726787,4.19738253965967));
#195351=CARTESIAN_POINT('Ctrl Pts',(-17.317527949004,17.6376820307599,4.19773600580456));
#195352=CARTESIAN_POINT('Ctrl Pts',(-17.3243811705881,17.6315458574981,
4.1982956677512));
#195353=CARTESIAN_POINT('Ctrl Pts',(-17.3269276389225,17.62927688783,4.19850271715049));
#195354=CARTESIAN_POINT('Ctrl Pts',(-17.3321988144442,17.6246029362627,
4.19892942087962));
#195355=CARTESIAN_POINT('Ctrl Pts',(-17.3349242327085,17.6221988150846,
4.19914900608805));
#195356=CARTESIAN_POINT('Ctrl Pts',(-17.3414341307431,17.6164861027618,
4.19967106828158));
#195357=CARTESIAN_POINT('Ctrl Pts',(-17.3452242593567,17.6131839241978,
4.19997306816115));
#195358=CARTESIAN_POINT('Ctrl Pts',(-17.3580511065571,17.6020885553827,
4.20098870327018));
#195359=CARTESIAN_POINT('Ctrl Pts',(-17.3671421337033,17.594358115691,4.20169785130045));
#195360=CARTESIAN_POINT('Ctrl Pts',(-17.4723890985755,17.5063852014455,
4.20979223754029));
#195361=CARTESIAN_POINT('Ctrl Pts',(-17.5754323550403,17.434738861008,4.21662725626206));
#195362=CARTESIAN_POINT('Ctrl Pts',(-17.8297782888984,17.2894984116068,
4.23254690378475));
#195363=CARTESIAN_POINT('Ctrl Pts',(-17.9846747828019,17.2239695446759,
4.24159473270096));
#195364=CARTESIAN_POINT('Ctrl Pts',(-18.1682311459902,17.1708661460297,
4.25269286268768));
#195365=CARTESIAN_POINT('Ctrl Pts',(-18.1908972254461,17.1647155990138,
4.25406828399201));
#195366=CARTESIAN_POINT('Ctrl Pts',(-18.2229927763016,17.1565771339279,
4.25602478122169));
#195367=CARTESIAN_POINT('Ctrl Pts',(-18.2323411768619,17.1542744189303,
4.25659569576602));
#195368=CARTESIAN_POINT('Ctrl Pts',(-18.2475226003015,17.1506445644508,
4.25752465905837));
#195369=CARTESIAN_POINT('Ctrl Pts',(-18.253346179477,17.1492782232074,4.25788144119941));
#195370=CARTESIAN_POINT('Ctrl Pts',(-18.2655216449632,17.146475977675,4.25862830898798));
#195371=CARTESIAN_POINT('Ctrl Pts',(-18.2718745141716,17.1450446660752,
4.2590185379482));
#195372=CARTESIAN_POINT('Ctrl Pts',(-18.286954905512,17.1417200679604,4.25994616334838));
#195373=CARTESIAN_POINT('Ctrl Pts',(-18.2956879512573,17.139852661505,4.26048438323833));
#195374=CARTESIAN_POINT('Ctrl Pts',(-18.32492261612,17.1337945286948,4.26228971333829));
#195375=CARTESIAN_POINT('Ctrl Pts',(-18.345474008329,17.1298526288414,4.2635647278182));
#195376=CARTESIAN_POINT('Ctrl Pts',(-18.4562178954664,17.1103086832154,
4.2704690663485));
#195377=CARTESIAN_POINT('Ctrl Pts',(-18.5472809602832,17.1002657380717,
4.2762725078705));
#195378=CARTESIAN_POINT('Ctrl Pts',(-18.7837439420155,17.0896100163733,
4.29162498583937));
#195379=CARTESIAN_POINT('Ctrl Pts',(-18.9290658749683,17.0980126758185,
4.30135479403314));
#195380=CARTESIAN_POINT('Ctrl Pts',(-19.0865430842553,17.1235114955406,
4.31173183814653));
#195381=CARTESIAN_POINT('Ctrl Pts',(-19.100683774883,17.125948944085,4.31266180418919));
#195382=CARTESIAN_POINT('Ctrl Pts',(-19.120066363348,17.1294932289692,4.31393308955556));
#195383=CARTESIAN_POINT('Ctrl Pts',(-19.125330267095,17.1304764366524,4.31427799662429));
#195384=CARTESIAN_POINT('Ctrl Pts',(-19.1756092459514,17.1400652637452,
4.31756877777429));
#195385=CARTESIAN_POINT('Ctrl Pts',(-19.2203412406334,17.1501112850594,
4.32046871052137));
#195386=CARTESIAN_POINT('Ctrl Pts',(-19.272101273721,17.1635151450424,4.32376474025844));
#195387=CARTESIAN_POINT('Ctrl Pts',(-19.2794770511915,17.1654677947515,
4.32423299237287));
#195388=CARTESIAN_POINT('Ctrl Pts',(-19.2912920776637,17.1686641337814,
4.32498059324628));
#195389=CARTESIAN_POINT('Ctrl Pts',(-19.2957380229532,17.1698825009898,
4.32526134776177));
#195390=CARTESIAN_POINT('Ctrl Pts',(-19.3036328512683,17.172073749403,4.32575884524867));
#195391=CARTESIAN_POINT('Ctrl Pts',(-19.307083282901,17.1730408757304,4.32597591777067));
#195392=CARTESIAN_POINT('Ctrl Pts',(-19.314422457802,17.1751180966599,4.32643686173727));
#195393=CARTESIAN_POINT('Ctrl Pts',(-19.3183104714978,17.1762305714414,
4.32668059263369));
#195394=CARTESIAN_POINT('Ctrl Pts',(-19.3288642272749,17.1792830546387,
4.32734099424625));
#195395=CARTESIAN_POINT('Ctrl Pts',(-19.3355237206898,17.1812447409963,
4.32775642060591));
#195396=CARTESIAN_POINT('Ctrl Pts',(-19.3694403074562,17.1914171295474,
4.32986614367105));
#195397=CARTESIAN_POINT('Ctrl Pts',(-19.3965408674416,17.200144676105,4.33153198673144));
#195398=CARTESIAN_POINT('Ctrl Pts',(-19.4756898391065,17.2274080625796,
4.33636077150797));
#195399=CARTESIAN_POINT('Ctrl Pts',(-19.5272005985897,17.2474383252249,
4.33945668235915));
#195400=CARTESIAN_POINT('Ctrl Pts',(-19.7259159502871,17.3338081697218,
4.35142543963522));
#195401=CARTESIAN_POINT('Ctrl Pts',(-19.8661127017717,17.4148737723795,
4.35996839628424));
#195402=CARTESIAN_POINT('Ctrl Pts',(-20.0519479649809,17.5528074995047,
4.37292802299029));
#195403=CARTESIAN_POINT('Ctrl Pts',(-20.1060490035588,17.5972871168664,
4.37692581698455));
#195404=CARTESIAN_POINT('Ctrl Pts',(-20.1673786866644,17.653026786268,4.38179011641081));
#195405=CARTESIAN_POINT('Ctrl Pts',(-20.1768336405713,17.6617788831947,
4.38254989036287));
#195406=CARTESIAN_POINT('Ctrl Pts',(-20.1921211863307,17.6761913311958,
4.38379489809854));
#195407=CARTESIAN_POINT('Ctrl Pts',(-20.1980021950148,17.6818000084878,
4.38427791398657));
#195408=CARTESIAN_POINT('Ctrl Pts',(-20.2084506497061,17.6918801445827,
4.38514344968623));
#195409=CARTESIAN_POINT('Ctrl Pts',(-20.2130304362591,17.6963387108741,
4.38552540553394));
#195410=CARTESIAN_POINT('Ctrl Pts',(-20.2218493349009,17.7050023212138,
4.38626593916208));
#195411=CARTESIAN_POINT('Ctrl Pts',(-20.2260909903834,17.7092046986508,
4.3866243976981));
#195412=CARTESIAN_POINT('Ctrl Pts',(-20.2374511255913,17.7205552736815,
4.38759063219959));
#195413=CARTESIAN_POINT('Ctrl Pts',(-20.2445363167496,17.7277364362605,
4.38819987051008));
#195414=CARTESIAN_POINT('Ctrl Pts',(-20.2725837053326,17.7565731190455,
4.39063837078836));
#195415=CARTESIAN_POINT('Ctrl Pts',(-20.2931329091294,17.7786237243496,
4.39248540385731));
#195416=CARTESIAN_POINT('Ctrl Pts',(-20.344199497341,17.8358226776798,4.39723505139397));
#195417=CARTESIAN_POINT('Ctrl Pts',(-20.3740400884609,17.8715511997458,
4.4001639251692));
#195418=CARTESIAN_POINT('Ctrl Pts',(-20.4508340277919,17.9699143125699,
4.40812607392659));
#195419=CARTESIAN_POINT('Ctrl Pts',(-20.4955297900635,18.0342146175184,
4.41322914731125));
#195420=CARTESIAN_POINT('Ctrl Pts',(-20.6177143447865,18.2326044191612,
4.42857136871366));
#195421=CARTESIAN_POINT('Ctrl Pts',(-20.6841792885624,18.3728803655174,
4.43893737344926));
#195422=CARTESIAN_POINT('Ctrl Pts',(-20.7397311164905,18.5335318573357,
4.44953435653013));
#195423=CARTESIAN_POINT('Ctrl Pts',(-20.7445474342756,18.5479619611808,
4.4504750949548));
#195424=CARTESIAN_POINT('Ctrl Pts',(-20.7509595400674,18.5678857772099,
4.45175754668922));
#195425=CARTESIAN_POINT('Ctrl Pts',(-20.7526891017257,18.5733355097367,
4.45210665204186));
#195426=CARTESIAN_POINT('Ctrl Pts',(-20.7554109991224,18.5820340937847,
4.45266112297374));
#195427=CARTESIAN_POINT('Ctrl Pts',(-20.7564176160349,18.5852783963428,
4.45286731466029));
#195428=CARTESIAN_POINT('Ctrl Pts',(-20.7584877194804,18.5920074733691,
4.4532936996337));
#195429=CARTESIAN_POINT('Ctrl Pts',(-20.7595500202379,18.5954925751611,
4.45351381769216));
#195430=CARTESIAN_POINT('Ctrl Pts',(-20.7620715715693,18.6038422824012,
4.45403950978165));
#195431=CARTESIAN_POINT('Ctrl Pts',(-20.7635223357588,18.6087094693374,
4.45434458876453));
#195432=CARTESIAN_POINT('Ctrl Pts',(-20.7684097856681,18.6253246229376,
4.45538156887731));
#195433=CARTESIAN_POINT('Ctrl Pts',(-20.7717621679711,18.6370974072122,
4.45610872234565));
#195434=CARTESIAN_POINT('Ctrl Pts',(-20.7901103991915,18.703720595444,4.46018435262102));
#195435=CARTESIAN_POINT('Ctrl Pts',(-20.8029949398621,18.7591333616955,
4.46342419049857));
#195436=CARTESIAN_POINT('Ctrl Pts',(-20.8383771231678,18.9449475174164,
4.47399382749415));
#195437=CARTESIAN_POINT('Ctrl Pts',(-20.8508874458946,19.0769265174022,
4.48104241160473));
#195438=CARTESIAN_POINT('Ctrl Pts',(-20.8509992439641,19.2092108506511,
4.48828862659254));
#195439=CARTESIAN_POINT('Ctrl Pts',(-20.8509992455944,19.2092127807703,
4.48828873231979));
#195440=CARTESIAN_POINT('Ctrl Pts',(-20.8510695258653,19.2924612585343,
4.49284888304316));
#195441=CARTESIAN_POINT('Ctrl Pts',(-20.8462293851984,19.3756367542194,
4.49747294574716));
#195442=CARTESIAN_POINT('Ctrl Pts',(-20.8325134256674,19.4922434801573,
4.50419755350081));
#195443=CARTESIAN_POINT('Ctrl Pts',(-20.8277010378865,19.526075018031,4.50617710565744));
#195444=CARTESIAN_POINT('Ctrl Pts',(-20.8203843855559,19.5698790278976,
4.50878348017379));
#195445=CARTESIAN_POINT('Ctrl Pts',(-20.8186232139868,19.5799715587436,
4.50938699187165));
#195446=CARTESIAN_POINT('Ctrl Pts',(-20.8155220145444,19.5970118712236,
4.51041121137972));
#195447=CARTESIAN_POINT('Ctrl Pts',(-20.8142202735552,19.6039665041733,
4.51083070588023));
#195448=CARTESIAN_POINT('Ctrl Pts',(-20.811575518071,19.6177147934122,4.51166297853968));
#195449=CARTESIAN_POINT('Ctrl Pts',(-20.8102339834277,19.6245086465562,
4.5120757049779));
#195450=CARTESIAN_POINT('Ctrl Pts',(-20.8075793183357,19.6376138382503,
4.51287469799734));
#195451=CARTESIAN_POINT('Ctrl Pts',(-20.8062706448965,19.6439260090253,
4.51326081796372));
#195452=CARTESIAN_POINT('Ctrl Pts',(-20.8031923800986,19.6584397055503,
4.51415162616798));
#195453=CARTESIAN_POINT('Ctrl Pts',(-20.8014028291732,19.6666368452202,
4.51465694945044));
#195454=CARTESIAN_POINT('Ctrl Pts',(-20.7964823801326,19.6885493087667,
4.51601378251425));
#195455=CARTESIAN_POINT('Ctrl Pts',(-20.7932634574221,19.7022442453515,
4.51686810563248));
#195456=CARTESIAN_POINT('Ctrl Pts',(-20.7715055147565,19.7908396492252,
4.52243687703536));
#195457=CARTESIAN_POINT('Ctrl Pts',(-20.7490266050673,19.8646832986012,
4.52727684458111));
#195458=CARTESIAN_POINT('Ctrl Pts',(-20.7225805792317,19.9371103772171,
4.53222349041431));
#195459=CARTESIAN_POINT('Origin',(-18.734,19.211,0.));
#195460=CARTESIAN_POINT('',(-20.722580628988,19.937110240951,5.55626853452768));
#195461=CARTESIAN_POINT('',(-20.7225805912209,19.9371103443827,5.33540100209137));
#195462=CARTESIAN_POINT('',(-20.7225806064498,19.9371103026755,0.));
#195463=CARTESIAN_POINT('Ctrl Pts',(-20.722580628988,19.937110240951,5.55626853452768));
#195464=CARTESIAN_POINT('Ctrl Pts',(-20.7320991031241,19.9110422250807,
5.55474537328154));
#195465=CARTESIAN_POINT('Ctrl Pts',(-20.7411068404243,19.8847819946634,
5.55321404310531));
#195466=CARTESIAN_POINT('Ctrl Pts',(-20.7754133503966,19.777963845185,5.54697990101072));
#195467=CARTESIAN_POINT('Ctrl Pts',(-20.7963949671106,19.6961196087105,
5.54218749179229));
#195468=CARTESIAN_POINT('Ctrl Pts',(-20.8151326623951,19.5993009538407,
5.5363985457184));
#195469=CARTESIAN_POINT('Ctrl Pts',(-20.8176912853412,19.5853279336306,
5.53556033389131));
#195470=CARTESIAN_POINT('Ctrl Pts',(-20.8214097407618,19.563800185921,5.53426431737361));
#195471=CARTESIAN_POINT('Ctrl Pts',(-20.8226696394578,19.5562629894375,
5.53380969628319));
#195472=CARTESIAN_POINT('Ctrl Pts',(-20.8248931359631,19.5425034518133,
5.53297812002155));
#195473=CARTESIAN_POINT('Ctrl Pts',(-20.8258698385693,19.5362832945917,
5.53260158575233));
#195474=CARTESIAN_POINT('Ctrl Pts',(-20.8279419771641,19.5226914148005,
5.5317774361913));
#195475=CARTESIAN_POINT('Ctrl Pts',(-20.829026260802,19.515318100229,5.53132947256093));
#195476=CARTESIAN_POINT('Ctrl Pts',(-20.8318905543936,19.495099272149,5.53009860290783));
#195477=CARTESIAN_POINT('Ctrl Pts',(-20.8335914776936,19.4822430454582,
5.52931320841856));
#195478=CARTESIAN_POINT('Ctrl Pts',(-20.8416314806073,19.4168589028857,
5.52530436524589));
#195479=CARTESIAN_POINT('Ctrl Pts',(-20.8461174158795,19.3641260456246,
5.52202308694846));
#195480=CARTESIAN_POINT('Ctrl Pts',(-20.8502336389503,19.2773299092953,
5.51653982374483));
#195481=CARTESIAN_POINT('Ctrl Pts',(-20.8510257892788,19.2433434161714,
5.51437226626602));
#195482=CARTESIAN_POINT('Ctrl Pts',(-20.8508977921059,19.0787312499579,
5.50378105246286));
#195483=CARTESIAN_POINT('Ctrl Pts',(-20.8387067170616,18.9484055163899,
5.49508951239572));
#195484=CARTESIAN_POINT('Ctrl Pts',(-20.7970384789104,18.7266530902619,
5.48023960354974));
#195485=CARTESIAN_POINT('Ctrl Pts',(-20.7732180821995,18.6345335431358,
5.47405981513811));
#195486=CARTESIAN_POINT('Ctrl Pts',(-20.7402342475941,18.5351250499886,
5.46758874833196));
#195487=CARTESIAN_POINT('Ctrl Pts',(-20.7371210654857,18.5259534253344,
5.46699366149591));
#195488=CARTESIAN_POINT('Ctrl Pts',(-20.7324307950927,18.5124409977714,
5.4661201473758));
#195489=CARTESIAN_POINT('Ctrl Pts',(-20.7309023232472,18.508083621821,5.46583896042605));
#195490=CARTESIAN_POINT('Ctrl Pts',(-20.7281650633123,18.5003612139798,
5.46534155039907));
#195491=CARTESIAN_POINT('Ctrl Pts',(-20.7269619964458,18.4969942119751,
5.46512499306352));
#195492=CARTESIAN_POINT('Ctrl Pts',(-20.7243657190294,18.4897857450031,
5.46466204853814));
#195493=CARTESIAN_POINT('Ctrl Pts',(-20.7229699190123,18.4859452717126,
5.46441581796844));
#195494=CARTESIAN_POINT('Ctrl Pts',(-20.7191070449355,18.4754118672103,
5.46374154692406));
#195495=CARTESIAN_POINT('Ctrl Pts',(-20.7166172237732,18.4687272548122,
5.46331484089741));
#195496=CARTESIAN_POINT('Ctrl Pts',(-20.7031297572366,18.4330684877702,
5.46104434321567));
#195497=CARTESIAN_POINT('Ctrl Pts',(-20.6915300445275,18.4043242337992,
5.45923443697878));
#195498=CARTESIAN_POINT('Ctrl Pts',(-20.6147735858126,18.2255379525746,
5.44804385098371));
#195499=CARTESIAN_POINT('Ctrl Pts',(-20.5330352088347,18.083201526635,5.43939871382255));
#195500=CARTESIAN_POINT('Ctrl Pts',(-20.3657123610359,17.8570979885976,
5.42400420355024));
#195501=CARTESIAN_POINT('Ctrl Pts',(-20.2879589510966,17.768522228232,5.41743778955221));
#195502=CARTESIAN_POINT('Ctrl Pts',(-20.1929613279495,17.6769448023356,
5.40970778591301));
#195503=CARTESIAN_POINT('Ctrl Pts',(-20.1825655608044,17.6671245817611,
5.40886565903804));
#195504=CARTESIAN_POINT('Ctrl Pts',(-20.1658644154931,17.6516652604515,
5.4075182737988));
#195505=CARTESIAN_POINT('Ctrl Pts',(-20.1596232412761,17.6459572194073,
5.4070159622059));
#195506=CARTESIAN_POINT('Ctrl Pts',(-20.1485570613703,17.6359574553908,
5.40612733892172));
#195507=CARTESIAN_POINT('Ctrl Pts',(-20.1437462831797,17.6316500980351,
5.40574169427212));
#195508=CARTESIAN_POINT('Ctrl Pts',(-20.1337566233701,17.622787809215,5.40494222486369));
#195509=CARTESIAN_POINT('Ctrl Pts',(-20.1285750443515,17.6182360465067,
5.40452827427119));
#195510=CARTESIAN_POINT('Ctrl Pts',(-20.1152202475009,17.6066196405179,
5.40346318284416));
#195511=CARTESIAN_POINT('Ctrl Pts',(-20.1070151011747,17.5995921574072,
5.40281051482796));
#195512=CARTESIAN_POINT('Ctrl Pts',(-20.0725673216113,17.5705426974243,
5.40007724362974));
#195513=CARTESIAN_POINT('Ctrl Pts',(-20.0458470645127,17.5490975660502,
5.39797336856799));
#195514=CARTESIAN_POINT('Ctrl Pts',(-19.9749015956946,17.4949354874195,
5.39242558435923));
#195515=CARTESIAN_POINT('Ctrl Pts',(-19.9299029427629,17.4632787646679,
5.3889434050106));
#195516=CARTESIAN_POINT('Ctrl Pts',(-19.8068132821667,17.3836656364043,
5.37952163931933));
#195517=CARTESIAN_POINT('Ctrl Pts',(-19.7267585117777,17.3389670105283,
5.37349488361626));
#195518=CARTESIAN_POINT('Ctrl Pts',(-19.5956081871651,17.2765230836912,
5.36389710543965));
#195519=CARTESIAN_POINT('Ctrl Pts',(-19.5462886858002,17.2553014380025,
5.36034708705668));
#195520=CARTESIAN_POINT('Ctrl Pts',(-19.4618385882378,17.2227098381535,
5.3544117276961));
#195521=CARTESIAN_POINT('Ctrl Pts',(-19.4271198685023,17.2103421495578,
5.35201124857902));
#195522=CARTESIAN_POINT('Ctrl Pts',(-19.3471122887055,17.1841743548467,
5.34659330557642));
#195523=CARTESIAN_POINT('Ctrl Pts',(-19.3016451612632,17.170973383084,5.343595801701));
#195524=CARTESIAN_POINT('Ctrl Pts',(-19.248303942376,17.1574080726403,5.34020235095851));
#195525=CARTESIAN_POINT('Ctrl Pts',(-19.2408273098978,17.1555500659615,
5.33972949057989));
#195526=CARTESIAN_POINT('Ctrl Pts',(-19.2288396384694,17.1526404142884,
5.33897596941318));
#195527=CARTESIAN_POINT('Ctrl Pts',(-19.2243350821869,17.1515627079204,
5.33869386801668));
#195528=CARTESIAN_POINT('Ctrl Pts',(-19.2163365248621,17.1496767993993,
5.33819485141022));
#195529=CARTESIAN_POINT('Ctrl Pts',(-19.2128439651575,17.1488626819948,
5.33797759935612));
#195530=CARTESIAN_POINT('Ctrl Pts',(-19.2054209649265,17.1471522525127,
5.33751723502928));
#195531=CARTESIAN_POINT('Ctrl Pts',(-19.2014900368851,17.1462582929048,
5.33727425836989));
#195532=CARTESIAN_POINT('Ctrl Pts',(-19.190838774945,17.1438679928824,5.33661803178459));
#195533=CARTESIAN_POINT('Ctrl Pts',(-19.1841135886215,17.1423931834554,
5.33620599962607));
#195534=CARTESIAN_POINT('Ctrl Pts',(-19.1502449490791,17.135138901002,5.33414202198858));
#195535=CARTESIAN_POINT('Ctrl Pts',(-19.1229955244772,17.1298604541951,
5.33251707659368));
#195536=CARTESIAN_POINT('Ctrl Pts',(-19.0432573198107,17.1160354936811,
5.32784501066362));
#195537=CARTESIAN_POINT('Ctrl Pts',(-18.990538550673,17.1089283747279,5.32485986019752));
#195538=CARTESIAN_POINT('Ctrl Pts',(-18.7974760941367,17.090273908465,5.31412852010918));
#195539=CARTESIAN_POINT('Ctrl Pts',(-18.6563453079949,17.0907452154768,
5.3066446959301));
#195540=CARTESIAN_POINT('Ctrl Pts',(-18.424923898893,17.1146698138369,5.29377537164573));
#195541=CARTESIAN_POINT('Ctrl Pts',(-18.3342673858073,17.1300533091335,
5.28858416500654));
#195542=CARTESIAN_POINT('Ctrl Pts',(-18.2315117169558,17.1544533890304,
5.28239269105735));
#195543=CARTESIAN_POINT('Ctrl Pts',(-18.2181520159386,17.1577637053465,
5.28158175805247));
#195544=CARTESIAN_POINT('Ctrl Pts',(-18.196788139878,17.1632789920246,5.28027501444872));
#195545=CARTESIAN_POINT('Ctrl Pts',(-18.1887628684888,17.1654012180818,
5.27978187592572));
#195546=CARTESIAN_POINT('Ctrl Pts',(-18.174541277107,17.1692516520653,5.27890387653416));
#195547=CARTESIAN_POINT('Ctrl Pts',(-18.1683399297347,17.1709610144871,
5.27851963149954));
#195548=CARTESIAN_POINT('Ctrl Pts',(-18.1554408730214,17.1745798956038,
5.27771744273082));
#195549=CARTESIAN_POINT('Ctrl Pts',(-18.1487446122199,17.1764942530753,
5.27729934529966));
#195550=CARTESIAN_POINT('Ctrl Pts',(-18.1313908689076,17.1815481840478,
5.27621145311304));
#195551=CARTESIAN_POINT('Ctrl Pts',(-18.120748540683,17.184738645085,5.27554000308284));
#195552=CARTESIAN_POINT('Ctrl Pts',(-18.0747485010194,17.1989245737963,
5.27261878435714));
#195553=CARTESIAN_POINT('Ctrl Pts',(-18.0396592970887,17.2107623200322,
5.27034155439784));
#195554=CARTESIAN_POINT('Ctrl Pts',(-17.9473759675078,17.2446160131358,
5.26421777951816));
#195555=CARTESIAN_POINT('Ctrl Pts',(-17.8907997043677,17.2682042025782,
5.26032231174481));
#195556=CARTESIAN_POINT('Ctrl Pts',(-17.6945052438671,17.3602351751819,
5.24632088884511));
#195557=CARTESIAN_POINT('Ctrl Pts',(-17.5613994025567,17.4415702276248,
5.23588323616264));
#195558=CARTESIAN_POINT('Ctrl Pts',(-17.4260086620967,17.5463398278746,
5.22475317908484));
#195559=CARTESIAN_POINT('Ctrl Pts',(-17.4137155305347,17.5560728816246,
5.22373793903934));
#195560=CARTESIAN_POINT('Ctrl Pts',(-17.363772096677,17.5965261950981,5.21959749635092));
#195561=CARTESIAN_POINT('Ctrl Pts',(-17.3270736037052,17.628404316633,5.21651747161211));
#195562=CARTESIAN_POINT('Ctrl Pts',(-17.2858216476618,17.6668080783347,
5.21304209592719));
#195563=CARTESIAN_POINT('Ctrl Pts',(-17.2801703134101,17.6721275303872,
5.21256569186294));
#195564=CARTESIAN_POINT('Ctrl Pts',(-17.2711810731022,17.6806825838358,
5.21180762150207));
#195565=CARTESIAN_POINT('Ctrl Pts',(-17.2678244109493,17.6838982515472,
5.21152448754234));
#195566=CARTESIAN_POINT('Ctrl Pts',(-17.2618953275107,17.6896158573227,
5.21102430209545));
#195567=CARTESIAN_POINT('Ctrl Pts',(-17.259318643427,17.6921133111173,5.21080690817546));
#195568=CARTESIAN_POINT('Ctrl Pts',(-17.2538675405774,17.6974237459058,
5.21034696861655));
#195569=CARTESIAN_POINT('Ctrl Pts',(-17.2509947898639,17.7002383636974,
5.21010455487945));
#195570=CARTESIAN_POINT('Ctrl Pts',(-17.2432564634526,17.7078634387398,
5.20945144187044));
#195571=CARTESIAN_POINT('Ctrl Pts',(-17.2384061106458,17.7126893731268,
5.20904194069538));
#195572=CARTESIAN_POINT('Ctrl Pts',(-17.2143686654116,17.7368388347746,
5.20701133541773));
#195573=CARTESIAN_POINT('Ctrl Pts',(-17.1955313062976,17.7565087586766,
5.20541619656832));
#195574=CARTESIAN_POINT('Ctrl Pts',(-17.1420511874591,17.8145544720225,
5.20085683390368));
#195575=CARTESIAN_POINT('Ctrl Pts',(-17.1084263736188,17.8538440616697,
5.19795107322898));
#195576=CARTESIAN_POINT('Ctrl Pts',(-16.9903960249174,18.0024476766135,
5.18743882826584));
#195577=CARTESIAN_POINT('Ctrl Pts',(-16.915302568965,18.1187108407294,5.18009490839895));
#195578=CARTESIAN_POINT('Ctrl Pts',(-16.8388693379274,18.2670726818203,
5.17088334409471));
#195579=CARTESIAN_POINT('Ctrl Pts',(-16.8261995589176,18.2929496688726,
5.16928315807119));
#195580=CARTESIAN_POINT('Ctrl Pts',(-16.7847811144197,18.3821062485957,
5.16377640171326));
#195581=CARTESIAN_POINT('Ctrl Pts',(-16.7586242460807,18.4465339742871,
5.15980631393645));
#195582=CARTESIAN_POINT('Ctrl Pts',(-16.7314405158915,18.5242614976182,
5.15497298446821));
#195583=CARTESIAN_POINT('Ctrl Pts',(-16.7273073673253,18.5364342692398,
5.1542148743871));
#195584=CARTESIAN_POINT('Ctrl Pts',(-16.7207454755999,18.556354200685,5.15297205301375));
#195585=CARTESIAN_POINT('Ctrl Pts',(-16.71824994359,18.5640791316891,5.15248954647548));
#195586=CARTESIAN_POINT('Ctrl Pts',(-16.713869394972,18.577910606753,5.15162457602174));
#195587=CARTESIAN_POINT('Ctrl Pts',(-16.7119674729204,18.5840117231868,
5.15124267320694));
#195588=CARTESIAN_POINT('Ctrl Pts',(-16.7080022488629,18.5969373460737,
5.15043278364849));
#195589=CARTESIAN_POINT('Ctrl Pts',(-16.7059457420443,18.6037638388475,
5.1500045796847));
#195590=CARTESIAN_POINT('Ctrl Pts',(-16.7005615631578,18.6219688739903,
5.14886131912339));
#195591=CARTESIAN_POINT('Ctrl Pts',(-16.6972949569897,18.6333650783994,
5.14814428039488));
#195592=CARTESIAN_POINT('Ctrl Pts',(-16.6821695114451,18.6878570807787,
5.14470875554201));
#195593=CARTESIAN_POINT('Ctrl Pts',(-16.6715825164489,18.7312912174133,
5.14194941235913));
#195594=CARTESIAN_POINT('Ctrl Pts',(-16.6272657512225,18.9418712911597,
5.12846151811008));
#195595=CARTESIAN_POINT('Ctrl Pts',(-16.6124427002331,19.1123276711236,
5.11714332292881));
#195596=CARTESIAN_POINT('Ctrl Pts',(-16.621593303117,19.3824338143902,5.09933685585448));
#195597=CARTESIAN_POINT('Ctrl Pts',(-16.6320240135644,19.4818381270174,
5.09283065032773));
#195598=CARTESIAN_POINT('Ctrl Pts',(-16.6511231033879,19.5896909190883,
5.08606333908144));
#195599=CARTESIAN_POINT('Ctrl Pts',(-16.6528790946176,19.599225146048,5.08546769257861));
#195600=CARTESIAN_POINT('Ctrl Pts',(-16.6555684523757,19.6132842780257,
5.08459351685813));
#195601=CARTESIAN_POINT('Ctrl Pts',(-16.6564512068669,19.6178185733118,
5.08431222206554));
#195602=CARTESIAN_POINT('Ctrl Pts',(-16.6580435817937,19.6258574875128,
5.08381469282955));
#195603=CARTESIAN_POINT('Ctrl Pts',(-16.658747245999,19.6293632308514,5.08359812353072));
#195604=CARTESIAN_POINT('Ctrl Pts',(-16.6602738691419,19.6368704290137,
5.08313523258017));
#195605=CARTESIAN_POINT('Ctrl Pts',(-16.661099526576,19.6408712784538,5.08288906713493));
#195606=CARTESIAN_POINT('Ctrl Pts',(-16.6633976410968,19.6518465506029,
5.08221515815609));
#195607=CARTESIAN_POINT('Ctrl Pts',(-16.6648937659527,19.6588160396763,
5.08178874668404));
#195608=CARTESIAN_POINT('Ctrl Pts',(-16.6730678008468,19.6959779764364,
5.07952262902255));
#195609=CARTESIAN_POINT('Ctrl Pts',(-16.6803717895789,19.7260306471612,
5.07771665357997));
#195610=CARTESIAN_POINT('Ctrl Pts',(-16.7044696619843,19.8164967108193,
5.07233159790743));
#195611=CARTESIAN_POINT('Ctrl Pts',(-16.7232918049739,19.8763370294956,
5.06883925126178));
#195612=CARTESIAN_POINT('Ctrl Pts',(-16.790731393191,20.0615675883191,5.05800552873976));
#195613=CARTESIAN_POINT('Ctrl Pts',(-16.8486437203579,20.1832090829031,
5.05083714358614));
#195614=CARTESIAN_POINT('Ctrl Pts',(-16.9386589113094,20.3335435202024,
5.04111267647721));
#195615=CARTESIAN_POINT('Ctrl Pts',(-16.9606248620693,20.3679329946825,
5.03882559446556));
#195616=CARTESIAN_POINT('Ctrl Pts',(-17.0109103046547,20.4418590277526,
5.0337442185717));
#195617=CARTESIAN_POINT('Ctrl Pts',(-17.039625252565,20.4810967389569,5.03093809825814));
#195618=CARTESIAN_POINT('Ctrl Pts',(-17.0774530845912,20.5292185647056,
5.02733816105284));
#195619=CARTESIAN_POINT('Ctrl Pts',(-17.0853307458046,20.5390578101946,
5.02659344170211));
#195620=CARTESIAN_POINT('Ctrl Pts',(-17.0979524461682,20.5545370122096,
5.02540774250612));
#195621=CARTESIAN_POINT('Ctrl Pts',(-17.1026389595176,20.5602236490171,
5.0249690860262));
#195622=CARTESIAN_POINT('Ctrl Pts',(-17.1114263488112,20.5707735892956,
5.024149493574));
#195623=CARTESIAN_POINT('Ctrl Pts',(-17.1155196515059,20.5756431137293,
5.02376886934872));
#195624=CARTESIAN_POINT('Ctrl Pts',(-17.1246595324915,20.5864172426741,
5.02292148873999));
#195625=CARTESIAN_POINT('Ctrl Pts',(-17.1297167666524,20.5923126497999,
5.02245429618397));
#195626=CARTESIAN_POINT('Ctrl Pts',(-17.1445047884387,20.6093608418579,
5.02109291545512));
#195627=CARTESIAN_POINT('Ctrl Pts',(-17.1543200885094,20.6204394032361,
5.02019521998889));
#195628=CARTESIAN_POINT('Ctrl Pts',(-17.2331999161843,20.7076122787318,
5.01302595550519));
#195629=CARTESIAN_POINT('Ctrl Pts',(-17.3075955090041,20.7786779026841,
5.00652387157226));
#195630=CARTESIAN_POINT('Ctrl Pts',(-17.5065788343861,20.9428249866548,
4.98977988397894));
#195631=CARTESIAN_POINT('Ctrl Pts',(-17.6368012799828,21.0281218309275,
4.97934997649047));
#195632=CARTESIAN_POINT('Ctrl Pts',(-17.8225521353499,21.1224852809525,
4.96588653368759));
#195633=CARTESIAN_POINT('Ctrl Pts',(-17.8708260118443,21.1447644328443,
4.96250866569724));
#195634=CARTESIAN_POINT('Ctrl Pts',(-17.927930024996,21.1685535829485,4.95869269202706));
#195635=CARTESIAN_POINT('Ctrl Pts',(-17.9359894236675,21.1718528656594,
4.95815821153822));
#195636=CARTESIAN_POINT('Ctrl Pts',(-17.9482261428433,21.1767742804217,
4.95735312975509));
#195637=CARTESIAN_POINT('Ctrl Pts',(-17.9523885185259,21.1784329897204,
4.95708039841341));
#195638=CARTESIAN_POINT('Ctrl Pts',(-17.9598709084113,21.1813872334743,
4.95659218076007));
#195639=CARTESIAN_POINT('Ctrl Pts',(-17.9631889406447,21.1826876049821,
4.95637640718105));
#195640=CARTESIAN_POINT('Ctrl Pts',(-17.9704075447413,21.185495644199,4.95590855402465));
#195641=CARTESIAN_POINT('Ctrl Pts',(-17.9743092922424,21.1870001305491,
4.95565666615287));
#195642=CARTESIAN_POINT('Ctrl Pts',(-17.9852859597766,21.1911953387302,
4.95495075583882));
#195643=CARTESIAN_POINT('Ctrl Pts',(-17.992370971887,21.1938597232629,4.95449828370537));
#195644=CARTESIAN_POINT('Ctrl Pts',(-18.0349027137804,21.2095943235298,
4.95180013023445));
#195645=CARTESIAN_POINT('Ctrl Pts',(-18.0706822325096,21.2217526508862,
4.94960525857077));
#195646=CARTESIAN_POINT('Ctrl Pts',(-18.1897098418822,21.2586762774794,
4.94248968232339));
#195647=CARTESIAN_POINT('Ctrl Pts',(-18.2741606569895,21.2792794972006,
4.93773445267811));
#195648=CARTESIAN_POINT('Ctrl Pts',(-18.5325898067884,21.3257100581067,
4.92344744838294));
#195649=CARTESIAN_POINT('Ctrl Pts',(-18.708709659957,21.3351276809138,4.91400184991385));
#195650=CARTESIAN_POINT('Ctrl Pts',(-18.9068829755556,21.3210541231441,
4.90245711757418));
#195651=CARTESIAN_POINT('Ctrl Pts',(-18.9297731782077,21.3190535400526,
4.90111100529415));
#195652=CARTESIAN_POINT('Ctrl Pts',(-18.9621183921039,21.3156952470103,
4.89918922482309));
#195653=CARTESIAN_POINT('Ctrl Pts',(-18.9716042424459,21.31464547941,4.89862323096034));
#195654=CARTESIAN_POINT('Ctrl Pts',(-18.9870082007834,21.3128352572332,
4.89770010637923));
#195655=CARTESIAN_POINT('Ctrl Pts',(-18.9929308300284,21.3121138527817,
4.89734421060249));
#195656=CARTESIAN_POINT('Ctrl Pts',(-19.0053240500873,21.31055110342,4.89659743474413));
#195657=CARTESIAN_POINT('Ctrl Pts',(-19.0117939501177,21.3097048615339,
4.89620640354894));
#195658=CARTESIAN_POINT('Ctrl Pts',(-19.0271804165713,21.3076199660945,
4.89527362367147));
#195659=CARTESIAN_POINT('Ctrl Pts',(-19.0360931435943,21.3063543298372,
4.89473102680214));
#195660=CARTESIAN_POINT('Ctrl Pts',(-19.0661121620077,21.3018960227297,
4.89289567225049));
#195661=CARTESIAN_POINT('Ctrl Pts',(-19.08717762895,21.2984410593016,4.89159464672465));
#195662=CARTESIAN_POINT('Ctrl Pts',(-19.2017081389943,21.2778735867718,
4.88444734441149));
#195663=CARTESIAN_POINT('Ctrl Pts',(-19.2939803393657,21.2548040864345,
4.87841292982892));
#195664=CARTESIAN_POINT('Ctrl Pts',(-19.5249047939371,21.1802545194414,
4.86264634674662));
#195665=CARTESIAN_POINT('Ctrl Pts',(-19.6602866100661,21.1203149804039,
4.85274046139437));
#195666=CARTESIAN_POINT('Ctrl Pts',(-19.8387282544129,21.017832256677,4.83940174197861));
#195667=CARTESIAN_POINT('Ctrl Pts',(-19.8879220787456,20.9868188126646,
4.83569642376248));
#195668=CARTESIAN_POINT('Ctrl Pts',(-19.9431004681535,20.948769864667,4.83156047351002));
#195669=CARTESIAN_POINT('Ctrl Pts',(-19.9503880085439,20.9436766183176,
4.83101466060256));
#195670=CARTESIAN_POINT('Ctrl Pts',(-19.9613316517685,20.9359250548254,
4.83019593874698));
#195671=CARTESIAN_POINT('Ctrl Pts',(-19.9650115766698,20.9333007655976,
4.82992079274058));
#195672=CARTESIAN_POINT('Ctrl Pts',(-19.9714971904929,20.9286442311516,
4.82943618907267));
#195673=CARTESIAN_POINT('Ctrl Pts',(-19.9743063144003,20.9266168710783,
4.82922640143909));
#195674=CARTESIAN_POINT('Ctrl Pts',(-19.9771213840895,20.9245746918649,
4.82901628298026));
#195675=CARTESIAN_POINT('Ctrl Pts',(-19.9771322559639,20.9245668047563,
4.82901547149881));
#195676=CARTESIAN_POINT('Ctrl Pts',(-19.9771538170015,20.9245511627754,
4.82901386217678));
#195677=CARTESIAN_POINT('Ctrl Pts',(-19.9771645062719,20.9245434078307,
4.82901306432817));
#195678=CARTESIAN_POINT('Ctrl Pts',(-19.977185704677,20.924528028325,4.82901148207944));
#195679=CARTESIAN_POINT('Ctrl Pts',(-19.9771962144594,20.9245204032991,
4.82901069763093));
#195680=CARTESIAN_POINT('Ctrl Pts',(-19.9772164300653,20.9245057362493,
4.82900918874423));
#195681=CARTESIAN_POINT('Ctrl Pts',(-19.9772261348795,20.9244986949795,
4.82900846438115));
#195682=CARTESIAN_POINT('Ctrl Pts',(-19.9772455073426,20.9244846391535,
4.8290070184316));
#195683=CARTESIAN_POINT('Ctrl Pts',(-19.9772551754023,20.9244776243004,
4.82900629681446));
#195684=CARTESIAN_POINT('Ctrl Pts',(-19.977274474704,20.9244636210586,4.82900485633081));
#195685=CARTESIAN_POINT('Ctrl Pts',(-19.9772841061407,20.9244566325296,
4.82900413744976));
#195686=CARTESIAN_POINT('Ctrl Pts',(-19.9773033339959,20.9244426806331,
4.82900270230395));
#195687=CARTESIAN_POINT('Ctrl Pts',(-19.9773129298098,20.9244357177053,
4.82900198608432));
#195688=CARTESIAN_POINT('Ctrl Pts',(-19.9773320848734,20.9244218181358,
4.8290005563767));
#195689=CARTESIAN_POINT('Ctrl Pts',(-19.9773416447492,20.9244148810407,
4.82899984284198));
#195690=CARTESIAN_POINT('Ctrl Pts',(-19.9806435439003,20.9220188256811,
4.82875339450335));
#195691=CARTESIAN_POINT('Ctrl Pts',(-19.9839290220744,20.9196201999858,
4.82850832208095));
#195692=CARTESIAN_POINT('Ctrl Pts',(-19.9907205618502,20.9146318346662,
4.82800198893054));
#195693=CARTESIAN_POINT('Ctrl Pts',(-19.9942255837985,20.9120407042059,
4.82774082473892));
#195694=CARTESIAN_POINT('Ctrl Pts',(-20.00311784422,20.9054244216732,4.82707855560906));
#195695=CARTESIAN_POINT('Ctrl Pts',(-20.0084939965409,20.9013843582822,
4.82667844274994));
#195696=CARTESIAN_POINT('Ctrl Pts',(-20.0239444708727,20.8896580437905,
4.82552910110643));
#195697=CARTESIAN_POINT('Ctrl Pts',(-20.0339693309556,20.8819067361304,
4.82478402985981));
#195698=CARTESIAN_POINT('Ctrl Pts',(-20.0681294779319,20.8550002796233,
4.82224515033091));
#195699=CARTESIAN_POINT('Ctrl Pts',(-20.0919168302753,20.8354077246413,
4.82047716128688));
#195700=CARTESIAN_POINT('Ctrl Pts',(-20.2105264225643,20.7332874393822,
4.81161260447306));
#195701=CARTESIAN_POINT('Ctrl Pts',(-20.298297160638,20.6429457611615,4.80487727607783));
#195702=CARTESIAN_POINT('Ctrl Pts',(-20.4010751592956,20.516352032551,4.79600101221062));
#195703=CARTESIAN_POINT('Ctrl Pts',(-20.4238409329932,20.4867433303909,
4.7939614558361));
#195704=CARTESIAN_POINT('Ctrl Pts',(-20.5058258214295,20.3740679454682,
4.78628948996169));
#195705=CARTESIAN_POINT('Ctrl Pts',(-20.5597935310681,20.2873679217427,
4.78055349557371));
#195706=CARTESIAN_POINT('Ctrl Pts',(-20.6138280496349,20.1847206731101,
4.7737553243962));
#195707=CARTESIAN_POINT('Ctrl Pts',(-20.6202333679171,20.1722539274884,
4.77292973281338));
#195708=CARTESIAN_POINT('Ctrl Pts',(-20.630267537414,20.1522377847369,4.77160387778149));
#195709=CARTESIAN_POINT('Ctrl Pts',(-20.6339762618876,20.1447287304431,
4.77110641393081));
#195710=CARTESIAN_POINT('Ctrl Pts',(-20.6404595832993,20.1314033804103,
4.77022342143287));
#195711=CARTESIAN_POINT('Ctrl Pts',(-20.6432523783057,20.1255960200773,
4.76983853270947));
#195712=CARTESIAN_POINT('Ctrl Pts',(-20.6489941600182,20.1135156033417,
4.76903770671365));
#195713=CARTESIAN_POINT('Ctrl Pts',(-20.6519389351825,20.1072406408504,
4.76862162915387));
#195714=CARTESIAN_POINT('Ctrl Pts',(-20.6594606048486,20.091006023374,4.76754483042365));
#195715=CARTESIAN_POINT('Ctrl Pts',(-20.6639910183447,20.081025174366,4.76688251676034));
#195716=CARTESIAN_POINT('Ctrl Pts',(-20.6829282360487,20.0384291676282,
4.76405428130858));
#195717=CARTESIAN_POINT('Ctrl Pts',(-20.696586664511,20.0054895457633,4.76186301747051));
#195718=CARTESIAN_POINT('Ctrl Pts',(-20.7139016543125,19.9605563628427,
4.75886649057087));
#195719=CARTESIAN_POINT('Ctrl Pts',(-20.7182932737024,19.9488519165805,
4.75808528715504));
#195720=CARTESIAN_POINT('Ctrl Pts',(-20.7225806084094,19.937110297309,4.75730094873459));
#195721=CARTESIAN_POINT('Ctrl Pts',(-20.7225805792317,19.9371103772171,
4.53222349041431));
#195722=CARTESIAN_POINT('Ctrl Pts',(-20.713233383926,19.9627093104351,4.53397185385458));
#195723=CARTESIAN_POINT('Ctrl Pts',(-20.7033905938547,19.988131302222,4.53573318148791));
#195724=CARTESIAN_POINT('Ctrl Pts',(-20.6611588232326,20.0912449146023,
4.54297538962527));
#195725=CARTESIAN_POINT('Ctrl Pts',(-20.6246459300555,20.1671532397865,
4.54854123331881));
#195726=CARTESIAN_POINT('Ctrl Pts',(-20.5387210126306,20.3215080464049,
4.56021214034759));
#195727=CARTESIAN_POINT('Ctrl Pts',(-20.4884753735683,20.3993032970082,
4.56630397075444));
#195728=CARTESIAN_POINT('Ctrl Pts',(-20.414586493627,20.498750912961,4.57416792408563));
#195729=CARTESIAN_POINT('Ctrl Pts',(-20.3953160225471,20.5235176923286,
4.57613279091625));
#195730=CARTESIAN_POINT('Ctrl Pts',(-20.3709791670432,20.5534006409387,
4.57850227352807));
#195731=CARTESIAN_POINT('Ctrl Pts',(-20.3664291607147,20.5589300103313,
4.5789406521064));
#195732=CARTESIAN_POINT('Ctrl Pts',(-20.3592348472954,20.5675830007218,
4.57962644155925));
#195733=CARTESIAN_POINT('Ctrl Pts',(-20.3566094380522,20.5707221623957,
4.5798751854453));
#195734=CARTESIAN_POINT('Ctrl Pts',(-20.3516737613268,20.5765890227675,
4.58033994428915));
#195735=CARTESIAN_POINT('Ctrl Pts',(-20.3493657145128,20.579318451889,4.58055610820751));
#195736=CARTESIAN_POINT('Ctrl Pts',(-20.3440663781821,20.5855531972313,
4.58104977617908));
#195737=CARTESIAN_POINT('Ctrl Pts',(-20.3410705547958,20.5890545950724,
4.58132694207588));
#195738=CARTESIAN_POINT('Ctrl Pts',(-20.3331962608604,20.5981971526258,
4.58205054214663));
#195739=CARTESIAN_POINT('Ctrl Pts',(-20.3282993228531,20.6038224200755,
4.58249564882668));
#195740=CARTESIAN_POINT('Ctrl Pts',(-20.2953704986368,20.6412475904341,
4.58545713018297));
#195741=CARTESIAN_POINT('Ctrl Pts',(-20.2664165505378,20.6722275878557,
4.58790944825523));
#195742=CARTESIAN_POINT('Ctrl Pts',(-20.1846186047802,20.7546415068214,
4.59450432799614));
#195743=CARTESIAN_POINT('Ctrl Pts',(-20.1299864055226,20.8042190182788,
4.59855349281472));
#195744=CARTESIAN_POINT('Ctrl Pts',(-20.0037168815403,20.907313456531,4.60743693862741));
#195745=CARTESIAN_POINT('Ctrl Pts',(-19.9310563503755,20.9593467060511,
4.61224964925924));
#195746=CARTESIAN_POINT('Ctrl Pts',(-19.794950098171,21.0443414970298,4.62107285801276));
#195747=CARTESIAN_POINT('Ctrl Pts',(-19.7327130127349,21.0789741100068,
4.62504159397318));
#195748=CARTESIAN_POINT('Ctrl Pts',(-19.6444797582201,21.122400948149,4.63066725320784));
#195749=CARTESIAN_POINT('Ctrl Pts',(-19.6198784643942,21.1339264747538,
4.63223545290629));
#195750=CARTESIAN_POINT('Ctrl Pts',(-19.5768896153128,21.1530663830061,
4.63497946636038));
#195751=CARTESIAN_POINT('Ctrl Pts',(-19.5586036068405,21.1609009183432,
4.6361478028167));
#195752=CARTESIAN_POINT('Ctrl Pts',(-19.5321442687545,21.1717985170344,
4.63784107725754));
#195753=CARTESIAN_POINT('Ctrl Pts',(-19.5240578219808,21.1750707045843,
4.63835893208218));
#195754=CARTESIAN_POINT('Ctrl Pts',(-19.5099047252628,21.180696219467,4.63926601681111));
#195755=CARTESIAN_POINT('Ctrl Pts',(-19.5038469813823,21.1830717439957,
4.63965449265329));
#195756=CARTESIAN_POINT('Ctrl Pts',(-19.492193445895,21.1875797627123,4.64040229919977));
#195757=CARTESIAN_POINT('Ctrl Pts',(-19.4865993615355,21.1897165182595,
4.64076148220421));
#195758=CARTESIAN_POINT('Ctrl Pts',(-19.4719543225548,21.1952393512042,
4.64170239407505));
#195759=CARTESIAN_POINT('Ctrl Pts',(-19.4628891923829,21.1985872120307,
4.64228539472868));
#195760=CARTESIAN_POINT('Ctrl Pts',(-19.4315146219173,21.2099307115649,
4.64430536920633));
#195761=CARTESIAN_POINT('Ctrl Pts',(-19.4090946836316,21.2176134988925,
4.64575266831049));
#195762=CARTESIAN_POINT('Ctrl Pts',(-19.230923269086,21.2753447296468,4.6572887560153));
#195763=CARTESIAN_POINT('Ctrl Pts',(-19.0700025548621,21.307553127075,4.66797862973147));
#195764=CARTESIAN_POINT('Ctrl Pts',(-18.7784687148216,21.3314590686806,
4.68730861918814));
#195765=CARTESIAN_POINT('Ctrl Pts',(-18.6492150723303,21.3302315799233,
4.69584464570825));
#195766=CARTESIAN_POINT('Ctrl Pts',(-18.5089911857911,21.3160421626598,
4.7045850312468));
#195767=CARTESIAN_POINT('Ctrl Pts',(-18.4971256831738,21.314740013913,4.70532038278404));
#195768=CARTESIAN_POINT('Ctrl Pts',(-18.4802789760351,21.3127468725763,
4.70635779451977));
#195769=CARTESIAN_POINT('Ctrl Pts',(-18.4752884926774,21.3121384132326,
4.70666427576211));
#195770=CARTESIAN_POINT('Ctrl Pts',(-18.4666941808978,21.3110594770468,
4.70719059281528));
#195771=CARTESIAN_POINT('Ctrl Pts',(-18.4630893251251,21.3105974888244,
4.70741090303321));
#195772=CARTESIAN_POINT('Ctrl Pts',(-18.4561039183034,21.3096839684002,
4.70783691937066));
#195773=CARTESIAN_POINT('Ctrl Pts',(-18.4527232689363,21.309233550486,4.70804268954486));
#195774=CARTESIAN_POINT('Ctrl Pts',(-18.4436089685325,21.3079967910042,
4.70859639529961));
#195775=CARTESIAN_POINT('Ctrl Pts',(-18.4378773803075,21.307195097918,4.7089434702055));
#195776=CARTESIAN_POINT('Ctrl Pts',(-18.4166388038024,21.3041355503146,
4.71022562629459));
#195777=CARTESIAN_POINT('Ctrl Pts',(-18.4011533056921,21.3017289808452,
4.71115267728231));
#195778=CARTESIAN_POINT('Ctrl Pts',(-18.2523765728645,21.276912948643,4.71999644537115));
#195779=CARTESIAN_POINT('Ctrl Pts',(-18.1214744451817,21.2419554305564,
4.72730362917144));
#195780=CARTESIAN_POINT('Ctrl Pts',(-17.8486617835098,21.140295868747,4.74311376677318));
#195781=CARTESIAN_POINT('Ctrl Pts',(-17.7090202495407,21.069874744594,4.75160379699766));
#195782=CARTESIAN_POINT('Ctrl Pts',(-17.5605587937187,20.9731513297329,
4.76192279316519));
#195783=CARTESIAN_POINT('Ctrl Pts',(-17.5429107640739,20.9612708238939,
4.76317118101039));
#195784=CARTESIAN_POINT('Ctrl Pts',(-17.51806424711,20.9439945362681,4.76496137328442));
#195785=CARTESIAN_POINT('Ctrl Pts',(-17.5107161160549,20.9388154859171,
4.76549493859828));
#195786=CARTESIAN_POINT('Ctrl Pts',(-17.4980937156258,20.9297981857111,
4.76641874720204));
#195787=CARTESIAN_POINT('Ctrl Pts',(-17.4928037498933,20.9259820448658,
4.76680813617712));
#195788=CARTESIAN_POINT('Ctrl Pts',(-17.4827068992902,20.9186270684645,
4.76755567312621));
#195789=CARTESIAN_POINT('Ctrl Pts',(-17.4778971727331,20.9150922260942,
4.76791366367569));
#195790=CARTESIAN_POINT('Ctrl Pts',(-17.4654248415636,20.9058443649018,
4.76884696658883));
#195791=CARTESIAN_POINT('Ctrl Pts',(-17.4577859267834,20.9000997568169,
4.76942351087295));
#195792=CARTESIAN_POINT('Ctrl Pts',(-17.4318482850916,20.8803177645991,
4.77139821373091));
#195793=CARTESIAN_POINT('Ctrl Pts',(-17.4137406663534,20.8660335687672,
4.77280608768999));
#195794=CARTESIAN_POINT('Ctrl Pts',(-17.2606270958368,20.7411380080771,
4.78496908566283));
#195795=CARTESIAN_POINT('Ctrl Pts',(-17.1395693085175,20.6145375798855,
4.79641924003365));
#195796=CARTESIAN_POINT('Ctrl Pts',(-16.9831019959069,20.4042031917327,
4.81374051816536));
#195797=CARTESIAN_POINT('Ctrl Pts',(-16.9351842757812,20.3306613782542,
4.81952114923206));
#195798=CARTESIAN_POINT('Ctrl Pts',(-16.873238946879,20.2212973608538,4.82754699855225));
#195799=CARTESIAN_POINT('Ctrl Pts',(-16.8554062532793,20.1877386570312,
4.82993711797288));
#195800=CARTESIAN_POINT('Ctrl Pts',(-16.8351092762402,20.1469276131491,
4.83274195447701));
#195801=CARTESIAN_POINT('Ctrl Pts',(-16.831769646756,20.1401211788707,4.83320640702422));
#195802=CARTESIAN_POINT('Ctrl Pts',(-16.8266436340144,20.1295304578039,
4.83392375458381));
#195803=CARTESIAN_POINT('Ctrl Pts',(-16.8248318236553,20.1257586479018,
4.83417818853336));
#195804=CARTESIAN_POINT('Ctrl Pts',(-16.821497732587,20.118764714034,4.83464801097033));
#195805=CARTESIAN_POINT('Ctrl Pts',(-16.8199724173638,20.115544146028,4.83486358236687));
#195806=CARTESIAN_POINT('Ctrl Pts',(-16.8165490113443,20.1082684947465,
4.83534885497302));
#195807=CARTESIAN_POINT('Ctrl Pts',(-16.8146556536927,20.1042112441671,
4.83561826209147));
#195808=CARTESIAN_POINT('Ctrl Pts',(-16.8091242923405,20.0922593653788,
4.8364084348112));
#195809=CARTESIAN_POINT('Ctrl Pts',(-16.8055219729698,20.0843481918064,
4.83692705227377));
#195810=CARTESIAN_POINT('Ctrl Pts',(-16.7804002270661,20.0282641025753,
4.84057408257743));
#195811=CARTESIAN_POINT('Ctrl Pts',(-16.7606376636852,19.9793194423272,
4.84360334408258));
#195812=CARTESIAN_POINT('Ctrl Pts',(-16.737302674407,19.9146645052183,4.84747088431362));
#195813=CARTESIAN_POINT('Ctrl Pts',(-16.7320521465366,19.8995846034768,
4.8483636327534));
#195814=CARTESIAN_POINT('Ctrl Pts',(-16.7108619521275,19.8364328889333,
4.85206901272793));
#195815=CARTESIAN_POINT('Ctrl Pts',(-16.6964788235245,19.7878549712471,
4.85483964212562));
#195816=CARTESIAN_POINT('Ctrl Pts',(-16.6565744201966,19.6328550733939,
4.86355394811894));
#195817=CARTESIAN_POINT('Ctrl Pts',(-16.6375521563209,19.5249495248811,
4.86944480571278));
#195818=CARTESIAN_POINT('Ctrl Pts',(-16.6216101786746,19.3611428764858,
4.87859557618059));
#195819=CARTESIAN_POINT('Ctrl Pts',(-16.618414858479,19.3060394768938,4.88170678099319));
#195820=CARTESIAN_POINT('Ctrl Pts',(-16.6167287868548,19.2165444817433,
4.88685635292515));
#195821=CARTESIAN_POINT('Ctrl Pts',(-16.6169174162056,19.1822029936109,
4.88885522061801));
#195822=CARTESIAN_POINT('Ctrl Pts',(-16.6182634844682,19.1370749970996,
4.89151787542284));
#195823=CARTESIAN_POINT('Ctrl Pts',(-16.6186686424979,19.1262701315257,
4.89215808886423));
#195824=CARTESIAN_POINT('Ctrl Pts',(-16.6194678676687,19.1085770685749,
4.89321104958199));
#195825=CARTESIAN_POINT('Ctrl Pts',(-16.6198128721122,19.1016867707712,
4.89362225411417));
#195826=CARTESIAN_POINT('Ctrl Pts',(-16.620545944099,19.088351558327,4.89442034858492));
#195827=CARTESIAN_POINT('Ctrl Pts',(-16.6209298286186,19.0819064833734,
4.89480710281834));
#195828=CARTESIAN_POINT('Ctrl Pts',(-16.6218843617584,19.0670278472426,
4.89570234673728));
#195829=CARTESIAN_POINT('Ctrl Pts',(-16.6224760472178,19.0585957885613,
4.89621149193062));
#195830=CARTESIAN_POINT('Ctrl Pts',(-16.6242033429986,19.0359254990372,
4.89758528708301));
#195831=CARTESIAN_POINT('Ctrl Pts',(-16.6254325647706,19.0216950339365,
4.898452861707));
#195832=CARTESIAN_POINT('Ctrl Pts',(-16.6403645156076,18.86709465359,4.9079366001282));
#195833=CARTESIAN_POINT('Ctrl Pts',(-16.6679152092711,18.7284435548166,
4.91700231892608));
#195834=CARTESIAN_POINT('Ctrl Pts',(-16.7372072757883,18.5011836776805,
4.9326328377619));
#195835=CARTESIAN_POINT('Ctrl Pts',(-16.7716712806174,18.4108209019477,
4.93905852807083));
#195836=CARTESIAN_POINT('Ctrl Pts',(-16.8327336459496,18.2786504652834,
4.94855953930433));
#195837=CARTESIAN_POINT('Ctrl Pts',(-16.8548209919588,18.2348973958161,
4.95172133382279));
#195838=CARTESIAN_POINT('Ctrl Pts',(-16.8910494056186,18.1689291004062,
4.95647396021502));
#195839=CARTESIAN_POINT('Ctrl Pts',(-16.9041185930277,18.146146565785,4.95811246632818));
#195840=CARTESIAN_POINT('Ctrl Pts',(-16.9210812293672,18.1178118972069,
4.9601410656946));
#195841=CARTESIAN_POINT('Ctrl Pts',(-16.9245812673146,18.1120284127145,
4.96055463808154));
#195842=CARTESIAN_POINT('Ctrl Pts',(-16.9301981844756,18.1028465637965,
4.96121031500938));
#195843=CARTESIAN_POINT('Ctrl Pts',(-16.9322970701134,18.0994373247938,
4.96145356817236));
#195844=CARTESIAN_POINT('Ctrl Pts',(-16.936297953282,18.0929797583861,4.96191390996638));
#195845=CARTESIAN_POINT('Ctrl Pts',(-16.9381980157753,18.0899303576313,
4.96213111362045));
#195846=CARTESIAN_POINT('Ctrl Pts',(-16.9425917585578,18.0829186954831,
4.96263015238819));
#195847=CARTESIAN_POINT('Ctrl Pts',(-16.945090824282,18.0789598597652,4.96291162780119));
#195848=CARTESIAN_POINT('Ctrl Pts',(-16.9518285652205,18.0683644560912,
4.96366429101311));
#195849=CARTESIAN_POINT('Ctrl Pts',(-16.9560912175355,18.0617431206457,
4.96413393484555));
#195850=CARTESIAN_POINT('Ctrl Pts',(-16.9884162903409,18.0121416767099,
4.96764793965742));
#195851=CARTESIAN_POINT('Ctrl Pts',(-17.0179990733392,17.9701674146237,
4.97059806226464));
#195852=CARTESIAN_POINT('Ctrl Pts',(-17.0626452480492,17.9114753802039,
4.97475229737124));
#195853=CARTESIAN_POINT('Ctrl Pts',(-17.0764918968775,17.8938599612684,
4.97600306807218));
#195854=CARTESIAN_POINT('Ctrl Pts',(-17.1195448496476,17.8408432492152,
4.97979050055642));
#195855=CARTESIAN_POINT('Ctrl Pts',(-17.1496253632879,17.8061682644905,
4.98229989190679));
#195856=CARTESIAN_POINT('Ctrl Pts',(-17.255114675471,17.6922685963979,4.99075210937858));
#195857=CARTESIAN_POINT('Ctrl Pts',(-17.3355233671548,17.6179183626198,
4.99664031276523));
#195858=CARTESIAN_POINT('Ctrl Pts',(-17.4645505988168,17.5159411090446,
5.00578491209592));
#195859=CARTESIAN_POINT('Ctrl Pts',(-17.5091045416287,17.483470869543,5.00889257928465));
#195860=CARTESIAN_POINT('Ctrl Pts',(-17.5833667270592,17.4336679624074,
5.0140368177582));
#195861=CARTESIAN_POINT('Ctrl Pts',(-17.6123201843384,17.4152549470559,
5.01603399682121));
#195862=CARTESIAN_POINT('Ctrl Pts',(-17.6509662748633,17.3919772442362,
5.01869472080579));
#195863=CARTESIAN_POINT('Ctrl Pts',(-17.6602678796239,17.3864712490936,
5.0193347356674));
#195864=CARTESIAN_POINT('Ctrl Pts',(-17.6755740158714,17.377568511949,5.02038745294817));
#195865=CARTESIAN_POINT('Ctrl Pts',(-17.6815537795617,17.3741294175667,
5.02079861402289));
#195866=CARTESIAN_POINT('Ctrl Pts',(-17.6931630205272,17.3675279842937,
5.02159668358584));
#195867=CARTESIAN_POINT('Ctrl Pts',(-17.6987903733775,17.3643620500906,
5.02198345668368));
#195868=CARTESIAN_POINT('Ctrl Pts',(-17.7118195196232,17.3571101579072,
5.0228788308503));
#195869=CARTESIAN_POINT('Ctrl Pts',(-17.7192314456833,17.3530427187341,
5.02338808802767));
#195870=CARTESIAN_POINT('Ctrl Pts',(-17.7392357772361,17.3422203616659,
5.02476238128829));
#195871=CARTESIAN_POINT('Ctrl Pts',(-17.7518723723176,17.3355484536332,
5.02563034533766));
#195872=CARTESIAN_POINT('Ctrl Pts',(-17.8684363630794,17.2755057766444,
5.03363648433267));
#195873=CARTESIAN_POINT('Ctrl Pts',(-17.976530576028,17.2307044244463,5.04107633799039));
#195874=CARTESIAN_POINT('Ctrl Pts',(-18.2426514564894,17.1453947565814,
5.05933040839353));
#195875=CARTESIAN_POINT('Ctrl Pts',(-18.4027530446898,17.1137580179814,
5.07028453074278));
#195876=CARTESIAN_POINT('Ctrl Pts',(-18.5973725200904,17.0981622479942,
5.0826915602721));
#195877=CARTESIAN_POINT('Ctrl Pts',(-18.6299059532684,17.0963096836068,
5.0847336114845));
#195878=CARTESIAN_POINT('Ctrl Pts',(-18.6697115475675,17.0949639705341,
5.08718279188374));
#195879=CARTESIAN_POINT('Ctrl Pts',(-18.6769532641206,17.0947563570008,
5.08762636912633));
#195880=CARTESIAN_POINT('Ctrl Pts',(-18.6883056354449,17.0944892102064,
5.08831845917592));
#195881=CARTESIAN_POINT('Ctrl Pts',(-18.6924155611055,17.0944044710028,
5.0885683450577));
#195882=CARTESIAN_POINT('Ctrl Pts',(-18.7000969193988,17.0942684774893,
5.08903408517602));
#195883=CARTESIAN_POINT('Ctrl Pts',(-18.7036681956824,17.0942142906892,
5.08925009527308));
#195884=CARTESIAN_POINT('Ctrl Pts',(-18.7118190225153,17.094111250438,5.08974191909529));
#195885=CARTESIAN_POINT('Ctrl Pts',(-18.7163985961855,17.094068219032,5.09001740418829));
#195886=CARTESIAN_POINT('Ctrl Pts',(-18.7304693501879,17.0939816681184,
5.09086132563016));
#195887=CARTESIAN_POINT('Ctrl Pts',(-18.7399608629648,17.0939871141838,
5.09142709314652));
#195888=CARTESIAN_POINT('Ctrl Pts',(-18.8249031590651,17.0946071339047,
5.09646148737402));
#195889=CARTESIAN_POINT('Ctrl Pts',(-18.9002795819994,17.0991913405416,
5.10072611330635));
#195890=CARTESIAN_POINT('Ctrl Pts',(-19.0180423249742,17.1126998415495,
5.1072883759256));
#195891=CARTESIAN_POINT('Ctrl Pts',(-19.0606682227336,17.1189121287575,
5.10964260969806));
#195892=CARTESIAN_POINT('Ctrl Pts',(-19.2107261167275,17.1454799597475,
5.11793932390216));
#195893=CARTESIAN_POINT('Ctrl Pts',(-19.3167371133434,17.1728495155747,
5.12382617277009));
#195894=CARTESIAN_POINT('Ctrl Pts',(-19.4722621403519,17.2261343217636,
5.13296762309385));
#195895=CARTESIAN_POINT('Ctrl Pts',(-19.5236485237689,17.2460121341427,
5.13607348535374));
#195896=CARTESIAN_POINT('Ctrl Pts',(-19.6056761766708,17.2814804463411,
5.14121500240233));
#195897=CARTESIAN_POINT('Ctrl Pts',(-19.6368166268502,17.2958532675417,
5.1432113196033));
#195898=CARTESIAN_POINT('Ctrl Pts',(-19.6772926816756,17.3157415176362,
5.1458710580706));
#195899=CARTESIAN_POINT('Ctrl Pts',(-19.6869555650449,17.3205816646126,
5.14651097151932));
#195900=CARTESIAN_POINT('Ctrl Pts',(-19.7027243744774,17.328631899363,5.14756356448092));
#195901=CARTESIAN_POINT('Ctrl Pts',(-19.7088524956181,17.3317982572225,
5.14797470336404));
#195902=CARTESIAN_POINT('Ctrl Pts',(-19.7206869043408,17.3379864802095,
5.14877276022434));
#195903=CARTESIAN_POINT('Ctrl Pts',(-19.7263950627273,17.3410046175037,
5.14915954297188));
#195904=CARTESIAN_POINT('Ctrl Pts',(-19.7395461324536,17.3480353002705,
5.15005498372877));
#195905=CARTESIAN_POINT('Ctrl Pts',(-19.7469789523099,17.3520663982091,
5.15056429815377));
#195906=CARTESIAN_POINT('Ctrl Pts',(-19.7669104229469,17.3630310213209,
5.1519388460782));
#195907=CARTESIAN_POINT('Ctrl Pts',(-19.7793631677644,17.370046681812,5.15280700923223));
#195908=CARTESIAN_POINT('Ctrl Pts',(-19.8931596885263,17.4356845638511,
5.16082846320481));
#195909=CARTESIAN_POINT('Ctrl Pts',(-19.9895317027028,17.5024835750581,
5.16828477314389));
#195910=CARTESIAN_POINT('Ctrl Pts',(-20.2060423060182,17.6808053590924,
5.18660785684195));
#195911=CARTESIAN_POINT('Ctrl Pts',(-20.3197459716108,17.7989751811815,
5.19761657700647));
#195912=CARTESIAN_POINT('Ctrl Pts',(-20.4378942683944,17.9542439776002,
5.21000427536224));
#195913=CARTESIAN_POINT('Ctrl Pts',(-20.4564998273439,17.9798680120139,
5.21198742626012));
#195914=CARTESIAN_POINT('Ctrl Pts',(-20.4786123357413,18.0118051192277,
5.21437581782508));
#195915=CARTESIAN_POINT('Ctrl Pts',(-20.4826700050878,18.0177297955606,
5.21481544872758));
#195916=CARTESIAN_POINT('Ctrl Pts',(-20.488995177713,18.0270668475793,5.21550275631196));
#195917=CARTESIAN_POINT('Ctrl Pts',(-20.4912830116499,18.0304652902939,
5.21575177561123));
#195918=CARTESIAN_POINT('Ctrl Pts',(-20.4955481618066,18.0368407919681,
5.21621676934283));
#195919=CARTESIAN_POINT('Ctrl Pts',(-20.4975277822605,18.039816182837,5.21643289440411));
#195920=CARTESIAN_POINT('Ctrl Pts',(-20.5020388918464,18.0466338002259,
5.21692610958048));
#195921=CARTESIAN_POINT('Ctrl Pts',(-20.5045653910778,18.0504792689952,
5.21720286387093));
#195922=CARTESIAN_POINT('Ctrl Pts',(-20.511141568415,18.0605600304962,5.21792468320672));
#195923=CARTESIAN_POINT('Ctrl Pts',(-20.5151710118547,18.0668085353283,
5.21836843136674));
#195924=CARTESIAN_POINT('Ctrl Pts',(-20.5417163990186,18.1084528422731,
5.22130250108755));
#195925=CARTESIAN_POINT('Ctrl Pts',(-20.5632105518177,18.1444925692471,
5.22373010620223));
#195926=CARTESIAN_POINT('Ctrl Pts',(-20.5941836418223,18.200120543654,5.22734779879829));
#195927=CARTESIAN_POINT('Ctrl Pts',(-20.6044541275495,18.2192531246507,
5.22856960795265));
#195928=CARTESIAN_POINT('Ctrl Pts',(-20.6222719321328,18.2537071279278,
5.23073593038642));
#195929=CARTESIAN_POINT('Ctrl Pts',(-20.6299315080533,18.2689680108981,
5.23168382475274));
#195930=CARTESIAN_POINT('Ctrl Pts',(-20.6957490246493,18.4041575655516,
5.23999255929711));
#195931=CARTESIAN_POINT('Ctrl Pts',(-20.742645368146,18.5292378966341,5.24709271865252));
#195932=CARTESIAN_POINT('Ctrl Pts',(-20.8031161572572,18.7526519636485,
5.25986490638718));
#195933=CARTESIAN_POINT('Ctrl Pts',(-20.8221382508542,18.8490612180803,
5.26540011154393));
#195934=CARTESIAN_POINT('Ctrl Pts',(-20.8362368145887,18.9609907704941,
5.27201872403664));
#195935=CARTESIAN_POINT('Ctrl Pts',(-20.8379188833009,18.9755651773305,
5.27288406086351));
#195936=CARTESIAN_POINT('Ctrl Pts',(-20.8402567481172,18.9978535229694,
5.2742132233605));
#195937=CARTESIAN_POINT('Ctrl Pts',(-20.8410219631316,19.0055557153255,
5.27467360114129));
#195938=CARTESIAN_POINT('Ctrl Pts',(-20.8422815026533,19.0189814911236,
5.27547799829814));
#195939=CARTESIAN_POINT('Ctrl Pts',(-20.8427948027886,19.0247032450434,
5.27582141648292));
#195940=CARTESIAN_POINT('Ctrl Pts',(-20.8438966146373,19.037573578127,5.27659527622887));
#195941=CARTESIAN_POINT('Ctrl Pts',(-20.8444720950536,19.0447231757292,
5.27702612346942));
#195942=CARTESIAN_POINT('Ctrl Pts',(-20.8459169690494,19.0638914689281,
5.27818387553732));
#195943=CARTESIAN_POINT('Ctrl Pts',(-20.8467200885576,19.0759147599919,
5.27891285187492));
#195944=CARTESIAN_POINT('Ctrl Pts',(-20.8498276623778,19.1292856925848,
5.28216148649077));
#195945=CARTESIAN_POINT('Ctrl Pts',(-20.8510211083768,19.1706865674428,
5.28471565814259));
#195946=CARTESIAN_POINT('Ctrl Pts',(-20.8509121657631,19.3815723388986,
5.29790828090238));
#195947=CARTESIAN_POINT('Ctrl Pts',(-20.8304727772938,19.5504051994466,
5.30913945498687));
#195948=CARTESIAN_POINT('Ctrl Pts',(-20.771698414488,19.7902026692572,5.32541888131401));
#195949=CARTESIAN_POINT('Ctrl Pts',(-20.7491431302945,19.8643641701078,
5.33048906851518));
#195950=CARTESIAN_POINT('Ctrl Pts',(-20.7225805912209,19.9371103443827,
5.33540100209138));
#195951=CARTESIAN_POINT('Origin',(-18.734,19.211,0.));
#195952=CARTESIAN_POINT('',(-20.7225806064499,19.9371103026755,6.3535037140067));
#195953=CARTESIAN_POINT('',(-20.7225806064498,19.9371103026755,6.13370788222325));
#195954=CARTESIAN_POINT('',(-20.7225806064498,19.9371103026755,0.));
#195955=CARTESIAN_POINT('',(-20.8509995791047,19.2123349421389,6.31236858093732));
#195956=CARTESIAN_POINT('Ctrl Pts',(-20.7225806064498,19.9371103026756,
6.35350371400671));
#195957=CARTESIAN_POINT('Ctrl Pts',(-20.7235885970627,19.9343497433268,
6.35332822035437));
#195958=CARTESIAN_POINT('Ctrl Pts',(-20.724590846667,19.9315870649596,6.35315305116633));
#195959=CARTESIAN_POINT('Ctrl Pts',(-20.7384657750112,19.8930912808199,
6.35071847537167));
#195960=CARTESIAN_POINT('Ctrl Pts',(-20.7503812099478,19.857017630369,6.34851222594941));
#195961=CARTESIAN_POINT('Ctrl Pts',(-20.7865572725681,19.736716450352,6.34134105663081));
#195962=CARTESIAN_POINT('Ctrl Pts',(-20.8065607469455,19.6512993602537,
6.33654457769394));
#195963=CARTESIAN_POINT('Ctrl Pts',(-20.8409626152498,19.4483957315726,
6.32534846007863));
#195964=CARTESIAN_POINT('Ctrl Pts',(-20.8509250852906,19.3304699297772,
6.31898334375529));
#195965=CARTESIAN_POINT('Ctrl Pts',(-20.8509995791047,19.2123349421389,
6.31236858093732));
#195966=CARTESIAN_POINT('Ctrl Pts',(-20.85099958079,19.2123322668744,6.3123684311405));
#195967=CARTESIAN_POINT('Ctrl Pts',(-20.8510434843996,19.1425685244161,
6.30846212993567));
#195968=CARTESIAN_POINT('Ctrl Pts',(-20.8476389261171,19.0728498012217,
6.30447848065918));
#195969=CARTESIAN_POINT('Ctrl Pts',(-20.8397869279037,18.9931536601121,
6.29977940203969));
#195970=CARTESIAN_POINT('Ctrl Pts',(-20.8386993799332,18.9828857128295,
6.29917123854736));
#195971=CARTESIAN_POINT('Ctrl Pts',(-20.8367363709343,18.9655630760309,
6.29814042520597));
#195972=CARTESIAN_POINT('Ctrl Pts',(-20.8359004048649,18.9585040288362,
6.29771901463873));
#195973=CARTESIAN_POINT('Ctrl Pts',(-20.8342948980459,18.9455076569588,
6.29694061396329));
#195974=CARTESIAN_POINT('Ctrl Pts',(-20.8335356902283,18.9395691113789,
6.29658395236896));
#195975=CARTESIAN_POINT('Ctrl Pts',(-20.8319163682403,18.9273161565484,
6.29584599643015));
#195976=CARTESIAN_POINT('Ctrl Pts',(-20.8310529127544,18.9210022570801,
6.29546459999048));
#195977=CARTESIAN_POINT('Ctrl Pts',(-20.8290506673527,18.9068378254571,
6.2946064050122));
#195978=CARTESIAN_POINT('Ctrl Pts',(-20.8278962379869,18.8989896330738,
6.29412911596063));
#195979=CARTESIAN_POINT('Ctrl Pts',(-20.8248469162425,18.8790388038057,
6.29291118497491));
#195980=CARTESIAN_POINT('Ctrl Pts',(-20.8228910539935,18.8669459089206,
6.29216862077348));
#195981=CARTESIAN_POINT('Ctrl Pts',(-20.8108421494137,18.7963422494321,
6.28780728121338));
#195982=CARTESIAN_POINT('Ctrl Pts',(-20.7983969467989,18.7382648606237,
6.28411428556892));
#195983=CARTESIAN_POINT('Ctrl Pts',(-20.768184864996,18.6214796440378,6.27646782283292));
#195984=CARTESIAN_POINT('Ctrl Pts',(-20.7502747202371,18.5628660550676,
6.27251334280754));
#195985=CARTESIAN_POINT('Ctrl Pts',(-20.6755356481374,18.3515455583173,
6.25787182674141));
#195986=CARTESIAN_POINT('Ctrl Pts',(-20.6036810235824,18.2047616685174,
6.24690184082058));
#195987=CARTESIAN_POINT('Ctrl Pts',(-20.4982581648339,18.0404761583438,
6.23450060265955));
#195988=CARTESIAN_POINT('Ctrl Pts',(-20.4801870803267,18.0136847196447,
6.23247583529186));
#195989=CARTESIAN_POINT('Ctrl Pts',(-20.4573317969455,17.981419285517,6.23004447346033));
#195990=CARTESIAN_POINT('Ctrl Pts',(-20.4531247089344,17.9755440297639,
6.22960204057148));
#195991=CARTESIAN_POINT('Ctrl Pts',(-20.446479581814,17.9663636889624,6.22891133710014));
#195992=CARTESIAN_POINT('Ctrl Pts',(-20.4440619140411,17.9630440249385,
6.22866170230413));
#195993=CARTESIAN_POINT('Ctrl Pts',(-20.4395231336304,17.9568498486629,
6.22819617957426));
#195994=CARTESIAN_POINT('Ctrl Pts',(-20.4374044286747,17.9539737019274,
6.22798013729281));
#195995=CARTESIAN_POINT('Ctrl Pts',(-20.432549214559,17.9474175548383,6.22748791547497));
#195996=CARTESIAN_POINT('Ctrl Pts',(-20.4298080270493,17.9437410815849,
6.22721206663253));
#195997=CARTESIAN_POINT('Ctrl Pts',(-20.4213381391625,17.9324579860471,
6.22636592169027));
#195998=CARTESIAN_POINT('Ctrl Pts',(-20.4155699543542,17.9248809644555,
6.22579831488482));
#195999=CARTESIAN_POINT('Ctrl Pts',(-20.3366220007337,17.8226149958194,
6.21814184625226));
#196000=CARTESIAN_POINT('Ctrl Pts',(-20.2555812996749,17.7342437984343,
6.21157123568353));
#196001=CARTESIAN_POINT('Ctrl Pts',(-20.0873438689919,17.5794322826007,
6.19912687077946));
#196002=CARTESIAN_POINT('Ctrl Pts',(-20.0016214805514,17.5119744870199,
6.19325974339119));
#196003=CARTESIAN_POINT('Ctrl Pts',(-19.8657158327931,17.4210589894665,
6.18416411522203));
#196004=CARTESIAN_POINT('Ctrl Pts',(-19.8191841601983,17.3924719535463,
6.18108449626243));
#196005=CARTESIAN_POINT('Ctrl Pts',(-19.7518700138761,17.3546212427312,
6.17664065565643));
#196006=CARTESIAN_POINT('Ctrl Pts',(-19.7319619168714,17.3438434954631,
6.17532783861267));
#196007=CARTESIAN_POINT('Ctrl Pts',(-19.6966134116401,17.3254335294786,
6.17299694498611));
#196008=CARTESIAN_POINT('Ctrl Pts',(-19.6812453606778,17.3176665122917,
6.17198361600958));
#196009=CARTESIAN_POINT('Ctrl Pts',(-19.6584068545006,17.3064715867414,
6.1704770517554));
#196010=CARTESIAN_POINT('Ctrl Pts',(-19.6510081966836,17.3028982013879,
6.16998889345795));
#196011=CARTESIAN_POINT('Ctrl Pts',(-19.6380627616575,17.2967385297406,
6.16913451216844));
#196012=CARTESIAN_POINT('Ctrl Pts',(-19.6325251896346,17.2941330416762,
6.16876896054389));
#196013=CARTESIAN_POINT('Ctrl Pts',(-19.6214722476851,17.2889909305909,
6.16803913168097));
#196014=CARTESIAN_POINT('Ctrl Pts',(-19.6159571092058,17.2864539471269,
6.16767487125934));
#196015=CARTESIAN_POINT('Ctrl Pts',(-19.6027565128356,17.2804502841944,
6.16680274611347));
#196016=CARTESIAN_POINT('Ctrl Pts',(-19.5950611519647,17.2770057463499,
6.16629412584133));
#196017=CARTESIAN_POINT('Ctrl Pts',(-19.5672754632262,17.2647672400747,
6.16445676650978));
#196018=CARTESIAN_POINT('Ctrl Pts',(-19.5470698885699,17.2562398477201,
6.1631189813563));
#196019=CARTESIAN_POINT('Ctrl Pts',(-19.3530644998931,17.1778917720344,
6.15025414341361));
#196020=CARTESIAN_POINT('Ctrl Pts',(-19.1708837222702,17.131126405521,6.13791080300001));
#196021=CARTESIAN_POINT('Ctrl Pts',(-18.9064965828143,17.0995593735971,
6.12033449500081));
#196022=CARTESIAN_POINT('Ctrl Pts',(-18.8275435838399,17.094590807783,6.11514392804049));
#196023=CARTESIAN_POINT('Ctrl Pts',(-18.7127636716571,17.0938049993789,
6.10782890704954));
#196024=CARTESIAN_POINT('Ctrl Pts',(-18.6770312462052,17.0944649628788,
6.10558452811651));
#196025=CARTESIAN_POINT('Ctrl Pts',(-18.6338894366461,17.0963552666428,
6.10292790187064));
#196026=CARTESIAN_POINT('Ctrl Pts',(-18.626450186497,17.096720568464,6.10247171559809));
#196027=CARTESIAN_POINT('Ctrl Pts',(-18.6148637028832,17.0973508310434,
6.10176436104888));
#196028=CARTESIAN_POINT('Ctrl Pts',(-18.610715144731,17.0975887499428,6.10151172047072));
#196029=CARTESIAN_POINT('Ctrl Pts',(-18.603007484209,17.0980535551069,6.10104353885059));
#196030=CARTESIAN_POINT('Ctrl Pts',(-18.5994482888448,17.0982772175513,
6.10082782548917));
#196031=CARTESIAN_POINT('Ctrl Pts',(-18.5913834213461,17.0988044825677,
6.10034011094005));
#196032=CARTESIAN_POINT('Ctrl Pts',(-18.5868781566768,17.0991135076777,
6.10006841686534));
#196033=CARTESIAN_POINT('Ctrl Pts',(-18.575238981094,17.0999492881576,6.09936838369463));
#196034=CARTESIAN_POINT('Ctrl Pts',(-18.5681066227213,17.1004977944205,
6.09894123492731));
#196035=CARTESIAN_POINT('Ctrl Pts',(-18.5241278525014,17.1041042556274,
6.09631790102283));
#196036=CARTESIAN_POINT('Ctrl Pts',(-18.4873615789615,17.1080910962504,
6.09417027794141));
#196037=CARTESIAN_POINT('Ctrl Pts',(-18.2817962903531,17.1358482011441,
6.08232481103278));
#196038=CARTESIAN_POINT('Ctrl Pts',(-18.1162345485755,17.1789761287412,
6.07335635840107));
#196039=CARTESIAN_POINT('Ctrl Pts',(-17.8691055451318,17.276394120929,6.05874253821852));
#196040=CARTESIAN_POINT('Ctrl Pts',(-17.7830487507644,17.3172125272942,
6.05340688478541));
#196041=CARTESIAN_POINT('Ctrl Pts',(-17.6813933922093,17.3741100527393,
6.04662317454197));
#196042=CARTESIAN_POINT('Ctrl Pts',(-17.6629118486344,17.3848249065455,
6.04536966723941));
#196043=CARTESIAN_POINT('Ctrl Pts',(-17.6368750407788,17.4004512126132,
6.0435734000358));
#196044=CARTESIAN_POINT('Ctrl Pts',(-17.6291837195674,17.4051342601596,
6.04303895689151));
#196045=CARTESIAN_POINT('Ctrl Pts',(-17.6159707144262,17.413295324851,6.04211410897012));
#196046=CARTESIAN_POINT('Ctrl Pts',(-17.6104347629344,17.4167500901378,
6.04172456370628));
#196047=CARTESIAN_POINT('Ctrl Pts',(-17.5998684001713,17.4234122103324,
6.04097706212021));
#196048=CARTESIAN_POINT('Ctrl Pts',(-17.5948353933899,17.4266153471257,
6.04061926483872));
#196049=CARTESIAN_POINT('Ctrl Pts',(-17.5817888909255,17.4349961755454,
6.03968720272675));
#196050=CARTESIAN_POINT('Ctrl Pts',(-17.573796803638,17.4402067983973,6.03911171244558));
#196051=CARTESIAN_POINT('Ctrl Pts',(-17.5466940638271,17.4581392887053,
6.03714446346937));
#196052=CARTESIAN_POINT('Ctrl Pts',(-17.5277557729903,17.471117573238,6.03574308840025));
#196053=CARTESIAN_POINT('Ctrl Pts',(-17.3655108966283,17.5862251519348,
6.0234989959911));
#196054=CARTESIAN_POINT('Ctrl Pts',(-17.2352706780062,17.7055291347743,
6.01194819141612));
#196055=CARTESIAN_POINT('Ctrl Pts',(-17.0651619122613,17.9055572688175,
5.99459965398099));
#196056=CARTESIAN_POINT('Ctrl Pts',(-17.0131158677944,17.974973706075,5.98888819890156));
#196057=CARTESIAN_POINT('Ctrl Pts',(-16.9447274514095,18.0789148274861,
5.98094501205016));
#196058=CARTESIAN_POINT('Ctrl Pts',(-16.924830335303,18.1109915351281,5.9785713809598));
#196059=CARTESIAN_POINT('Ctrl Pts',(-16.9019848554932,18.1501198148435,
5.97578326406884));
#196060=CARTESIAN_POINT('Ctrl Pts',(-16.8982045707327,18.1566749064866,
5.97531971527384));
#196061=CARTESIAN_POINT('Ctrl Pts',(-16.8923900894788,18.1668834261588,
5.974603459683));
#196062=CARTESIAN_POINT('Ctrl Pts',(-16.8903314771768,18.1705227724988,
5.97434922129647));
#196063=CARTESIAN_POINT('Ctrl Pts',(-16.8865382088722,18.1772753601127,
5.97387957961708));
#196064=CARTESIAN_POINT('Ctrl Pts',(-16.8848006469526,18.1803868554234,
5.9736639945653));
#196065=CARTESIAN_POINT('Ctrl Pts',(-16.8808958751458,18.187420894747,5.97317846397312));
#196066=CARTESIAN_POINT('Ctrl Pts',(-16.8787332642552,18.1913459300575,
5.97290881390909));
#196067=CARTESIAN_POINT('Ctrl Pts',(-16.8724034036225,18.2029211329634,
5.97211726735905));
#196068=CARTESIAN_POINT('Ctrl Pts',(-16.8682708338209,18.2105902968383,
5.97159753021339));
#196069=CARTESIAN_POINT('Ctrl Pts',(-16.8392385361524,18.2652736667509,
5.96792340350182));
#196070=CARTESIAN_POINT('Ctrl Pts',(-16.8160692644747,18.3131904387904,
5.96486984281173));
#196071=CARTESIAN_POINT('Ctrl Pts',(-16.7880791762991,18.3771199194924,
5.96094459639308));
#196072=CARTESIAN_POINT('Ctrl Pts',(-16.7816085926323,18.3923843066682,
5.96001820504389));
#196073=CARTESIAN_POINT('Ctrl Pts',(-16.7187292951286,18.5457070303135,
5.95080645080096));
#196074=CARTESIAN_POINT('Ctrl Pts',(-16.6768784295116,18.6892863407392,
5.94290170800813));
#196075=CARTESIAN_POINT('Ctrl Pts',(-16.6395521323042,18.8967175714134,
5.93124048580072));
#196076=CARTESIAN_POINT('Ctrl Pts',(-16.6312934351056,18.9578013333906,
5.92778256618447));
#196077=CARTESIAN_POINT('Ctrl Pts',(-16.6223416737196,19.0561772179567,
5.92211326607198));
#196078=CARTESIAN_POINT('Ctrl Pts',(-16.6199487523165,19.0932797601167,
5.91995269090957));
#196079=CARTESIAN_POINT('Ctrl Pts',(-16.6181104870815,19.1415424115342,
5.91710563011443));
#196080=CARTESIAN_POINT('Ctrl Pts',(-16.6177746779774,19.1526633326378,
5.91644708928978));
#196081=CARTESIAN_POINT('Ctrl Pts',(-16.6173711488613,19.1707525170337,
5.91537164258326));
#196082=CARTESIAN_POINT('Ctrl Pts',(-16.6172501428516,19.1777194676155,
5.91495641066516));
#196083=CARTESIAN_POINT('Ctrl Pts',(-16.6170835953851,19.1911178413868,
5.91415583484454));
#196084=CARTESIAN_POINT('Ctrl Pts',(-16.617032962678,19.197549132552,5.91377065508149));
#196085=CARTESIAN_POINT('Ctrl Pts',(-16.6169841377683,19.2122740797372,
5.91288665504818));
#196086=CARTESIAN_POINT('Ctrl Pts',(-16.617005375271,19.2205676554675,5.91238723118004));
#196087=CARTESIAN_POINT('Ctrl Pts',(-16.6171912512708,19.2425983293028,
5.91105643836946));
#196088=CARTESIAN_POINT('Ctrl Pts',(-16.6174408737861,19.2563341415234,
5.910222422906));
#196089=CARTESIAN_POINT('Ctrl Pts',(-16.6203593388622,19.3608943568631,
5.90384010850424));
#196090=CARTESIAN_POINT('Ctrl Pts',(-16.6287390252885,19.4514529004444,
5.89811312666068));
#196091=CARTESIAN_POINT('Ctrl Pts',(-16.664836764059,19.6800641311033,5.88316588084904));
#196092=CARTESIAN_POINT('Ctrl Pts',(-16.7005470077048,19.8164103179136,
5.87376836695336));
#196093=CARTESIAN_POINT('Ctrl Pts',(-16.768326615805,19.9988702428161,5.86102877477234));
#196094=CARTESIAN_POINT('Ctrl Pts',(-16.7890868596193,20.048809671569,5.85752804886356));
#196095=CARTESIAN_POINT('Ctrl Pts',(-16.8234929313602,20.1233809940084,
5.85233226288481));
#196096=CARTESIAN_POINT('Ctrl Pts',(-16.8357543484,20.1486246375683,5.85057920977994));
#196097=CARTESIAN_POINT('Ctrl Pts',(-16.8516566273907,20.1797725080392,
5.84843020079177));
#196098=CARTESIAN_POINT('Ctrl Pts',(-16.8548287155888,20.1859112942341,
5.8480073552443));
#196099=CARTESIAN_POINT('Ctrl Pts',(-16.8599015295176,20.1956117095243,
5.84734041314579));
#196100=CARTESIAN_POINT('Ctrl Pts',(-16.8617824514703,20.1991835594688,
5.84709510035074));
#196101=CARTESIAN_POINT('Ctrl Pts',(-16.8653530515628,20.2059173001764,
5.84663316531952));
#196102=CARTESIAN_POINT('Ctrl Pts',(-16.8670405233587,20.2090802396831,
5.84641641516736));
#196103=CARTESIAN_POINT('Ctrl Pts',(-16.870922073583,20.2163113963391,5.84592137814805));
#196104=CARTESIAN_POINT('Ctrl Pts',(-16.8731214438711,20.2203767204462,
5.84564343141904));
#196105=CARTESIAN_POINT('Ctrl Pts',(-16.8790065080989,20.2311700812277,
5.84490636216305));
#196106=CARTESIAN_POINT('Ctrl Pts',(-16.8827155268657,20.2378854138571,
5.84444868489924));
#196107=CARTESIAN_POINT('Ctrl Pts',(-16.9092561666818,20.2853271602103,
5.84122071899547));
#196108=CARTESIAN_POINT('Ctrl Pts',(-16.933394932927,20.3253118980481,5.83852828084531));
#196109=CARTESIAN_POINT('Ctrl Pts',(-16.9612803690312,20.3682269434661,
5.83563328125264));
#196110=CARTESIAN_POINT('Ctrl Pts',(-16.9637343984861,20.3719775145429,
5.8353802278577));
#196111=CARTESIAN_POINT('Ctrl Pts',(-16.9790341052072,20.3951992414694,
5.83381298876503));
#196112=CARTESIAN_POINT('Ctrl Pts',(-16.9921892848664,20.4144652565201,
5.83251072265505));
#196113=CARTESIAN_POINT('Ctrl Pts',(-17.031938258186,20.4706608691324,5.8286944360761));
#196114=CARTESIAN_POINT('Ctrl Pts',(-17.0594077533745,20.5069555234893,
5.82620624392669));
#196115=CARTESIAN_POINT('Ctrl Pts',(-17.1567931128374,20.6273560458897,
5.81777527866447));
#196116=CARTESIAN_POINT('Ctrl Pts',(-17.2320430416328,20.7069179205334,
5.81188726902176));
#196117=CARTESIAN_POINT('Ctrl Pts',(-17.3539495714906,20.8172959610812,
5.80274312010775));
#196118=CARTESIAN_POINT('Ctrl Pts',(-17.3962267306153,20.8526722980612,
5.7996357110908));
#196119=CARTESIAN_POINT('Ctrl Pts',(-17.4669834455431,20.9073298627378,
5.7944918618775));
#196120=CARTESIAN_POINT('Ctrl Pts',(-17.4946377665465,20.927638287524,5.79249480608614));
#196121=CARTESIAN_POINT('Ctrl Pts',(-17.5316370964553,20.9534492183662,
5.78983422306384));
#196122=CARTESIAN_POINT('Ctrl Pts',(-17.5405490858929,20.9595653374878,
5.78919422271112));
#196123=CARTESIAN_POINT('Ctrl Pts',(-17.5552247276767,20.9694724740131,
5.78814152322078));
#196124=CARTESIAN_POINT('Ctrl Pts',(-17.5609608346986,20.9733040882436,
5.78773036532537));
#196125=CARTESIAN_POINT('Ctrl Pts',(-17.5721021360872,20.9806677780441,
5.78693229759204));
#196126=CARTESIAN_POINT('Ctrl Pts',(-17.5775049705407,20.9842032980501,
5.7865455231215));
#196127=CARTESIAN_POINT('Ctrl Pts',(-17.5900196115848,20.9923111334808,
5.7856501394523));
#196128=CARTESIAN_POINT('Ctrl Pts',(-17.5971427684536,20.9968656486933,
5.78514087410114));
#196129=CARTESIAN_POINT('Ctrl Pts',(-17.6163783330885,21.009003064068,5.78376654446671));
#196130=CARTESIAN_POINT('Ctrl Pts',(-17.6285403917863,21.0165060918307,
5.78289855197605));
#196131=CARTESIAN_POINT('Ctrl Pts',(-17.7408542623367,21.084234634933,5.77489024909518));
#196132=CARTESIAN_POINT('Ctrl Pts',(-17.8457399606368,21.1361838213998,
5.7674480708377));
#196133=CARTESIAN_POINT('Ctrl Pts',(-18.1056903762818,21.2391543620767,
5.74918452659896));
#196134=CARTESIAN_POINT('Ctrl Pts',(-18.2634245468998,21.2814448611377,
5.7382229855241));
#196135=CARTESIAN_POINT('Ctrl Pts',(-18.4565498267117,21.3099910951027,
5.72581868247732));
#196136=CARTESIAN_POINT('Ctrl Pts',(-18.4887612653043,21.313997966307,5.72378473181657));
#196137=CARTESIAN_POINT('Ctrl Pts',(-18.5282532400213,21.3179906570333,
5.72134390059341));
#196138=CARTESIAN_POINT('Ctrl Pts',(-18.5354562325502,21.3186816016554,
5.72090085829218));
#196139=CARTESIAN_POINT('Ctrl Pts',(-18.5467547795702,21.3197069758705,
5.72020941639157));
#196140=CARTESIAN_POINT('Ctrl Pts',(-18.5508479270595,21.3200664288968,
5.71995964786274));
#196141=CARTESIAN_POINT('Ctrl Pts',(-18.5585013383062,21.3207160896551,
5.71949400946267));
#196142=CARTESIAN_POINT('Ctrl Pts',(-18.562061250733,21.3210092004386,5.71927798443774));
#196143=CARTESIAN_POINT('Ctrl Pts',(-18.5701900261697,21.321657786677,5.7187859751206));
#196144=CARTESIAN_POINT('Ctrl Pts',(-18.5747593033939,21.3220074375608,
5.71851032042195));
#196145=CARTESIAN_POINT('Ctrl Pts',(-18.5888100988992,21.3230367545008,
5.71766536263211));
#196146=CARTESIAN_POINT('Ctrl Pts',(-18.5982952388894,21.3236674099768,
5.71709873790055));
#196147=CARTESIAN_POINT('Ctrl Pts',(-18.6836875767826,21.3287675718274,
5.71202892657737));
#196148=CARTESIAN_POINT('Ctrl Pts',(-18.759788751183,21.3292087683342,5.70773293424254));
#196149=CARTESIAN_POINT('Ctrl Pts',(-18.8781801227877,21.3235115463132,
5.7011733252909));
#196150=CARTESIAN_POINT('Ctrl Pts',(-18.9205339217518,21.3201937367961,
5.69885159883338));
#196151=CARTESIAN_POINT('Ctrl Pts',(-19.0714390388761,21.3037910866686,
5.69058745326399));
#196152=CARTESIAN_POINT('Ctrl Pts',(-19.1790385582027,21.2835779676184,
5.6847008706784));
#196153=CARTESIAN_POINT('Ctrl Pts',(-19.337769272666,21.2408238079544,5.67556003937225));
#196154=CARTESIAN_POINT('Ctrl Pts',(-19.3903645313063,21.22443164367,5.6724545318912));
#196155=CARTESIAN_POINT('Ctrl Pts',(-19.4745732107129,21.1945362817295,
5.66731354979412));
#196156=CARTESIAN_POINT('Ctrl Pts',(-19.5066030770277,21.1822810937091,
5.66531740203229));
#196157=CARTESIAN_POINT('Ctrl Pts',(-19.5483165278224,21.1651479942459,
5.66265785732385));
#196158=CARTESIAN_POINT('Ctrl Pts',(-19.5582814048659,21.1609656278861,
5.6620179638236));
#196159=CARTESIAN_POINT('Ctrl Pts',(-19.5745533179218,21.1539891144056,
5.66096539532043));
#196160=CARTESIAN_POINT('Ctrl Pts',(-19.5808795703622,21.1512400806446,
5.6605542608067));
#196161=CARTESIAN_POINT('Ctrl Pts',(-19.5931016127375,21.1458579048335,
5.65975620645533));
#196162=CARTESIAN_POINT('Ctrl Pts',(-19.5989990193485,21.1432286065573,
5.65936942181559));
#196163=CARTESIAN_POINT('Ctrl Pts',(-19.6125913970298,21.1370938858507,
5.65847396797539));
#196164=CARTESIAN_POINT('Ctrl Pts',(-19.6202775402769,21.1335692753205,
5.6579646422989));
#196165=CARTESIAN_POINT('Ctrl Pts',(-19.6408989806712,21.1239630276172,
5.65659004430657));
#196166=CARTESIAN_POINT('Ctrl Pts',(-19.653793968036,21.1177963569317,5.65572184200403));
#196167=CARTESIAN_POINT('Ctrl Pts',(-19.7717736563679,21.05990061519,5.64769732733988));
#196168=CARTESIAN_POINT('Ctrl Pts',(-19.8724412122536,20.9996730816309,
5.64023772750553));
#196169=CARTESIAN_POINT('Ctrl Pts',(-20.100565671935,20.8361020534301,5.6219002579477));
#196170=CARTESIAN_POINT('Ctrl Pts',(-20.2220273583324,20.7256726417926,
5.61087999345474));
#196171=CARTESIAN_POINT('Ctrl Pts',(-20.3502422298733,20.5786404347042,
5.59849616853959));
#196172=CARTESIAN_POINT('Ctrl Pts',(-20.3703945966566,20.5544627919728,
5.59652526307071));
#196173=CARTESIAN_POINT('Ctrl Pts',(-20.394466628494,20.5242368201498,5.59414953339098));
#196174=CARTESIAN_POINT('Ctrl Pts',(-20.3989032659307,20.5186075438063,
5.59371073975647));
#196175=CARTESIAN_POINT('Ctrl Pts',(-20.4058289597471,20.5097277190205,
5.59302444712903));
#196176=CARTESIAN_POINT('Ctrl Pts',(-20.4083372744581,20.5064923584559,
5.59277561194386));
#196177=CARTESIAN_POINT('Ctrl Pts',(-20.4130180116902,20.5004185867781,
5.59231077536583));
#196178=CARTESIAN_POINT('Ctrl Pts',(-20.4151926059839,20.497581982351,5.59209462445893));
#196179=CARTESIAN_POINT('Ctrl Pts',(-20.4201529604497,20.4910775003369,
5.59160110718075));
#196180=CARTESIAN_POINT('Ctrl Pts',(-20.4229339368643,20.4874060367804,
5.59132407819034));
#196181=CARTESIAN_POINT('Ctrl Pts',(-20.430181993639,20.4777719412308,5.59060107055908));
#196182=CARTESIAN_POINT('Ctrl Pts',(-20.4346296633213,20.4717946932659,
5.59015641587812));
#196183=CARTESIAN_POINT('Ctrl Pts',(-20.4640846174746,20.4317705577963,
5.58720408883549));
#196184=CARTESIAN_POINT('Ctrl Pts',(-20.4881014047042,20.3970026724826,
5.58476002387392));
#196185=CARTESIAN_POINT('Ctrl Pts',(-20.5515185183681,20.299051676216,5.57813170930489));
#196186=CARTESIAN_POINT('Ctrl Pts',(-20.5886527365288,20.234471898914,5.57404402846568));
#196187=CARTESIAN_POINT('Ctrl Pts',(-20.6602976389824,20.0931151602238,
5.56540883367988));
#196188=CARTESIAN_POINT('Ctrl Pts',(-20.6937775095326,20.0159926504986,
5.56087765513829));
#196189=CARTESIAN_POINT('Ctrl Pts',(-20.722580628988,19.937110240951,5.55626853452768));
#196190=CARTESIAN_POINT('',(-20.8509995343428,19.212404133962,6.0890562790225));
#196191=CARTESIAN_POINT('Ctrl Pts',(-20.7225805912209,19.9371103443827,
5.33540100209138));
#196192=CARTESIAN_POINT('Ctrl Pts',(-20.7135660345865,19.9617982895418,
5.33706797012045));
#196193=CARTESIAN_POINT('Ctrl Pts',(-20.7040899507275,19.9863232427178,
5.33871648488639));
#196194=CARTESIAN_POINT('Ctrl Pts',(-20.6904971184,20.0196419938108,5.34093976153892));
#196195=CARTESIAN_POINT('Ctrl Pts',(-20.6867761549495,20.028586781516,5.34153499025804));
#196196=CARTESIAN_POINT('Ctrl Pts',(-20.6811908871778,20.0417574708377,
5.34240867211156));
#196197=CARTESIAN_POINT('Ctrl Pts',(-20.6793740071793,20.0460031733982,
5.342689886409));
#196198=CARTESIAN_POINT('Ctrl Pts',(-20.6761257889705,20.053525491649,5.34318732666474));
#196199=CARTESIAN_POINT('Ctrl Pts',(-20.6747000297133,20.0568044570775,
5.34340388703281));
#196200=CARTESIAN_POINT('Ctrl Pts',(-20.6716271655759,20.0638227612115,
5.34386681796256));
#196201=CARTESIAN_POINT('Ctrl Pts',(-20.6699775451052,20.067560937888,5.34411303200905));
#196202=CARTESIAN_POINT('Ctrl Pts',(-20.6654189064737,20.0778107467186,
5.34478721117637));
#196203=CARTESIAN_POINT('Ctrl Pts',(-20.6624877592546,20.0843125606631,
5.34521384245481));
#196204=CARTESIAN_POINT('Ctrl Pts',(-20.6466515865044,20.1189715090635,
5.34748322760273));
#196205=CARTESIAN_POINT('Ctrl Pts',(-20.6331619181897,20.1468592785305,
5.34929213537687));
#196206=CARTESIAN_POINT('Ctrl Pts',(-20.5446480095021,20.3200449097339,
5.36047878659695));
#196207=CARTESIAN_POINT('Ctrl Pts',(-20.4536052171951,20.4565509095654,
5.36912130513015));
#196208=CARTESIAN_POINT('Ctrl Pts',(-20.2715338366188,20.6709803975028,
5.38451644388529));
#196209=CARTESIAN_POINT('Ctrl Pts',(-20.1879783781721,20.7542091843604,
5.39108669184648));
#196210=CARTESIAN_POINT('Ctrl Pts',(-20.0870076702794,20.8392701787546,
5.39882101046907));
#196211=CARTESIAN_POINT('Ctrl Pts',(-20.075977228451,20.8483730895036,5.3996631879519));
#196212=CARTESIAN_POINT('Ctrl Pts',(-20.058277885152,20.8626805446235,5.40101063904461));
#196213=CARTESIAN_POINT('Ctrl Pts',(-20.0516684383127,20.8679581835696,
5.40151296542724));
#196214=CARTESIAN_POINT('Ctrl Pts',(-20.039957501663,20.8771949770625,5.40240160594772));
#196215=CARTESIAN_POINT('Ctrl Pts',(-20.0348691625804,20.8811706853371,
5.40278725296098));
#196216=CARTESIAN_POINT('Ctrl Pts',(-20.0243087481201,20.8893443927697,
5.4035867185068));
#196217=CARTESIAN_POINT('Ctrl Pts',(-20.0188341943366,20.8935390508185,
5.40400066282992));
#196218=CARTESIAN_POINT('Ctrl Pts',(-20.0047322464095,20.9042351454735,
5.40506571968163));
#196219=CARTESIAN_POINT('Ctrl Pts',(-19.9960754864076,20.9106973729951,
5.4057183592004));
#196220=CARTESIAN_POINT('Ctrl Pts',(-19.9597641693583,20.9373732387904,
5.40845135447529));
#196221=CARTESIAN_POINT('Ctrl Pts',(-19.9316717813474,20.9569795094198,
5.41055497623381));
#196222=CARTESIAN_POINT('Ctrl Pts',(-19.857271187706,21.0062646145043,5.41610193348169));
#196223=CARTESIAN_POINT('Ctrl Pts',(-19.8102625012957,21.0348342603711,
5.41958352494815));
#196224=CARTESIAN_POINT('Ctrl Pts',(-19.6666534953555,21.1146263806904,
5.4301425048208));
#196225=CARTESIAN_POINT('Ctrl Pts',(-19.5671475887808,21.1602299932548,
5.43736831881349));
#196226=CARTESIAN_POINT('Ctrl Pts',(-19.4286063014337,21.2111699333928,
5.44711919345343));
#196227=CARTESIAN_POINT('Ctrl Pts',(-19.3922842171244,21.2234163749141,
5.44964693207065));
#196228=CARTESIAN_POINT('Ctrl Pts',(-19.3246533106698,21.2441918430126,
5.45428210398152));
#196229=CARTESIAN_POINT('Ctrl Pts',(-19.2934416935216,21.253000376649,5.45639373279736));
#196230=CARTESIAN_POINT('Ctrl Pts',(-19.25593813785,21.262660125563,5.45888980568219));
#196231=CARTESIAN_POINT('Ctrl Pts',(-19.249830177726,21.2642043054003,5.45929502693071));
#196232=CARTESIAN_POINT('Ctrl Pts',(-19.2015192301592,21.2761888179575,
5.46248943829245));
#196233=CARTESIAN_POINT('Ctrl Pts',(-19.1590072001206,21.2853549748665,
5.46523622537189));
#196234=CARTESIAN_POINT('Ctrl Pts',(-19.1088498456021,21.2945625851522,
5.46837909211825));
#196235=CARTESIAN_POINT('Ctrl Pts',(-19.1014525170888,21.2958798777215,
5.46884012772329));
#196236=CARTESIAN_POINT('Ctrl Pts',(-19.0894908303876,21.297944335113,5.46958145635208));
#196237=CARTESIAN_POINT('Ctrl Pts',(-19.0849308383423,21.2987159615205,
5.46986308398426));
#196238=CARTESIAN_POINT('Ctrl Pts',(-19.0768402819635,21.3000577613761,
5.47036098142376));
#196239=CARTESIAN_POINT('Ctrl Pts',(-19.073310767816,21.3006339375186,5.47057758792936));
#196240=CARTESIAN_POINT('Ctrl Pts',(-19.0657496693643,21.3018485878729,
5.4710403148354));
#196241=CARTESIAN_POINT('Ctrl Pts',(-19.0617177047297,21.302484345432,5.47128628030116));
#196242=CARTESIAN_POINT('Ctrl Pts',(-19.0506547154868,21.3041959734194,
5.47195907772502));
#196243=CARTESIAN_POINT('Ctrl Pts',(-19.0436199936327,21.3052480881673,
5.47238458493671));
#196244=CARTESIAN_POINT('Ctrl Pts',(-19.0061840729049,21.3106542596439,
5.47463731965919));
#196245=CARTESIAN_POINT('Ctrl Pts',(-18.9756944251468,21.3143820877623,
5.47643128668597));
#196246=CARTESIAN_POINT('Ctrl Pts',(-18.8834083949871,21.3236320781564,
5.48176744818545));
#196247=CARTESIAN_POINT('Ctrl Pts',(-18.8214372885932,21.3271032599958,
5.48522475002098));
#196248=CARTESIAN_POINT('Ctrl Pts',(-18.6125869234852,21.3296091649353,
5.49670838165205));
#196249=CARTESIAN_POINT('Ctrl Pts',(-18.465992946418,21.3160935516277,5.50451808001055));
#196250=CARTESIAN_POINT('Ctrl Pts',(-18.2486289311332,21.2729639755249,
5.51689097089301));
#196251=CARTESIAN_POINT('Ctrl Pts',(-18.1761119603627,21.2545360753492,
5.52115152578509));
#196252=CARTESIAN_POINT('Ctrl Pts',(-18.0922002379856,21.2284127449467,
5.52630815978251));
#196253=CARTESIAN_POINT('Ctrl Pts',(-18.0797105919105,21.2243967509875,
5.52708163424079));
#196254=CARTESIAN_POINT('Ctrl Pts',(-18.0594783470984,21.2176830216465,
5.52834463408212));
#196255=CARTESIAN_POINT('Ctrl Pts',(-18.0517125571541,21.2150559004289,
5.52883183202753));
#196256=CARTESIAN_POINT('Ctrl Pts',(-18.0379118724071,21.2102976962042,
5.52970203066707));
#196257=CARTESIAN_POINT('Ctrl Pts',(-18.0318709826287,21.2081842180928,
5.53008444386483));
#196258=CARTESIAN_POINT('Ctrl Pts',(-18.0191632818446,21.2036734953266,
5.53089211289025));
#196259=CARTESIAN_POINT('Ctrl Pts',(-18.0124987464797,21.2012701153033,
5.53131756916379));
#196260=CARTESIAN_POINT('Ctrl Pts',(-17.9949047563192,21.194825346598,5.53244577956629));
#196261=CARTESIAN_POINT('Ctrl Pts',(-17.9839965041616,21.1907271359354,
5.5331504247071));
#196262=CARTESIAN_POINT('Ctrl Pts',(-17.9334956544943,21.1712767773999,
5.53643707146966));
#196263=CARTESIAN_POINT('Ctrl Pts',(-17.8943391386625,21.1548265048645,
5.53905575800747));
#196264=CARTESIAN_POINT('Ctrl Pts',(-17.787868518414,21.1062791072656,5.54637750231929));
#196265=CARTESIAN_POINT('Ctrl Pts',(-17.72171900158,21.0717882666089,5.55115661438224));
#196266=CARTESIAN_POINT('Ctrl Pts',(-17.5531236676056,20.9722275716033,
5.56391168800682));
#196267=CARTESIAN_POINT('Ctrl Pts',(-17.4542113403519,20.9017189459469,
5.57200186061405));
#196268=CARTESIAN_POINT('Ctrl Pts',(-17.3030462510381,20.7730593194106,
5.58499180765804));
#196269=CARTESIAN_POINT('Ctrl Pts',(-17.246990504661,20.7197953368602,5.58997006572426));
#196270=CARTESIAN_POINT('Ctrl Pts',(-17.1874400658751,20.6566596653488,
5.59533057441974));
#196271=CARTESIAN_POINT('Ctrl Pts',(-17.1809592735439,20.6496952448621,
5.59591495009343));
#196272=CARTESIAN_POINT('Ctrl Pts',(-17.1714254380028,20.6393104533852,
5.59677578992672));
#196273=CARTESIAN_POINT('Ctrl Pts',(-17.1683363077027,20.6359235827177,
5.59705490177421));
#196274=CARTESIAN_POINT('Ctrl Pts',(-17.1628595701602,20.6298796670671,
5.59755002693678));
#196275=CARTESIAN_POINT('Ctrl Pts',(-17.1604676675143,20.6272265917477,
5.59776636301128));
#196276=CARTESIAN_POINT('Ctrl Pts',(-17.1553394962875,20.6215094430481,
5.59823037956115));
#196277=CARTESIAN_POINT('Ctrl Pts',(-17.1526054354679,20.6184434648815,
5.59847789530395));
#196278=CARTESIAN_POINT('Ctrl Pts',(-17.1450830115729,20.6099582195034,
5.59915932034447));
#196279=CARTESIAN_POINT('Ctrl Pts',(-17.1403134134999,20.6045222866787,
5.599591847653));
#196280=CARTESIAN_POINT('Ctrl Pts',(-17.1143338902617,20.5746054619374,
5.6019510564018));
#196281=CARTESIAN_POINT('Ctrl Pts',(-17.0936588560968,20.5496632710242,
5.60384063874464));
#196282=CARTESIAN_POINT('Ctrl Pts',(-16.9725697307351,20.3965621157053,
5.61505004650333));
#196283=CARTESIAN_POINT('Ctrl Pts',(-16.8866325848176,20.2576325301369,
5.62365501079258));
#196284=CARTESIAN_POINT('Ctrl Pts',(-16.7678204063314,20.0044022091073,
5.63896791783413));
#196285=CARTESIAN_POINT('Ctrl Pts',(-16.7270298344355,19.8946773723757,
5.64549249748144));
#196286=CARTESIAN_POINT('Ctrl Pts',(-16.6916475320491,19.7683953861157,
5.65317541318284));
#196287=CARTESIAN_POINT('Ctrl Pts',(-16.6879315188447,19.7545963349029,
5.65401695884199));
#196288=CARTESIAN_POINT('Ctrl Pts',(-16.6822397980225,19.7325750749912,
5.65536358780497));
#196289=CARTESIAN_POINT('Ctrl Pts',(-16.6801731154415,19.7243766749394,
5.65586572957054));
#196290=CARTESIAN_POINT('Ctrl Pts',(-16.6766148625333,19.7098958680802,
5.65675415501764));
#196291=CARTESIAN_POINT('Ctrl Pts',(-16.6751028112034,19.7036185700887,
5.65713977260974));
#196292=CARTESIAN_POINT('Ctrl Pts',(-16.6720348246296,19.6906208913539,
5.65793928666919));
#196293=CARTESIAN_POINT('Ctrl Pts',(-16.6704829736021,19.683899634042,5.65835330946692));
#196294=CARTESIAN_POINT('Ctrl Pts',(-16.6665839212048,19.6666276802532,
5.65941879883399));
#196295=CARTESIAN_POINT('Ctrl Pts',(-16.6642846438029,19.656066470778,5.66007179478921));
#196296=CARTESIAN_POINT('Ctrl Pts',(-16.6550256923499,19.6119135344231,
5.6628082424807));
#196297=CARTESIAN_POINT('Ctrl Pts',(-16.6488024887766,19.5781742867419,
5.66491503381012));
#196298=CARTESIAN_POINT('Ctrl Pts',(-16.634726328015,19.4898827353299,5.67047234159992));
#196299=CARTESIAN_POINT('Ctrl Pts',(-16.6281792838235,19.4351513336547,
5.67396129228824));
#196300=CARTESIAN_POINT('Ctrl Pts',(-16.6150299603028,19.2711853157515,
5.68453441106383));
#196301=CARTESIAN_POINT('Ctrl Pts',(-16.614751119347,19.1616338439582,5.69176695807165));
#196302=CARTESIAN_POINT('Ctrl Pts',(-16.6317988055526,18.9344877472608,
5.70681380616292));
#196303=CARTESIAN_POINT('Ctrl Pts',(-16.6505518532563,18.8173513797986,
5.71460005278452));
#196304=CARTESIAN_POINT('Ctrl Pts',(-16.681294158312,18.693140498366,5.72250355889524));
#196305=CARTESIAN_POINT('Ctrl Pts',(-16.6836451175635,18.683909305912,5.72308871218566));
#196306=CARTESIAN_POINT('Ctrl Pts',(-16.687220254165,18.670257263039,5.72395047294302));
#196307=CARTESIAN_POINT('Ctrl Pts',(-16.6883965816445,18.6658241648208,
5.72422973615586));
#196308=CARTESIAN_POINT('Ctrl Pts',(-16.6905147514381,18.6579450294181,
5.72472502739638));
#196309=CARTESIAN_POINT('Ctrl Pts',(-16.6914509166828,18.6544975251854,
5.72494137902286));
#196310=CARTESIAN_POINT('Ctrl Pts',(-16.6934819415484,18.6470922817078,
5.72540531467222));
#196311=CARTESIAN_POINT('Ctrl Pts',(-16.6945795875958,18.6431353649466,
5.72565273456437));
#196312=CARTESIAN_POINT('Ctrl Pts',(-16.6976400750763,18.6322259112284,
5.7263336254351));
#196313=CARTESIAN_POINT('Ctrl Pts',(-16.6996270233462,18.6252801139184,
5.72676571799974));
#196314=CARTESIAN_POINT('Ctrl Pts',(-16.7106873875433,18.5873516092909,
5.72911815673883));
#196315=CARTESIAN_POINT('Ctrl Pts',(-16.720433586824,18.5565675749139,5.73100165451978));
#196316=CARTESIAN_POINT('Ctrl Pts',(-16.7835874233358,18.3718847288774,
5.74221145155072));
#196317=CARTESIAN_POINT('Ctrl Pts',(-16.8539128066446,18.2243350421972,
5.75082103770599));
#196318=CARTESIAN_POINT('Ctrl Pts',(-17.0025823754461,17.9872561163335,
5.76614036298775));
#196319=CARTESIAN_POINT('Ctrl Pts',(-17.0727799955103,17.8935407360068,
5.7726664777862));
#196320=CARTESIAN_POINT('Ctrl Pts',(-17.1598309163756,17.7954135749015,
5.78035112157564));
#196321=CARTESIAN_POINT('Ctrl Pts',(-17.1694225770657,17.7848195403478,
5.78119268949349));
#196322=CARTESIAN_POINT('Ctrl Pts',(-17.1848584795014,17.7681136439012,
5.78253934742032));
#196323=CARTESIAN_POINT('Ctrl Pts',(-17.1906334541554,17.7619381693133,
5.78304149569069));
#196324=CARTESIAN_POINT('Ctrl Pts',(-17.2008835922263,17.7511079589549,
5.78392992871479));
#196325=CARTESIAN_POINT('Ctrl Pts',(-17.2053433731096,17.7464387664115,
5.78431554734269));
#196326=CARTESIAN_POINT('Ctrl Pts',(-17.214611700035,17.7368236953573,5.78511505968871));
#196327=CARTESIAN_POINT('Ctrl Pts',(-17.2194231934055,17.7318807761324,
5.78552907971818));
#196328=CARTESIAN_POINT('Ctrl Pts',(-17.2318355104677,17.7192534840602,
5.7865945538288));
#196329=CARTESIAN_POINT('Ctrl Pts',(-17.2394711123522,17.7116037152801,
5.78724753721127));
#196330=CARTESIAN_POINT('Ctrl Pts',(-17.2715836106546,17.679920637143,5.78998386305156));
#196331=CARTESIAN_POINT('Ctrl Pts',(-17.2965831283632,17.6564266720209,
5.79209054250307));
#196332=CARTESIAN_POINT('Ctrl Pts',(-17.3631987245203,17.5968039285216,
5.79764748483304));
#196333=CARTESIAN_POINT('Ctrl Pts',(-17.4056721213409,17.5616761021321,
5.8011361756376));
#196334=CARTESIAN_POINT('Ctrl Pts',(-17.5364174871662,17.4618711576012,
5.8117087952138));
#196335=CARTESIAN_POINT('Ctrl Pts',(-17.628378576334,17.4023393397481,5.81894110457133));
#196336=CARTESIAN_POINT('Ctrl Pts',(-17.8285948623188,17.2937232366365,
5.83398768012246));
#196337=CARTESIAN_POINT('Ctrl Pts',(-17.9372370829309,17.2460867622619,
5.84177389782223));
#196338=CARTESIAN_POINT('Ctrl Pts',(-18.0583237921455,17.2046995424321,
5.84967785102848));
#196339=CARTESIAN_POINT('Ctrl Pts',(-18.0673646321356,17.2016774380356,
5.85026342187156));
#196340=CARTESIAN_POINT('Ctrl Pts',(-18.0807866039397,17.1972914046923,
5.85112567708158));
#196341=CARTESIAN_POINT('Ctrl Pts',(-18.0851521077671,17.1958805342439,
5.85140502152598));
#196342=CARTESIAN_POINT('Ctrl Pts',(-18.0929251048228,17.1933962873606,
5.85190040193272));
#196343=CARTESIAN_POINT('Ctrl Pts',(-18.0963307563977,17.1923173357591,
5.85211676194425));
#196344=CARTESIAN_POINT('Ctrl Pts',(-18.1036560369449,17.1900169860328,
5.85258065435672));
#196345=CARTESIAN_POINT('Ctrl Pts',(-18.1075764809091,17.1887983706138,
5.85282802294923));
#196346=CARTESIAN_POINT('Ctrl Pts',(-18.1184015830366,17.1854680397902,
5.85350862797166));
#196347=CARTESIAN_POINT('Ctrl Pts',(-18.1253136125156,17.1833802087406,
5.85394048789924));
#196348=CARTESIAN_POINT('Ctrl Pts',(-18.1631336266428,17.1721672104047,
5.85628931374581));
#196349=CARTESIAN_POINT('Ctrl Pts',(-18.1942380155433,17.1637128156178,
5.8581695646932));
#196350=CARTESIAN_POINT('Ctrl Pts',(-18.3836984204913,17.1168347097578,
5.86937957679986));
#196351=CARTESIAN_POINT('Ctrl Pts',(-18.5458775879473,17.0960859650852,
5.87799163459532));
#196352=CARTESIAN_POINT('Ctrl Pts',(-18.8257594220325,17.0927601852233,
5.89331438631325));
#196353=CARTESIAN_POINT('Ctrl Pts',(-18.9425714843823,17.1010586806702,
5.89984131559868));
#196354=CARTESIAN_POINT('Ctrl Pts',(-19.0722154209582,17.1211426925299,
5.90752687623506));
#196355=CARTESIAN_POINT('Ctrl Pts',(-19.0863153124905,17.1234734391554,
5.90836845593411));
#196356=CARTESIAN_POINT('Ctrl Pts',(-19.1087177474292,17.1274100456412,
5.90971512919105));
#196357=CARTESIAN_POINT('Ctrl Pts',(-19.1170362866386,17.1289232271365,
5.91021728090427));
#196358=CARTESIAN_POINT('Ctrl Pts',(-19.1316910526064,17.1316797942373,
5.91110571793882));
#196359=CARTESIAN_POINT('Ctrl Pts',(-19.1380311090591,17.1329024197831,
5.91149133711498));
#196360=CARTESIAN_POINT('Ctrl Pts',(-19.1511326181378,17.1354911559339,
5.91229084855421));
#196361=CARTESIAN_POINT('Ctrl Pts',(-19.15789317787,17.1368613462658,5.91270486711858));
#196362=CARTESIAN_POINT('Ctrl Pts',(-19.1752291546862,17.1404631971072,
5.91377033315474));
#196363=CARTESIAN_POINT('Ctrl Pts',(-19.1857943003088,17.1427428296988,
5.91442330988309));
#196364=CARTESIAN_POINT('Ctrl Pts',(-19.2298156142123,17.1525946650549,
5.91715957123579));
#196365=CARTESIAN_POINT('Ctrl Pts',(-19.2631011747635,17.1608982032967,
5.91926619147819));
#196366=CARTESIAN_POINT('Ctrl Pts',(-19.3492893336922,17.1846377670335,
5.92482294039926));
#196367=CARTESIAN_POINT('Ctrl Pts',(-19.4018143762248,17.2013363461486,
5.92831149366923));
#196368=CARTESIAN_POINT('Ctrl Pts',(-19.6495380313013,17.2908761807727,
5.94524262438293));
#196369=CARTESIAN_POINT('Ctrl Pts',(-19.8338999692612,17.3902055265442,
5.9594330960303));
#196370=CARTESIAN_POINT('Ctrl Pts',(-20.0044081025877,17.5175500468468,
5.97284956146776));
#196371=CARTESIAN_POINT('Ctrl Pts',(-20.0080262622954,17.5202704016807,
5.9731343409666));
#196372=CARTESIAN_POINT('Ctrl Pts',(-20.0280040859915,17.5353915014961,
5.9747071046111));
#196373=CARTESIAN_POINT('Ctrl Pts',(-20.0441921156617,17.5480186089009,
5.9759827930487));
#196374=CARTESIAN_POINT('Ctrl Pts',(-20.0652189787214,17.5649178084252,
5.97763868684087));
#196375=CARTESIAN_POINT('Ctrl Pts',(-20.070224983017,17.5689788832143,5.97803283113335));
#196376=CARTESIAN_POINT('Ctrl Pts',(-20.0782557942458,17.575554852066,5.97866488456012));
#196377=CARTESIAN_POINT('Ctrl Pts',(-20.0812922316185,17.5780553850578,
5.97890380565795));
#196378=CARTESIAN_POINT('Ctrl Pts',(-20.0869640878364,17.5827527987693,
5.9793499572337));
#196379=CARTESIAN_POINT('Ctrl Pts',(-20.0896011359208,17.5849476233226,
5.97955733017561));
#196380=CARTESIAN_POINT('Ctrl Pts',(-20.0958375189305,17.5901639021519,
5.98004763376747));
#196381=CARTESIAN_POINT('Ctrl Pts',(-20.0994321731156,17.5931909674969,
5.98033015555393));
#196382=CARTESIAN_POINT('Ctrl Pts',(-20.1106650992561,17.6027143449578,
5.98121283432028));
#196383=CARTESIAN_POINT('Ctrl Pts',(-20.1182674443845,17.6092530802175,
5.98180997166686));
#196384=CARTESIAN_POINT('Ctrl Pts',(-20.136093300074,17.6248067104469,5.98321032302283));
#196385=CARTESIAN_POINT('Ctrl Pts',(-20.1462768884792,17.633866909768,5.98401047099876));
#196386=CARTESIAN_POINT('Ctrl Pts',(-20.1816927556655,17.6659940541057,
5.98679666377056));
#196387=CARTESIAN_POINT('Ctrl Pts',(-20.206454279316,17.6895742430562,5.98875100413453));
#196388=CARTESIAN_POINT('Ctrl Pts',(-20.284326861425,17.7674145850838,5.99496011804458));
#196389=CARTESIAN_POINT('Ctrl Pts',(-20.3350961644106,17.8239366791848,
5.99910812051783));
#196390=CARTESIAN_POINT('Ctrl Pts',(-20.4906344006038,18.0170482748422,
6.01259290952664));
#196391=CARTESIAN_POINT('Ctrl Pts',(-20.5818013932796,18.1636660924551,
6.02185812120613));
#196392=CARTESIAN_POINT('Ctrl Pts',(-20.6640047949979,18.3407643008365,
6.0332008999858));
#196393=CARTESIAN_POINT('Ctrl Pts',(-20.6734378025314,18.3619949186689,
6.03456168596892));
#196394=CARTESIAN_POINT('Ctrl Pts',(-20.6862667084011,18.392198690298,6.03650083631797));
#196395=CARTESIAN_POINT('Ctrl Pts',(-20.689954142672,18.4010467466129,6.03706928387687));
#196396=CARTESIAN_POINT('Ctrl Pts',(-20.6958419121568,18.4154492468315,
6.03799531862334));
#196397=CARTESIAN_POINT('Ctrl Pts',(-20.6980790756813,18.4209885617876,
6.03835165511188));
#196398=CARTESIAN_POINT('Ctrl Pts',(-20.7027082005255,18.4325916804175,
6.03909846932074));
#196399=CARTESIAN_POINT('Ctrl Pts',(-20.7050956580236,18.4386572028839,
6.03948909424094));
#196400=CARTESIAN_POINT('Ctrl Pts',(-20.7107003746611,18.4530916820114,
6.04041927369869));
#196401=CARTESIAN_POINT('Ctrl Pts',(-20.7138925354333,18.4614701914324,
6.04095966393404));
#196402=CARTESIAN_POINT('Ctrl Pts',(-20.7244298539957,18.489664697399,6.0427798374509));
#196403=CARTESIAN_POINT('Ctrl Pts',(-20.7315313067871,18.5095698537705,
6.04406770366818));
#196404=CARTESIAN_POINT('Ctrl Pts',(-20.7683470824126,18.6178596171728,
6.05109151753182));
#196405=CARTESIAN_POINT('Ctrl Pts',(-20.792491513349,18.7080166308508,6.05700840220353));
#196406=CARTESIAN_POINT('Ctrl Pts',(-20.8375614472673,18.9354384765633,
6.07205895999174));
#196407=CARTESIAN_POINT('Ctrl Pts',(-20.8510859071177,19.0737188231497,
6.08133524835691));
#196408=CARTESIAN_POINT('Ctrl Pts',(-20.85099958945,19.2123184341987,6.09037084431718));
#196409=CARTESIAN_POINT('Ctrl Pts',(-20.7225806064498,19.9371103026755,
6.13370788222325));
#196410=CARTESIAN_POINT('Ctrl Pts',(-20.7475746254701,19.8686597913444,
6.12932688331225));
#196411=CARTESIAN_POINT('Ctrl Pts',(-20.7690040796656,19.7989891620996,
6.12494588440125));
#196412=CARTESIAN_POINT('Ctrl Pts',(-20.7867733146095,19.7285043176892,
6.12056488549025));
#196413=CARTESIAN_POINT('Ctrl Pts',(-20.8045716231428,19.6579041476937,
6.11617671849557));
#196414=CARTESIAN_POINT('Ctrl Pts',(-20.8186976743736,19.5864875772687,
6.11178855150089));
#196415=CARTESIAN_POINT('Ctrl Pts',(-20.829107237801,19.5146686716041,6.10740038450622));
#196416=CARTESIAN_POINT('Ctrl Pts',(-20.8314491136676,19.4985113213839,
6.10641316324043));
#196417=CARTESIAN_POINT('Ctrl Pts',(-20.8336030954032,19.4823336157705,
6.10542594197464));
#196418=CARTESIAN_POINT('Ctrl Pts',(-20.8355690425741,19.4661402737596,
6.10443872070885));
#196419=CARTESIAN_POINT('Ctrl Pts',(-20.8457798800574,19.3820344615431,
6.09931124014673));
#196420=CARTESIAN_POINT('Ctrl Pts',(-20.8509432233709,19.2973036553198,
6.09418375958461));
#196421=CARTESIAN_POINT('Ctrl Pts',(-20.8509995343428,19.212404133962,6.0890562790225));
#196422=CARTESIAN_POINT('Origin',(-18.734,19.211,0.));
#196423=CARTESIAN_POINT('',(-20.7225806520317,19.9371101778417,7.1561613891005));
#196424=CARTESIAN_POINT('',(-20.7193263846487,19.9359291807798,6.93361859104258));
#196425=CARTESIAN_POINT('',(-20.7225806064498,19.9371103026755,0.));
#196426=CARTESIAN_POINT('Ctrl Pts',(-20.7225806520317,19.9371101778416,
7.15616138910049));
#196427=CARTESIAN_POINT('Ctrl Pts',(-20.7474159484405,19.8690943430094,
7.15141138139249));
#196428=CARTESIAN_POINT('Ctrl Pts',(-20.7687705059422,19.7997803889042,
7.14660726507682));
#196429=CARTESIAN_POINT('Ctrl Pts',(-20.804820214685,19.6570554559655,7.13689820720307));
#196430=CARTESIAN_POINT('Ctrl Pts',(-20.8192617654728,19.5837555936372,
7.13200643852526));
#196431=CARTESIAN_POINT('Ctrl Pts',(-20.8346727888099,19.4756767824713,
7.12505658086314));
#196432=CARTESIAN_POINT('Ctrl Pts',(-20.8387085624094,19.4413956374211,
7.12289062882407));
#196433=CARTESIAN_POINT('Ctrl Pts',(-20.8425871755636,19.3996888097489,
7.12031417054245));
#196434=CARTESIAN_POINT('Ctrl Pts',(-20.8432314558288,19.392345011776,7.11986270620306));
#196435=CARTESIAN_POINT('Ctrl Pts',(-20.8441775334979,19.3808732048737,
7.11916106506936));
#196436=CARTESIAN_POINT('Ctrl Pts',(-20.844505601465,19.3767475051867,7.11890945347458));
#196437=CARTESIAN_POINT('Ctrl Pts',(-20.8450939760417,19.3690631383027,
7.11844219556558));
#196438=CARTESIAN_POINT('Ctrl Pts',(-20.8453573820951,19.3655048112482,
7.11822638305092));
#196439=CARTESIAN_POINT('Ctrl Pts',(-20.8459354331692,19.3574183335078,
7.1177371868206));
#196440=CARTESIAN_POINT('Ctrl Pts',(-20.8462445117178,19.3528898370633,
7.11746411802914));
#196441=CARTESIAN_POINT('Ctrl Pts',(-20.847008104894,19.3411461236721,7.11675818511216));
#196442=CARTESIAN_POINT('Ctrl Pts',(-20.8474402335132,19.3339294415992,
7.11632654499942));
#196443=CARTESIAN_POINT('Ctrl Pts',(-20.8499256632896,19.288524865479,7.11362366095009));
#196444=CARTESIAN_POINT('Ctrl Pts',(-20.8509809805453,19.2502868206115,
7.11140442024796));
#196445=CARTESIAN_POINT('Ctrl Pts',(-20.8510792904772,19.0499008437116,
7.09997626877871));
#196446=CARTESIAN_POINT('Ctrl Pts',(-20.8325322788689,18.8882767547124,
7.09141462739975));
#196447=CARTESIAN_POINT('Ctrl Pts',(-20.7706268732764,18.6227424192177,
7.07645435582679));
#196448=CARTESIAN_POINT('Ctrl Pts',(-20.7371602945164,18.5172852286702,
7.07026709047522));
#196449=CARTESIAN_POINT('Ctrl Pts',(-20.6902873326397,18.4017842691172,
7.06296369090374));
#196450=CARTESIAN_POINT('Ctrl Pts',(-20.684821191827,18.3886941628057,7.06212824975919));
#196451=CARTESIAN_POINT('Ctrl Pts',(-20.6758998544184,18.3679193835598,
7.0607895662524));
#196452=CARTESIAN_POINT('Ctrl Pts',(-20.6725295629709,18.3601985538532,
7.0602892107299));
#196453=CARTESIAN_POINT('Ctrl Pts',(-20.6664968925576,18.3466005626899,
7.05940286367353));
#196454=CARTESIAN_POINT('Ctrl Pts',(-20.6638535463824,18.3407150380137,
7.05901752822334));
#196455=CARTESIAN_POINT('Ctrl Pts',(-20.6583232643876,18.3285507203292,
7.05821753221439));
#196456=CARTESIAN_POINT('Ctrl Pts',(-20.6554324090558,18.3222738032876,
7.05780274005969));
#196457=CARTESIAN_POINT('Ctrl Pts',(-20.6479172872326,18.3061642795821,
7.05673301278907));
#196458=CARTESIAN_POINT('Ctrl Pts',(-20.6432480026516,18.2963530075546,
7.05607652474451));
#196459=CARTESIAN_POINT('Ctrl Pts',(-20.6233051496814,18.2552665307349,
7.05330602627178));
#196460=CARTESIAN_POINT('Ctrl Pts',(-20.6073377264045,18.2243359488252,
7.05116794373237));
#196461=CARTESIAN_POINT('Ctrl Pts',(-20.5636050560382,18.1445129866121,
7.04550809799605));
#196462=CARTESIAN_POINT('Ctrl Pts',(-20.5346432954162,18.096310776336,7.04194610903537));
#196463=CARTESIAN_POINT('Ctrl Pts',(-20.434764503102,17.9441469727673,7.03023625290669));
#196464=CARTESIAN_POINT('Ctrl Pts',(-20.3564951910324,17.8453422172027,
7.02187677949724));
#196465=CARTESIAN_POINT('Ctrl Pts',(-20.2011017406371,17.6815219570291,
7.00699928978879));
#196466=CARTESIAN_POINT('Ctrl Pts',(-20.1272124737288,17.6139231839679,
7.00047974092646));
#196467=CARTESIAN_POINT('Ctrl Pts',(-20.0412146249944,17.5457754210711,
6.99370038661416));
#196468=CARTESIAN_POINT('Ctrl Pts',(-20.0335754797707,17.5398068469953,
6.99310475478002));
#196469=CARTESIAN_POINT('Ctrl Pts',(-20.0222359705239,17.531071899654,6.99223059639909));
#196470=CARTESIAN_POINT('Ctrl Pts',(-20.0185672438359,17.5282649242732,
6.99194930443228));
#196471=CARTESIAN_POINT('Ctrl Pts',(-20.0120424370305,17.5233065105439,
6.99145177832036));
#196472=CARTESIAN_POINT('Ctrl Pts',(-20.0091900673442,17.521150279454,6.99123520933562));
#196473=CARTESIAN_POINT('Ctrl Pts',(-20.0030671636771,17.51654604004,6.99077231698397));
#196474=CARTESIAN_POINT('Ctrl Pts',(-19.9997950121448,17.5141002751413,
6.99052614983439));
#196475=CARTESIAN_POINT('Ctrl Pts',(-19.990793867831,17.5074129063896,6.98985223138026));
#196476=CARTESIAN_POINT('Ctrl Pts',(-19.9850504388006,17.5031906972378,
6.98942581219983));
#196477=CARTESIAN_POINT('Ctrl Pts',(-19.9542778843873,17.4808071889138,
6.98715958004473));
#196478=CARTESIAN_POINT('Ctrl Pts',(-19.9288730018968,17.463165907458,6.98535350185525));
#196479=CARTESIAN_POINT('Ctrl Pts',(-19.8508165769635,17.4114608631174,
6.97996802680115));
#196480=CARTESIAN_POINT('Ctrl Pts',(-19.7970274258183,17.3791718932772,
6.97647537940241));
#196481=CARTESIAN_POINT('Ctrl Pts',(-19.6236648602482,17.285316648407,6.96564100763522));
#196482=CARTESIAN_POINT('Ctrl Pts',(-19.4996236656572,17.2327227096628,
6.95847225909595));
#196483=CARTESIAN_POINT('Ctrl Pts',(-19.3325234696925,17.1799600140554,
6.94874721448145));
#196484=CARTESIAN_POINT('Ctrl Pts',(-19.2932699637651,17.1688024996675,
6.94645998174456));
#196485=CARTESIAN_POINT('Ctrl Pts',(-19.2066104760124,17.1468561155067,
6.94137924087289));
#196486=CARTESIAN_POINT('Ctrl Pts',(-19.1591071501854,17.1365521178183,
6.93857393472468));
#196487=CARTESIAN_POINT('Ctrl Pts',(-19.0988926627521,17.1256460301408,
6.9349749174683));
#196488=CARTESIAN_POINT('Ctrl Pts',(-19.0864718544085,17.1235107386015,
6.93423027297472));
#196489=CARTESIAN_POINT('Ctrl Pts',(-19.0667599272158,17.1203029564151,
6.93304466656341));
#196490=CARTESIAN_POINT('Ctrl Pts',(-19.0594808772578,17.1191573927158,
6.93260602739138));
#196491=CARTESIAN_POINT('Ctrl Pts',(-19.0459068925946,17.1170937083349,
6.93178645097233));
#196492=CARTESIAN_POINT('Ctrl Pts',(-19.0396134965892,17.1161659117588,
6.93140582537003));
#196493=CARTESIAN_POINT('Ctrl Pts',(-19.0256263745375,17.1141682482353,
6.93055842098074));
#196494=CARTESIAN_POINT('Ctrl Pts',(-19.017930776983,17.1131123364422,6.93009120589956));
#196495=CARTESIAN_POINT('Ctrl Pts',(-18.995553342206,17.110167314363,6.92872969528718));
#196496=CARTESIAN_POINT('Ctrl Pts',(-18.980857510327,17.1083898421266,6.92783189143561));
#196497=CARTESIAN_POINT('Ctrl Pts',(-18.8639363752578,17.0954907962451,
6.92065851496285));
#196498=CARTESIAN_POINT('Ctrl Pts',(-18.7610577829605,17.0916781524953,
6.91415212142113));
#196499=CARTESIAN_POINT('Ctrl Pts',(-18.5026291718104,17.1009223459463,
6.8973658959693));
#196500=CARTESIAN_POINT('Ctrl Pts',(-18.3480384893603,17.123659548595,6.88689556588299));
#196501=CARTESIAN_POINT('Ctrl Pts',(-18.1465318942574,17.1764657291575,
6.87343968836));
#196502=CARTESIAN_POINT('Ctrl Pts',(-18.0962255101378,17.1916701186656,
6.87010195033607));
#196503=CARTESIAN_POINT('Ctrl Pts',(-18.0383148380403,17.2115534137393,
6.86632510580336));
#196504=CARTESIAN_POINT('Ctrl Pts',(-18.03011418316,17.2144256190468,6.86579183522964));
#196505=CARTESIAN_POINT('Ctrl Pts',(-18.017715663448,17.2188539742878,6.86498821128459));
#196506=CARTESIAN_POINT('Ctrl Pts',(-18.0135047835897,17.22037304285,6.86471573915166));
#196507=CARTESIAN_POINT('Ctrl Pts',(-18.0059505318238,17.2231253383946,
6.86422779793998));
#196508=CARTESIAN_POINT('Ctrl Pts',(-18.0026054427477,17.2243536548834,
6.86401204304164));
#196509=CARTESIAN_POINT('Ctrl Pts',(-17.9953385679417,17.2270428929411,
6.86354401496542));
#196510=CARTESIAN_POINT('Ctrl Pts',(-17.9914180204604,17.2285069941563,
6.86329193466112));
#196511=CARTESIAN_POINT('Ctrl Pts',(-17.9804047509988,17.2326570770059,
6.86258494077132));
#196512=CARTESIAN_POINT('Ctrl Pts',(-17.9733220014942,17.2353695925575,
6.86213158514618));
#196513=CARTESIAN_POINT('Ctrl Pts',(-17.9308014885549,17.2519164490607,
6.85941699620796));
#196514=CARTESIAN_POINT('Ctrl Pts',(-17.8957249109265,17.2666668265909,
6.85720729545368));
#196515=CARTESIAN_POINT('Ctrl Pts',(-17.7810018099989,17.3185924623995,
6.85001919777146));
#196516=CARTESIAN_POINT('Ctrl Pts',(-17.7032684351311,17.3597823663654,
6.84521015032519));
#196517=CARTESIAN_POINT('Ctrl Pts',(-17.4797361855879,17.4966873266967,
6.83095048302239));
#196518=CARTESIAN_POINT('Ctrl Pts',(-17.3429762592581,17.6056676806631,
6.8215775166648));
#196519=CARTESIAN_POINT('Ctrl Pts',(-17.2049682210269,17.746662712521,6.81011397695195));
#196520=CARTESIAN_POINT('Ctrl Pts',(-17.1890924168149,17.7634218948917,
6.80876166928866));
#196521=CARTESIAN_POINT('Ctrl Pts',(-17.1670331356938,17.7874848904002,
6.80683255740365));
#196522=CARTESIAN_POINT('Ctrl Pts',(-17.160619897499,17.7945765218028,6.80626552955011));
#196523=CARTESIAN_POINT('Ctrl Pts',(-17.1502810119813,17.8061659160412,
6.80534117894736));
#196524=CARTESIAN_POINT('Ctrl Pts',(-17.1463259169105,17.8106373179689,
6.80498509777216));
#196525=CARTESIAN_POINT('Ctrl Pts',(-17.1380892762196,17.8200289357792,
6.80423830760795));
#196526=CARTESIAN_POINT('Ctrl Pts',(-17.1338114564981,17.8249523227737,
6.80384744916028));
#196527=CARTESIAN_POINT('Ctrl Pts',(-17.1236935921876,17.8367063500857,
6.8029157725516));
#196528=CARTESIAN_POINT('Ctrl Pts',(-17.1178741922442,17.8435545228971,
6.80237411150478));
#196529=CARTESIAN_POINT('Ctrl Pts',(-17.098437849695,17.8667242602627,6.80054520621698));
#196530=CARTESIAN_POINT('Ctrl Pts',(-17.0850235049045,17.8832133910639,
6.79924977295498));
#196531=CARTESIAN_POINT('Ctrl Pts',(-17.0134819153951,17.973909939644,6.79215509273577));
#196532=CARTESIAN_POINT('Ctrl Pts',(-16.960119539907,18.051725096893,6.78617079542213));
#196533=CARTESIAN_POINT('Ctrl Pts',(-16.8276106994564,18.2756361114449,
6.76927204727213));
#196534=CARTESIAN_POINT('Ctrl Pts',(-16.7601866743178,18.427875982354,6.75808945758863));
#196535=CARTESIAN_POINT('Ctrl Pts',(-16.6988405050568,18.6265525091958,
6.74476051668973));
#196536=CARTESIAN_POINT('Ctrl Pts',(-16.6876451407811,18.667046533975,6.74210942100237));
#196537=CARTESIAN_POINT('Ctrl Pts',(-16.6758936051212,18.7150742148555,
6.73906264223644));
#196538=CARTESIAN_POINT('Ctrl Pts',(-16.6741639689389,18.7223080255509,
6.73860632595696));
#196539=CARTESIAN_POINT('Ctrl Pts',(-16.6714258940046,18.7340322496468,
6.73787109212545));
#196540=CARTESIAN_POINT('Ctrl Pts',(-16.6703939285332,18.7385170264142,
6.73759087448883));
#196541=CARTESIAN_POINT('Ctrl Pts',(-16.6685865293825,18.7464906159896,
6.73709453390167));
#196542=CARTESIAN_POINT('Ctrl Pts',(-16.6678052991537,18.7499780576742,
6.73687808206201));
#196543=CARTESIAN_POINT('Ctrl Pts',(-16.666147599959,18.7574669464904,6.73641464663031));
#196544=CARTESIAN_POINT('Ctrl Pts',(-16.665273914459,18.7614689525322,6.73616782341115));
#196545=CARTESIAN_POINT('Ctrl Pts',(-16.6629011176809,18.7724912199035,
6.73549025550176));
#196546=CARTESIAN_POINT('Ctrl Pts',(-16.6614260730888,18.7795166846653,
6.73506086707742));
#196547=CARTESIAN_POINT('Ctrl Pts',(-16.6536456238116,18.817534686077,6.73275000685802));
#196548=CARTESIAN_POINT('Ctrl Pts',(-16.6479992476788,18.8486598462564,
6.73090386350648));
#196549=CARTESIAN_POINT('Ctrl Pts',(-16.6174874829022,19.0413473482141,
6.71969127953706));
#196550=CARTESIAN_POINT('Ctrl Pts',(-16.6107039487309,19.2052275802291,
6.71105303120492));
#196551=CARTESIAN_POINT('Ctrl Pts',(-16.6315476577752,19.4850274368413,
6.69569421920797));
#196552=CARTESIAN_POINT('Ctrl Pts',(-16.6499147097709,19.6008462592448,
6.68915893316017));
#196553=CARTESIAN_POINT('Ctrl Pts',(-16.6811576349148,19.7284277916752,
6.68146396571602));
#196554=CARTESIAN_POINT('Ctrl Pts',(-16.6846978299566,19.7422757254214,
6.68062226628924));
#196555=CARTESIAN_POINT('Ctrl Pts',(-16.6905550866421,19.7642570689267,
6.6792754372436));
#196556=CARTESIAN_POINT('Ctrl Pts',(-16.6927811641099,19.7724144272182,
6.67877325054711));
#196557=CARTESIAN_POINT('Ctrl Pts',(-16.6967932165038,19.786777052302,6.67788477276624));
#196558=CARTESIAN_POINT('Ctrl Pts',(-16.6985588336342,19.7929879290143,
6.67749914802318));
#196559=CARTESIAN_POINT('Ctrl Pts',(-16.7022693161085,19.8058167849814,
6.67669964580785));
#196560=CARTESIAN_POINT('Ctrl Pts',(-16.7042181656882,19.8124335232657,
6.6762856421367));
#196561=CARTESIAN_POINT('Ctrl Pts',(-16.7093033174183,19.8293923824911,
6.67522025816239));
#196562=CARTESIAN_POINT('Ctrl Pts',(-16.7124865114523,19.8397201317102,
6.67456734905721));
#196563=CARTESIAN_POINT('Ctrl Pts',(-16.7260999404175,19.8827159645232,
6.6718317429244));
#196564=CARTESIAN_POINT('Ctrl Pts',(-16.7372436170309,19.9151510614031,
6.66972572425325));
#196565=CARTESIAN_POINT('Ctrl Pts',(-16.7683257312138,19.9989385695156,
6.66417094024307));
#196566=CARTESIAN_POINT('Ctrl Pts',(-16.7894882993709,20.0498062628873,
6.66068378418232));
#196567=CARTESIAN_POINT('Ctrl Pts',(-16.8585267617138,20.1990543854575,
6.65011411278765));
#196568=CARTESIAN_POINT('Ctrl Pts',(-16.9120656113153,20.2946064567013,
6.64288320705827));
#196569=CARTESIAN_POINT('Ctrl Pts',(-16.9983212096584,20.4239442703683,
6.63261379142985));
#196570=CARTESIAN_POINT('Ctrl Pts',(-17.0251487058255,20.4614567637566,
6.62957390294652));
#196571=CARTESIAN_POINT('Ctrl Pts',(-17.0664506570113,20.5153943539174,
6.62513730781065));
#196572=CARTESIAN_POINT('Ctrl Pts',(-17.0799886265947,20.5325187718193,
6.62371857433765));
#196573=CARTESIAN_POINT('Ctrl Pts',(-17.1264807415379,20.5894935841201,
6.61897107655121));
#196574=CARTESIAN_POINT('Ctrl Pts',(-17.1606320400863,20.6283485614777,
6.61568726421669));
#196575=CARTESIAN_POINT('Ctrl Pts',(-17.2021191079627,20.6721997602585,
6.61196390906098));
#196576=CARTESIAN_POINT('Ctrl Pts',(-17.2081017951444,20.6784462446857,
6.611433107483));
#196577=CARTESIAN_POINT('Ctrl Pts',(-17.2172328180984,20.68786366253,6.61063245937614));
#196578=CARTESIAN_POINT('Ctrl Pts',(-17.2203531029418,20.6910614965833,
6.61036051703167));
#196579=CARTESIAN_POINT('Ctrl Pts',(-17.2259798538746,20.6967916857548,
6.60987313972427));
#196580=CARTESIAN_POINT('Ctrl Pts',(-17.2284825974368,20.6993276002713,
6.60965742190244));
#196581=CARTESIAN_POINT('Ctrl Pts',(-17.2339436879374,20.7048332004119,
6.60918903127947));
#196582=CARTESIAN_POINT('Ctrl Pts',(-17.2369044465714,20.7078004124182,
6.60893655375838));
#196583=CARTESIAN_POINT('Ctrl Pts',(-17.2452688562879,20.7161334066703,
6.60822732145767));
#196584=CARTESIAN_POINT('Ctrl Pts',(-17.2506927376745,20.7214789173162,
6.60777214049947));
#196585=CARTESIAN_POINT('Ctrl Pts',(-17.2837779319999,20.7537359843825,
6.60502316864112));
#196586=CARTESIAN_POINT('Ctrl Pts',(-17.3121439347961,20.7799181356111,
6.60278244002634));
#196587=CARTESIAN_POINT('Ctrl Pts',(-17.409060098475,20.8645839310836,6.59544077474898));
#196588=CARTESIAN_POINT('Ctrl Pts',(-17.4806283980295,20.919469422023,6.59051754334627));
#196589=CARTESIAN_POINT('Ctrl Pts',(-17.6976390539644,21.0648956765038,
6.57631271833151));
#196590=CARTESIAN_POINT('Ctrl Pts',(-17.8508044851328,21.1425620640347,
6.56709216618477));
#196591=CARTESIAN_POINT('Ctrl Pts',(-18.033530476002,21.208892315459,6.55579961310107));
#196592=CARTESIAN_POINT('Ctrl Pts',(-18.0555482980019,21.2164761237761,
6.5544356318778));
#196593=CARTESIAN_POINT('Ctrl Pts',(-18.0868082411315,21.2266695881688,
6.5524926962936));
#196594=CARTESIAN_POINT('Ctrl Pts',(-18.0959503648643,21.2295821063095,
6.55192371190417));
#196595=CARTESIAN_POINT('Ctrl Pts',(-18.1108178102877,21.2342075196495,
6.55099704011313));
#196596=CARTESIAN_POINT('Ctrl Pts',(-18.1165312065234,21.2359585173766,
6.55064060686663));
#196597=CARTESIAN_POINT('Ctrl Pts',(-18.1284909605486,21.239568528711,6.54989378227633));
#196598=CARTESIAN_POINT('Ctrl Pts',(-18.1347386340321,21.2414229328685,
6.54950324458259));
#196599=CARTESIAN_POINT('Ctrl Pts',(-18.1495943130068,21.2457577848136,
6.54857362602149));
#196600=CARTESIAN_POINT('Ctrl Pts',(-18.1582096447353,21.2482124859175,
6.5480337121475));
#196601=CARTESIAN_POINT('Ctrl Pts',(-18.1871570075988,21.2562619470124,
6.54621680396353));
#196602=CARTESIAN_POINT('Ctrl Pts',(-18.2075564953543,21.2616074407743,
6.54493176620196));
#196603=CARTESIAN_POINT('Ctrl Pts',(-18.3182065143664,21.2888423594308,
6.53793434184216));
#196604=CARTESIAN_POINT('Ctrl Pts',(-18.4097320175698,21.3050772261686,
6.53204253693035));
#196605=CARTESIAN_POINT('Ctrl Pts',(-18.6540738514673,21.3320145923123,
6.51608767430365));
#196606=CARTESIAN_POINT('Ctrl Pts',(-18.8074878043951,21.3322465440226,
6.50581418189735));
#196607=CARTESIAN_POINT('Ctrl Pts',(-18.9637890465428,21.3154961144103,
6.49564082129242));
#196608=CARTESIAN_POINT('Ctrl Pts',(-18.9679946320586,21.31503265517,6.49536734032383));
#196609=CARTESIAN_POINT('Ctrl Pts',(-19.0233901029746,21.308759880766,6.49176863443538));
#196610=CARTESIAN_POINT('Ctrl Pts',(-19.0743574849866,21.3010959012391,
6.48849724382151));
#196611=CARTESIAN_POINT('Ctrl Pts',(-19.1334909402154,21.2899830820584,
6.48478614725468));
#196612=CARTESIAN_POINT('Ctrl Pts',(-19.141973591269,21.2883351249777,6.48425584852443));
#196613=CARTESIAN_POINT('Ctrl Pts',(-19.1548249262914,21.2857566911744,
6.48345580664324));
#196614=CARTESIAN_POINT('Ctrl Pts',(-19.1592010294498,21.2848642751063,
6.48318397233643));
#196615=CARTESIAN_POINT('Ctrl Pts',(-19.1670630405896,21.2832350486138,
6.48269670983927));
#196616=CARTESIAN_POINT('Ctrl Pts',(-19.1705499242318,21.2825032845863,
6.48248099939427));
#196617=CARTESIAN_POINT('Ctrl Pts',(-19.1781364844311,21.2808911480469,
6.48201253399976));
#196618=CARTESIAN_POINT('Ctrl Pts',(-19.1822353846312,21.2800074002357,
6.48175997482424));
#196619=CARTESIAN_POINT('Ctrl Pts',(-19.1937771523654,21.2774830164301,
6.48105028209307));
#196620=CARTESIAN_POINT('Ctrl Pts',(-19.2012139118971,21.2758143382789,
6.48059472563071));
#196621=CARTESIAN_POINT('Ctrl Pts',(-19.2463629007858,21.2654272837154,
6.47783860814311));
#196622=CARTESIAN_POINT('Ctrl Pts',(-19.2838417977379,21.2557155375536,
6.47559143028487));
#196623=CARTESIAN_POINT('Ctrl Pts',(-19.4080422008667,21.2198695309842,
6.46821752830712));
#196624=CARTESIAN_POINT('Ctrl Pts',(-19.493354889713,21.1891992921138,6.46327028952659));
#196625=CARTESIAN_POINT('Ctrl Pts',(-19.6380711399754,21.1264259320897,
6.45469347809467));
#196626=CARTESIAN_POINT('Ctrl Pts',(-19.6983881938933,21.096777397878,6.4510591451169));
#196627=CARTESIAN_POINT('Ctrl Pts',(-19.8577506079979,21.008795194398,6.44108688046683));
#196628=CARTESIAN_POINT('Ctrl Pts',(-19.953610171947,20.9451940339582,6.4346682451235));
#196629=CARTESIAN_POINT('Ctrl Pts',(-20.05503703672,20.8653136257788,6.42710452864922));
#196630=CARTESIAN_POINT('Ctrl Pts',(-20.0661522976138,20.8563761472563,
6.42626460005117));
#196631=CARTESIAN_POINT('Ctrl Pts',(-20.083705142669,20.8419679263199,6.42492007541292));
#196632=CARTESIAN_POINT('Ctrl Pts',(-20.0902018760824,20.8365696899818,
6.42441840637474));
#196633=CARTESIAN_POINT('Ctrl Pts',(-20.101606460532,20.8269774884282,6.42353053142399));
#196634=CARTESIAN_POINT('Ctrl Pts',(-20.106527787608,20.8227996602601,6.42314498895113));
#196635=CARTESIAN_POINT('Ctrl Pts',(-20.111652681476,20.8184085278175,6.42274095410773));
#196636=CARTESIAN_POINT('Ctrl Pts',(-20.1118754359795,20.81821758608,6.42272338760807));
#196637=CARTESIAN_POINT('Ctrl Pts',(-20.1122323321248,20.8179115314575,
6.42269523455801));
#196638=CARTESIAN_POINT('Ctrl Pts',(-20.1123664976654,20.8177964492612,
6.42268464934));
#196639=CARTESIAN_POINT('Ctrl Pts',(-20.1125825233666,20.8176111035055,
6.42266760267269));
#196640=CARTESIAN_POINT('Ctrl Pts',(-20.1126643933786,20.8175408497975,
6.42266114159677));
#196641=CARTESIAN_POINT('Ctrl Pts',(-20.1128530619556,20.8173789258285,
6.42264625054099));
#196642=CARTESIAN_POINT('Ctrl Pts',(-20.1129598580791,20.8172872500319,
6.42263782027382));
#196643=CARTESIAN_POINT('Ctrl Pts',(-20.1131635444003,20.8171123665886,
6.42262173947406));
#196644=CARTESIAN_POINT('Ctrl Pts',(-20.1132604385858,20.8170291587835,
6.42261408883189));
#196645=CARTESIAN_POINT('Ctrl Pts',(-20.1134453820028,20.8168703096903,
6.4225994841047));
#196646=CARTESIAN_POINT('Ctrl Pts',(-20.1135334334701,20.8167946691315,
6.42259253000973));
#196647=CARTESIAN_POINT('Ctrl Pts',(-20.1137016140503,20.816650169666,6.42257924599601));
#196648=CARTESIAN_POINT('Ctrl Pts',(-20.1137817453715,20.816581311022,6.42257291603884));
#196649=CARTESIAN_POINT('Ctrl Pts',(-20.1139349047252,20.8164496778142,
6.42256081599268));
#196650=CARTESIAN_POINT('Ctrl Pts',(-20.1140079293599,20.8163869079373,
6.42255504628345));
#196651=CARTESIAN_POINT('Ctrl Pts',(-20.1141475825316,20.8162668495155,
6.42254401118085));
#196652=CARTESIAN_POINT('Ctrl Pts',(-20.1142142117707,20.8162095618166,
6.42253874582322));
#196653=CARTESIAN_POINT('Ctrl Pts',(-20.1143417033352,20.8160999309942,
6.42252866996785));
#196654=CARTESIAN_POINT('Ctrl Pts',(-20.1144025662271,20.8160475885773,
6.42252385950047));
#196655=CARTESIAN_POINT('Ctrl Pts',(-20.1145190819811,20.8159473728678,
6.42251464962918));
#196656=CARTESIAN_POINT('Ctrl Pts',(-20.1145747354105,20.8158995000732,
6.42251025024249));
#196657=CARTESIAN_POINT('Ctrl Pts',(-20.1146813267376,20.8158078011132,
6.42250182362322));
#196658=CARTESIAN_POINT('Ctrl Pts',(-20.1147322651533,20.8157639753185,
6.42249779640108));
#196659=CARTESIAN_POINT('Ctrl Pts',(-20.1148298672938,20.8156799934502,
6.42249007940737));
#196660=CARTESIAN_POINT('Ctrl Pts',(-20.1148765312182,20.8156398378828,
6.4224863896627));
#196661=CARTESIAN_POINT('Ctrl Pts',(-20.1149659774766,20.8155628601704,
6.42247931666552));
#196662=CARTESIAN_POINT('Ctrl Pts',(-20.1150087600802,20.8155260383577,
6.42247593342723));
#196663=CARTESIAN_POINT('Ctrl Pts',(-20.1150907957113,20.81545542683,6.42246944570909));
#196664=CARTESIAN_POINT('Ctrl Pts',(-20.1151300489563,20.8154216373985,
6.42246634124169));
#196665=CARTESIAN_POINT('Ctrl Pts',(-20.1152263508583,20.815338733984,6.42245872451287));
#196666=CARTESIAN_POINT('Ctrl Pts',(-20.1152833981331,20.8152896184,6.4224542121849));
#196667=CARTESIAN_POINT('Ctrl Pts',(-20.1153964173092,20.8151923025939,
6.42244527192838));
#196668=CARTESIAN_POINT('Ctrl Pts',(-20.1154523954955,20.8151440971553,
6.42244084351495));
#196669=CARTESIAN_POINT('Ctrl Pts',(-20.1155633300425,20.8150485561047,
6.42243206688703));
#196670=CARTESIAN_POINT('Ctrl Pts',(-20.1156182802615,20.8150012259681,
6.4224277191703));
#196671=CARTESIAN_POINT('Ctrl Pts',(-20.1157271840613,20.8149074143782,
6.42241910197791));
#196672=CARTESIAN_POINT('Ctrl Pts',(-20.1157811377431,20.8148609330141,
6.42241483250535));
#196673=CARTESIAN_POINT('Ctrl Pts',(-20.1158880806818,20.814768791741,6.42240636928512));
#196674=CARTESIAN_POINT('Ctrl Pts',(-20.1159410700041,20.8147231319429,
6.4224021755428));
#196675=CARTESIAN_POINT('Ctrl Pts',(-20.1160461150854,20.8146326077067,
6.42239386137188));
#196676=CARTESIAN_POINT('Ctrl Pts',(-20.1160981709156,20.8145877433662,
6.42238974094765));
#196677=CARTESIAN_POINT('Ctrl Pts',(-20.1162013787273,20.8144987849092,
6.42238157109064));
#196678=CARTESIAN_POINT('Ctrl Pts',(-20.1162525307486,20.8144546909096,
6.42237752166424));
#196679=CARTESIAN_POINT('Ctrl Pts',(-20.1219737525498,20.8095224134375,
6.4219245736898));
#196680=CARTESIAN_POINT('Ctrl Pts',(-20.1276177980228,20.8046042403366,
6.42147443244445));
#196681=CARTESIAN_POINT('Ctrl Pts',(-20.143432311124,20.7906753435144,6.42020372841422));
#196682=CARTESIAN_POINT('Ctrl Pts',(-20.1535421456085,20.7815966108094,
6.41938032429356));
#196683=CARTESIAN_POINT('Ctrl Pts',(-20.17605592011,20.7609840613083,6.41752129041665));
#196684=CARTESIAN_POINT('Ctrl Pts',(-20.1884101370702,20.7493975409849,
6.41648345144874));
#196685=CARTESIAN_POINT('Ctrl Pts',(-20.2267855313752,20.7125313719577,
6.41320286292116));
#196686=CARTESIAN_POINT('Ctrl Pts',(-20.2522956523426,20.6867314009479,
6.41093806964548));
#196687=CARTESIAN_POINT('Ctrl Pts',(-20.3332489087791,20.6005365479115,
6.40346954403985));
#196688=CARTESIAN_POINT('Ctrl Pts',(-20.3858454393956,20.5375795423985,
6.39816081263688));
#196689=CARTESIAN_POINT('Ctrl Pts',(-20.4744527974017,20.4180537661683,
6.38839567876478));
#196690=CARTESIAN_POINT('Ctrl Pts',(-20.5116850375621,20.3625165480716,
6.38396924015682));
#196691=CARTESIAN_POINT('Ctrl Pts',(-20.5679592240902,20.2693241531686,
6.37678464319172));
#196692=CARTESIAN_POINT('Ctrl Pts',(-20.5886146683364,20.2326951918525,
6.3740185151432));
#196693=CARTESIAN_POINT('Ctrl Pts',(-20.6155608226734,20.1813971995547,
6.37024248010079));
#196694=CARTESIAN_POINT('Ctrl Pts',(-20.6227967858953,20.1672366726796,
6.36921014956012));
#196695=CARTESIAN_POINT('Ctrl Pts',(-20.6533657214605,20.1057132414828,
6.36477175695282));
#196696=CARTESIAN_POINT('Ctrl Pts',(-20.6750839771968,20.0575639723816,
6.36141656965233));
#196697=CARTESIAN_POINT('Ctrl Pts',(-20.6982561911844,20.0005962193275,
6.35762296356075));
#196698=CARTESIAN_POINT('Ctrl Pts',(-20.70148212357,19.9925233032807,6.35708941315014));
#196699=CARTESIAN_POINT('Ctrl Pts',(-20.7062940891013,19.9802626816277,
6.35628545200047));
#196700=CARTESIAN_POINT('Ctrl Pts',(-20.7079166710991,19.9760895527051,
6.3560129198921));
#196701=CARTESIAN_POINT('Ctrl Pts',(-20.7108068575052,19.9685858676909,
6.35552491474905));
#196702=CARTESIAN_POINT('Ctrl Pts',(-20.7120792971525,19.9652572462766,
6.35530915555972));
#196703=CARTESIAN_POINT('Ctrl Pts',(-20.7148275429871,19.9580132211009,
6.35484116809913));
#196704=CARTESIAN_POINT('Ctrl Pts',(-20.7163001432577,19.9540966628185,
6.35458913243066));
#196705=CARTESIAN_POINT('Ctrl Pts',(-20.7193819323901,19.9458259183912,
6.35405892678559));
#196706=CARTESIAN_POINT('Ctrl Pts',(-20.7209884312978,19.9414707539978,
6.35378091562846));
#196707=CARTESIAN_POINT('Ctrl Pts',(-20.7225806064498,19.9371103026756,
6.35350371400671));
#196708=CARTESIAN_POINT('',(-20.8509992748742,19.2092478064745,6.8890562790225));
#196709=CARTESIAN_POINT('Ctrl Pts',(-20.8509992748742,19.2092478064745,
6.8890562790225));
#196710=CARTESIAN_POINT('Ctrl Pts',(-20.8509006165464,19.0900488678703,
6.88186870628081));
#196711=CARTESIAN_POINT('Ctrl Pts',(-20.8407310772906,18.9712546433194,
6.87468113353913));
#196712=CARTESIAN_POINT('Ctrl Pts',(-20.8207141748805,18.8541905938,6.86749356079745));
#196713=CARTESIAN_POINT('Ctrl Pts',(-20.8084933107471,18.7827198030267,
6.86310535186655));
#196714=CARTESIAN_POINT('Ctrl Pts',(-20.7925724893354,18.7117380828087,
6.85871714293565));
#196715=CARTESIAN_POINT('Ctrl Pts',(-20.7730042905685,18.6416578330713,
6.85432893400475));
#196716=CARTESIAN_POINT('Ctrl Pts',(-20.7534651342531,18.5716815940441,
6.84994723790348));
#196717=CARTESIAN_POINT('Ctrl Pts',(-20.7302894754045,18.5026046302858,
6.84556554180221));
#196718=CARTESIAN_POINT('Ctrl Pts',(-20.7035811449958,18.4348304867639,
6.84118384570094));
#196719=CARTESIAN_POINT('Ctrl Pts',(-20.6769041990008,18.3671359832543,
6.8368072984413));
#196720=CARTESIAN_POINT('Ctrl Pts',(-20.6467030037516,18.3007417053632,
6.83243075118166));
#196721=CARTESIAN_POINT('Ctrl Pts',(-20.6131310722286,18.2360356860966,
6.82805420392202));
#196722=CARTESIAN_POINT('Ctrl Pts',(-20.5795804315366,18.171370702447,6.82368043220504));
#196723=CARTESIAN_POINT('Ctrl Pts',(-20.5426635175971,18.1083922801994,
6.81930666048806));
#196724=CARTESIAN_POINT('Ctrl Pts',(-20.5025812162806,18.0474668112085,
6.81493288877108));
#196725=CARTESIAN_POINT('Ctrl Pts',(-20.462511112143,17.9865598820423,6.81056044800752));
#196726=CARTESIAN_POINT('Ctrl Pts',(-20.419277797915,17.9277050686151,6.80618800724397));
#196727=CARTESIAN_POINT('Ctrl Pts',(-20.3731263263944,17.87124110896,6.80181556648041));
#196728=CARTESIAN_POINT('Ctrl Pts',(-20.3269736747756,17.8147757055152,
6.79744301391307));
#196729=CARTESIAN_POINT('Ctrl Pts',(-20.2779030245425,17.7607016494435,
6.79307046134572));
#196730=CARTESIAN_POINT('Ctrl Pts',(-20.2261996115099,17.709324495968,6.78869790877838));
#196731=CARTESIAN_POINT('Ctrl Pts',(-20.1744425387249,17.6578940213447,
6.78432081821105));
#196732=CARTESIAN_POINT('Ctrl Pts',(-20.120047590661,17.6091663783431,6.77994372764372));
#196733=CARTESIAN_POINT('Ctrl Pts',(-20.0633361651207,17.5634095290084,
6.77556663707639));
#196734=CARTESIAN_POINT('Ctrl Pts',(-20.006593767366,17.5176276901601,6.77118715601744));
#196735=CARTESIAN_POINT('Ctrl Pts',(-19.9475327641501,17.4748201585675,
6.76680767495849));
#196736=CARTESIAN_POINT('Ctrl Pts',(-19.8865046696903,17.4352122913079,
6.76242819389955));
#196737=CARTESIAN_POINT('Ctrl Pts',(-19.8253684033427,17.3955342193693,
6.75804095023982));
#196738=CARTESIAN_POINT('Ctrl Pts',(-19.7622585010731,17.3590673788382,
6.7536537065801));
#196739=CARTESIAN_POINT('Ctrl Pts',(-19.6975517419859,17.3259915012086,
6.74926646292037));
#196740=CARTESIAN_POINT('Ctrl Pts',(-19.6535573809355,17.3035030916047,
6.74628355998558));
#196741=CARTESIAN_POINT('Ctrl Pts',(-19.6088253272203,17.2825812380497,
6.74330065705079));
#196742=CARTESIAN_POINT('Ctrl Pts',(-19.5634785608967,17.2632694444527,
6.74031775411601));
#196743=CARTESIAN_POINT('Ctrl Pts',(-19.496768014386,17.2348594737004,6.73592954518511));
#196744=CARTESIAN_POINT('Ctrl Pts',(-19.4284659821156,17.2098253061038,
6.73154133625421));
#196745=CARTESIAN_POINT('Ctrl Pts',(-19.3589476876742,17.1883459545264,
6.72715312732332));
#196746=CARTESIAN_POINT('Ctrl Pts',(-19.2895325699082,17.1668984818681,
6.72277143122206));
#196747=CARTESIAN_POINT('Ctrl Pts',(-19.2189052304805,17.1489954929981,
6.71838973512079));
#196748=CARTESIAN_POINT('Ctrl Pts',(-19.1474611885827,17.1347681137369,
6.71400803901953));
#196749=CARTESIAN_POINT('Ctrl Pts',(-19.0761010991198,17.1205574527785,
6.70963149175989));
#196750=CARTESIAN_POINT('Ctrl Pts',(-19.0039266843584,17.1100139151849,
6.70525494450025));
#196751=CARTESIAN_POINT('Ctrl Pts',(-18.9313473123135,17.1032184557401,
6.70087839724061));
#196752=CARTESIAN_POINT('Ctrl Pts',(-18.8588139690515,17.0964273058769,
6.69650462552364));
#196753=CARTESIAN_POINT('Ctrl Pts',(-18.7858766571619,17.0933795627893,
6.69213085380667));
#196754=CARTESIAN_POINT('Ctrl Pts',(-18.7129521899235,17.0941046342129,
6.6877570820897));
#196755=CARTESIAN_POINT('Ctrl Pts',(-18.6400499138453,17.0948294849948,
6.68338464132615));
#196756=CARTESIAN_POINT('Ctrl Pts',(-18.5671609567223,17.0993248662018,
6.6790122005626));
#196757=CARTESIAN_POINT('Ctrl Pts',(-18.4947027860656,17.1075680796842,
6.67463975979905));
#196758=CARTESIAN_POINT('Ctrl Pts',(-18.4222427626455,17.1158115039466,
6.67026720723171));
#196759=CARTESIAN_POINT('Ctrl Pts',(-18.3502140266214,17.1278028942377,
6.66589465466437));
#196760=CARTESIAN_POINT('Ctrl Pts',(-18.2790278943175,17.1434678036241,
6.66152210209703));
#196761=CARTESIAN_POINT('Ctrl Pts',(-18.2077678823605,17.1591489706443,
6.6571450115297));
#196762=CARTESIAN_POINT('Ctrl Pts',(-18.1373526922077,17.1785111648149,
6.65276792096238));
#196763=CARTESIAN_POINT('Ctrl Pts',(-18.0681816040679,17.2014291842191,
6.64839083039505));
#196764=CARTESIAN_POINT('Ctrl Pts',(-17.9989727390297,17.2243597200042,
6.64401134933611));
#196765=CARTESIAN_POINT('Ctrl Pts',(-17.931009778539,17.2508497721603,6.63963186827717));
#196766=CARTESIAN_POINT('Ctrl Pts',(-17.8646724802128,17.2807257543705,
6.63525238721823));
#196767=CARTESIAN_POINT('Ctrl Pts',(-17.7982175994706,17.3106546915586,
6.63086514355852));
#196768=CARTESIAN_POINT('Ctrl Pts',(-17.733394564462,17.3439813228775,6.6264778998988));
#196769=CARTESIAN_POINT('Ctrl Pts',(-17.6705584443135,17.3804861219758,
6.62209065623908));
#196770=CARTESIAN_POINT('Ctrl Pts',(-17.6278359374864,17.4053058677688,
6.61910775330425));
#196771=CARTESIAN_POINT('Ctrl Pts',(-17.5860313573357,17.4315938434277,
6.61612485036941));
#196772=CARTESIAN_POINT('Ctrl Pts',(-17.545247850536,17.459270190028,6.61314194743458));
#196773=CARTESIAN_POINT('Ctrl Pts',(-17.485250407548,17.4999854241402,6.60875373850368));
#196774=CARTESIAN_POINT('Ctrl Pts',(-17.4272300397246,17.5438661041392,
6.60436552957278));
#196775=CARTESIAN_POINT('Ctrl Pts',(-17.3715403699668,17.590693622635,6.59997732064189));
#196776=CARTESIAN_POINT('Ctrl Pts',(-17.3159333529123,17.6374516413293,
6.59559562454062));
#196777=CARTESIAN_POINT('Ctrl Pts',(-17.2626505332032,17.687147508451,6.59121392843936));
#196778=CARTESIAN_POINT('Ctrl Pts',(-17.2120162539402,17.7395196308717,
6.58683223233809));
#196779=CARTESIAN_POINT('Ctrl Pts',(-17.161441473985,17.7918302118807,6.58245568507845));
#196780=CARTESIAN_POINT('Ctrl Pts',(-17.1135093856054,17.846810455921,6.57807913781881));
#196781=CARTESIAN_POINT('Ctrl Pts',(-17.0685096421059,17.9041599685647,
6.57370259055918));
#196782=CARTESIAN_POINT('Ctrl Pts',(-17.0235384367897,17.9614731109811,
6.5693288188422));
#196783=CARTESIAN_POINT('Ctrl Pts',(-16.9814961836085,18.021152162172,6.56495504712523));
#196784=CARTESIAN_POINT('Ctrl Pts',(-16.9426332229364,18.0828625659819,
6.56058127540825));
#196785=CARTESIAN_POINT('Ctrl Pts',(-16.9037820883938,18.1445541911087,
6.5562088346447));
#196786=CARTESIAN_POINT('Ctrl Pts',(-16.8681085825371,18.2082755337074,
6.55183639388115));
#196787=CARTESIAN_POINT('Ctrl Pts',(-16.8358195870604,18.2736632835888,
6.5474639531176));
#196788=CARTESIAN_POINT('Ctrl Pts',(-16.8035297659506,18.3390527054421,
6.54309140055025));
#196789=CARTESIAN_POINT('Ctrl Pts',(-16.77462483883,18.4061081857738,6.53871884798291));
#196790=CARTESIAN_POINT('Ctrl Pts',(-16.749264845334,18.474443575934,6.53434629541557));
#196791=CARTESIAN_POINT('Ctrl Pts',(-16.7238785322802,18.5428498871397,
6.52996920484824));
#196792=CARTESIAN_POINT('Ctrl Pts',(-16.702044666544,18.6125383070843,6.52559211428092));
#196793=CARTESIAN_POINT('Ctrl Pts',(-16.6838740959311,18.6831053348767,
6.52121502371359));
#196794=CARTESIAN_POINT('Ctrl Pts',(-16.6656936016952,18.753710901942,6.51683554265465));
#196795=CARTESIAN_POINT('Ctrl Pts',(-16.6511804819227,18.8251955591515,
6.51245606159571));
#196796=CARTESIAN_POINT('Ctrl Pts',(-16.6403943335872,18.8971460314664,
6.50807658053677));
#196797=CARTESIAN_POINT('Ctrl Pts',(-16.6295890668762,18.9692240355104,
6.50368933687705));
#196798=CARTESIAN_POINT('Ctrl Pts',(-16.6225240103776,19.0417690229283,
6.49930209321733));
#196799=CARTESIAN_POINT('Ctrl Pts',(-16.6192067693545,19.1143636113253,
6.49491484955761));
#196800=CARTESIAN_POINT('Ctrl Pts',(-16.6169513651074,19.1637209362375,
6.49193194662279));
#196801=CARTESIAN_POINT('Ctrl Pts',(-16.6164273661252,19.213101155059,6.48894904368797));
#196802=CARTESIAN_POINT('Ctrl Pts',(-16.6176234550289,19.2623743116388,
6.48596614075314));
#196803=CARTESIAN_POINT('Ctrl Pts',(-16.6193830456439,19.33486105039,6.48157793182225));
#196804=CARTESIAN_POINT('Ctrl Pts',(-16.6248744285954,19.4073987776277,
6.47718972289135));
#196805=CARTESIAN_POINT('Ctrl Pts',(-16.6341051990332,19.4795718244204,
6.47280151396045));
#196806=CARTESIAN_POINT('Ctrl Pts',(-16.6433222694771,19.5516377544453,
6.46841981785918));
#196807=CARTESIAN_POINT('Ctrl Pts',(-16.6562676494651,19.6233396039479,
6.46403812175792));
#196808=CARTESIAN_POINT('Ctrl Pts',(-16.6728969413429,19.6942630563101,
6.45965642565665));
#196809=CARTESIAN_POINT('Ctrl Pts',(-16.6895066924793,19.7651031679716,
6.45527987839701));
#196810=CARTESIAN_POINT('Ctrl Pts',(-16.709791646569,19.8351662321976,6.45090333113737));
#196811=CARTESIAN_POINT('Ctrl Pts',(-16.7336560032766,19.9040460985914,
6.44652678387773));
#196812=CARTESIAN_POINT('Ctrl Pts',(-16.7575052255561,19.9728822823751,
6.44215301216076));
#196813=CARTESIAN_POINT('Ctrl Pts',(-16.7849291889405,20.0405363024766,
6.43777924044378));
#196814=CARTESIAN_POINT('Ctrl Pts',(-16.8157820891441,20.1066165733569,
6.43340546872681));
#196815=CARTESIAN_POINT('Ctrl Pts',(-16.8466256007065,20.1726767357888,
6.42903302796326));
#196816=CARTESIAN_POINT('Ctrl Pts',(-16.8808957735922,20.2371636629374,
6.4246605871997));
#196817=CARTESIAN_POINT('Ctrl Pts',(-16.9183991025644,20.299706747123,6.42028814643615));
#196818=CARTESIAN_POINT('Ctrl Pts',(-16.9559033905009,20.3622514305421,
6.41591559386881));
#196819=CARTESIAN_POINT('Ctrl Pts',(-16.9966407488749,20.4228517596424,
6.41154304130146));
#196820=CARTESIAN_POINT('Ctrl Pts',(-17.0403731142006,20.4811641514771,
6.40717048873412));
#196821=CARTESIAN_POINT('Ctrl Pts',(-17.0841508666247,20.5395370621115,
6.40279339816679));
#196822=CARTESIAN_POINT('Ctrl Pts',(-17.1309295419556,20.5956169078821,
6.39841630759946));
#196823=CARTESIAN_POINT('Ctrl Pts',(-17.1804298596141,20.6490920759469,
6.39403921703214));
#196824=CARTESIAN_POINT('Ctrl Pts',(-17.2299572112332,20.7025964487856,
6.3896597359732));
#196825=CARTESIAN_POINT('Ctrl Pts',(-17.2822088187844,20.7534929748971,
6.38528025491425));
#196826=CARTESIAN_POINT('Ctrl Pts',(-17.3368694420736,20.8015078447176,
6.38090077385531));
#196827=CARTESIAN_POINT('Ctrl Pts',(-17.3916269509507,20.8496078205726,
6.37651353019559));
#196828=CARTESIAN_POINT('Ctrl Pts',(-17.4488016237927,20.8948156407834,
6.37212628653587));
#196829=CARTESIAN_POINT('Ctrl Pts',(-17.5080466246426,20.936898989353,6.36773904287615));
#196830=CARTESIAN_POINT('Ctrl Pts',(-17.5483275163857,20.9655116112385,
6.36475613994134));
#196831=CARTESIAN_POINT('Ctrl Pts',(-17.5895648351149,20.992680787336,6.36177323700652));
#196832=CARTESIAN_POINT('Ctrl Pts',(-17.6316431823902,21.0183456909703,
6.35879033407171));
#196833=CARTESIAN_POINT('Ctrl Pts',(-17.6935454914314,21.0561018505907,
6.35440212514081));
#196834=CARTESIAN_POINT('Ctrl Pts',(-17.7575106221335,21.0907477625256,
6.35001391620991));
#196835=CARTESIAN_POINT('Ctrl Pts',(-17.8231931738165,21.1220520467474,
6.34562570727901));
#196836=CARTESIAN_POINT('Ctrl Pts',(-17.8887782417024,21.1533098702211,
6.34124401117774));
#196837=CARTESIAN_POINT('Ctrl Pts',(-17.9560752387294,21.1812357055046,
6.33686231507648));
#196838=CARTESIAN_POINT('Ctrl Pts',(-18.0247117585804,21.2056426222719,
6.33248061897521));
#196839=CARTESIAN_POINT('Ctrl Pts',(-18.0932676250583,21.2300208589697,
6.32810407171557));
#196840=CARTESIAN_POINT('Ctrl Pts',(-18.1631594352662,21.2508882305582,
6.32372752445593));
#196841=CARTESIAN_POINT('Ctrl Pts',(-18.2339938260908,21.2681054484524,
6.31935097719629));
#196842=CARTESIAN_POINT('Ctrl Pts',(-18.3047832947742,21.2853117474373,
6.31497720547931));
#196843=CARTESIAN_POINT('Ctrl Pts',(-18.3765136904421,21.2988723720882,
6.31060343376233));
#196844=CARTESIAN_POINT('Ctrl Pts',(-18.4487768305315,21.3086979629104,
6.30622966204536));
#196845=CARTESIAN_POINT('Ctrl Pts',(-18.5210179807047,21.3185205637723,
6.3018572212818));
#196846=CARTESIAN_POINT('Ctrl Pts',(-18.593791075757,21.324610322322,6.29748478051825));
#196847=CARTESIAN_POINT('Ctrl Pts',(-18.6666797525652,21.3269293429331,
6.2931123397547));
#196848=CARTESIAN_POINT('Ctrl Pts',(-18.739570293145,21.3292484228418,6.28873978718735));
#196849=CARTESIAN_POINT('Ctrl Pts',(-18.8125759391511,21.3277965600418,
6.28436723462));
#196850=CARTESIAN_POINT('Ctrl Pts',(-18.885278932449,21.3225879533179,6.27999468205265));
#196851=CARTESIAN_POINT('Ctrl Pts',(-18.9580573796556,21.3173739409053,
6.27561759148533));
#196852=CARTESIAN_POINT('Ctrl Pts',(-19.0305320648495,21.3083954347151,
6.271240500918));
#196853=CARTESIAN_POINT('Ctrl Pts',(-19.1022898016639,21.2957185953961,
6.26686341035067));
#196854=CARTESIAN_POINT('Ctrl Pts',(-19.1740867280417,21.2830348327846,
6.26248392929173));
#196855=CARTESIAN_POINT('Ctrl Pts',(-19.2451654560889,21.2666488240854,
6.25810444823278));
#196856=CARTESIAN_POINT('Ctrl Pts',(-19.3151251217559,21.2466774284901,
6.25372496717384));
#196857=CARTESIAN_POINT('Ctrl Pts',(-19.3852087904606,21.2266706337303,
6.24933772351412));
#196858=CARTESIAN_POINT('Ctrl Pts',(-19.4541689789711,21.2030659176042,
6.2449504798544));
#196859=CARTESIAN_POINT('Ctrl Pts',(-19.5216226105736,21.176029166021,6.24056323619467));
#196860=CARTESIAN_POINT('Ctrl Pts',(-19.5674845802465,21.1576467801997,
6.23758033325987));
#196861=CARTESIAN_POINT('Ctrl Pts',(-19.6126505362295,21.1376788808132,
6.23459743032507));
#196862=CARTESIAN_POINT('Ctrl Pts',(-19.6570068699279,21.1161895753614,
6.23161452739027));
#196863=CARTESIAN_POINT('Ctrl Pts',(-19.7222419452859,21.0845851494847,
6.22722755755952));
#196864=CARTESIAN_POINT('Ctrl Pts',(-19.7859792078907,21.0495646312771,
6.22284058772878));
#196865=CARTESIAN_POINT('Ctrl Pts',(-19.8478374654086,21.0112930596579,
6.21845361789804));
#196866=CARTESIAN_POINT('Ctrl Pts',(-19.909611732559,20.9730734526993,6.21407260463999));
#196867=CARTESIAN_POINT('Ctrl Pts',(-19.9695116495685,20.9316118007376,
6.20969159138194));
#196868=CARTESIAN_POINT('Ctrl Pts',(-20.0271786199974,20.8871199410489,
6.2053105781239));
#196869=CARTESIAN_POINT('Ctrl Pts',(-20.0847863205701,20.842673809896,6.20093406765183));
#196870=CARTESIAN_POINT('Ctrl Pts',(-20.1401652493039,20.7952039448503,
6.19655755717977));
#196871=CARTESIAN_POINT('Ctrl Pts',(-20.1929853613383,20.744965682602,6.19218104670771));
#196872=CARTESIAN_POINT('Ctrl Pts',(-20.2457686121849,20.6947624797648,
6.18780759043921));
#196873=CARTESIAN_POINT('Ctrl Pts',(-20.2959962435443,20.6417950475088,
6.18343413417072));
#196874=CARTESIAN_POINT('Ctrl Pts',(-20.3433722233214,20.5863581521922,
6.17906067790223));
#196875=CARTESIAN_POINT('Ctrl Pts',(-20.3907430256954,20.5309273152021,
6.17468769957944));
#196876=CARTESIAN_POINT('Ctrl Pts',(-20.4352624726779,20.4730279095114,
6.17031472125665));
#196877=CARTESIAN_POINT('Ctrl Pts',(-20.4766732169317,20.4129896251586,
6.16594174293386));
#196878=CARTESIAN_POINT('Ctrl Pts',(-20.5180810237668,20.3529555995455,
6.16156907480276));
#196879=CARTESIAN_POINT('Ctrl Pts',(-20.5563802984135,20.2907833982918,
6.15719640667166));
#196880=CARTESIAN_POINT('Ctrl Pts',(-20.5913568209819,20.2268319937627,
6.15282373854055));
#196881=CARTESIAN_POINT('Ctrl Pts',(-20.6263573794093,20.1628366418419,
6.14844806551282));
#196882=CARTESIAN_POINT('Ctrl Pts',(-20.6580304038045,20.097060073715,6.1440723924851));
#196883=CARTESIAN_POINT('Ctrl Pts',(-20.6862080123007,20.029885142562,6.13969671945737));
#196884=CARTESIAN_POINT('Ctrl Pts',(-20.699063262214,19.999238449178,6.13770044037933));
#196885=CARTESIAN_POINT('Ctrl Pts',(-20.7111916428231,19.9683009800593,
6.13570416130129));
#196886=CARTESIAN_POINT('Ctrl Pts',(-20.7225806064498,19.9371103026755,
6.13370788222325));
#196887=CARTESIAN_POINT('Ctrl Pts',(-20.7193263846487,19.9359291807798,
6.93361859104258));
#196888=CARTESIAN_POINT('Ctrl Pts',(-20.8041092873412,19.7029525977831,
6.91876474293293));
#196889=CARTESIAN_POINT('Ctrl Pts',(-20.8501557633723,19.455755786691,6.90391089482328));
#196890=CARTESIAN_POINT('Ctrl Pts',(-20.8523540255571,19.2092594247491,
6.88905704671363));
#196891=CARTESIAN_POINT('Origin',(-18.734,19.211,0.));
#196892=CARTESIAN_POINT('',(-20.7225806376299,19.9371102172836,7.95734465602265));
#196893=CARTESIAN_POINT('',(-20.7225805951215,19.9371103337003,7.73405229189664));
#196894=CARTESIAN_POINT('',(-20.7225806064498,19.9371103026755,0.));
#196895=CARTESIAN_POINT('',(-20.8509992001742,19.2090893169909,7.9107295377978));
#196896=CARTESIAN_POINT('Ctrl Pts',(-20.7225806376299,19.9371102172836,
7.95734465602265));
#196897=CARTESIAN_POINT('Ctrl Pts',(-20.7291121252103,19.919222588893,7.95624414180481));
#196898=CARTESIAN_POINT('Ctrl Pts',(-20.7354039661561,19.9012421605658,
7.95513590187344));
#196899=CARTESIAN_POINT('Ctrl Pts',(-20.7459519908274,19.8697403662776,
7.95318939765545));
#196900=CARTESIAN_POINT('Ctrl Pts',(-20.750314926476,19.8562625715911,7.95235506982288));
#196901=CARTESIAN_POINT('Ctrl Pts',(-20.7570544827814,19.8347070115582,
7.95101783580892));
#196902=CARTESIAN_POINT('Ctrl Pts',(-20.7595187944765,19.8266569553473,
7.95051780654351));
#196903=CARTESIAN_POINT('Ctrl Pts',(-20.7637864744158,19.8124129061224,
7.94963183860058));
#196904=CARTESIAN_POINT('Ctrl Pts',(-20.7656096801624,19.8062249334664,
7.94924655418107));
#196905=CARTESIAN_POINT('Ctrl Pts',(-20.7693280068598,19.7933887822314,
7.94844646764524));
#196906=CARTESIAN_POINT('Ctrl Pts',(-20.7712189012909,19.7867394685418,
7.94803153296288));
#196907=CARTESIAN_POINT('Ctrl Pts',(-20.776000877776,19.7696051452156,7.94696102106728));
#196908=CARTESIAN_POINT('Ctrl Pts',(-20.7788437604023,19.7591069984308,
7.94630388655289));
#196909=CARTESIAN_POINT('Ctrl Pts',(-20.7848190493571,19.7363478502189,
7.94487644813674));
#196910=CARTESIAN_POINT('Ctrl Pts',(-20.7879226517855,19.7240797857062,
7.94410523988962));
#196911=CARTESIAN_POINT('Ctrl Pts',(-20.79663369605,19.6883001750311,7.9418506504463));
#196912=CARTESIAN_POINT('Ctrl Pts',(-20.8019485508008,19.6647201088789,
7.94035804879104));
#196913=CARTESIAN_POINT('Ctrl Pts',(-20.8363441701446,19.4989337435183,
7.92981464048068));
#196914=CARTESIAN_POINT('Ctrl Pts',(-20.8511300496375,19.354183419222,7.92031689761982));
#196915=CARTESIAN_POINT('Ctrl Pts',(-20.8509991383138,19.2090899270172,
7.9107294698959));
#196916=CARTESIAN_POINT('Ctrl Pts',(-20.8509991377698,19.2090893241665,
7.91072943006099));
#196917=CARTESIAN_POINT('Ctrl Pts',(-20.8508884781824,19.0864802207074,
7.90262771640683));
#196918=CARTESIAN_POINT('Ctrl Pts',(-20.8401264233866,18.9640980462868,
7.89450602327149));
#196919=CARTESIAN_POINT('Ctrl Pts',(-20.8166444877547,18.8309488995711,
7.88604140362766));
#196920=CARTESIAN_POINT('Ctrl Pts',(-20.8143518770747,18.8185933419533,
7.88525966249503));
#196921=CARTESIAN_POINT('Ctrl Pts',(-20.8106712447903,18.79969691162,7.88407055609758));
#196922=CARTESIAN_POINT('Ctrl Pts',(-20.8093620685976,18.7931412004733,
7.88365922007583));
#196923=CARTESIAN_POINT('Ctrl Pts',(-20.8071513246146,18.7823376149929,
7.88298345591827));
#196924=CARTESIAN_POINT('Ctrl Pts',(-20.8062677126641,18.7780861715292,
7.88271806667172));
#196925=CARTESIAN_POINT('Ctrl Pts',(-20.8045210245981,18.7698099847755,
7.88220252958522));
#196926=CARTESIAN_POINT('Ctrl Pts',(-20.8036592792767,18.7657849831742,
7.8819523088479));
#196927=CARTESIAN_POINT('Ctrl Pts',(-20.8020280139237,18.758272835495,7.88148627742611));
#196928=CARTESIAN_POINT('Ctrl Pts',(-20.8012614185466,18.7547851608302,
7.88127030886671));
#196929=CARTESIAN_POINT('Ctrl Pts',(-20.7994932703637,18.7468368285063,
7.88077900949322));
#196930=CARTESIAN_POINT('Ctrl Pts',(-20.798486093141,18.7423774740627,7.8805040045889));
#196931=CARTESIAN_POINT('Ctrl Pts',(-20.7953527020585,18.7287103144358,
7.87966301332656));
#196932=CARTESIAN_POINT('Ctrl Pts',(-20.7931792402859,18.7195133094844,
7.87909966895684));
#196933=CARTESIAN_POINT('Ctrl Pts',(-20.7619486492839,18.5912058239648,
7.87127265776304));
#196934=CARTESIAN_POINT('Ctrl Pts',(-20.7226547857507,18.4748060396478,
7.86455352025937));
#196935=CARTESIAN_POINT('Ctrl Pts',(-20.6449226699513,18.2971368669933,
7.85400321025685));
#196936=CARTESIAN_POINT('Ctrl Pts',(-20.6130669211926,18.2333095354677,
7.85014917507173));
#196937=CARTESIAN_POINT('Ctrl Pts',(-20.5342699927172,18.093564082889,7.841359277442));
#196938=CARTESIAN_POINT('Ctrl Pts',(-20.4856310622552,18.0187661967483,
7.8364009271598));
#196939=CARTESIAN_POINT('Ctrl Pts',(-20.4120571944111,17.9198852277896,
7.82930999235392));
#196940=CARTESIAN_POINT('Ctrl Pts',(-20.3910302400536,17.8930076279039,
7.82732377723733));
#196941=CARTESIAN_POINT('Ctrl Pts',(-20.362452302932,17.8582433502222,7.82466997628898));
#196942=CARTESIAN_POINT('Ctrl Pts',(-20.3554761973758,17.8498892803699,
7.82402559363929));
#196943=CARTESIAN_POINT('Ctrl Pts',(-20.3439632617759,17.8363163608519,
7.82296752082302));
#196944=CARTESIAN_POINT('Ctrl Pts',(-20.3394646764143,17.8310652250735,
7.82255540289719));
#196945=CARTESIAN_POINT('Ctrl Pts',(-20.3307199814935,17.820958307142,7.82175677518002));
#196946=CARTESIAN_POINT('Ctrl Pts',(-20.3264772410794,17.8160997016274,
7.82137040766717));
#196947=CARTESIAN_POINT('Ctrl Pts',(-20.3166485638874,17.8049476064496,
7.820477854729));
#196948=CARTESIAN_POINT('Ctrl Pts',(-20.3110472026305,17.7986679116916,
7.8199710262088));
#196949=CARTESIAN_POINT('Ctrl Pts',(-20.2959250278497,17.7819165499962,
7.81860752145994));
#196950=CARTESIAN_POINT('Ctrl Pts',(-20.2863365214536,17.7715068223187,
7.81774798835765));
#196951=CARTESIAN_POINT('Ctrl Pts',(-20.2021785208533,17.6819597386844,
7.810245842946));
#196952=CARTESIAN_POINT('Ctrl Pts',(-20.121730411581,17.6085923620633,7.80334364909822));
#196953=CARTESIAN_POINT('Ctrl Pts',(-19.9589817777189,17.4816495084809,
7.78990413415877));
#196954=CARTESIAN_POINT('Ctrl Pts',(-19.8778834651647,17.4269701061156,
7.78341902518482));
#196955=CARTESIAN_POINT('Ctrl Pts',(-19.7310607048379,17.3421160455268,
7.77224181004057));
#196956=CARTESIAN_POINT('Ctrl Pts',(-19.6670207069335,17.3093346565223,
7.76753757203429));
#196957=CARTESIAN_POINT('Ctrl Pts',(-19.5707250730171,17.2660801092606,
7.76082224655149));
#196958=CARTESIAN_POINT('Ctrl Pts',(-19.5396905692237,17.2530201145167,
7.75871054995631));
#196959=CARTESIAN_POINT('Ctrl Pts',(-19.5015752441705,17.2380402126393,
7.75619162059581));
#196960=CARTESIAN_POINT('Ctrl Pts',(-19.4947808259641,17.2354103117293,
7.7557454429911));
#196961=CARTESIAN_POINT('Ctrl Pts',(-19.4840926732908,17.231336588093,7.75504818249384));
#196962=CARTESIAN_POINT('Ctrl Pts',(-19.4802081111425,17.2298690859721,
7.75479571859328));
#196963=CARTESIAN_POINT('Ctrl Pts',(-19.4729791093083,17.227162406764,7.75432769652576));
#196964=CARTESIAN_POINT('Ctrl Pts',(-19.4696358885392,17.2259202635427,
7.75411196708751));
#196965=CARTESIAN_POINT('Ctrl Pts',(-19.4620487625848,17.2231231358259,
7.75362400244998));
#196966=CARTESIAN_POINT('Ctrl Pts',(-19.4578030177817,17.2215732935993,
7.75335207568659));
#196967=CARTESIAN_POINT('Ctrl Pts',(-19.4451910887339,17.2170152266156,
7.75254760100316));
#196968=CARTESIAN_POINT('Ctrl Pts',(-19.436810762246,17.2140460496254,7.75201731924416));
#196969=CARTESIAN_POINT('Ctrl Pts',(-19.3737732032367,17.1921576173445,
7.74805873576126));
#196970=CARTESIAN_POINT('Ctrl Pts',(-19.3183746982198,17.1754308417801,
7.74474981606306));
#196971=CARTESIAN_POINT('Ctrl Pts',(-19.1043129817761,17.1202599492673,
7.7323629742475));
#196972=CARTESIAN_POINT('Ctrl Pts',(-18.9420847437622,17.097937580278,7.72375664881158));
#196973=CARTESIAN_POINT('Ctrl Pts',(-18.7188554461252,17.0932025716156,
7.71138884768571));
#196974=CARTESIAN_POINT('Ctrl Pts',(-18.6587933218688,17.0944843586101,
7.7080148190298));
#196975=CARTESIAN_POINT('Ctrl Pts',(-18.5747314139418,17.0998610731298,
7.70317775289833));
#196976=CARTESIAN_POINT('Ctrl Pts',(-18.5506218788211,17.1018185359142,
7.70177728718358));
#196977=CARTESIAN_POINT('Ctrl Pts',(-18.5085725004037,17.1059589473461,
7.69930876151794));
#196978=CARTESIAN_POINT('Ctrl Pts',(-18.4906169854242,17.1079593277413,
7.69824637307862));
#196979=CARTESIAN_POINT('Ctrl Pts',(-18.4642189510212,17.1112428595442,
7.6966713796779));
#196980=CARTESIAN_POINT('Ctrl Pts',(-18.4557547752273,17.1123477050929,
7.69616439461756));
#196981=CARTESIAN_POINT('Ctrl Pts',(-18.4409105262776,17.1143767345143,
7.69527168229698));
#196982=CARTESIAN_POINT('Ctrl Pts',(-18.4345275227525,17.1152789329362,
7.69488665477982));
#196983=CARTESIAN_POINT('Ctrl Pts',(-18.4221294422942,17.1170891231432,
7.6941364939277));
#196984=CARTESIAN_POINT('Ctrl Pts',(-18.4161139566688,17.1179939161013,
7.69377146551617));
#196985=CARTESIAN_POINT('Ctrl Pts',(-18.4017239139267,17.1202217989332,
7.69289569594962));
#196986=CARTESIAN_POINT('Ctrl Pts',(-18.3933532906341,17.1215692881651,
7.69238418490325));
#196987=CARTESIAN_POINT('Ctrl Pts',(-18.3630631698079,17.1266321977784,
7.69052555047807));
#196988=CARTESIAN_POINT('Ctrl Pts',(-18.3411950439062,17.1306424648036,
7.68916910549212));
#196989=CARTESIAN_POINT('Ctrl Pts',(-18.1386253576824,17.171098294024,7.67646388002575));
#196990=CARTESIAN_POINT('Ctrl Pts',(-17.9633777793561,17.2306504682647,
7.66432808122214));
#196991=CARTESIAN_POINT('Ctrl Pts',(-17.7254567075873,17.3479144450112,
7.64681365653401));
#196992=CARTESIAN_POINT('Ctrl Pts',(-17.6549258545252,17.3878576331209,
7.64149071346173));
#196993=CARTESIAN_POINT('Ctrl Pts',(-17.5563829640792,17.4513916650659,
7.63401506756869));
#196994=CARTESIAN_POINT('Ctrl Pts',(-17.5264201602187,17.4718178155546,
7.63173696514549));
#196995=CARTESIAN_POINT('Ctrl Pts',(-17.490924800733,17.4973754796636,7.62904595716123));
#196996=CARTESIAN_POINT('Ctrl Pts',(-17.4848778515958,17.5017783028714,
7.62858780101063));
#196997=CARTESIAN_POINT('Ctrl Pts',(-17.4755024628351,17.5086809131879,
7.62787806404683));
#196998=CARTESIAN_POINT('Ctrl Pts',(-17.4721579151976,17.5111585726648,
7.62762499516659));
#196999=CARTESIAN_POINT('Ctrl Pts',(-17.4659618997561,17.5157769794248,
7.62715642516368));
#197000=CARTESIAN_POINT('Ctrl Pts',(-17.4631085596196,17.5179150463709,
7.62694074918401));
#197001=CARTESIAN_POINT('Ctrl Pts',(-17.4566611315629,17.5227717208308,
7.62645363365325));
#197002=CARTESIAN_POINT('Ctrl Pts',(-17.4530703236504,17.5254945943378,
7.62618249803873));
#197003=CARTESIAN_POINT('Ctrl Pts',(-17.4422374838663,17.533763639891,7.62536491255871));
#197004=CARTESIAN_POINT('Ctrl Pts',(-17.4350224684698,17.5393452554135,
7.62482089516974));
#197005=CARTESIAN_POINT('Ctrl Pts',(-17.3795517396309,17.5828340261551,
7.62064045331588));
#197006=CARTESIAN_POINT('Ctrl Pts',(-17.3329239421351,17.6227802750898,
7.61713848545565));
#197007=CARTESIAN_POINT('Ctrl Pts',(-17.1808267450645,17.7650025452924,
7.60550154960405));
#197008=CARTESIAN_POINT('Ctrl Pts',(-17.084283840583,17.8761977818435,7.59771434168961));
#197009=CARTESIAN_POINT('Ctrl Pts',(-16.9468098732126,18.0724725975678,
7.58451605297771));
#197010=CARTESIAN_POINT('Ctrl Pts',(-16.8986515413068,18.1518558403687,
7.57930752797287));
#197011=CARTESIAN_POINT('Ctrl Pts',(-16.8461314348078,18.2528322508335,
7.57267773573088));
#197012=CARTESIAN_POINT('Ctrl Pts',(-16.8366866412711,18.2716730459892,
7.57144084183032));
#197013=CARTESIAN_POINT('Ctrl Pts',(-16.8236313699821,18.2987166511657,
7.56966429638799));
#197014=CARTESIAN_POINT('Ctrl Pts',(-16.8197890595803,18.3068066119795,
7.5691327109669));
#197015=CARTESIAN_POINT('Ctrl Pts',(-16.8132398647239,18.3208247530898,
7.56821124401));
#197016=CARTESIAN_POINT('Ctrl Pts',(-16.8105087868877,18.3267415428209,
7.56782220508813));
#197017=CARTESIAN_POINT('Ctrl Pts',(-16.8053256186095,18.3381083427666,
7.56707457790801));
#197018=CARTESIAN_POINT('Ctrl Pts',(-16.8028691982743,18.3435563187227,
7.56671614340484));
#197019=CARTESIAN_POINT('Ctrl Pts',(-16.7965280894982,18.3577803879535,
7.56577999846621));
#197020=CARTESIAN_POINT('Ctrl Pts',(-16.7926799869105,18.3665725535029,
7.56520104125838));
#197021=CARTESIAN_POINT('Ctrl Pts',(-16.7796942813231,18.3968003104181,
7.56320933573633));
#197022=CARTESIAN_POINT('Ctrl Pts',(-16.7708511295329,18.4183598415019,
7.56178664467392));
#197023=CARTESIAN_POINT('Ctrl Pts',(-16.7001114915971,18.5992724084999,
7.54982651489317));
#197024=CARTESIAN_POINT('Ctrl Pts',(-16.6573822139315,18.7654105610991,
7.53862576974281));
#197025=CARTESIAN_POINT('Ctrl Pts',(-16.6233196920247,19.0242948317757,
7.52137082320096));
#197026=CARTESIAN_POINT('Ctrl Pts',(-16.6172798314759,19.1144189239202,
7.51541615508234));
#197027=CARTESIAN_POINT('Ctrl Pts',(-16.6168937886914,19.2432832556249,
7.50718309105437));
#197028=CARTESIAN_POINT('Ctrl Pts',(-16.617835188313,19.2819072844477,7.50475216117236));
#197029=CARTESIAN_POINT('Ctrl Pts',(-16.620227030745,19.3280933502732,7.50190599293462));
#197030=CARTESIAN_POINT('Ctrl Pts',(-16.6206620214824,19.3356980787129,
7.50143933646228));
#197031=CARTESIAN_POINT('Ctrl Pts',(-16.6214000350863,19.3474842907115,
7.50071932659188));
#197032=CARTESIAN_POINT('Ctrl Pts',(-16.6216744442227,19.3516674108587,
7.5004644162781));
#197033=CARTESIAN_POINT('Ctrl Pts',(-16.6222050637877,19.3594043190833,
7.49999415175133));
#197034=CARTESIAN_POINT('Ctrl Pts',(-16.6224578180082,19.3629582459515,
7.49977861183135));
#197035=CARTESIAN_POINT('Ctrl Pts',(-16.623047714322,19.3709668867107,7.49929395951222));
#197036=CARTESIAN_POINT('Ctrl Pts',(-16.6233899845081,19.3754211683442,
7.49902513786399));
#197037=CARTESIAN_POINT('Ctrl Pts',(-16.6244361112424,19.3884935642485,
7.49823827140866));
#197038=CARTESIAN_POINT('Ctrl Pts',(-16.6251786804385,19.3971086082078,
7.49772234790087));
#197039=CARTESIAN_POINT('Ctrl Pts',(-16.6307250118559,19.4571531292284,
7.49414343353275));
#197040=CARTESIAN_POINT('Ctrl Pts',(-16.6373572613694,19.5084007390801,
7.49117542686747));
#197041=CARTESIAN_POINT('Ctrl Pts',(-16.649441741637,19.58083789402,7.48703950299129));
#197042=CARTESIAN_POINT('Ctrl Pts',(-16.6533563583955,19.6022611432054,
7.48582377498518));
#197043=CARTESIAN_POINT('Ctrl Pts',(-16.6665988012666,19.6689000647081,
7.48205532923447));
#197044=CARTESIAN_POINT('Ctrl Pts',(-16.6770756471482,19.7138743759228,
7.47953088263622));
#197045=CARTESIAN_POINT('Ctrl Pts',(-16.717294840193,19.8641062705399,7.47106357103666));
#197046=CARTESIAN_POINT('Ctrl Pts',(-16.7537170579818,19.9673901696016,
7.46517522828271));
#197047=CARTESIAN_POINT('Ctrl Pts',(-16.8202492903854,20.1177993306105,
7.45603030492175));
#197048=CARTESIAN_POINT('Ctrl Pts',(-16.844504154324,20.1673114598088,7.45292245199185));
#197049=CARTESIAN_POINT('Ctrl Pts',(-16.8869471168382,20.2460178037331,
7.44777793347763));
#197050=CARTESIAN_POINT('Ctrl Pts',(-16.9039633395199,20.2758153980377,
7.44578066574025));
#197051=CARTESIAN_POINT('Ctrl Pts',(-16.9272822633564,20.3144386524507,
7.44311984036657));
#197052=CARTESIAN_POINT('Ctrl Pts',(-16.9329397970283,20.3236490813987,
7.4424798150795));
#197053=CARTESIAN_POINT('Ctrl Pts',(-16.9423229770063,20.3386657443901,
7.44142708502273));
#197054=CARTESIAN_POINT('Ctrl Pts',(-16.9460069521331,20.3444978803873,
7.44101592167097));
#197055=CARTESIAN_POINT('Ctrl Pts',(-16.9531942096207,20.3557538719202,
7.440217850813));
#197056=CARTESIAN_POINT('Ctrl Pts',(-16.9566939348732,20.3611799162546,
7.43983107871379));
#197057=CARTESIAN_POINT('Ctrl Pts',(-16.9648334168325,20.3736736775419,
7.43893571141123));
#197058=CARTESIAN_POINT('Ctrl Pts',(-16.969490776145,20.3807297444866,7.43842646013092));
#197059=CARTESIAN_POINT('Ctrl Pts',(-16.9821331264652,20.3996360433032,
7.43705219308795));
#197060=CARTESIAN_POINT('Ctrl Pts',(-16.9901959320627,20.4114334812718,
7.43618424953288));
#197061=CARTESIAN_POINT('Ctrl Pts',(-17.0652574951864,20.5189108909993,
7.42817966372938));
#197062=CARTESIAN_POINT('Ctrl Pts',(-17.1399371159666,20.6089585720942,
7.42074147848734));
#197063=CARTESIAN_POINT('Ctrl Pts',(-17.335419970133,20.8085286160105,7.40249415789795));
#197064=CARTESIAN_POINT('Ctrl Pts',(-17.4621895539076,20.9111829371932,
7.3915453069707));
#197065=CARTESIAN_POINT('Ctrl Pts',(-17.6270395001458,21.0158254108335,
7.3791363212405));
#197066=CARTESIAN_POINT('Ctrl Pts',(-17.6550249419876,21.0326941039494,
7.37708849567842));
#197067=CARTESIAN_POINT('Ctrl Pts',(-17.6896861232336,21.0525075614244,
7.37463336584474));
#197068=CARTESIAN_POINT('Ctrl Pts',(-17.6959994512029,21.0560735584769,
7.37418940877789));
#197069=CARTESIAN_POINT('Ctrl Pts',(-17.7059218465245,21.061611039547,7.37349685855344));
#197070=CARTESIAN_POINT('Ctrl Pts',(-17.7095184795922,21.0636045245423,
7.37324688937465));
#197071=CARTESIAN_POINT('Ctrl Pts',(-17.716249764005,21.0673098375628,7.37278107694451));
#197072=CARTESIAN_POINT('Ctrl Pts',(-17.7193829044525,21.0690241940178,
7.37256507733113));
#197073=CARTESIAN_POINT('Ctrl Pts',(-17.7265418257936,21.0729178237728,
7.37207338465479));
#197074=CARTESIAN_POINT('Ctrl Pts',(-17.7305703380924,21.0750919692347,
7.37179801954381));
#197075=CARTESIAN_POINT('Ctrl Pts',(-17.7429638625097,21.0817288049946,
7.37095483077659));
#197076=CARTESIAN_POINT('Ctrl Pts',(-17.7513519592315,21.0861484536394,
7.37038966922786));
#197077=CARTESIAN_POINT('Ctrl Pts',(-17.8671858038654,21.1461900317482,
7.36265696430112));
#197078=CARTESIAN_POINT('Ctrl Pts',(-17.9791941460035,21.1925660476455,
7.35601946546277));
#197079=CARTESIAN_POINT('Ctrl Pts',(-18.2651921078252,21.2831834505258,
7.33969351215518));
#197080=CARTESIAN_POINT('Ctrl Pts',(-18.4419635784852,21.3153841835301,
7.33007482409207));
#197081=CARTESIAN_POINT('Ctrl Pts',(-18.6421236143948,21.3261144541572,
7.31840385987958));
#197082=CARTESIAN_POINT('Ctrl Pts',(-18.6635892547781,21.3269377829711,
7.31714350484512));
#197083=CARTESIAN_POINT('Ctrl Pts',(-18.6940855872039,21.3276429287101,
7.31533911515375));
#197084=CARTESIAN_POINT('Ctrl Pts',(-18.7031091637951,21.3277938492931,
7.31480350167427));
#197085=CARTESIAN_POINT('Ctrl Pts',(-18.7186621427026,21.3279545059231,
7.31387726708604));
#197086=CARTESIAN_POINT('Ctrl Pts',(-18.725191180662,21.3279917414208,7.3134875124314));
#197087=CARTESIAN_POINT('Ctrl Pts',(-18.7376819724583,21.3280051925979,
7.31274005361289));
#197088=CARTESIAN_POINT('Ctrl Pts',(-18.7436436668569,21.3279864290939,
7.31238251063461));
#197089=CARTESIAN_POINT('Ctrl Pts',(-18.7591228073831,21.3278723237761,
7.31145208466416));
#197090=CARTESIAN_POINT('Ctrl Pts',(-18.7686397536666,21.3277379794056,
7.31087798473954));
#197091=CARTESIAN_POINT('Ctrl Pts',(-18.8009696850212,21.3270635107853,
7.30892057196584));
#197092=CARTESIAN_POINT('Ctrl Pts',(-18.8237740957008,21.3262187282114,
7.30752777270334));
#197093=CARTESIAN_POINT('Ctrl Pts',(-19.0240757464297,21.3155537148001,
7.29518346973431));
#197094=CARTESIAN_POINT('Ctrl Pts',(-19.1996626688947,21.2837817598868,
7.2835074205324));
#197095=CARTESIAN_POINT('Ctrl Pts',(-19.4506665521142,21.204834478496,7.26612447551382));
#197096=CARTESIAN_POINT('Ctrl Pts',(-19.5305375913909,21.1742922897261,
7.2604981719138));
#197097=CARTESIAN_POINT('Ctrl Pts',(-19.6424270641354,21.1235505092953,
7.25265697583508));
#197098=CARTESIAN_POINT('Ctrl Pts',(-19.6760922453198,21.1071940250878,
7.25030385331795));
#197099=CARTESIAN_POINT('Ctrl Pts',(-19.7160080819044,21.0864749017882,
7.24753654948697));
#197100=CARTESIAN_POINT('Ctrl Pts',(-19.7226892725834,21.0829614062218,
7.24707413568986));
#197101=CARTESIAN_POINT('Ctrl Pts',(-19.7330383412919,21.0774481888547,
7.24635925167028));
#197102=CARTESIAN_POINT('Ctrl Pts',(-19.7367192565314,21.0754732613603,
7.24610525906218));
#197103=CARTESIAN_POINT('Ctrl Pts',(-19.7435300027832,21.0717930773486,
7.24563584392917));
#197104=CARTESIAN_POINT('Ctrl Pts',(-19.746661345274,21.0700908270737,7.24542024109249));
#197105=CARTESIAN_POINT('Ctrl Pts',(-19.7537247519062,21.0662278995091,
7.24493438344008));
#197106=CARTESIAN_POINT('Ctrl Pts',(-19.7576542443098,21.0640626318949,
7.24466442585344));
#197107=CARTESIAN_POINT('Ctrl Pts',(-19.7692143329098,21.0576446856342,
7.24387113874183));
#197108=CARTESIAN_POINT('Ctrl Pts',(-19.7768256316007,21.053357190685,7.24334998279018));
#197109=CARTESIAN_POINT('Ctrl Pts',(-19.8310962761209,21.0223420962979,
7.23964069520895));
#197110=CARTESIAN_POINT('Ctrl Pts',(-19.8767530674185,20.9938900408248,
7.23655559273803));
#197111=CARTESIAN_POINT('Ctrl Pts',(-20.0608280282725,20.8691994595296,
7.22405651303708));
#197112=CARTESIAN_POINT('Ctrl Pts',(-20.1885934818829,20.7583408221315,
7.21518664224068));
#197113=CARTESIAN_POINT('Ctrl Pts',(-20.3564535135819,20.5733266073679,
7.20134226267846));
#197114=CARTESIAN_POINT('Ctrl Pts',(-20.4075288840627,20.5100720445777,
7.19675115653915));
#197115=CARTESIAN_POINT('Ctrl Pts',(-20.4662740161408,20.4280871280923,
7.19086730588545));
#197116=CARTESIAN_POINT('Ctrl Pts',(-20.4774848024831,20.4119725432133,
7.18971402008575));
#197117=CARTESIAN_POINT('Ctrl Pts',(-20.4933402561387,20.3884916625691,
7.18803707213709));
#197118=CARTESIAN_POINT('Ctrl Pts',(-20.4981663232809,20.381248662739,7.18752027265259));
#197119=CARTESIAN_POINT('Ctrl Pts',(-20.5065035620197,20.3685672871109,
7.18661617200641));
#197120=CARTESIAN_POINT('Ctrl Pts',(-20.5100347313983,20.3631421496468,
7.18622962706426));
#197121=CARTESIAN_POINT('Ctrl Pts',(-20.5168105267371,20.3526269362594,
7.18548081979802));
#197122=CARTESIAN_POINT('Ctrl Pts',(-20.5200583767544,20.3475390048255,
7.18511868266969));
#197123=CARTESIAN_POINT('Ctrl Pts',(-20.5277198427574,20.3354229629952,
7.18425671472095));
#197124=CARTESIAN_POINT('Ctrl Pts',(-20.5321139541324,20.3283826913369,
7.18375616803042));
#197125=CARTESIAN_POINT('Ctrl Pts',(-20.5475456153652,20.3033312362296,
7.18197606998159));
#197126=CARTESIAN_POINT('Ctrl Pts',(-20.5583545735578,20.2851813477433,
7.18068818849549));
#197127=CARTESIAN_POINT('Ctrl Pts',(-20.6295618924453,20.1614377216284,
7.17191698304319));
#197128=CARTESIAN_POINT('Ctrl Pts',(-20.680959667771,20.0510965762493,7.16412183349376));
#197129=CARTESIAN_POINT('Ctrl Pts',(-20.7225806520317,19.9371101778416,
7.15616138910049));
#197130=CARTESIAN_POINT('',(-20.8478091512629,19.2105385443279,7.68893948891723));
#197131=CARTESIAN_POINT('Ctrl Pts',(-20.8476071281599,19.2105314192558,
7.68905589350251));
#197132=CARTESIAN_POINT('Ctrl Pts',(-20.8482399779405,18.8850442033519,
7.6695533959637));
#197133=CARTESIAN_POINT('Ctrl Pts',(-20.6243347262999,17.8528832328165,
7.6076589628644));
#197134=CARTESIAN_POINT('Ctrl Pts',(-19.0148744805716,16.7235434527702,
7.5033725942046));
#197135=CARTESIAN_POINT('Ctrl Pts',(-16.7944747214404,17.6284159605188,
7.37619678752319));
#197136=CARTESIAN_POINT('Ctrl Pts',(-16.3534690248723,19.9852110982479,
7.24902098084175));
#197137=CARTESIAN_POINT('Ctrl Pts',(-18.0964527455682,21.6317156062949,
7.12184517416031));
#197138=CARTESIAN_POINT('Ctrl Pts',(-20.0208839011405,21.1569084882251,
7.01671104422726));
#197139=CARTESIAN_POINT('Ctrl Pts',(-20.6031710288178,20.2551147363436,
6.95396884985468));
#197140=CARTESIAN_POINT('Ctrl Pts',(-20.7193263846487,19.9359291807798,
6.93361859104258));
#197141=CARTESIAN_POINT('Ctrl Pts',(-20.8509999712458,19.2106510800831,
7.68710095623848));
#197142=CARTESIAN_POINT('Ctrl Pts',(-20.8510014361103,19.219538844338,7.68762152174537));
#197143=CARTESIAN_POINT('Ctrl Pts',(-20.8509469309451,19.2284264498996,
7.68814377561739));
#197144=CARTESIAN_POINT('Ctrl Pts',(-20.8507292584609,19.245937586264,7.68917624627481));
#197145=CARTESIAN_POINT('Ctrl Pts',(-20.8505693533295,19.2545609662676,
7.68968635124469));
#197146=CARTESIAN_POINT('Ctrl Pts',(-20.8502036147335,19.2693940125878,
7.69056674046743));
#197147=CARTESIAN_POINT('Ctrl Pts',(-20.8500231310445,19.2756042362602,
7.6909362299724));
#197148=CARTESIAN_POINT('Ctrl Pts',(-20.8496088606952,19.2879820912782,
7.69167449272669));
#197149=CARTESIAN_POINT('Ctrl Pts',(-20.8493754334253,19.2941496737455,
7.69204325113524));
#197150=CARTESIAN_POINT('Ctrl Pts',(-20.848855723493,19.3064570441778,7.69278093717845));
#197151=CARTESIAN_POINT('Ctrl Pts',(-20.8485696657275,19.3125967815423,
7.69314985421297));
#197152=CARTESIAN_POINT('Ctrl Pts',(-20.8477228781319,19.3292146330669,
7.69415087300361));
#197153=CARTESIAN_POINT('Ctrl Pts',(-20.847110980948,19.339689863623,7.69478457423149));
#197154=CARTESIAN_POINT('Ctrl Pts',(-20.8445147256942,19.3791005136108,
7.69717913939528));
#197155=CARTESIAN_POINT('Ctrl Pts',(-20.8420137559092,19.4079976241779,
7.69895610657007));
#197156=CARTESIAN_POINT('Ctrl Pts',(-20.8205669688998,19.6078964006027,
7.71140145936347));
#197157=CARTESIAN_POINT('Ctrl Pts',(-20.7814483759014,19.7758905836106,
7.72271594700901));
#197158=CARTESIAN_POINT('Ctrl Pts',(-20.7225805951212,19.9371103337009,
7.73405229189668));
#197159=CARTESIAN_POINT('Origin',(-18.734,19.211,0.));
#197160=CARTESIAN_POINT('',(-20.7225807266241,19.9371099735572,8.75434675637709));
#197161=CARTESIAN_POINT('',(-20.7225805753213,19.9371103879265,8.53521114927007));
#197162=CARTESIAN_POINT('',(-20.7225806064498,19.9371103026755,0.));
#197163=CARTESIAN_POINT('Ctrl Pts',(-20.7225807266241,19.9371099735572,
8.75434675637709));
#197164=CARTESIAN_POINT('Ctrl Pts',(-20.7522189772263,19.855940376575,8.74958604064089));
#197165=CARTESIAN_POINT('Ctrl Pts',(-20.7768869137611,19.7729578191594,
8.74492442009262));
#197166=CARTESIAN_POINT('Ctrl Pts',(-20.8270296549,19.5564351630452,8.73282225603236));
#197167=CARTESIAN_POINT('Ctrl Pts',(-20.8448588521927,19.4216336957187,
8.72532554013257));
#197168=CARTESIAN_POINT('Ctrl Pts',(-20.8502665613375,19.2692153684893,
8.71640096977841));
#197169=CARTESIAN_POINT('Ctrl Pts',(-20.850663023119,19.2523619374726,8.7154084679584));
#197170=CARTESIAN_POINT('Ctrl Pts',(-20.850952894071,19.2273224522688,8.71392477790426));
#197171=CARTESIAN_POINT('Ctrl Pts',(-20.8510001744524,19.2191385907097,
8.71343840732951));
#197172=CARTESIAN_POINT('Ctrl Pts',(-20.8509998627484,19.2045564795729,
8.71256913422892));
#197173=CARTESIAN_POINT('Ctrl Pts',(-20.850970719493,19.198158300236,8.71218681454019));
#197174=CARTESIAN_POINT('Ctrl Pts',(-20.8508481156843,19.1846683309743,
8.71137877086441));
#197175=CARTESIAN_POINT('Ctrl Pts',(-20.8507480205187,19.1775766938449,
8.71095284353293));
#197176=CARTESIAN_POINT('Ctrl Pts',(-20.850388624328,19.1588005204232,8.70982205354763));
#197177=CARTESIAN_POINT('Ctrl Pts',(-20.8500681972138,19.1471175218895,
8.7091152843866));
#197178=CARTESIAN_POINT('Ctrl Pts',(-20.8481220038578,19.0926263275845,
8.7058036403396));
#197179=CARTESIAN_POINT('Ctrl Pts',(-20.8452939286764,19.0498736478181,
8.70316139690633));
#197180=CARTESIAN_POINT('Ctrl Pts',(-20.8339020509085,18.9320661419609,
8.69575361357748));
#197181=CARTESIAN_POINT('Ctrl Pts',(-20.8226163050611,18.8573438067687,
8.69090980039786));
#197182=CARTESIAN_POINT('Ctrl Pts',(-20.7814380041058,18.6576814010828,
8.67762194008139));
#197183=CARTESIAN_POINT('Ctrl Pts',(-20.7441346497488,18.5345972382031,
8.66904372550594));
#197184=CARTESIAN_POINT('Ctrl Pts',(-20.6896744297274,18.4002580836196,
8.65959209010676));
#197185=CARTESIAN_POINT('Ctrl Pts',(-20.6832526056217,18.3849375144138,
8.6585131754329));
#197186=CARTESIAN_POINT('Ctrl Pts',(-20.6554930393278,18.3208381981372,
8.65399898740556));
#197187=CARTESIAN_POINT('Ctrl Pts',(-20.6324975721535,18.2727934484049,
8.65061473408322));
#197188=CARTESIAN_POINT('Ctrl Pts',(-20.6036571480965,18.2179506167347,
8.64679238727182));
#197189=CARTESIAN_POINT('Ctrl Pts',(-20.5995537700675,18.210263238401,8.64625757047998));
#197190=CARTESIAN_POINT('Ctrl Pts',(-20.5932681260821,18.1986605697957,
8.64545208353504));
#197191=CARTESIAN_POINT('Ctrl Pts',(-20.59112075744,18.1947266215475,8.64517928019296));
#197192=CARTESIAN_POINT('Ctrl Pts',(-20.5872434530345,18.1876767839009,
8.64469098568992));
#197193=CARTESIAN_POINT('Ctrl Pts',(-20.5855181356665,18.1845584309354,
8.64447520685968));
#197194=CARTESIAN_POINT('Ctrl Pts',(-20.581751667315,18.1777912819227,8.64400740200665));
#197195=CARTESIAN_POINT('Ctrl Pts',(-20.579707586274,18.1741441827135,8.6437555673661));
#197196=CARTESIAN_POINT('Ctrl Pts',(-20.5739344716727,18.1639148215671,
8.6430499566995));
#197197=CARTESIAN_POINT('Ctrl Pts',(-20.5701808972544,18.1573463816715,
8.64259772886939));
#197198=CARTESIAN_POINT('Ctrl Pts',(-20.547508229109,18.1181602433038,8.63990409673108));
#197199=CARTESIAN_POINT('Ctrl Pts',(-20.5277543658324,18.0860304440255,
8.63771330417982));
#197200=CARTESIAN_POINT('Ctrl Pts',(-20.4598654099191,17.9819478666145,
8.63061757981418));
#197201=CARTESIAN_POINT('Ctrl Pts',(-20.4081740321556,17.9124145235897,
8.62587707032943));
#197202=CARTESIAN_POINT('Ctrl Pts',(-20.2388260349945,17.7115978620897,
8.61158242665742));
#197203=CARTESIAN_POINT('Ctrl Pts',(-20.1089429969067,17.5916688874991,
8.60211687861015));
#197204=CARTESIAN_POINT('Ctrl Pts',(-19.9470525525317,17.4758576359767,
8.59054987254004));
#197205=CARTESIAN_POINT('Ctrl Pts',(-19.9281749310122,17.4628118830596,
8.58920552810913));
#197206=CARTESIAN_POINT('Ctrl Pts',(-19.9011551756503,17.4447812186854,
8.58728583925829));
#197207=CARTESIAN_POINT('Ctrl Pts',(-19.8931852443964,17.4395402764492,
8.5867201401416));
#197208=CARTESIAN_POINT('Ctrl Pts',(-19.8801738369424,17.431109519426,8.58579736495819));
#197209=CARTESIAN_POINT('Ctrl Pts',(-19.8751537608159,17.4278868010182,
8.58544152194468));
#197210=CARTESIAN_POINT('Ctrl Pts',(-19.8646137051622,17.4211831836323,
8.58469474966484));
#197211=CARTESIAN_POINT('Ctrl Pts',(-19.8590911251408,17.4177065089332,
8.5843036688113));
#197212=CARTESIAN_POINT('Ctrl Pts',(-19.845908544811,17.4094924352094,8.58337057243101));
#197213=CARTESIAN_POINT('Ctrl Pts',(-19.8382342601107,17.4047783046091,
8.58282770719576));
#197214=CARTESIAN_POINT('Ctrl Pts',(-19.8122482811057,17.389043244018,8.5809905001653));
#197215=CARTESIAN_POINT('Ctrl Pts',(-19.7938003050354,17.3782509617353,
8.5796878678121));
#197216=CARTESIAN_POINT('Ctrl Pts',(-19.6922718200734,17.3209010946873,
8.57252540608278));
#197217=CARTESIAN_POINT('Ctrl Pts',(-19.60629607635,17.279716986503,8.56647654423669));
#197218=CARTESIAN_POINT('Ctrl Pts',(-19.3593928288266,17.1813027939518,
8.54920496637082));
#197219=CARTESIAN_POINT('Ctrl Pts',(-19.1938931216584,17.1375289722929,
8.53769538467965));
#197220=CARTESIAN_POINT('Ctrl Pts',(-18.9884969801305,17.1090309416229,
8.52446042131896));
#197221=CARTESIAN_POINT('Ctrl Pts',(-18.9519260576004,17.1049251566184,
8.52214609667416));
#197222=CARTESIAN_POINT('Ctrl Pts',(-18.9081484127797,17.1011629589259,
8.5194403182823));
#197223=CARTESIAN_POINT('Ctrl Pts',(-18.9010293781574,17.1005874337673,
8.51900234602093));
#197224=CARTESIAN_POINT('Ctrl Pts',(-18.8894079540945,17.0997070952935,
8.51829085213219));
#197225=CARTESIAN_POINT('Ctrl Pts',(-18.8849073291344,17.0993806354967,
8.51801616090054));
#197226=CARTESIAN_POINT('Ctrl Pts',(-18.8768482173678,17.0988219528371,
8.51752584193458));
#197227=CARTESIAN_POINT('Ctrl Pts',(-18.8732901690566,17.0985843293676,
8.5173099160037));
#197228=CARTESIAN_POINT('Ctrl Pts',(-18.865582191699,17.0980891135052,8.51684333475449));
#197229=CARTESIAN_POINT('Ctrl Pts',(-18.8614321122457,17.0978347568418,
8.51659286250341));
#197230=CARTESIAN_POINT('Ctrl Pts',(-18.8498344687612,17.0971582321789,
8.51589490737903));
#197231=CARTESIAN_POINT('Ctrl Pts',(-18.84238529839,17.0967631933984,8.51544891916857));
#197232=CARTESIAN_POINT('Ctrl Pts',(-18.7990572879299,17.0946950537844,
8.51286745236707));
#197233=CARTESIAN_POINT('Ctrl Pts',(-18.763140298489,17.0938957832013,8.51077780604867));
#197234=CARTESIAN_POINT('Ctrl Pts',(-18.6474876313785,17.0942662865556,
8.50416158025336));
#197235=CARTESIAN_POINT('Ctrl Pts',(-18.5678287752104,17.0990257784595,
8.49977504680067));
#197236=CARTESIAN_POINT('Ctrl Pts',(-18.303670200793,17.1298516104654,8.48527502577618));
#197237=CARTESIAN_POINT('Ctrl Pts',(-18.1223947764205,17.1757370078603,
8.47531877649175));
#197238=CARTESIAN_POINT('Ctrl Pts',(-17.928982359863,17.2529086555016,8.46320677996891));
#197239=CARTESIAN_POINT('Ctrl Pts',(-17.908633746059,17.2613986029627,8.46191426416473));
#197240=CARTESIAN_POINT('Ctrl Pts',(-17.8806755942569,17.2735795872288,
8.46011152509643));
#197241=CARTESIAN_POINT('Ctrl Pts',(-17.8729495613334,17.2770008955054,
8.45961048060932));
#197242=CARTESIAN_POINT('Ctrl Pts',(-17.8597038628253,17.282961572672,8.45874644290631));
#197243=CARTESIAN_POINT('Ctrl Pts',(-17.854174227724,17.2854786363202,8.45838421785751));
#197244=CARTESIAN_POINT('Ctrl Pts',(-17.8427963070774,17.2907170558703,
8.45763572271638));
#197245=CARTESIAN_POINT('Ctrl Pts',(-17.8369494767149,17.293441405057,8.45724935223141));
#197246=CARTESIAN_POINT('Ctrl Pts',(-17.8233713535461,17.2998438658396,
8.4563479868652));
#197247=CARTESIAN_POINT('Ctrl Pts',(-17.8156497815401,17.3035422222832,
8.45583229372291));
#197248=CARTESIAN_POINT('Ctrl Pts',(-17.7910027527337,17.3155316140947,
8.45417611930579));
#197249=CARTESIAN_POINT('Ctrl Pts',(-17.7741658616627,17.3240016955108,
8.45302941331345));
#197250=CARTESIAN_POINT('Ctrl Pts',(-17.6906059658894,17.367445581228,8.44725974889972));
#197251=CARTESIAN_POINT('Ctrl Pts',(-17.6256769756934,17.4057349475905,
8.44252039714175));
#197252=CARTESIAN_POINT('Ctrl Pts',(-17.471989834757,17.5077864351577,8.43066494321757));
#197253=CARTESIAN_POINT('Ctrl Pts',(-17.3858611623779,17.5751136019879,
8.42344900590162));
#197254=CARTESIAN_POINT('Ctrl Pts',(-17.2947692253699,17.6584189222742,
8.4152944800237));
#197255=CARTESIAN_POINT('Ctrl Pts',(-17.2843213512106,17.668169794222,8.41435092368692));
#197256=CARTESIAN_POINT('Ctrl Pts',(-17.1982981693816,17.7500995263564,
8.40651689939572));
#197257=CARTESIAN_POINT('Ctrl Pts',(-17.1280545891836,17.8276870070585,
8.39968927472637));
#197258=CARTESIAN_POINT('Ctrl Pts',(-17.0578713896505,17.917796338987,8.39263256760226));
#197259=CARTESIAN_POINT('Ctrl Pts',(-17.0519716884127,17.9254792516289,
8.39203740685896));
#197260=CARTESIAN_POINT('Ctrl Pts',(-17.0433375216818,17.9368843424134,
8.39116380536707));
#197261=CARTESIAN_POINT('Ctrl Pts',(-17.0405622653227,17.940575281961,8.39088260417272));
#197262=CARTESIAN_POINT('Ctrl Pts',(-17.0356596557997,17.9471400950401,
8.39038517840229));
#197263=CARTESIAN_POINT('Ctrl Pts',(-17.0335274861383,17.9500103036172,
8.39016861948917));
#197264=CARTESIAN_POINT('Ctrl Pts',(-17.0289742399249,17.9561721817755,
8.38970568205226));
#197265=CARTESIAN_POINT('Ctrl Pts',(-17.0265554252253,17.9594654536803,
8.38945946009394));
#197266=CARTESIAN_POINT('Ctrl Pts',(-17.0199406846569,17.9685264449346,
8.388785236927));
#197267=CARTESIAN_POINT('Ctrl Pts',(-17.0157643036456,17.974308459388,8.38835856985102));
#197268=CARTESIAN_POINT('Ctrl Pts',(-16.9936033866211,18.0053182423631,
8.38608865195067));
#197269=CARTESIAN_POINT('Ctrl Pts',(-16.9761440462928,18.0309188388782,
8.38427926604911));
#197270=CARTESIAN_POINT('Ctrl Pts',(-16.8700946452666,18.1939984183922,
8.37309073227626));
#197271=CARTESIAN_POINT('Ctrl Pts',(-16.7971150548607,18.3409859508417,
8.36444696119417));
#197272=CARTESIAN_POINT('Ctrl Pts',(-16.7019681138647,18.6056973860495,
8.34905212373271));
#197273=CARTESIAN_POINT('Ctrl Pts',(-16.6714655090452,18.7195826938641,
8.34248371027389));
#197274=CARTESIAN_POINT('Ctrl Pts',(-16.6480481134493,18.8494778762623,
8.3347514563089));
#197275=CARTESIAN_POINT('Ctrl Pts',(-16.6456535663897,18.8635770916592,
8.33390930298938));
#197276=CARTESIAN_POINT('Ctrl Pts',(-16.6420704779496,18.8860516789945,
8.33256188334131));
#197277=CARTESIAN_POINT('Ctrl Pts',(-16.6407889426206,18.8944119353988,
8.33205956402231));
#197278=CARTESIAN_POINT('Ctrl Pts',(-16.6386174080589,18.9091681082599,
8.33117093173656));
#197279=CARTESIAN_POINT('Ctrl Pts',(-16.6377065046466,18.9155608736227,
8.3307852858548));
#197280=CARTESIAN_POINT('Ctrl Pts',(-16.6358832135593,18.9287899410996,
8.32998581847218));
#197281=CARTESIAN_POINT('Ctrl Pts',(-16.6349749583236,18.935626726872,8.3295718711602));
#197282=CARTESIAN_POINT('Ctrl Pts',(-16.6327298227402,18.9531835015115,
8.32850679781504));
#197283=CARTESIAN_POINT('Ctrl Pts',(-16.6314415732576,18.9639094091344,
8.32785414470023));
#197284=CARTESIAN_POINT('Ctrl Pts',(-16.6264109047706,19.0086866375756,
8.3251210177569));
#197285=CARTESIAN_POINT('Ctrl Pts',(-16.6234133439509,19.0428148553765,
8.32301727512132));
#197286=CARTESIAN_POINT('Ctrl Pts',(-16.6177640404778,19.1318859648987,
8.31746992324235));
#197287=CARTESIAN_POINT('Ctrl Pts',(-16.6164232626926,19.1868833638701,
8.31398805123392));
#197288=CARTESIAN_POINT('Ctrl Pts',(-16.6188187798023,19.3511610559734,
8.30342853226656));
#197289=CARTESIAN_POINT('Ctrl Pts',(-16.6288746993541,19.4601600212713,
8.2962024614806));
#197290=CARTESIAN_POINT('Ctrl Pts',(-16.6538348611804,19.6061014651274,
8.28642180140493));
#197291=CARTESIAN_POINT('Ctrl Pts',(-16.6614195817952,19.6441312584114,
8.28386460186058));
#197292=CARTESIAN_POINT('Ctrl Pts',(-16.6765391024102,19.7103956554802,
8.27941247669198));
#197293=CARTESIAN_POINT('Ctrl Pts',(-16.6836219886273,19.7387229185453,
8.27751047142428));
#197294=CARTESIAN_POINT('Ctrl Pts',(-16.7049052557349,19.8169311006764,
8.27227724577364));
#197295=CARTESIAN_POINT('Ctrl Pts',(-16.7203568740495,19.8664542720522,
8.26898378640082));
#197296=CARTESIAN_POINT('Ctrl Pts',(-16.7404929734054,19.9235262454128,
8.26525091262465));
#197297=CARTESIAN_POINT('Ctrl Pts',(-16.7434228587391,19.931670913839,8.2647197207549));
#197298=CARTESIAN_POINT('Ctrl Pts',(-16.7479412427383,19.9439935788488,
8.26391860215429));
#197299=CARTESIAN_POINT('Ctrl Pts',(-16.7494931146006,19.9481847777726,
8.26364657598865));
#197300=CARTESIAN_POINT('Ctrl Pts',(-16.752306032159,19.9557084751685,8.26315910956213));
#197301=CARTESIAN_POINT('Ctrl Pts',(-16.7535622224513,19.9590427160238,
8.26294338597385));
#197302=CARTESIAN_POINT('Ctrl Pts',(-16.7563141961476,19.9662916140888,
8.26247505316576));
#197303=CARTESIAN_POINT('Ctrl Pts',(-16.757813182072,19.970204993673,8.26222263884353));
#197304=CARTESIAN_POINT('Ctrl Pts',(-16.7620670397321,19.9812125131534,
8.26151376283832));
#197305=CARTESIAN_POINT('Ctrl Pts',(-16.7648485905373,19.9882963693495,
8.2610588724472));
#197306=CARTESIAN_POINT('Ctrl Pts',(-16.7819343837916,20.031128887543,8.2583154128152));
#197307=CARTESIAN_POINT('Ctrl Pts',(-16.7971745171345,20.0664992874279,
8.25607965902514));
#197308=CARTESIAN_POINT('Ctrl Pts',(-16.8511153954923,20.1828470977651,
8.24876278512226));
#197309=CARTESIAN_POINT('Ctrl Pts',(-16.8939998397795,20.2617821768188,
8.24385800745585));
#197310=CARTESIAN_POINT('Ctrl Pts',(-17.0331143137692,20.4830581434268,
8.22964458679385));
#197311=CARTESIAN_POINT('Ctrl Pts',(-17.1417772167226,20.61668979378,8.22039953697715));
#197312=CARTESIAN_POINT('Ctrl Pts',(-17.2821225632538,20.7518704488831,
8.20907945685341));
#197313=CARTESIAN_POINT('Ctrl Pts',(-17.2991363799216,20.76772610319,8.20771724328775));
#197314=CARTESIAN_POINT('Ctrl Pts',(-17.3235298112837,20.7897193578265,
8.20577640190152));
#197315=CARTESIAN_POINT('Ctrl Pts',(-17.3306956155906,20.7960923519253,
8.20520771462507));
#197316=CARTESIAN_POINT('Ctrl Pts',(-17.342395822329,20.8063565465964,8.20428139542877));
#197317=CARTESIAN_POINT('Ctrl Pts',(-17.3469038845547,20.8102776692836,
8.20392501575092));
#197318=CARTESIAN_POINT('Ctrl Pts',(-17.3563643580573,20.818436319324,8.20317819700084));
#197319=CARTESIAN_POINT('Ctrl Pts',(-17.3613198544722,20.822670158324,8.2027876111085));
#197320=CARTESIAN_POINT('Ctrl Pts',(-17.3731357820508,20.8326713315079,
8.20185768248212));
#197321=CARTESIAN_POINT('Ctrl Pts',(-17.3800134008482,20.8384180816819,
8.20131750525384));
#197322=CARTESIAN_POINT('Ctrl Pts',(-17.4032144384937,20.8575553579756,
8.19949879234696));
#197323=CARTESIAN_POINT('Ctrl Pts',(-17.4197012313071,20.870744996537,8.19821219140667));
#197324=CARTESIAN_POINT('Ctrl Pts',(-17.5099226896532,20.9407360272897,
8.19120018920189));
#197325=CARTESIAN_POINT('Ctrl Pts',(-17.5871358780116,20.9928671966894,
8.18529453154263));
#197326=CARTESIAN_POINT('Ctrl Pts',(-17.7908374746254,21.1116611367534,
8.16998787943476));
#197327=CARTESIAN_POINT('Ctrl Pts',(-17.9211043921061,21.1709146918714,
8.1604250858041));
#197328=CARTESIAN_POINT('Ctrl Pts',(-18.0694780540287,21.221047752965,8.15023441275153));
#197329=CARTESIAN_POINT('Ctrl Pts',(-18.0826620844429,21.2253585376332,
8.14933502201538));
#197330=CARTESIAN_POINT('Ctrl Pts',(-18.1452850713814,21.2451552747318,
8.14509462323706));
#197331=CARTESIAN_POINT('Ctrl Pts',(-18.1952435944756,21.2589539651773,
8.1418043431698));
#197332=CARTESIAN_POINT('Ctrl Pts',(-18.2540821953621,21.2729027087739,
8.13807460621232));
#197333=CARTESIAN_POINT('Ctrl Pts',(-18.2625144527184,21.274847199825,8.13754354295905));
#197334=CARTESIAN_POINT('Ctrl Pts',(-18.2753191277537,21.2777174038476,
8.13674257940073));
#197335=CARTESIAN_POINT('Ctrl Pts',(-18.2796828262511,21.2786810383653,
8.1364705808534));
#197336=CARTESIAN_POINT('Ctrl Pts',(-18.2875311824239,21.2803881438492,
8.13598314379505));
#197337=CARTESIAN_POINT('Ctrl Pts',(-18.291014677566,21.2811366379184,8.13576742211088));
#197338=CARTESIAN_POINT('Ctrl Pts',(-18.2985997636358,21.2827464126165,
8.13529907027226));
#197339=CARTESIAN_POINT('Ctrl Pts',(-18.3027020142004,21.2836043067019,
8.13504663514132));
#197340=CARTESIAN_POINT('Ctrl Pts',(-18.3142620634424,21.2859860251302,
8.13433764182958));
#197341=CARTESIAN_POINT('Ctrl Pts',(-18.3217256590964,21.2874818351457,
8.13388265577327));
#197342=CARTESIAN_POINT('Ctrl Pts',(-18.3670193537988,21.2963054939349,
8.13113738295973));
#197343=CARTESIAN_POINT('Ctrl Pts',(-18.4050382575322,21.3026401196899,
8.12889999277953));
#197344=CARTESIAN_POINT('Ctrl Pts',(-18.5322115249753,21.3202756433572,
8.1215749713631));
#197345=CARTESIAN_POINT('Ctrl Pts',(-18.6219144331793,21.3269399137165,
8.11666412986314));
#197346=CARTESIAN_POINT('Ctrl Pts',(-18.7802711693372,21.328602455447,8.1080524359446));
#197347=CARTESIAN_POINT('Ctrl Pts',(-18.8487610398305,21.3259966753661,
8.10434710093293));
#197348=CARTESIAN_POINT('Ctrl Pts',(-19.0310225401261,21.3101819681524,
8.09432351852859));
#197349=CARTESIAN_POINT('Ctrl Pts',(-19.144037020099,21.2910605606187,8.0879268651006));
#197350=CARTESIAN_POINT('Ctrl Pts',(-19.2687608141137,21.2593952425081,
8.08038797141464));
#197351=CARTESIAN_POINT('Ctrl Pts',(-19.2825411921549,21.2557480880415,
8.07954850510587));
#197352=CARTESIAN_POINT('Ctrl Pts',(-19.3044246480172,21.2497192133218,
8.07820458210845));
#197353=CARTESIAN_POINT('Ctrl Pts',(-19.3125522702886,21.2474276508693,
8.07770304827235));
#197354=CARTESIAN_POINT('Ctrl Pts',(-19.3268682220086,21.2432986838705,
8.07681533070574));
#197355=CARTESIAN_POINT('Ctrl Pts',(-19.3330622999406,21.2414814770135,
8.07642980965722));
#197356=CARTESIAN_POINT('Ctrl Pts',(-19.3458621526463,21.2376626133774,
8.07563013415225));
#197357=CARTESIAN_POINT('Ctrl Pts',(-19.3524666353939,21.235656924383,8.07521585158188));
#197358=CARTESIAN_POINT('Ctrl Pts',(-19.3694062850543,21.2304219707778,
8.07414893078798));
#197359=CARTESIAN_POINT('Ctrl Pts',(-19.3797266046036,21.2271456763914,
8.07349475524054));
#197360=CARTESIAN_POINT('Ctrl Pts',(-19.4221500904483,21.2133187495646,
8.07078815670395));
#197361=CARTESIAN_POINT('Ctrl Pts',(-19.4540220945009,21.2020798322743,
8.06871317277053));
#197362=CARTESIAN_POINT('Ctrl Pts',(-19.5363378606131,21.1708182091661,
8.06324182460417));
#197363=CARTESIAN_POINT('Ctrl Pts',(-19.5863024304945,21.1496111617254,
8.05980816256132));
#197364=CARTESIAN_POINT('Ctrl Pts',(-19.7604204463906,21.0676752926659,
8.04744754443502));
#197365=CARTESIAN_POINT('Ctrl Pts',(-19.8793790981298,20.9967442980095,
8.03824118458765));
#197366=CARTESIAN_POINT('Ctrl Pts',(-20.0636019481919,20.8608738260176,
8.02319282210838));
#197367=CARTESIAN_POINT('Ctrl Pts',(-20.1331082337134,20.8023594796302,
8.01730392784608));
#197368=CARTESIAN_POINT('Ctrl Pts',(-20.2056248303938,20.7328747198928,
8.01109910231789));
#197369=CARTESIAN_POINT('Ctrl Pts',(-20.212553648507,20.7261440265151,8.01050562250322));
#197370=CARTESIAN_POINT('Ctrl Pts',(-20.2227227842827,20.7161294786751,
8.00963400844907));
#197371=CARTESIAN_POINT('Ctrl Pts',(-20.2259987142839,20.7128821902946,
8.00935313147938));
#197372=CARTESIAN_POINT('Ctrl Pts',(-20.2317947414299,20.7070991587303,
8.00885606385245));
#197373=CARTESIAN_POINT('Ctrl Pts',(-20.2343190520514,20.7045677162204,
8.00863954065362));
#197374=CARTESIAN_POINT('Ctrl Pts',(-20.2397172002792,20.6991268211573,
8.00817644098127));
#197375=CARTESIAN_POINT('Ctrl Pts',(-20.2425890157268,20.6962154407168,
8.00793002232114));
#197376=CARTESIAN_POINT('Ctrl Pts',(-20.2484661114418,20.6902227428497,
8.0074255841677));
#197377=CARTESIAN_POINT('Ctrl Pts',(-20.2514704690679,20.6871405427362,
8.00716763603248));
#197378=CARTESIAN_POINT('Ctrl Pts',(-20.2652694054864,20.6728974296868,
8.00598239252414));
#197379=CARTESIAN_POINT('Ctrl Pts',(-20.2759507162323,20.6616267981184,
8.00506353270242));
#197380=CARTESIAN_POINT('Ctrl Pts',(-20.341053716511,20.5914001931569,7.99944663224406));
#197381=CARTESIAN_POINT('Ctrl Pts',(-20.39221704071,20.5295011652345,7.99495937219235));
#197382=CARTESIAN_POINT('Ctrl Pts',(-20.4809424811497,20.4087975083693,
7.98672379063677));
#197383=CARTESIAN_POINT('Ctrl Pts',(-20.519351799775,20.3507571006085,7.98296163937517));
#197384=CARTESIAN_POINT('Ctrl Pts',(-20.6215884078398,20.1783793228182,
7.97206933466951));
#197385=CARTESIAN_POINT('Ctrl Pts',(-20.6777336515715,20.0599315824275,
7.96490108863878));
#197386=CARTESIAN_POINT('Ctrl Pts',(-20.7225806376299,19.9371102172836,
7.95734465602265));
#197387=CARTESIAN_POINT('Ctrl Pts',(-20.7225805951212,19.9371103337009,
7.73405229189668));
#197388=CARTESIAN_POINT('Ctrl Pts',(-20.7059081256316,19.9827708177362,
7.73726295928993));
#197389=CARTESIAN_POINT('Ctrl Pts',(-20.6876516167336,20.0278883447379,
7.7404696596753));
#197390=CARTESIAN_POINT('Ctrl Pts',(-20.6420223308054,20.1303280441212,
7.7477806534552));
#197391=CARTESIAN_POINT('Ctrl Pts',(-20.6136163554537,20.1870927986601,
7.75185458536201));
#197392=CARTESIAN_POINT('Ctrl Pts',(-20.576383744976,20.2538227232164,7.75660091562334));
#197393=CARTESIAN_POINT('Ctrl Pts',(-20.5699624506865,20.2650868060294,
7.75740054882405));
#197394=CARTESIAN_POINT('Ctrl Pts',(-20.56082238396,20.2807831524705,7.75851187618657));
#197395=CARTESIAN_POINT('Ctrl Pts',(-20.5581903057717,20.2852652118984,
7.75882887302775));
#197396=CARTESIAN_POINT('Ctrl Pts',(-20.5536739979807,20.2928913882206,
7.7593675973071));
#197397=CARTESIAN_POINT('Ctrl Pts',(-20.5517980700973,20.2960403734056,
7.75958985817844));
#197398=CARTESIAN_POINT('Ctrl Pts',(-20.5481825822257,20.3020737388305,
7.76001531982343));
#197399=CARTESIAN_POINT('Ctrl Pts',(-20.5464443125057,20.3049588473293,
7.76021860518643));
#197400=CARTESIAN_POINT('Ctrl Pts',(-20.541813441999,20.3126036402632,7.7607568486212));
#197401=CARTESIAN_POINT('Ctrl Pts',(-20.5389089077131,20.3173561170672,
7.76109103068396));
#197402=CARTESIAN_POINT('Ctrl Pts',(-20.5284943718626,20.3342464888969,
7.76227741130615));
#197403=CARTESIAN_POINT('Ctrl Pts',(-20.5208802232821,20.3463201389289,
7.76312304973539));
#197404=CARTESIAN_POINT('Ctrl Pts',(-20.4262135723245,20.4931198015513,
7.77338697852945));
#197405=CARTESIAN_POINT('Ctrl Pts',(-20.3242301878234,20.6176277329912,
7.78193357094547));
#197406=CARTESIAN_POINT('Ctrl Pts',(-20.1176551141693,20.8183139245327,
7.79760618697211));
#197407=CARTESIAN_POINT('Ctrl Pts',(-20.0183307108183,20.898734786947,7.80463064801423));
#197408=CARTESIAN_POINT('Ctrl Pts',(-19.8984138110616,20.9790814700711,
7.81300661851793));
#197409=CARTESIAN_POINT('Ctrl Pts',(-19.8843372390406,20.9882720166535,
7.81398795001884));
#197410=CARTESIAN_POINT('Ctrl Pts',(-19.8618924247821,21.0025478000978,
7.81555050508725));
#197411=CARTESIAN_POINT('Ctrl Pts',(-19.8535956196823,21.0077444129569,
7.81612764833895));
#197412=CARTESIAN_POINT('Ctrl Pts',(-19.8378158724346,21.017476149014,7.81722461744339));
#197413=CARTESIAN_POINT('Ctrl Pts',(-19.8303402576475,21.0220228030466,
7.81774400818197));
#197414=CARTESIAN_POINT('Ctrl Pts',(-19.8173503255901,21.0298133493605,
7.81864610892895));
#197415=CARTESIAN_POINT('Ctrl Pts',(-19.8118490547738,21.0330788516159,
7.8190280235752));
#197416=CARTESIAN_POINT('Ctrl Pts',(-19.8011918609186,21.0393397077895,
7.81976766989241));
#197417=CARTESIAN_POINT('Ctrl Pts',(-19.7960379123843,21.0423383157185,
7.82012527859326));
#197418=CARTESIAN_POINT('Ctrl Pts',(-19.7826193281046,21.0500696581299,
7.82105612777202));
#197419=CARTESIAN_POINT('Ctrl Pts',(-19.7743353688876,21.0547684286086,
7.82163058738429));
#197420=CARTESIAN_POINT('Ctrl Pts',(-19.7460997960504,21.0705331460496,
7.8235881083859));
#197421=CARTESIAN_POINT('Ctrl Pts',(-19.7260016533377,21.0813321026709,
7.82498064918288));
#197422=CARTESIAN_POINT('Ctrl Pts',(-19.5478706013185,21.1733650465343,
7.83731985341981));
#197423=CARTESIAN_POINT('Ctrl Pts',(-19.3803952998433,21.2347121207924,
7.84899033568395));
#197424=CARTESIAN_POINT('Ctrl Pts',(-19.1239525566482,21.2935304869191,
7.86637171246791));
#197425=CARTESIAN_POINT('Ctrl Pts',(-19.0395472050749,21.307577927766,7.87200175458928));
#197426=CARTESIAN_POINT('Ctrl Pts',(-18.9172896008661,21.3203826478635,
7.87984743408718));
#197427=CARTESIAN_POINT('Ctrl Pts',(-18.8799605886957,21.3232940462605,
7.8822014619914));
#197428=CARTESIAN_POINT('Ctrl Pts',(-18.835032090921,21.3256012647865,7.88496968505304));
#197429=CARTESIAN_POINT('Ctrl Pts',(-18.8274905441352,21.3259481115464,
7.8854321492189));
#197430=CARTESIAN_POINT('Ctrl Pts',(-18.8157732354548,21.3264242100556,
7.88614709411299));
#197431=CARTESIAN_POINT('Ctrl Pts',(-18.8115987622944,21.3265814527719,
7.88640109763492));
#197432=CARTESIAN_POINT('Ctrl Pts',(-18.8038618105417,21.326849954639,7.8868705228168));
#197433=CARTESIAN_POINT('Ctrl Pts',(-18.8002995479283,21.3269645728029,
7.88708612485283));
#197434=CARTESIAN_POINT('Ctrl Pts',(-18.7922526206524,21.3272031468839,
7.88757196792881));
#197435=CARTESIAN_POINT('Ctrl Pts',(-18.7877678538963,21.3273218435374,
7.88784191181774));
#197436=CARTESIAN_POINT('Ctrl Pts',(-18.7745505751485,21.3276296185542,
7.88863512135165));
#197437=CARTESIAN_POINT('Ctrl Pts',(-18.7658171089093,21.3277789135414,
7.88915621405879));
#197438=CARTESIAN_POINT('Ctrl Pts',(-18.7033406311677,21.3284601689682,
7.89286386473415));
#197439=CARTESIAN_POINT('Ctrl Pts',(-18.6495906671543,21.3269994492115,
7.89594749674496));
#197440=CARTESIAN_POINT('Ctrl Pts',(-18.4277929341148,21.3125051277613,
7.90844343641566));
#197441=CARTESIAN_POINT('Ctrl Pts',(-18.2615422372231,21.2814777195697,
7.91731160883427));
#197442=CARTESIAN_POINT('Ctrl Pts',(-18.0440072963975,21.2132816028175,
7.92994523889008));
#197443=CARTESIAN_POINT('Ctrl Pts',(-17.9880711769933,21.1931228414789,
7.93328606720602));
#197444=CARTESIAN_POINT('Ctrl Pts',(-17.8995223143132,21.1569313091949,
7.93878049672084));
#197445=CARTESIAN_POINT('Ctrl Pts',(-17.8663436806855,21.142365824822,7.94088728903817));
#197446=CARTESIAN_POINT('Ctrl Pts',(-17.8235791965282,21.1222677714113,
7.9436731223323));
#197447=CARTESIAN_POINT('Ctrl Pts',(-17.813638829013,21.1175009418869,7.94432571525014));
#197448=CARTESIAN_POINT('Ctrl Pts',(-17.7974972358892,21.1096047017761,
7.94539386078333));
#197449=CARTESIAN_POINT('Ctrl Pts',(-17.7912733013405,21.1065219889679,
7.94580778246322));
#197450=CARTESIAN_POINT('Ctrl Pts',(-17.7793087618844,21.1005224532569,
7.94660751524662));
#197451=CARTESIAN_POINT('Ctrl Pts',(-17.7735660660613,21.097609954022,7.94699317131128));
#197452=CARTESIAN_POINT('Ctrl Pts',(-17.7604131590436,21.0908636312334,
7.94788065867894));
#197453=CARTESIAN_POINT('Ctrl Pts',(-17.7530121812613,21.0870121282368,
7.94838310969595));
#197454=CARTESIAN_POINT('Ctrl Pts',(-17.7333358995081,21.0766242289473,
7.94972724318828));
#197455=CARTESIAN_POINT('Ctrl Pts',(-17.7211020684611,21.070010535593,7.95057165702834));
#197456=CARTESIAN_POINT('Ctrl Pts',(-17.6244979286178,21.0165489989904,
7.95730995360965));
#197457=CARTESIAN_POINT('Ctrl Pts',(-17.5433670933995,20.9641088965459,
7.96340628651434));
#197458=CARTESIAN_POINT('Ctrl Pts',(-17.3555905179406,20.8236749875157,
7.97859188909507));
#197459=CARTESIAN_POINT('Ctrl Pts',(-17.2534258940791,20.7304175344374,
7.98781904442629));
#197460=CARTESIAN_POINT('Ctrl Pts',(-17.1264880300849,20.589500763277,8.00021586564108));
#197461=CARTESIAN_POINT('Ctrl Pts',(-17.0933185488935,20.549851814843,8.00355674254035));
#197462=CARTESIAN_POINT('Ctrl Pts',(-17.0449390794276,20.4875200178973,
8.00854439749442));
#197463=CARTESIAN_POINT('Ctrl Pts',(-17.0286622677056,20.465692604177,8.01024420199237));
#197464=CARTESIAN_POINT('Ctrl Pts',(-17.0088269594253,20.4379938001621,
8.01233734662302));
#197465=CARTESIAN_POINT('Ctrl Pts',(-17.0048706605102,20.432412107289,8.01275596403065));
#197466=CARTESIAN_POINT('Ctrl Pts',(-16.9986317825306,20.4235189990875,
8.01341777080889));
#197467=CARTESIAN_POINT('Ctrl Pts',(-16.9963315008191,20.420220145767,8.01366214539806));
#197468=CARTESIAN_POINT('Ctrl Pts',(-16.9919965104328,20.4139653857415,
8.01412334436727));
#197469=CARTESIAN_POINT('Ctrl Pts',(-16.9899599425139,20.4110108978688,
8.01434029081668));
#197470=CARTESIAN_POINT('Ctrl Pts',(-16.9853023300974,20.4042171087152,
8.01483710480832));
#197471=CARTESIAN_POINT('Ctrl Pts',(-16.9826864142448,20.4003743458416,
8.01511662349943));
#197472=CARTESIAN_POINT('Ctrl Pts',(-16.9757366084039,20.3900924854034,
8.01586062619177));
#197473=CARTESIAN_POINT('Ctrl Pts',(-16.9714253902685,20.3836380484482,
8.01632362143275));
#197474=CARTESIAN_POINT('Ctrl Pts',(-16.9403725292692,20.3365898217684,
8.01967033045463));
#197475=CARTESIAN_POINT('Ctrl Pts',(-16.9149983631457,20.2951059854337,
8.02246960419527));
#197476=CARTESIAN_POINT('Ctrl Pts',(-16.8776488356574,20.2290341465277,
8.02675538725693));
#197477=CARTESIAN_POINT('Ctrl Pts',(-16.8646843920881,20.205028378103,8.02827838995078));
#197478=CARTESIAN_POINT('Ctrl Pts',(-16.8320346153005,20.1416728833261,
8.03222637896995));
#197479=CARTESIAN_POINT('Ctrl Pts',(-16.8131053414653,20.1019479545533,
8.03463153073949));
#197480=CARTESIAN_POINT('Ctrl Pts',(-16.7514944818302,19.9615428790987,
8.04297926617324));
#197481=CARTESIAN_POINT('Ctrl Pts',(-16.7153842798536,19.8581726444359,
8.048866543847));
#197482=CARTESIAN_POINT('Ctrl Pts',(-16.6733296115924,19.6992227593264,
8.05800899104279));
#197483=CARTESIAN_POINT('Ctrl Pts',(-16.6613239008439,19.6454387823337,
8.06111542466533));
#197484=CARTESIAN_POINT('Ctrl Pts',(-16.6452691824588,19.557509689075,8.0662578032176));
#197485=CARTESIAN_POINT('Ctrl Pts',(-16.6399297149581,19.5236257149206,
8.0682543932694));
#197486=CARTESIAN_POINT('Ctrl Pts',(-16.6339934187422,19.4789144804222,
8.07091444373784));
#197487=CARTESIAN_POINT('Ctrl Pts',(-16.632653030641,19.468190042488,8.0715543892965));
#197488=CARTESIAN_POINT('Ctrl Pts',(-16.6305917976356,19.4506049162507,
8.07260702162063));
#197489=CARTESIAN_POINT('Ctrl Pts',(-16.6298222525402,19.4437500526939,
8.07301816753006));
#197490=CARTESIAN_POINT('Ctrl Pts',(-16.6283972524419,19.4304715502349,
8.07381622841105));
#197491=CARTESIAN_POINT('Ctrl Pts',(-16.6277376567048,19.424048425647,8.07420300810208));
#197492=CARTESIAN_POINT('Ctrl Pts',(-16.6262822125982,19.4092075189795,
8.07509842776938));
#197493=CARTESIAN_POINT('Ctrl Pts',(-16.6255073941229,19.4007878279325,
8.07560772406402));
#197494=CARTESIAN_POINT('Ctrl Pts',(-16.6235586533811,19.3781244482184,
8.07698219133443));
#197495=CARTESIAN_POINT('Ctrl Pts',(-16.6224785135233,19.3638733303569,
8.07785029143001));
#197496=CARTESIAN_POINT('Ctrl Pts',(-16.6138821960484,19.232865412346,8.08586685095066));
#197497=CARTESIAN_POINT('Ctrl Pts',(-16.6159139970288,19.1157033712371,
8.09331790069542));
#197498=CARTESIAN_POINT('Ctrl Pts',(-16.6439261312307,18.8369532615406,
8.11161841221763));
#197499=CARTESIAN_POINT('Ctrl Pts',(-16.678961738514,18.6770172015832,8.12260913299497));
#197500=CARTESIAN_POINT('Ctrl Pts',(-16.7424115425657,18.4924696231516,
8.13500301822888));
#197501=CARTESIAN_POINT('Ctrl Pts',(-16.7534868025287,18.4624826542192,
8.13700540556683));
#197502=CARTESIAN_POINT('Ctrl Pts',(-16.7678850706322,18.4260586319558,
8.13941367108017));
#197503=CARTESIAN_POINT('Ctrl Pts',(-16.7705667948012,18.4193745084273,
8.13985460542663));
#197504=CARTESIAN_POINT('Ctrl Pts',(-16.7748291971933,18.4089055001951,
8.1405434928729));
#197505=CARTESIAN_POINT('Ctrl Pts',(-16.7763868242902,18.4051113748571,
8.14079279861833));
#197506=CARTESIAN_POINT('Ctrl Pts',(-16.7793220711869,18.3980203190071,
8.14125803784942));
#197507=CARTESIAN_POINT('Ctrl Pts',(-16.7806969960787,18.3947223865673,
8.14147412369647));
#197508=CARTESIAN_POINT('Ctrl Pts',(-16.7838587973271,18.387192137581,8.14196687342175));
#197509=CARTESIAN_POINT('Ctrl Pts',(-16.7856511012649,18.3829621540919,
8.14224320387674));
#197510=CARTESIAN_POINT('Ctrl Pts',(-16.7903707548436,18.3719235536176,
8.14296319095771));
#197511=CARTESIAN_POINT('Ctrl Pts',(-16.7933201421351,18.3651243481323,
8.14340554157212));
#197512=CARTESIAN_POINT('Ctrl Pts',(-16.8130208723595,18.320353828152,8.14631173183565));
#197513=CARTESIAN_POINT('Ctrl Pts',(-16.8308512241318,18.2828638773544,
8.14871420285737));
#197514=CARTESIAN_POINT('Ctrl Pts',(-16.856854723179,18.2320945458635,8.15195670077456));
#197515=CARTESIAN_POINT('Ctrl Pts',(-16.8640879328477,18.2183474126275,
8.15283355396699));
#197516=CARTESIAN_POINT('Ctrl Pts',(-16.9510819817204,18.057336008428,8.16310429943982));
#197517=CARTESIAN_POINT('Ctrl Pts',(-17.0478976167338,17.9199526745816,
8.1719219540689));
#197518=CARTESIAN_POINT('Ctrl Pts',(-17.1991011828333,17.7518181780007,
8.18446065900252));
#197519=CARTESIAN_POINT('Ctrl Pts',(-17.240094160354,17.7098769015472,8.18775790768115));
#197520=CARTESIAN_POINT('Ctrl Pts',(-17.3088923979976,17.645099493803,8.19318708614097));
#197521=CARTESIAN_POINT('Ctrl Pts',(-17.3356318961005,17.6211753257712,
8.19527364775611));
#197522=CARTESIAN_POINT('Ctrl Pts',(-17.3713355287599,17.5908286461716,
8.19803642376453));
#197523=CARTESIAN_POINT('Ctrl Pts',(-17.3797609550363,17.5837795849484,
8.19868674200622));
#197524=CARTESIAN_POINT('Ctrl Pts',(-17.3935956969629,17.5723867368785,
8.19975209617776));
#197525=CARTESIAN_POINT('Ctrl Pts',(-17.3989722426677,17.5680033453869,
8.20016551751472));
#197526=CARTESIAN_POINT('Ctrl Pts',(-17.4093831264271,17.5596004000483,
8.20096493711652));
#197527=CARTESIAN_POINT('Ctrl Pts',(-17.4144144649471,17.5555772398776,
8.20135078385419));
#197528=CARTESIAN_POINT('Ctrl Pts',(-17.4260191713226,17.5463844029268,
8.20223964463269));
#197529=CARTESIAN_POINT('Ctrl Pts',(-17.4326049336731,17.5412306110087,
8.20274328472942));
#197530=CARTESIAN_POINT('Ctrl Pts',(-17.4502763470162,17.5275696198153,
8.20409267074068));
#197531=CARTESIAN_POINT('Ctrl Pts',(-17.4614158399239,17.5191330421731,
8.20494118178057));
#197532=CARTESIAN_POINT('Ctrl Pts',(-17.5530591320337,17.4511434569791,
8.21190585675373));
#197533=CARTESIAN_POINT('Ctrl Pts',(-17.6376005716226,17.3972691324647,
8.21824065428656));
#197534=CARTESIAN_POINT('Ctrl Pts',(-17.8766910709276,17.2677480485023,
8.23588031393972));
#197535=CARTESIAN_POINT('Ctrl Pts',(-18.0371444923131,17.2046114781734,
8.24747418828235));
#197536=CARTESIAN_POINT('Ctrl Pts',(-18.2421074788598,17.1515523289697,
8.26101541126133));
#197537=CARTESIAN_POINT('Ctrl Pts',(-18.2810361568902,17.1426414248922,
8.26353024509604));
#197538=CARTESIAN_POINT('Ctrl Pts',(-18.3277358010742,17.1333336402528,
8.26646116532803));
#197539=CARTESIAN_POINT('Ctrl Pts',(-18.3352835356523,17.1318719887964,
8.26693221048458));
#197540=CARTESIAN_POINT('Ctrl Pts',(-18.3469741293242,17.1296740578538,
8.26765751927432));
#197541=CARTESIAN_POINT('Ctrl Pts',(-18.3511114120148,17.1289089760713,
8.2679133758901));
#197542=CARTESIAN_POINT('Ctrl Pts',(-18.3587553666576,17.127518982115,8.26838452603219));
#197543=CARTESIAN_POINT('Ctrl Pts',(-18.3622613077221,17.1268905902695,
8.26860001080609));
#197544=CARTESIAN_POINT('Ctrl Pts',(-18.3701492747312,17.1254973181441,
8.2690834644603));
#197545=CARTESIAN_POINT('Ctrl Pts',(-18.3745321215583,17.1247374011151,
8.26935114908574));
#197546=CARTESIAN_POINT('Ctrl Pts',(-18.3857515363549,17.1228285354607,
8.27003405143593));
#197547=CARTESIAN_POINT('Ctrl Pts',(-18.3925914726191,17.1216993327484,
8.27044817418967));
#197548=CARTESIAN_POINT('Ctrl Pts',(-18.4325569593004,17.1153029495475,
8.27285563263566));
#197549=CARTESIAN_POINT('Ctrl Pts',(-18.4658003924063,17.1107897038376,
8.27480912193584));
#197550=CARTESIAN_POINT('Ctrl Pts',(-18.5173161577985,17.1050390230867,
8.27778010475004));
#197551=CARTESIAN_POINT('Ctrl Pts',(-18.5355192604008,17.1032455183656,
8.27881910965807));
#197552=CARTESIAN_POINT('Ctrl Pts',(-18.5848659527931,17.0990284805709,
8.28161193344054));
#197553=CARTESIAN_POINT('Ctrl Pts',(-18.6160442207572,17.0970578945792,
8.28335091143438));
#197554=CARTESIAN_POINT('Ctrl Pts',(-18.6857196928507,17.0942005329805,
8.28720145669691));
#197555=CARTESIAN_POINT('Ctrl Pts',(-18.7242204789699,17.0936725663777,
8.28930500759233));
#197556=CARTESIAN_POINT('Ctrl Pts',(-18.8719901639284,17.0956770990601,
8.29735064100863));
#197557=CARTESIAN_POINT('Ctrl Pts',(-18.980985409116,17.1056188997904,8.30323557223068));
#197558=CARTESIAN_POINT('Ctrl Pts',(-19.1429757530996,17.1331510207277,
8.31237256474343));
#197559=CARTESIAN_POINT('Ctrl Pts',(-19.1968464535868,17.1444835919757,
8.31547587219654));
#197560=CARTESIAN_POINT('Ctrl Pts',(-19.2834498064641,17.166258326963,8.32061353689087));
#197561=CARTESIAN_POINT('Ctrl Pts',(-19.3164783828135,17.1754208841652,
8.32260863380442));
#197562=CARTESIAN_POINT('Ctrl Pts',(-19.3596071713676,17.188520973581,8.32526697685399));
#197563=CARTESIAN_POINT('Ctrl Pts',(-19.3699213037584,17.1917402757332,
8.32590674664606));
#197564=CARTESIAN_POINT('Ctrl Pts',(-19.3867782964009,17.1971437319635,
8.32695916350532));
#197565=CARTESIAN_POINT('Ctrl Pts',(-19.3933360061244,17.199281182208,8.32737027095488));
#197566=CARTESIAN_POINT('Ctrl Pts',(-19.4060125448454,17.2034816725861,
8.32816830984156));
#197567=CARTESIAN_POINT('Ctrl Pts',(-19.4121326172762,17.2055407390612,
8.32855510627682));
#197568=CARTESIAN_POINT('Ctrl Pts',(-19.4262461202849,17.2103611449444,
8.32945064144796));
#197569=CARTESIAN_POINT('Ctrl Pts',(-19.4342325758616,17.2131424335383,
8.32996003703496));
#197570=CARTESIAN_POINT('Ctrl Pts',(-19.4556758288085,17.2207544329344,
8.33133494603361));
#197571=CARTESIAN_POINT('Ctrl Pts',(-19.4691005273186,17.2256736746559,
8.33220339149475));
#197572=CARTESIAN_POINT('Ctrl Pts',(-19.592328785133,17.2722496910301,8.34024729981518));
#197573=CARTESIAN_POINT('Ctrl Pts',(-19.6985198071124,17.3228329826092,
8.34772775414923));
#197574=CARTESIAN_POINT('Ctrl Pts',(-19.9414512150667,17.4644115162342,
8.366097995634));
#197575=CARTESIAN_POINT('Ctrl Pts',(-20.0728962069752,17.5630112190283,
8.37712903630611));
#197576=CARTESIAN_POINT('Ctrl Pts',(-20.2141768423464,17.697154076175,8.38949108659114));
#197577=CARTESIAN_POINT('Ctrl Pts',(-20.2362207425394,17.719026125441,8.39143502611078));
#197578=CARTESIAN_POINT('Ctrl Pts',(-20.2627314364054,17.7465136959262,
8.39378284325434));
#197579=CARTESIAN_POINT('Ctrl Pts',(-20.2676601513897,17.7516760185421,
8.39421977215372));
#197580=CARTESIAN_POINT('Ctrl Pts',(-20.2753701238397,17.7598336257244,
8.39490380395357));
#197581=CARTESIAN_POINT('Ctrl Pts',(-20.2781689225278,17.7628121517406,
8.39515222878185));
#197582=CARTESIAN_POINT('Ctrl Pts',(-20.2833998748466,17.7684114200506,
8.39561671695541));
#197583=CARTESIAN_POINT('Ctrl Pts',(-20.2858339871367,17.7710301879021,
8.39583292732478));
#197584=CARTESIAN_POINT('Ctrl Pts',(-20.2913956814051,17.7770442821801,
8.39632712641415));
#197585=CARTESIAN_POINT('Ctrl Pts',(-20.2945187948374,17.7804436742958,
8.39660477424792));
#197586=CARTESIAN_POINT('Ctrl Pts',(-20.3041550089116,17.7910014403703,
8.39746196491707));
#197587=CARTESIAN_POINT('Ctrl Pts',(-20.3106302663716,17.7981943967577,
8.39803871563367));
#197588=CARTESIAN_POINT('Ctrl Pts',(-20.3791740923844,17.8753935760489,
8.40415511606866));
#197589=CARTESIAN_POINT('Ctrl Pts',(-20.436594232468,17.9494059028784,8.40937983738445));
#197590=CARTESIAN_POINT('Ctrl Pts',(-20.5627793036262,18.1364358418443,
8.4217570558849));
#197591=CARTESIAN_POINT('Ctrl Pts',(-20.626221908922,18.2525541619432,8.42880645400543));
#197592=CARTESIAN_POINT('Ctrl Pts',(-20.7007281723604,18.4256038098187,
8.43927202716953));
#197593=CARTESIAN_POINT('Ctrl Pts',(-20.7209425133857,18.4782478969764,
8.44244777749486));
#197594=CARTESIAN_POINT('Ctrl Pts',(-20.7502231604259,18.5646645643423,
8.44769454993827));
#197595=CARTESIAN_POINT('Ctrl Pts',(-20.7605967214757,18.597965865278,8.44972408798674));
#197596=CARTESIAN_POINT('Ctrl Pts',(-20.7731190924357,18.6419652347483,
8.4524217926519));
#197597=CARTESIAN_POINT('Ctrl Pts',(-20.7760149186633,18.6524462402941,
8.45306558621039));
#197598=CARTESIAN_POINT('Ctrl Pts',(-20.780619322395,18.6696257019675,8.45412293658782));
#197599=CARTESIAN_POINT('Ctrl Pts',(-20.7823760845448,18.6763111223398,
8.45453492534631));
#197600=CARTESIAN_POINT('Ctrl Pts',(-20.785709036761,18.6892523151405,8.45533347655018));
#197601=CARTESIAN_POINT('Ctrl Pts',(-20.7872894372562,18.6955069315638,
8.45571989764198));
#197602=CARTESIAN_POINT('Ctrl Pts',(-20.7908666324012,18.7099415644316,
8.45661282583453));
#197603=CARTESIAN_POINT('Ctrl Pts',(-20.7928432517832,18.7181264252095,
8.45711997776139));
#197604=CARTESIAN_POINT('Ctrl Pts',(-20.7980153380129,18.7401173182463,
8.45848491741164));
#197605=CARTESIAN_POINT('Ctrl Pts',(-20.8011210540926,18.7539438241007,
8.45934557141486));
#197606=CARTESIAN_POINT('Ctrl Pts',(-20.835418189816,18.914138118302,8.46934714878289));
#197607=CARTESIAN_POINT('Ctrl Pts',(-20.8511375062333,19.0633573065089,
8.47899867178888));
#197608=CARTESIAN_POINT('Ctrl Pts',(-20.8508605241245,19.3627302277456,
8.49872823249889));
#197609=CARTESIAN_POINT('Ctrl Pts',(-20.8348287881732,19.5120733039284,
8.50874338999506));
#197610=CARTESIAN_POINT('Ctrl Pts',(-20.7998455026436,19.6738371168233,
8.51906813430362));
#197611=CARTESIAN_POINT('Ctrl Pts',(-20.7963536195941,19.6891562701088,
8.52004022624648));
#197612=CARTESIAN_POINT('Ctrl Pts',(-20.7913410449969,19.7100695229154,
8.5213581947173));
#197613=CARTESIAN_POINT('Ctrl Pts',(-20.7899675523737,19.7156979190889,
8.52171199357563));
#197614=CARTESIAN_POINT('Ctrl Pts',(-20.7877485339342,19.7246317738117,
8.52227205176301));
#197615=CARTESIAN_POINT('Ctrl Pts',(-20.7869181049227,19.7279409004603,
8.52247916680007));
#197616=CARTESIAN_POINT('Ctrl Pts',(-20.7851867319715,19.7347701723075,
8.52290589698809));
#197617=CARTESIAN_POINT('Ctrl Pts',(-20.784284724395,19.7382900073752,8.52312544347718));
#197618=CARTESIAN_POINT('Ctrl Pts',(-20.7821142197515,19.7466700224278,
8.52364723769655));
#197619=CARTESIAN_POINT('Ctrl Pts',(-20.7808374690448,19.7515280812075,
8.52394900964438));
#197620=CARTESIAN_POINT('Ctrl Pts',(-20.7764750779721,19.7678899464896,
8.52496307732118));
#197621=CARTESIAN_POINT('Ctrl Pts',(-20.7733095863126,19.7793724857016,
8.5256709046725));
#197622=CARTESIAN_POINT('Ctrl Pts',(-20.7559961610421,19.8401680194646,
8.52940116969203));
#197623=CARTESIAN_POINT('Ctrl Pts',(-20.7401620000124,19.8889605746082,
8.53233413666553));
#197624=CARTESIAN_POINT('Ctrl Pts',(-20.7225805753213,19.9371103879265,
8.53521114927006));
#197625=CARTESIAN_POINT('Origin',(-18.734,19.211,0.));
#197626=CARTESIAN_POINT('',(-20.7242505210392,19.9377358132316,9.55561791545399));
#197627=CARTESIAN_POINT('',(-20.7225805876262,19.9371103542273,9.33206810105871));
#197628=CARTESIAN_POINT('',(-20.7225806064498,19.9371103026755,0.));
#197629=CARTESIAN_POINT('',(-20.8516474640139,19.2128935159626,9.51094372097752));
#197630=CARTESIAN_POINT('Ctrl Pts',(-20.8516474640139,19.2128935159626,
9.51094372097752));
#197631=CARTESIAN_POINT('Ctrl Pts',(-20.8529701716602,19.3558822341493,
9.51955279572483));
#197632=CARTESIAN_POINT('Ctrl Pts',(-20.8300642449213,19.60279312627,9.53444419388365));
#197633=CARTESIAN_POINT('Ctrl Pts',(-20.7608946891188,19.8401887340949,
9.54933559204247));
#197634=CARTESIAN_POINT('Ctrl Pts',(-20.7242505210392,19.9377358132316,
9.55561791545399));
#197635=CARTESIAN_POINT('Ctrl Pts',(-20.8509991358369,19.2129128162075,
9.51057061419727));
#197636=CARTESIAN_POINT('Ctrl Pts',(-20.8511559691561,19.0393383766676,
9.5011330483765));
#197637=CARTESIAN_POINT('Ctrl Pts',(-20.8299671724295,18.8664171384252,
9.49177670366586));
#197638=CARTESIAN_POINT('Ctrl Pts',(-20.7843368967414,18.6837193760699,
9.48081374476068));
#197639=CARTESIAN_POINT('Ctrl Pts',(-20.7806161718462,18.6694573187251,
9.47995111246624));
#197640=CARTESIAN_POINT('Ctrl Pts',(-20.773518702582,18.6433701286444,9.47836008568776));
#197641=CARTESIAN_POINT('Ctrl Pts',(-20.7701872476492,18.6315332693462,
9.47763316323647));
#197642=CARTESIAN_POINT('Ctrl Pts',(-20.764734343102,18.6127866086901,9.47647366771282));
#197643=CARTESIAN_POINT('Ctrl Pts',(-20.7626802698959,18.6058573768575,
9.47604329462245));
#197644=CARTESIAN_POINT('Ctrl Pts',(-20.7587476230344,18.5928360210117,
9.4752311027985));
#197645=CARTESIAN_POINT('Ctrl Pts',(-20.7568769301004,18.5867415870071,
9.47484954600881));
#197646=CARTESIAN_POINT('Ctrl Pts',(-20.752608361724,18.5730559129435,9.4739894745682));
#197647=CARTESIAN_POINT('Ctrl Pts',(-20.7501951460048,18.5654695926931,
9.47351046013454));
#197648=CARTESIAN_POINT('Ctrl Pts',(-20.7439317413241,18.5461573762994,
9.4722852100489));
#197649=CARTESIAN_POINT('Ctrl Pts',(-20.7400217357975,18.5344513288329,
9.47153701225101));
#197650=CARTESIAN_POINT('Ctrl Pts',(-20.7162375517952,18.4652638756844,
9.4670815034937));
#197651=CARTESIAN_POINT('Ctrl Pts',(-20.6939978155362,18.4086313417106,
9.46329619240764));
#197652=CARTESIAN_POINT('Ctrl Pts',(-20.6538456531141,18.3180577755908,
9.45700994059909));
#197653=CARTESIAN_POINT('Ctrl Pts',(-20.637393387781,18.2835052489031,9.45455461815358));
#197654=CARTESIAN_POINT('Ctrl Pts',(-20.6004011271601,18.2109498055082,
9.44928102316068));
#197655=CARTESIAN_POINT('Ctrl Pts',(-20.5796160197152,18.1730911319284,
9.44645782497732));
#197656=CARTESIAN_POINT('Ctrl Pts',(-20.5313904732275,18.0912866216843,
9.44021384017038));
#197657=CARTESIAN_POINT('Ctrl Pts',(-20.5034647752896,18.0476578976974,
9.43678795584091));
#197658=CARTESIAN_POINT('Ctrl Pts',(-20.4261773035582,17.9361416352318,
9.42782578576444));
#197659=CARTESIAN_POINT('Ctrl Pts',(-20.3743265135844,17.8700829118253,
9.42230396495895));
#197660=CARTESIAN_POINT('Ctrl Pts',(-20.2941750854437,17.7795987783291,
9.41459171138658));
#197661=CARTESIAN_POINT('Ctrl Pts',(-20.2689389923727,17.752569875177,9.41226741038714));
#197662=CARTESIAN_POINT('Ctrl Pts',(-20.237711667764,17.7208331616046,9.40952769656623));
#197663=CARTESIAN_POINT('Ctrl Pts',(-20.2323883056122,17.7154805332041,
9.40906525154867));
#197664=CARTESIAN_POINT('Ctrl Pts',(-20.2240722599483,17.7072077469141,
9.40835010409874));
#197665=CARTESIAN_POINT('Ctrl Pts',(-20.2210994270836,17.7042678489612,
9.4080958804236));
#197666=CARTESIAN_POINT('Ctrl Pts',(-20.2155764514367,17.6988383289213,
9.40762625232393));
#197667=CARTESIAN_POINT('Ctrl Pts',(-20.2130287538194,17.6963463608455,
9.40741066622708));
#197668=CARTESIAN_POINT('Ctrl Pts',(-20.2072629717085,17.6907351213598,
9.40692511614676));
#197669=CARTESIAN_POINT('Ctrl Pts',(-20.2040412768835,17.6876196370761,
9.40665544774422));
#197670=CARTESIAN_POINT('Ctrl Pts',(-20.1945271404959,17.6784774433315,
9.40586379744822));
#197671=CARTESIAN_POINT('Ctrl Pts',(-20.1882072705577,17.6724792380394,
9.40534397574228));
#197672=CARTESIAN_POINT('Ctrl Pts',(-20.1430187722334,17.6301179312946,
9.40166826143151));
#197673=CARTESIAN_POINT('Ctrl Pts',(-20.1028245138211,17.5951898380279,
9.39861329471255));
#197674=CARTESIAN_POINT('Ctrl Pts',(-20.0473663573213,17.5505542303653,
9.39460933187972));
#197675=CARTESIAN_POINT('Ctrl Pts',(-20.0332369662225,17.5394753446671,
9.39360664033081));
#197676=CARTESIAN_POINT('Ctrl Pts',(-19.8680039002404,17.4132768455391,
9.38205940906762));
#197677=CARTESIAN_POINT('Ctrl Pts',(-19.7022117454792,17.3188201487658,
9.37209533211099));
#197678=CARTESIAN_POINT('Ctrl Pts',(-19.4761253839409,17.2276101249819,
9.35828423896989));
#197679=CARTESIAN_POINT('Ctrl Pts',(-19.4254688054686,17.2093867359589,
9.35518351965897));
#197680=CARTESIAN_POINT('Ctrl Pts',(-19.3621326820846,17.189293302759,9.35127493777951));
#197681=CARTESIAN_POINT('Ctrl Pts',(-19.3500557423843,17.1855805501502,
9.35052828883226));
#197682=CARTESIAN_POINT('Ctrl Pts',(-19.3309481249756,17.1798930967592,
9.34934454829694));
#197683=CARTESIAN_POINT('Ctrl Pts',(-19.3239391025258,17.1778462503868,
9.34890981937109));
#197684=CARTESIAN_POINT('Ctrl Pts',(-19.3107990751556,17.1740826324432,
9.34809380708692));
#197685=CARTESIAN_POINT('Ctrl Pts',(-19.3046706277604,17.1723571748354,
9.3477128120859));
#197686=CARTESIAN_POINT('Ctrl Pts',(-19.2909642967012,17.1685648191219,
9.34685975621558));
#197687=CARTESIAN_POINT('Ctrl Pts',(-19.2833825342924,17.1665124054402,
9.34638723044095));
#197688=CARTESIAN_POINT('Ctrl Pts',(-19.2641915353184,17.1614317823313,
9.34518944998548));
#197689=CARTESIAN_POINT('Ctrl Pts',(-19.2525677664978,17.15846001129,9.3444623809298));
#197690=CARTESIAN_POINT('Ctrl Pts',(-19.1869849573172,17.1422855431112,
9.34035074575119));
#197691=CARTESIAN_POINT('Ctrl Pts',(-19.1325521135701,17.1311129391091,
9.33690150386763));
#197692=CARTESIAN_POINT('Ctrl Pts',(-19.0530877062572,17.1180364154442,
9.33181011684537));
#197693=CARTESIAN_POINT('Ctrl Pts',(-19.0283595798706,17.1144156598576,
9.3302181370853));
#197694=CARTESIAN_POINT('Ctrl Pts',(-18.8435190769908,17.0906853214812,
9.31826531538477));
#197695=CARTESIAN_POINT('Ctrl Pts',(-18.6816452567446,17.0885064889055,
9.30744571711568));
#197696=CARTESIAN_POINT('Ctrl Pts',(-18.472364140057,17.1096582020175,9.29371900255726));
#197697=CARTESIAN_POINT('Ctrl Pts',(-18.4237880965037,17.1162780889317,
9.29055634194354));
#197698=CARTESIAN_POINT('Ctrl Pts',(-18.3495961162417,17.1290267639684,
9.28580257402245));
#197699=CARTESIAN_POINT('Ctrl Pts',(-18.323793152767,17.1339565746499,9.28416376714254));
#197700=CARTESIAN_POINT('Ctrl Pts',(-18.2914718063994,17.1407576227936,
9.28213485044928));
#197701=CARTESIAN_POINT('Ctrl Pts',(-18.2848629142585,17.1421813555613,
9.28172125283126));
#197702=CARTESIAN_POINT('Ctrl Pts',(-18.2743511524818,17.1444986170921,
9.28106554524337));
#197703=CARTESIAN_POINT('Ctrl Pts',(-18.2704438668137,17.1453715870018,
9.28082228646957));
#197704=CARTESIAN_POINT('Ctrl Pts',(-18.2630347853453,17.1470490132159,
9.28036194045529));
#197705=CARTESIAN_POINT('Ctrl Pts',(-18.2595326054409,17.147851289675,9.28014473815641));
#197706=CARTESIAN_POINT('Ctrl Pts',(-18.2514718861814,17.1497194429433,
9.2796457108216));
#197707=CARTESIAN_POINT('Ctrl Pts',(-18.2469148297085,17.150791526721,9.27936424543075));
#197708=CARTESIAN_POINT('Ctrl Pts',(-18.2347025832605,17.1537073398141,
9.27861162665503));
#197709=CARTESIAN_POINT('Ctrl Pts',(-18.2270539768432,17.1555786967189,
9.27814201695103));
#197710=CARTESIAN_POINT('Ctrl Pts',(-18.1696396492156,17.1699660343753,
9.2746289165798));
#197711=CARTESIAN_POINT('Ctrl Pts',(-18.1203289767207,17.1842461798905,
9.2716796097489));
#197712=CARTESIAN_POINT('Ctrl Pts',(-18.0580841587589,17.2047525718405,
9.26798767910132));
#197713=CARTESIAN_POINT('Ctrl Pts',(-18.0446311652383,17.2093352952193,
9.26719163207716));
#197714=CARTESIAN_POINT('Ctrl Pts',(-17.8962977516328,17.2615374856272,
9.25842527575048));
#197715=CARTESIAN_POINT('Ctrl Pts',(-17.7665260879398,17.3225754600111,
9.25083107093263));
#197716=CARTESIAN_POINT('Ctrl Pts',(-17.5641927797872,17.4441143205237,
9.23783246533079));
#197717=CARTESIAN_POINT('Ctrl Pts',(-17.4877379719492,17.497184957882,9.23261225904014));
#197718=CARTESIAN_POINT('Ctrl Pts',(-17.3985182025594,17.5682514972969,
9.22596832926444));
#197719=CARTESIAN_POINT('Ctrl Pts',(-17.3822107581231,17.5816442768511,
9.22472990058551));
#197720=CARTESIAN_POINT('Ctrl Pts',(-17.3592678173514,17.6010681013727,
9.2229515322736));
#197721=CARTESIAN_POINT('Ctrl Pts',(-17.3524658875809,17.6069012546947,
9.22241968175527));
#197722=CARTESIAN_POINT('Ctrl Pts',(-17.3407808917075,17.6170514455098,
9.22149790146752));
#197723=CARTESIAN_POINT('Ctrl Pts',(-17.3358803166845,17.6213482055074,
9.22110881587689));
#197724=CARTESIAN_POINT('Ctrl Pts',(-17.3265251231498,17.6296274398158,
9.22036120163581));
#197725=CARTESIAN_POINT('Ctrl Pts',(-17.3220673647039,17.6336062839874,
9.22000282723378));
#197726=CARTESIAN_POINT('Ctrl Pts',(-17.3104975240537,17.6440214714459,
9.21906706637876));
#197727=CARTESIAN_POINT('Ctrl Pts',(-17.3034122950557,17.6504873208781,
9.21848843516319));
#197728=CARTESIAN_POINT('Ctrl Pts',(-17.2792900875575,17.672803150644,9.21649902038868));
#197729=CARTESIAN_POINT('Ctrl Pts',(-17.2624710974058,17.6888853204343,
9.21507832483139));
#197730=CARTESIAN_POINT('Ctrl Pts',(-17.1239831722456,17.8257471635445,
9.20309061536465));
#197731=CARTESIAN_POINT('Ctrl Pts',(-17.0171565492406,17.9605975606064,
9.19185603875112));
#197732=CARTESIAN_POINT('Ctrl Pts',(-16.8808909923973,18.1835007217766,
9.17459208411309));
#197733=CARTESIAN_POINT('Ctrl Pts',(-16.8389388339357,18.2631007839323,
9.16866114095377));
#197734=CARTESIAN_POINT('Ctrl Pts',(-16.7864087608085,18.3802998744849,
9.16045626214705));
#197735=CARTESIAN_POINT('Ctrl Pts',(-16.7716077329849,18.4158953805543,
9.15803083968417));
#197736=CARTESIAN_POINT('Ctrl Pts',(-16.7550562675883,18.458983610703,9.15519024499545));
#197737=CARTESIAN_POINT('Ctrl Pts',(-16.7523649478733,18.4661043898327,
9.15472388324137));
#197738=CARTESIAN_POINT('Ctrl Pts',(-16.7482515035196,18.4771679528309,
9.1540042293374));
#197739=CARTESIAN_POINT('Ctrl Pts',(-16.7468026116876,18.4811006197332,
9.15374938268126));
#197740=CARTESIAN_POINT('Ctrl Pts',(-16.7441435620844,18.4883845755958,
9.15327917737922));
#197741=CARTESIAN_POINT('Ctrl Pts',(-16.7429301961312,18.4917345889518,
9.15306363339954));
#197742=CARTESIAN_POINT('Ctrl Pts',(-16.7402140829829,18.4992931178714,
9.15257889885626));
#197743=CARTESIAN_POINT('Ctrl Pts',(-16.7387162044095,18.5035033251944,
9.15230999948717));
#197744=CARTESIAN_POINT('Ctrl Pts',(-16.7343571326063,18.5158796694874,
9.15152269448925));
#197745=CARTESIAN_POINT('Ctrl Pts',(-16.7315326211589,18.5240587554339,
9.15100641371015));
#197746=CARTESIAN_POINT('Ctrl Pts',(-16.712151895311,18.5813159653651,9.14741874754831));
#197747=CARTESIAN_POINT('Ctrl Pts',(-16.6973501207357,18.6309741794751,
9.14444287593275));
#197748=CARTESIAN_POINT('Ctrl Pts',(-16.679004293762,18.7019385099139,9.14031538506015));
#197749=CARTESIAN_POINT('Ctrl Pts',(-16.6739418011842,18.7228287039686,
9.13911544917261));
#197750=CARTESIAN_POINT('Ctrl Pts',(-16.6387809784156,18.8782204368672,
9.13027795592624));
#197751=CARTESIAN_POINT('Ctrl Pts',(-16.6215632619407,19.0152994916703,
9.12294767849478));
#197752=CARTESIAN_POINT('Ctrl Pts',(-16.6153091871384,19.2438168920291,
9.11034425721557));
#197753=CARTESIAN_POINT('Ctrl Pts',(-16.6186639937089,19.3346064462657,
9.10524191930659));
#197754=CARTESIAN_POINT('Ctrl Pts',(-16.6299381193021,19.4456200996201,
9.09874059515106));
#197755=CARTESIAN_POINT('Ctrl Pts',(-16.6323487084567,19.4663131254915,
9.09751773049638));
#197756=CARTESIAN_POINT('Ctrl Pts',(-16.6362262961191,19.4958051188765,
9.0957578566073));
#197757=CARTESIAN_POINT('Ctrl Pts',(-16.6374441697689,19.5046360254691,
9.09522870481878));
#197758=CARTESIAN_POINT('Ctrl Pts',(-16.6396477609538,19.5199013915578,
9.09431011127916));
#197759=CARTESIAN_POINT('Ctrl Pts',(-16.6406074540549,19.5263395281692,
9.09392149780407));
#197760=CARTESIAN_POINT('Ctrl Pts',(-16.6425065464657,19.538688811675,9.09317373918762));
#197761=CARTESIAN_POINT('Ctrl Pts',(-16.643441353199,19.5446006094361,9.09281474324452));
#197762=CARTESIAN_POINT('Ctrl Pts',(-16.6459483385153,19.5600305509882,
9.09187501990433));
#197763=CARTESIAN_POINT('Ctrl Pts',(-16.6475605171581,19.5695419726771,
9.0912930269693));
#197764=CARTESIAN_POINT('Ctrl Pts',(-16.6533405544899,19.6022828199195,
9.08928007747117));
#197765=CARTESIAN_POINT('Ctrl Pts',(-16.6578316888106,19.6254527068738,
9.08783889123328));
#197766=CARTESIAN_POINT('Ctrl Pts',(-16.6968550896355,19.8101865676598,
9.07621033483751));
#197767=CARTESIAN_POINT('Ctrl Pts',(-16.7497996744501,19.9672494842331,
9.06540847775969));
#197768=CARTESIAN_POINT('Ctrl Pts',(-16.8749459872598,20.2317073680745,
9.04607396881135));
#197769=CARTESIAN_POINT('Ctrl Pts',(-16.9397429627165,20.341740366408,9.0376463430569));
#197770=CARTESIAN_POINT('Ctrl Pts',(-17.0210404075602,20.4550266046997,
9.02899835365822));
#197771=CARTESIAN_POINT('Ctrl Pts',(-17.0281137779997,20.4647084874021,
9.02825964815667));
#197772=CARTESIAN_POINT('Ctrl Pts',(-17.0382747683764,20.4783714156561,
9.02721836220784));
#197773=CARTESIAN_POINT('Ctrl Pts',(-17.0412947758136,20.4824021360694,
9.02691131657579));
#197774=CARTESIAN_POINT('Ctrl Pts',(-17.0465196730008,20.4893240456284,
9.02638433797518));
#197775=CARTESIAN_POINT('Ctrl Pts',(-17.0487176698331,20.4922203901149,
9.02616392744933));
#197776=CARTESIAN_POINT('Ctrl Pts',(-17.0529903498914,20.4978205666287,
9.02573795867371));
#197777=CARTESIAN_POINT('Ctrl Pts',(-17.055064100227,20.5005250518273,9.02553233522139));
#197778=CARTESIAN_POINT('Ctrl Pts',(-17.0606692116394,20.5077985265467,
9.02497953393736));
#197779=CARTESIAN_POINT('Ctrl Pts',(-17.0642127810733,20.5123581332659,
9.02463321175031));
#197780=CARTESIAN_POINT('Ctrl Pts',(-17.0773898817796,20.5291710285477,
9.02335677304543));
#197781=CARTESIAN_POINT('Ctrl Pts',(-17.0871402614938,20.5413326568561,
9.02243459462963));
#197782=CARTESIAN_POINT('Ctrl Pts',(-17.1836996709749,20.6590822551381,
9.01350490219508));
#197783=CARTESIAN_POINT('Ctrl Pts',(-17.2804207792035,20.7561508504849,
9.00612147989973));
#197784=CARTESIAN_POINT('Ctrl Pts',(-17.5049797301052,20.9416288576053,
8.99030488527974));
#197785=CARTESIAN_POINT('Ctrl Pts',(-17.6345190125573,21.0266820112385,
8.98188548047938));
#197786=CARTESIAN_POINT('Ctrl Pts',(-17.791100556187,21.10654268022,8.9716490606345));
#197787=CARTESIAN_POINT('Ctrl Pts',(-17.8101924758871,21.1159202144791,
8.97040088994565));
#197788=CARTESIAN_POINT('Ctrl Pts',(-17.8375492478874,21.1288492786132,
8.96861095540869));
#197789=CARTESIAN_POINT('Ctrl Pts',(-17.8457008261013,21.1326384624313,
8.96807742739034));
#197790=CARTESIAN_POINT('Ctrl Pts',(-17.8598084692161,21.1390873198482,
8.96715366293316));
#197791=CARTESIAN_POINT('Ctrl Pts',(-17.8657531920121,21.1417716137348,
8.96676428058841));
#197792=CARTESIAN_POINT('Ctrl Pts',(-17.8771616963411,21.1468596932149,
8.96601674208702));
#197793=CARTESIAN_POINT('Ctrl Pts',(-17.8826234330424,21.1492679305329,
8.96565874328606));
#197794=CARTESIAN_POINT('Ctrl Pts',(-17.8968576550487,21.1554724380157,
8.96472538742464));
#197795=CARTESIAN_POINT('Ctrl Pts',(-17.9056457241828,21.1592324186198,
8.96414879816729));
#197796=CARTESIAN_POINT('Ctrl Pts',(-17.935727412096,21.1718625575481,8.96217377747856));
#197797=CARTESIAN_POINT('Ctrl Pts',(-17.9571398155571,21.1804439017053,
8.96076562643059));
#197798=CARTESIAN_POINT('Ctrl Pts',(-18.1416935738649,21.2509286223824,
8.94860483103081));
#197799=CARTESIAN_POINT('Ctrl Pts',(-18.3117420805782,21.2927806997673,
8.9371575300774));
#197800=CARTESIAN_POINT('Ctrl Pts',(-18.5720579469652,21.3236185719297,
8.91983713730217));
#197801=CARTESIAN_POINT('Ctrl Pts',(-18.6597239996754,21.3285144555854,
8.91405464175905));
#197802=CARTESIAN_POINT('Ctrl Pts',(-18.785444532426,21.3277159552842,8.90602656685559));
#197803=CARTESIAN_POINT('Ctrl Pts',(-18.8234328776712,21.3264515241592,
8.90363600516227));
#197804=CARTESIAN_POINT('Ctrl Pts',(-18.8689372378835,21.323708788634,8.90083072035237));
#197805=CARTESIAN_POINT('Ctrl Pts',(-18.8765029332506,21.3232119689433,
8.90036624367531));
#197806=CARTESIAN_POINT('Ctrl Pts',(-18.8882398338724,21.3223778873363,
8.89964886696501));
#197807=CARTESIAN_POINT('Ctrl Pts',(-18.8924128945056,21.3220688915901,
8.89939442779831));
#197808=CARTESIAN_POINT('Ctrl Pts',(-18.9001380735038,21.3214738423841,
8.89892460053718));
#197809=CARTESIAN_POINT('Ctrl Pts',(-18.9036903552748,21.3211911957173,
8.89870902950286));
#197810=CARTESIAN_POINT('Ctrl Pts',(-18.9117040921103,21.3205331948636,
8.89822376376608));
#197811=CARTESIAN_POINT('Ctrl Pts',(-18.9161650673336,21.3201526577454,
8.89795436311789));
#197812=CARTESIAN_POINT('Ctrl Pts',(-18.9292829712937,21.318991724684,8.89716422695986));
#197813=CARTESIAN_POINT('Ctrl Pts',(-18.9379364606908,21.3181721515048,
8.89664563929106));
#197814=CARTESIAN_POINT('Ctrl Pts',(-18.9990565093854,21.3120034199951,
8.89299996408863));
#197815=CARTESIAN_POINT('Ctrl Pts',(-19.0513167611672,21.3047481667129,
8.88997194202517));
#197816=CARTESIAN_POINT('Ctrl Pts',(-19.1187993044587,21.2927943406484,
8.88611580630671));
#197817=CARTESIAN_POINT('Ctrl Pts',(-19.1343118021733,21.2898671578818,
8.88523312987995));
#197818=CARTESIAN_POINT('Ctrl Pts',(-19.199642153134,21.2767810383419,8.8815263668416));
#197819=CARTESIAN_POINT('Ctrl Pts',(-19.2491197703036,21.265002405892,8.87874487264263));
#197820=CARTESIAN_POINT('Ctrl Pts',(-19.4035795705845,21.2222987070093,
8.87001965697419));
#197821=CARTESIAN_POINT('Ctrl Pts',(-19.5066125666359,21.1850132307558,
8.86412867689407));
#197822=CARTESIAN_POINT('Ctrl Pts',(-19.656577444329,21.1171964308693,8.85497762160709));
#197823=CARTESIAN_POINT('Ctrl Pts',(-19.7059453446942,21.0925035405958,
8.85186625349982));
#197824=CARTESIAN_POINT('Ctrl Pts',(-19.78437845965,21.0493615848196,8.84671643539947));
#197825=CARTESIAN_POINT('Ctrl Pts',(-19.814058467919,21.0320825719288,8.8447174897858));
#197826=CARTESIAN_POINT('Ctrl Pts',(-19.8525132503375,21.0084242741805,
8.84205474589328));
#197827=CARTESIAN_POINT('Ctrl Pts',(-19.8616788879715,21.0026880955267,
8.84141452329861));
#197828=CARTESIAN_POINT('Ctrl Pts',(-19.8766199767308,20.9931773718663,
8.84036155136416));
#197829=CARTESIAN_POINT('Ctrl Pts',(-19.8824217014148,20.9894443173751,
8.83995034483313));
#197830=CARTESIAN_POINT('Ctrl Pts',(-19.8936175176188,20.9821628663962,
8.8391522492247));
#197831=CARTESIAN_POINT('Ctrl Pts',(-19.8990138330768,20.9786180169302,
8.83876549586705));
#197832=CARTESIAN_POINT('Ctrl Pts',(-19.9114372720954,20.9703754343297,
8.83787025796834));
#197833=CARTESIAN_POINT('Ctrl Pts',(-19.9184526093742,20.965660212563,8.8373611179472));
#197834=CARTESIAN_POINT('Ctrl Pts',(-19.9372457763804,20.952864692812,8.83598734578536));
#197835=CARTESIAN_POINT('Ctrl Pts',(-19.9489702229855,20.9447071113675,
8.83511978913189));
#197836=CARTESIAN_POINT('Ctrl Pts',(-20.0755780769391,20.8547014682906,
8.82563481138858));
#197837=CARTESIAN_POINT('Ctrl Pts',(-20.1820673788121,20.7617010578141,
8.81656769436383));
#197838=CARTESIAN_POINT('Ctrl Pts',(-20.3445945741313,20.5883208222221,
8.80093331629477));
#197839=CARTESIAN_POINT('Ctrl Pts',(-20.4057792424103,20.5133754808729,
8.7945051455001));
#197840=CARTESIAN_POINT('Ctrl Pts',(-20.4993339082288,20.3812739366933,
8.78394200650054));
#197841=CARTESIAN_POINT('Ctrl Pts',(-20.5345602895933,20.3263157282221,
8.77974788110164));
#197842=CARTESIAN_POINT('Ctrl Pts',(-20.5737749596308,20.2584207312087,
8.77487643836234));
#197843=CARTESIAN_POINT('Ctrl Pts',(-20.5802489430024,20.2469666745198,
8.77406484960454));
#197844=CARTESIAN_POINT('Ctrl Pts',(-20.5891459478426,20.2308773685124,
8.77293985106746));
#197845=CARTESIAN_POINT('Ctrl Pts',(-20.5916590613372,20.2262926414462,
8.7726209663652));
#197846=CARTESIAN_POINT('Ctrl Pts',(-20.5959079048546,20.2184727944828,
8.77207999840212));
#197847=CARTESIAN_POINT('Ctrl Pts',(-20.5976522424459,20.2152423998883,
8.77185737102709));
#197848=CARTESIAN_POINT('Ctrl Pts',(-20.6009776731038,20.2090454238673,
8.77143194155917));
#197849=CARTESIAN_POINT('Ctrl Pts',(-20.6025601088368,20.2060796048557,
8.77122905136491));
#197850=CARTESIAN_POINT('Ctrl Pts',(-20.6067291659063,20.198220898131,8.77069330195796));
#197851=CARTESIAN_POINT('Ctrl Pts',(-20.6093036962946,20.1933215760522,
8.77036120535277));
#197852=CARTESIAN_POINT('Ctrl Pts',(-20.6183487943044,20.175943626707,8.76918977970356));
#197853=CARTESIAN_POINT('Ctrl Pts',(-20.6247144238561,20.1634104012543,
8.76835679554186));
#197854=CARTESIAN_POINT('Ctrl Pts',(-20.6654151976915,20.0812585002503,
8.76296778464621));
#197855=CARTESIAN_POINT('Ctrl Pts',(-20.6959972507266,20.0099135291362,
8.75861679153289));
#197856=CARTESIAN_POINT('Ctrl Pts',(-20.7225807266241,19.9371099735572,
8.75434675637709));
#197857=CARTESIAN_POINT('',(-20.8509999019989,19.2103558441126,9.29097300469246));
#197858=CARTESIAN_POINT('Ctrl Pts',(-20.7225805753213,19.9371103879265,
8.53521114927006));
#197859=CARTESIAN_POINT('Ctrl Pts',(-20.697266443062,20.0064375763663,8.5393535369811));
#197860=CARTESIAN_POINT('Ctrl Pts',(-20.6683301049202,20.0744322566373,
8.54338088181996));
#197861=CARTESIAN_POINT('Ctrl Pts',(-20.5622080177643,20.2914993392095,
8.55651379520119));
#197862=CARTESIAN_POINT('Ctrl Pts',(-20.4709008767018,20.432880427387,8.56556724285402));
#197863=CARTESIAN_POINT('Ctrl Pts',(-20.3488895873905,20.580076994319,8.57667163327324));
#197864=CARTESIAN_POINT('Ctrl Pts',(-20.3336077786475,20.5979012529915,
8.57804663419689));
#197865=CARTESIAN_POINT('Ctrl Pts',(-20.3116466052538,20.6226702379959,
8.58000263285212));
#197866=CARTESIAN_POINT('Ctrl Pts',(-20.3052111021477,20.6298295668434,
8.5805734762658));
#197867=CARTESIAN_POINT('Ctrl Pts',(-20.2946981104799,20.6413657526999,
8.58150235508359));
#197868=CARTESIAN_POINT('Ctrl Pts',(-20.2906504611549,20.6457697094684,
8.58185912434024));
#197869=CARTESIAN_POINT('Ctrl Pts',(-20.2821571010096,20.6549324779371,
8.58260599037739));
#197870=CARTESIAN_POINT('Ctrl Pts',(-20.2777079926067,20.6596880417603,
8.58299623058215));
#197871=CARTESIAN_POINT('Ctrl Pts',(-20.2671051411325,20.6709169147557,
8.58392392879231));
#197872=CARTESIAN_POINT('Ctrl Pts',(-20.2609322715509,20.6773719194094,
8.58446221059677));
#197873=CARTESIAN_POINT('Ctrl Pts',(-20.2401569293829,20.6988233858868,
8.58626796294337));
#197874=CARTESIAN_POINT('Ctrl Pts',(-20.2253732824973,20.7136419421783,
8.58754334280867));
#197875=CARTESIAN_POINT('Ctrl Pts',(-20.1447384681493,20.7921049169803,
8.5944510628809));
#197876=CARTESIAN_POINT('Ctrl Pts',(-20.0750377662661,20.8516369818007,
8.60025771159307));
#197877=CARTESIAN_POINT('Ctrl Pts',(-19.926079662512,20.9630139522418,8.61232145198565));
#197878=CARTESIAN_POINT('Ctrl Pts',(-19.8467534181857,21.0144369746358,
8.61857374253698));
#197879=CARTESIAN_POINT('Ctrl Pts',(-19.6994150782486,21.0965167257679,
8.62971096555022));
#197880=CARTESIAN_POINT('Ctrl Pts',(-19.6327063832409,21.1292094997095,
8.6345931002256));
#197881=CARTESIAN_POINT('Ctrl Pts',(-19.525553203944,21.1749036061143,8.64206180819788));
#197882=CARTESIAN_POINT('Ctrl Pts',(-19.4862011987982,21.1903099195942,
8.64472892160001));
#197883=CARTESIAN_POINT('Ctrl Pts',(-19.4393956551154,21.2070364423741,
8.64779180719334));
#197884=CARTESIAN_POINT('Ctrl Pts',(-19.4323664138277,21.2095066588165,
8.64824892665264));
#197885=CARTESIAN_POINT('Ctrl Pts',(-19.420970858578,21.2134438201632,8.64898519812854));
#197886=CARTESIAN_POINT('Ctrl Pts',(-19.416612612505,21.2149336904248,8.64926565607755));
#197887=CARTESIAN_POINT('Ctrl Pts',(-19.4088636481995,21.2175544676354,
8.64976226145896));
#197888=CARTESIAN_POINT('Ctrl Pts',(-19.405474898281,21.2186910212727,8.64997873911183));
#197889=CARTESIAN_POINT('Ctrl Pts',(-19.3981986884573,21.2211109075731,
8.65044205126195));
#197890=CARTESIAN_POINT('Ctrl Pts',(-19.3943103909334,21.2223915448691,
8.65068872632256));
#197891=CARTESIAN_POINT('Ctrl Pts',(-19.383604480465,21.2258832191108,8.6513654696876));
#197892=CARTESIAN_POINT('Ctrl Pts',(-19.3767792431543,21.2280709495722,
8.65179418719733));
#197893=CARTESIAN_POINT('Ctrl Pts',(-19.3399295084886,21.2396765602429,
8.6540948708341));
#197894=CARTESIAN_POINT('Ctrl Pts',(-19.3097072531193,21.2484593376342,
8.6559318753607));
#197895=CARTESIAN_POINT('Ctrl Pts',(-19.1212225145105,21.2987048423835,
8.66714524680859));
#197896=CARTESIAN_POINT('Ctrl Pts',(-18.9587779355933,21.3223834116316,
8.67579058385937));
#197897=CARTESIAN_POINT('Ctrl Pts',(-18.6781394172706,21.3305013979011,
8.6911590786924));
#197898=CARTESIAN_POINT('Ctrl Pts',(-18.5610028501522,21.3241666469738,
8.69769654112037));
#197899=CARTESIAN_POINT('Ctrl Pts',(-18.4308397135022,21.3062296178131,
8.70539395836518));
#197900=CARTESIAN_POINT('Ctrl Pts',(-18.4167001939912,21.3041350001508,
8.7062356886414));
#197901=CARTESIAN_POINT('Ctrl Pts',(-18.3942316654552,21.3005736358623,
8.70758255783291));
#197902=CARTESIAN_POINT('Ctrl Pts',(-18.3858882084579,21.2991998655002,
8.70808475354811));
#197903=CARTESIAN_POINT('Ctrl Pts',(-18.3711884695228,21.2966889716256,
8.70897324183996));
#197904=CARTESIAN_POINT('Ctrl Pts',(-18.364828704794,21.2955726771639,8.70935886802469));
#197905=CARTESIAN_POINT('Ctrl Pts',(-18.3516858572312,21.2932037544248,
8.71015836788225));
#197906=CARTESIAN_POINT('Ctrl Pts',(-18.3449035980984,21.2919470360817,
8.71057236772773));
#197907=CARTESIAN_POINT('Ctrl Pts',(-18.3275113943058,21.2886363499116,
8.71163773059789));
#197908=CARTESIAN_POINT('Ctrl Pts',(-18.3169109127072,21.2865342626689,
8.71229062230758));
#197909=CARTESIAN_POINT('Ctrl Pts',(-18.2727439655658,21.2774238885508,
8.71502605984439));
#197910=CARTESIAN_POINT('Ctrl Pts',(-18.2393357130508,21.2696820647382,
8.71713192371956));
#197911=CARTESIAN_POINT('Ctrl Pts',(-18.1527992335397,21.247400644919,8.72268620213861));
#197912=CARTESIAN_POINT('Ctrl Pts',(-18.1000269286452,21.2315937847153,
8.72617299869131));
#197913=CARTESIAN_POINT('Ctrl Pts',(-17.944468683369,21.1783054266116,8.73674197945718));
#197914=CARTESIAN_POINT('Ctrl Pts',(-17.843912389027,21.1348999245577,8.74397255635639));
#197915=CARTESIAN_POINT('Ctrl Pts',(-17.7067680854319,21.0626395000149,
8.75421258502946));
#197916=CARTESIAN_POINT('Ctrl Pts',(-17.6670667403258,21.040051080264,8.75722349561681));
#197917=CARTESIAN_POINT('Ctrl Pts',(-17.6086446024923,21.0042613295778,
8.7616987443569));
#197918=CARTESIAN_POINT('Ctrl Pts',(-17.5893569571793,20.9920118820241,
8.76318373530252));
#197919=CARTESIAN_POINT('Ctrl Pts',(-17.5696866576269,20.9790678521909,
8.76470338976718));
#197920=CARTESIAN_POINT('Ctrl Pts',(-17.5691025874667,20.9786830902211,
8.76474851762825));
#197921=CARTESIAN_POINT('Ctrl Pts',(-17.5591782945465,20.9721383097217,
8.76551539240275));
#197922=CARTESIAN_POINT('Ctrl Pts',(-17.5498867106956,20.9659045306252,
8.76623457765257));
#197923=CARTESIAN_POINT('Ctrl Pts',(-17.507398438208,20.9369078029994,8.76952734238311));
#197924=CARTESIAN_POINT('Ctrl Pts',(-17.4748033299085,20.9132729997179,
8.77206510497319));
#197925=CARTESIAN_POINT('Ctrl Pts',(-17.4370801352088,20.8842428960584,
8.77499764394009));
#197926=CARTESIAN_POINT('Ctrl Pts',(-17.4312837722089,20.8797340586053,
8.77544811122722));
#197927=CARTESIAN_POINT('Ctrl Pts',(-17.4219156215332,20.872368261596,8.77617578407163));
#197928=CARTESIAN_POINT('Ctrl Pts',(-17.4183294818204,20.8695297722246,
8.77645424746876));
#197929=CARTESIAN_POINT('Ctrl Pts',(-17.4119596097382,20.864454250754,8.77694866223357));
#197930=CARTESIAN_POINT('Ctrl Pts',(-17.4091723176459,20.8622217796344,
8.77716493276392));
#197931=CARTESIAN_POINT('Ctrl Pts',(-17.4031854246193,20.8574016819738,
8.77762930085621));
#197932=CARTESIAN_POINT('Ctrl Pts',(-17.3999877246197,20.8548117843139,
8.77787723108875));
#197933=CARTESIAN_POINT('Ctrl Pts',(-17.3911665577945,20.8476246069269,
8.77856096723779));
#197934=CARTESIAN_POINT('Ctrl Pts',(-17.3855591068744,20.8430076343961,
8.77899537564996));
#197935=CARTESIAN_POINT('Ctrl Pts',(-17.3547167627444,20.8173456758358,
8.7813841566111));
#197936=CARTESIAN_POINT('Ctrl Pts',(-17.3299492133875,20.7957429876211,
8.78330032437692));
#197937=CARTESIAN_POINT('Ctrl Pts',(-17.1858166763207,20.6639950709991,
8.79450824017));
#197938=CARTESIAN_POINT('Ctrl Pts',(-17.0789354462819,20.5409771900929,
8.80309316148495));
#197939=CARTESIAN_POINT('Ctrl Pts',(-16.9212132977192,20.3106014038456,
8.81837806893171));
#197940=CARTESIAN_POINT('Ctrl Pts',(-16.8633508000439,20.2089905778889,
8.82489580739017));
#197941=CARTESIAN_POINT('Ctrl Pts',(-16.8081397131977,20.0901787794864,
8.83257102198007));
#197942=CARTESIAN_POINT('Ctrl Pts',(-16.8022496382064,20.0771603173696,
8.83341246760097));
#197943=CARTESIAN_POINT('Ctrl Pts',(-16.7930850546525,20.0563458769969,
8.83475896639015));
#197944=CARTESIAN_POINT('Ctrl Pts',(-16.7897246222875,20.0485880427077,
8.83526107892037));
#197945=CARTESIAN_POINT('Ctrl Pts',(-16.7838798922056,20.0348702902614,
8.83614947031357));
#197946=CARTESIAN_POINT('Ctrl Pts',(-16.7813762090455,20.0289187120811,
8.83653508325107));
#197947=CARTESIAN_POINT('Ctrl Pts',(-16.7762540305768,20.0165850705351,
8.83733460501504));
#197948=CARTESIAN_POINT('Ctrl Pts',(-16.7736394274112,20.0102014829498,
8.83774864025748));
#197949=CARTESIAN_POINT('Ctrl Pts',(-16.7670079847104,19.9937823820435,
8.83881419820976));
#197950=CARTESIAN_POINT('Ctrl Pts',(-16.7630367604073,19.9837287669281,
8.83946725068541));
#197951=CARTESIAN_POINT('Ctrl Pts',(-16.7467815462405,19.941636163221,8.84220424622047));
#197952=CARTESIAN_POINT('Ctrl Pts',(-16.735200988927,19.9093327880421,8.84431154056221));
#197953=CARTESIAN_POINT('Ctrl Pts',(-16.7070758831044,19.8244379469762,
8.84987049159078));
#197954=CARTESIAN_POINT('Ctrl Pts',(-16.6917922885381,19.7714590369049,
8.85336061084803));
#197955=CARTESIAN_POINT('Ctrl Pts',(-16.6523943002885,19.6117209069783,
8.86393597418552));
#197956=CARTESIAN_POINT('Ctrl Pts',(-16.6344706181297,19.5036302164386,
8.8711695896824));
#197957=CARTESIAN_POINT('Ctrl Pts',(-16.6206897590714,19.3453708529905,
8.88166329541942));
#197958=CARTESIAN_POINT('Ctrl Pts',(-16.6181270523272,19.2959566120396,
8.88492412782601));
#197959=CARTESIAN_POINT('Ctrl Pts',(-16.6170179167089,19.2298180558959,
8.88923735167777));
#197960=CARTESIAN_POINT('Ctrl Pts',(-16.6169353534846,19.2131362265077,
8.89032085944812));
#197961=CARTESIAN_POINT('Ctrl Pts',(-16.6174160277454,19.1431772098436,
8.8948421801714));
#197962=CARTESIAN_POINT('Ctrl Pts',(-16.6197932752915,19.0899272909105,
8.89822896713506));
#197963=CARTESIAN_POINT('Ctrl Pts',(-16.6248948323449,19.0281329449414,
8.90205384845788));
#197964=CARTESIAN_POINT('Ctrl Pts',(-16.6256656088748,19.019450869866,8.90258880433776));
#197965=CARTESIAN_POINT('Ctrl Pts',(-16.6269139357158,19.0063114350199,
8.90339445884502));
#197966=CARTESIAN_POINT('Ctrl Pts',(-16.6273520469587,19.0018505468898,
8.9036672919615));
#197967=CARTESIAN_POINT('Ctrl Pts',(-16.6281639264406,18.9938453722729,
8.90415561825538));
#197968=CARTESIAN_POINT('Ctrl Pts',(-16.6285324777938,18.9903006240027,
8.9043713992682));
#197969=CARTESIAN_POINT('Ctrl Pts',(-16.6293528007749,18.9825998185874,
8.90483918419298));
#197970=CARTESIAN_POINT('Ctrl Pts',(-16.6298079303377,18.9784441771552,
8.90509099685626));
#197971=CARTESIAN_POINT('Ctrl Pts',(-16.6311210653119,18.9667738933941,
8.90579648380971));
#197972=CARTESIAN_POINT('Ctrl Pts',(-16.6320070464334,18.9592623743418,
8.9062486107759));
#197973=CARTESIAN_POINT('Ctrl Pts',(-16.6375471916381,18.9143618234692,
8.90894037907243));
#197974=CARTESIAN_POINT('Ctrl Pts',(-16.6431588843496,18.877095208706,8.91112949011558));
#197975=CARTESIAN_POINT('Ctrl Pts',(-16.6649107936157,18.7548967700036,
8.91821704310322));
#197976=CARTESIAN_POINT('Ctrl Pts',(-16.6852577460059,18.6707983339279,
8.92295149499236));
#197977=CARTESIAN_POINT('Ctrl Pts',(-16.7625567222436,18.4196853984783,
8.93724930263314));
#197978=CARTESIAN_POINT('Ctrl Pts',(-16.8352561405136,18.2583550030579,
8.94672307059035));
#197979=CARTESIAN_POINT('Ctrl Pts',(-16.9390550078285,18.088330232005,8.95829925095575));
#197980=CARTESIAN_POINT('Ctrl Pts',(-16.9513216341481,18.0689524018888,
8.95964285881243));
#197981=CARTESIAN_POINT('Ctrl Pts',(-16.969131358301,18.0418042828294,8.96156167622395));
#197982=CARTESIAN_POINT('Ctrl Pts',(-16.9744161734379,18.0338658953712,
8.96212725255675));
#197983=CARTESIAN_POINT('Ctrl Pts',(-16.9830934919021,18.0210205956828,
8.96304988220527));
#197984=CARTESIAN_POINT('Ctrl Pts',(-16.9864534535734,18.016091781872,8.9634057032543));
#197985=CARTESIAN_POINT('Ctrl Pts',(-16.9935329185366,18.0058004608563,
8.96415247412125));
#197986=CARTESIAN_POINT('Ctrl Pts',(-16.9972564722743,18.0004408282812,
8.96454357572377));
#197987=CARTESIAN_POINT('Ctrl Pts',(-17.0061786955254,17.9877241967286,
8.96547680424103));
#197988=CARTESIAN_POINT('Ctrl Pts',(-17.0113996273458,17.9803830395787,
8.96601978149938));
#197989=CARTESIAN_POINT('Ctrl Pts',(-17.0291710971178,17.9557292513476,
8.96785776217277));
#197990=CARTESIAN_POINT('Ctrl Pts',(-17.0419367201608,17.9385739530716,
8.96916106564162));
#197991=CARTESIAN_POINT('Ctrl Pts',(-17.1130192831018,17.8460100314751,
8.97632986409577));
#197992=CARTESIAN_POINT('Ctrl Pts',(-17.1761113462918,17.7744225395055,
8.9823847662244));
#197993=CARTESIAN_POINT('Ctrl Pts',(-17.3649871583612,17.5872384093068,
8.99966511063359));
#197994=CARTESIAN_POINT('Ctrl Pts',(-17.500235715532,17.4822373117944,9.01117699066875));
#197995=CARTESIAN_POINT('Ctrl Pts',(-17.6780757781581,17.3757731528818,
9.02440467292287));
#197996=CARTESIAN_POINT('Ctrl Pts',(-17.7100233243319,17.3577580611091,
9.02671101795702));
#197997=CARTESIAN_POINT('Ctrl Pts',(-17.7487283094343,17.3372391839079,
9.0294086543798));
#197998=CARTESIAN_POINT('Ctrl Pts',(-17.7550487046079,17.3339293394465,
9.02984615095221));
#197999=CARTESIAN_POINT('Ctrl Pts',(-17.7653917042542,17.3285794014119,
9.03055702819858));
#198000=CARTESIAN_POINT('Ctrl Pts',(-17.7694042494542,17.3265201302546,
9.03083157517174));
#198001=CARTESIAN_POINT('Ctrl Pts',(-17.7766009793685,17.3228557178617,
9.03132173881997));
#198002=CARTESIAN_POINT('Ctrl Pts',(-17.7797826548772,17.3212457901225,
9.03153765288808));
#198003=CARTESIAN_POINT('Ctrl Pts',(-17.7866846432542,17.3177752598759,
9.03200432479047));
#198004=CARTESIAN_POINT('Ctrl Pts',(-17.7904063647455,17.3159175865058,
9.03225489893297));
#198005=CARTESIAN_POINT('Ctrl Pts',(-17.8008246586814,17.3107556621284,
9.0329534257104));
#198006=CARTESIAN_POINT('Ctrl Pts',(-17.8075333504167,17.3074758177955,
9.03339987971469));
#198007=CARTESIAN_POINT('Ctrl Pts',(-17.8467272179401,17.2885704330329,
9.03598950609465));
#198008=CARTESIAN_POINT('Ctrl Pts',(-17.879591988789,17.2737401492536,9.03808650695643));
#198009=CARTESIAN_POINT('Ctrl Pts',(-17.9867534853252,17.2286413910437,
9.04473680285233));
#198010=CARTESIAN_POINT('Ctrl Pts',(-18.0624000274753,17.2017517584273,
9.04914838643406));
#198011=CARTESIAN_POINT('Ctrl Pts',(-18.3174041456543,17.1271243204877,
9.06363240847603));
#198012=CARTESIAN_POINT('Ctrl Pts',(-18.5014653802449,17.0986525905144,
9.07355317091278));
#198013=CARTESIAN_POINT('Ctrl Pts',(-18.7089948933894,17.0940320884639,
9.08562592997281));
#198014=CARTESIAN_POINT('Ctrl Pts',(-18.7311173724334,17.0938863918305,
9.08692273217236));
#198015=CARTESIAN_POINT('Ctrl Pts',(-18.7616984633517,17.0941642979843,
9.08873050711022));
#198016=CARTESIAN_POINT('Ctrl Pts',(-18.7701588174278,17.0942919117261,
9.08923223288706));
#198017=CARTESIAN_POINT('Ctrl Pts',(-18.7846953954136,17.0945983540511,
9.09009713397423));
#198018=CARTESIAN_POINT('Ctrl Pts',(-18.7907720744447,17.0947526419464,
9.09045953758247));
#198019=CARTESIAN_POINT('Ctrl Pts',(-18.8032939124053,17.0951245450867,
9.09120811123557));
#198020=CARTESIAN_POINT('Ctrl Pts',(-18.8097389038583,17.0953454431273,
9.09159438038085));
#198021=CARTESIAN_POINT('Ctrl Pts',(-18.8247274460454,17.0959277428672,
9.09249501089743));
#198022=CARTESIAN_POINT('Ctrl Pts',(-18.8332699718761,17.0963114669789,
9.09301006703614));
#198023=CARTESIAN_POINT('Ctrl Pts',(-18.8605757342882,17.0977038404696,
9.09466214790892));
#198024=CARTESIAN_POINT('Ctrl Pts',(-18.879327559702,17.0989105276866,9.09580535420733));
#198025=CARTESIAN_POINT('Ctrl Pts',(-18.9727481865047,17.1061721504019,
9.10154549134328));
#198026=CARTESIAN_POINT('Ctrl Pts',(-19.0470671003556,17.1159372733713,
9.10625747982172));
#198027=CARTESIAN_POINT('Ctrl Pts',(-19.2277700331182,17.1495105884135,
9.11806559652373));
#198028=CARTESIAN_POINT('Ctrl Pts',(-19.333132455298,17.1776322855539,9.12526207470022));
#198029=CARTESIAN_POINT('Ctrl Pts',(-19.5489466401678,17.2534709350268,
9.14037430552462));
#198030=CARTESIAN_POINT('Ctrl Pts',(-19.6584722050729,17.3027505745684,
9.14826221120722));
#198031=CARTESIAN_POINT('Ctrl Pts',(-19.7715535833672,17.3656648203867,
9.15625475703304));
#198032=CARTESIAN_POINT('Ctrl Pts',(-19.7798294055048,17.3703424474378,
9.15683869334073));
#198033=CARTESIAN_POINT('Ctrl Pts',(-19.7920477901601,17.3773574846551,
9.15769901278247));
#198034=CARTESIAN_POINT('Ctrl Pts',(-19.7960145901564,17.3796521325673,
9.15797803905649));
#198035=CARTESIAN_POINT('Ctrl Pts',(-19.8029605202583,17.3837002557399,
9.15846607718493));
#198036=CARTESIAN_POINT('Ctrl Pts',(-19.8059428341996,17.3854481628643,
9.15867544418998));
#198037=CARTESIAN_POINT('Ctrl Pts',(-19.8123456343186,17.3892218862082,
9.15912454741573));
#198038=CARTESIAN_POINT('Ctrl Pts',(-19.8157646904125,17.3912500286798,
9.15936412924731));
#198039=CARTESIAN_POINT('Ctrl Pts',(-19.8228158807722,17.3954596043279,
9.15985777752131));
#198040=CARTESIAN_POINT('Ctrl Pts',(-19.8264472234304,17.3976423366422,
9.16011175914375));
#198041=CARTESIAN_POINT('Ctrl Pts',(-19.8355735642533,17.4031653741656,
9.16074951296143));
#198042=CARTESIAN_POINT('Ctrl Pts',(-19.8410599837193,17.4065198680463,
9.16113239711954));
#198043=CARTESIAN_POINT('Ctrl Pts',(-19.8566518707262,17.4161509008407,
9.16221931258732));
#198044=CARTESIAN_POINT('Ctrl Pts',(-19.8667200032386,17.4224877916183,
9.16291971426939));
#198045=CARTESIAN_POINT('Ctrl Pts',(-19.9004526476336,17.44411825938,9.16526333451959));
#198046=CARTESIAN_POINT('Ctrl Pts',(-19.9238660135968,17.4597998731897,
9.16688494411293));
#198047=CARTESIAN_POINT('Ctrl Pts',(-20.1096085667809,17.5896507172134,
9.17976728332988));
#198048=CARTESIAN_POINT('Ctrl Pts',(-20.2554714790839,17.7256674728927,
9.19008536896605));
#198049=CARTESIAN_POINT('Ctrl Pts',(-20.4259994360632,17.9365909473618,
9.20524794634643));
#198050=CARTESIAN_POINT('Ctrl Pts',(-20.4687833597732,17.9954731225062,
9.20939667530289));
#198051=CARTESIAN_POINT('Ctrl Pts',(-20.5155582447735,18.0673614571342,
9.21442962601142));
#198052=CARTESIAN_POINT('Ctrl Pts',(-20.5225657501326,18.0783520218739,
9.21519815903774));
#198053=CARTESIAN_POINT('Ctrl Pts',(-20.533800983204,18.0963376253222,9.21645467177886));
#198054=CARTESIAN_POINT('Ctrl Pts',(-20.5380905460369,18.1032937720209,
9.21694036383617));
#198055=CARTESIAN_POINT('Ctrl Pts',(-20.5456657214597,18.1157387370824,
9.21780887901529));
#198056=CARTESIAN_POINT('Ctrl Pts',(-20.5489669522373,18.1212179661699,
9.21819112311947));
#198057=CARTESIAN_POINT('Ctrl Pts',(-20.5558791164178,18.1328089791901,
9.21899947937157));
#198058=CARTESIAN_POINT('Ctrl Pts',(-20.5594842373245,18.1389241213593,
9.21942579725972));
#198059=CARTESIAN_POINT('Ctrl Pts',(-20.568957764628,18.1551798116322,9.22055872609264));
#198060=CARTESIAN_POINT('Ctrl Pts',(-20.5747728000763,18.1653510350095,
9.22126725643068));
#198061=CARTESIAN_POINT('Ctrl Pts',(-20.601608681013,18.2132079908139,9.22459978666674));
#198062=CARTESIAN_POINT('Ctrl Pts',(-20.6215572963592,18.2514802743453,
9.22726173152773));
#198063=CARTESIAN_POINT('Ctrl Pts',(-20.6735197136441,18.3590730335041,
9.2347418326464));
#198064=CARTESIAN_POINT('Ctrl Pts',(-20.7029724481655,18.4295514923801,
9.23964015626457));
#198065=CARTESIAN_POINT('Ctrl Pts',(-20.7868720819469,18.6653977969546,
9.25596369974907));
#198066=CARTESIAN_POINT('Ctrl Pts',(-20.8247559190743,18.8358935776873,
9.26771398111092));
#198067=CARTESIAN_POINT('Ctrl Pts',(-20.8438467744343,19.0351570450412,
9.28035994964475));
#198068=CARTESIAN_POINT('Ctrl Pts',(-20.8458598063493,19.0612586913657,
9.28199395121779));
#198069=CARTESIAN_POINT('Ctrl Pts',(-20.8477953023107,19.0943509189102,
9.28403153909177));
#198070=CARTESIAN_POINT('Ctrl Pts',(-20.8481679339001,19.101311629713,9.28445822647419));
#198071=CARTESIAN_POINT('Ctrl Pts',(-20.8487046766269,19.1123599294185,
9.28513232332365));
#198072=CARTESIAN_POINT('Ctrl Pts',(-20.8488913285337,19.1164463008669,
9.28538096266836));
#198073=CARTESIAN_POINT('Ctrl Pts',(-20.8492163340703,19.1240447614429,
9.28584199273702));
#198074=CARTESIAN_POINT('Ctrl Pts',(-20.8493577841925,19.1275566150248,
9.28605454922297));
#198075=CARTESIAN_POINT('Ctrl Pts',(-20.8496218268837,19.1345448797432,
9.28647649266277));
#198076=CARTESIAN_POINT('Ctrl Pts',(-20.8497445966673,19.138021223141,9.28668588806037));
#198077=CARTESIAN_POINT('Ctrl Pts',(-20.8500062528851,19.1459868452829,
9.28716457379975));
#198078=CARTESIAN_POINT('Ctrl Pts',(-20.8501394227778,19.1504763126595,
9.28743354980515));
#198079=CARTESIAN_POINT('Ctrl Pts',(-20.8504746952607,19.1631387302945,
9.28818997906115));
#198080=CARTESIAN_POINT('Ctrl Pts',(-20.8506437465519,19.1713125745779,
9.28867567321112));
#198081=CARTESIAN_POINT('Ctrl Pts',(-20.850918614115,19.1897759511114,9.28976732408507));
#198082=CARTESIAN_POINT('Ctrl Pts',(-20.8509967709457,19.2000657272674,
9.29037188547692));
#198083=CARTESIAN_POINT('Ctrl Pts',(-20.8509999019989,19.2103558441126,
9.29097300469246));
#198084=CARTESIAN_POINT('Ctrl Pts',(-20.8509999014157,19.2103539304217,
9.29097289290007));
#198085=CARTESIAN_POINT('Ctrl Pts',(-20.8510612394758,19.4113426033819,
9.30271408510573));
#198086=CARTESIAN_POINT('Ctrl Pts',(-20.8225007204989,19.6113597274272,
9.31315832230768));
#198087=CARTESIAN_POINT('Ctrl Pts',(-20.7530794884102,19.8491047828837,
9.32683241854603));
#198088=CARTESIAN_POINT('Ctrl Pts',(-20.7385514545259,19.8933713334306,
9.32943048944104));
#198089=CARTESIAN_POINT('Ctrl Pts',(-20.7225805876262,19.9371103542273,
9.33206810105871));
#198090=CARTESIAN_POINT('Origin',(-18.734,19.211,0.));
#198091=CARTESIAN_POINT('',(-20.7225806064498,19.9371103026755,10.3555828687981));
#198092=CARTESIAN_POINT('',(-20.7225805927058,19.9371103403161,10.1325349747556));
#198093=CARTESIAN_POINT('',(-20.7225806064498,19.9371103026755,0.));
#198094=CARTESIAN_POINT('',(-20.8533536084667,19.2099228989533,10.3109437268627));
#198095=CARTESIAN_POINT('Ctrl Pts',(-20.8509997268492,19.2099245835976,
10.3109437563769));
#198096=CARTESIAN_POINT('Ctrl Pts',(-20.8510361522909,19.2816295063777,
10.3152783077138));
#198097=CARTESIAN_POINT('Ctrl Pts',(-20.8474252680846,19.3534823809604,
10.3196128590508));
#198098=CARTESIAN_POINT('Ctrl Pts',(-20.8401482596367,19.4250759407999,
10.3239474103877));
#198099=CARTESIAN_POINT('Ctrl Pts',(-20.8328800282355,19.496583149219,10.3282767336752));
#198100=CARTESIAN_POINT('Ctrl Pts',(-20.8219544852716,19.5678311749355,
10.3326060569628));
#198101=CARTESIAN_POINT('Ctrl Pts',(-20.8074048164028,19.6384125259253,
10.3369353802504));
#198102=CARTESIAN_POINT('Ctrl Pts',(-20.7928691087884,19.7089261499988,
10.3412605493001));
#198103=CARTESIAN_POINT('Ctrl Pts',(-20.774716275487,19.7787738864939,10.3455857183499));
#198104=CARTESIAN_POINT('Ctrl Pts',(-20.7530311027341,19.8475551085275,
10.3499108873996));
#198105=CARTESIAN_POINT('Ctrl Pts',(-20.7435518665807,19.8776214332925,
10.3518015478658));
#198106=CARTESIAN_POINT('Ctrl Pts',(-20.7333983238929,19.9074840833062,
10.353692208332));
#198107=CARTESIAN_POINT('Ctrl Pts',(-20.7225806064498,19.9371103026755,
10.3555828687981));
#198108=CARTESIAN_POINT('Ctrl Pts',(-20.7242505210392,19.9377358132316,
9.55561791545399));
#198109=CARTESIAN_POINT('Ctrl Pts',(-20.5136267421919,20.4984180581842,
9.59172752760294));
#198110=CARTESIAN_POINT('Ctrl Pts',(-19.5197099108043,21.5302730444029,
9.67022907531242));
#198111=CARTESIAN_POINT('Ctrl Pts',(-17.2597752658646,21.2341144066335,
9.79112255858229));
#198112=CARTESIAN_POINT('Ctrl Pts',(-16.2349110611132,19.0664837566254,
9.91829836526376));
#198113=CARTESIAN_POINT('Ctrl Pts',(-17.5028058468379,17.0314377902239,
10.0454741719452));
#198114=CARTESIAN_POINT('Ctrl Pts',(-19.9002448515612,16.9960048724045,
10.1726499786266));
#198115=CARTESIAN_POINT('Ctrl Pts',(-20.8239162838523,18.3853146252952,
10.2611398283041));
#198116=CARTESIAN_POINT('Ctrl Pts',(-20.8542040821902,19.1485339254976,
10.307237742421));
#198117=CARTESIAN_POINT('Ctrl Pts',(-20.853822977789,19.2099225630314,10.3109437209775));
#198118=CARTESIAN_POINT('Ctrl Pts',(-20.7225805876262,19.9371103542273,
9.33206810105871));
#198119=CARTESIAN_POINT('Ctrl Pts',(-20.7083723124747,19.9760222083078,
9.33441461811644));
#198120=CARTESIAN_POINT('Ctrl Pts',(-20.6930221015738,20.0145165505172,
9.33679237043968));
#198121=CARTESIAN_POINT('Ctrl Pts',(-20.6684009468031,20.0713499495902,
9.3404023341193));
#198122=CARTESIAN_POINT('Ctrl Pts',(-20.6599812476126,20.0900365459304,
9.34160569950588));
#198123=CARTESIAN_POINT('Ctrl Pts',(-20.6475367889476,20.1166182362245,
9.34334237469629));
#198124=CARTESIAN_POINT('Ctrl Pts',(-20.6437315509185,20.1246152539405,
9.34386811257265));
#198125=CARTESIAN_POINT('Ctrl Pts',(-20.6370470770801,20.1384389791352,
9.34478268475076));
#198126=CARTESIAN_POINT('Ctrl Pts',(-20.6341909611294,20.1442767796274,
9.34517071080896));
#198127=CARTESIAN_POINT('Ctrl Pts',(-20.6286470866176,20.155477315503,9.34591869353401));
#198128=CARTESIAN_POINT('Ctrl Pts',(-20.6259633238204,20.1608419671164,
9.34627850748558));
#198129=CARTESIAN_POINT('Ctrl Pts',(-20.6188715784058,20.1748685554156,
9.34722341538004));
#198130=CARTESIAN_POINT('Ctrl Pts',(-20.6144267200328,20.1835115962596,
9.34780980218194));
#198131=CARTESIAN_POINT('Ctrl Pts',(-20.5987863506719,20.2134162090647,
9.34985330554818));
#198132=CARTESIAN_POINT('Ctrl Pts',(-20.587288806225,20.2345169348483,9.35132107029404));
#198133=CARTESIAN_POINT('Ctrl Pts',(-20.503433765002,20.3823636704645,9.36179375158657));
#198134=CARTESIAN_POINT('Ctrl Pts',(-20.4185109819538,20.5015028249208,
9.37126617387904));
#198135=CARTESIAN_POINT('Ctrl Pts',(-20.2315226373376,20.7136136358815,
9.38992783241288));
#198136=CARTESIAN_POINT('Ctrl Pts',(-20.1312641727334,20.8072707252901,
9.39904492515672));
#198137=CARTESIAN_POINT('Ctrl Pts',(-20.0125804369365,20.8983299731808,
9.4084127902312));
#198138=CARTESIAN_POINT('Ctrl Pts',(-20.0024322113572,20.9059720098676,
9.40920324599229));
#198139=CARTESIAN_POINT('Ctrl Pts',(-19.9867977229504,20.9175263694816,
9.41040421042433));
#198140=CARTESIAN_POINT('Ctrl Pts',(-19.9813607329896,20.9215044837379,
9.41081878247207));
#198141=CARTESIAN_POINT('Ctrl Pts',(-19.9723708079735,20.9280165357094,
9.41149909799248));
#198142=CARTESIAN_POINT('Ctrl Pts',(-19.9688289086725,20.9305655291434,
9.41176582084513));
#198143=CARTESIAN_POINT('Ctrl Pts',(-19.9619672203779,20.9354715368968,
9.41227997022959));
#198144=CARTESIAN_POINT('Ctrl Pts',(-19.9586484668834,20.9378299595197,
9.4125274910382));
#198145=CARTESIAN_POINT('Ctrl Pts',(-19.9553132045175,20.9401856628517,
9.41277506997446));
#198146=CARTESIAN_POINT('Ctrl Pts',(-19.95530351068,20.9401925095089,9.41277578954511));
#198147=CARTESIAN_POINT('Ctrl Pts',(-19.9552840886592,20.9402062268364,
9.41277723121601));
#198148=CARTESIAN_POINT('Ctrl Pts',(-19.9552743605407,20.9402130974602,
9.41277795331139));
#198149=CARTESIAN_POINT('Ctrl Pts',(-19.9552548697881,20.9402268628383,
9.41277940004412));
#198150=CARTESIAN_POINT('Ctrl Pts',(-19.9552451069065,20.9402337577667,
9.41278012469979));
#198151=CARTESIAN_POINT('Ctrl Pts',(-19.9552249130926,20.9402480191705,
9.41278162357678));
#198152=CARTESIAN_POINT('Ctrl Pts',(-19.9552144826606,20.9402553852751,
9.41278239775954));
#198153=CARTESIAN_POINT('Ctrl Pts',(-19.9551934538178,20.9402702358281,
9.41278395856987));
#198154=CARTESIAN_POINT('Ctrl Pts',(-19.9551828549229,20.9402777206137,
9.41278474523301));
#198155=CARTESIAN_POINT('Ctrl Pts',(-19.9551614854613,20.9402928111225,
9.41278633127706));
#198156=CARTESIAN_POINT('Ctrl Pts',(-19.9551507150833,20.9403004167077,
9.41278713064358));
#198157=CARTESIAN_POINT('Ctrl Pts',(-19.9551289992166,20.9403157512299,
9.41278874234848));
#198158=CARTESIAN_POINT('Ctrl Pts',(-19.9551180532273,20.9403234805154,
9.41278955472362));
#198159=CARTESIAN_POINT('Ctrl Pts',(-19.9550959816806,20.9403390655707,
9.41279119277532));
#198160=CARTESIAN_POINT('Ctrl Pts',(-19.9550848569857,20.9403469207263,
9.41279201838747));
#198161=CARTESIAN_POINT('Ctrl Pts',(-19.9550624244507,20.9403627600322,
9.41279368317742));
#198162=CARTESIAN_POINT('Ctrl Pts',(-19.9550511163289,20.940370744376,9.41279452237571));
#198163=CARTESIAN_POINT('Ctrl Pts',(-19.9550283129778,20.9403868448397,
9.41279621463067));
#198164=CARTESIAN_POINT('Ctrl Pts',(-19.9550168179877,20.9403949607852,
9.41279706766915));
#198165=CARTESIAN_POINT('Ctrl Pts',(-19.9549936369887,20.9404113271972,
9.41279878789342));
#198166=CARTESIAN_POINT('Ctrl Pts',(-19.9549819506578,20.9404195778851,
9.41279965510262));
#198167=CARTESIAN_POINT('Ctrl Pts',(-19.9549583829434,20.9404362166127,
9.41280140396625));
#198168=CARTESIAN_POINT('Ctrl Pts',(-19.9549465012232,20.940444604884,9.41280228564519));
#198169=CARTESIAN_POINT('Ctrl Pts',(-19.9549225377146,20.9404615223009,
9.41280406381898));
#198170=CARTESIAN_POINT('Ctrl Pts',(-19.9549104565878,20.9404700509732,
9.41280496026424));
#198171=CARTESIAN_POINT('Ctrl Pts',(-19.9548860899369,20.9404872522296,
9.41280676829041));
#198172=CARTESIAN_POINT('Ctrl Pts',(-19.9548738043449,20.9404959248551,
9.41280767987582));
#198173=CARTESIAN_POINT('Ctrl Pts',(-19.9548490244136,20.9405134170692,
9.41280951850347));
#198174=CARTESIAN_POINT('Ctrl Pts',(-19.9548365299727,20.9405222367226,
9.4128104455527));
#198175=CARTESIAN_POINT('Ctrl Pts',(-19.9548113274381,20.940540026435,9.41281231547029));
#198176=CARTESIAN_POINT('Ctrl Pts',(-19.9547986194878,20.9405489963856,
9.41281325832745));
#198177=CARTESIAN_POINT('Ctrl Pts',(-19.9547729853794,20.9405670898864,
9.41281516019715));
#198178=CARTESIAN_POINT('Ctrl Pts',(-19.9547600587298,20.9405762137762,
9.41281611924557));
#198179=CARTESIAN_POINT('Ctrl Pts',(-19.9547339820759,20.940594618766,9.41281805387785));
#198180=CARTESIAN_POINT('Ctrl Pts',(-19.9547208320502,20.9406038998735,
9.41281902946268));
#198181=CARTESIAN_POINT('Ctrl Pts',(-19.9518702664365,20.9426157412384,
9.41303050559343));
#198182=CARTESIAN_POINT('Ctrl Pts',(-19.9490279680172,20.9446112881187,
9.41324051485031));
#198183=CARTESIAN_POINT('Ctrl Pts',(-19.9424087524699,20.949234292255,9.41372762670196));
#198184=CARTESIAN_POINT('Ctrl Pts',(-19.9386281761675,20.9518564346082,
9.41400436526241));
#198185=CARTESIAN_POINT('Ctrl Pts',(-19.9269336087204,20.9599112467264,
9.41485596276838));
#198186=CARTESIAN_POINT('Ctrl Pts',(-19.9189910658487,20.9653025182226,
9.41542808190676));
#198187=CARTESIAN_POINT('Ctrl Pts',(-19.8165021515012,21.0338567104904,
9.42273437345601));
#198188=CARTESIAN_POINT('Ctrl Pts',(-19.717038601259,21.0893662932825,9.42900134393215));
#198189=CARTESIAN_POINT('Ctrl Pts',(-19.5099110397039,21.1839779160608,
9.44141177246223));
#198190=CARTESIAN_POINT('Ctrl Pts',(-19.4025860162462,21.2228826377151,
9.44753907605117));
#198191=CARTESIAN_POINT('Ctrl Pts',(-19.2395033767298,21.2674998371823,
9.45694036405629));
#198192=CARTESIAN_POINT('Ctrl Pts',(-19.1858102519556,21.2799591816438,
9.46004745135552));
#198193=CARTESIAN_POINT('Ctrl Pts',(-19.0980015922924,21.2967537267562,
9.46519081550471));
#198194=CARTESIAN_POINT('Ctrl Pts',(-19.0641581510429,21.3023778153729,
9.46718771769038));
#198195=CARTESIAN_POINT('Ctrl Pts',(-19.0194921664403,21.3086892159295,
9.46984812507602));
#198196=CARTESIAN_POINT('Ctrl Pts',(-19.0087787071528,21.3101194533097,
9.47048810736266));
#198197=CARTESIAN_POINT('Ctrl Pts',(-18.9912106985769,21.3123279706189,
9.47154078471046));
#198198=CARTESIAN_POINT('Ctrl Pts',(-18.9843623827013,21.3131549084605,
9.47195193865683));
#198199=CARTESIAN_POINT('Ctrl Pts',(-18.9710961970775,21.3146910620382,
9.47275000413827));
#198200=CARTESIAN_POINT('Ctrl Pts',(-18.9646788765133,21.3154044159015,
9.4731367803345));
#198201=CARTESIAN_POINT('Ctrl Pts',(-18.9498510711551,21.3169840458204,
9.47403217588533));
#198202=CARTESIAN_POINT('Ctrl Pts',(-18.9414385017158,21.3178293122451,
9.47454145144701));
#198203=CARTESIAN_POINT('Ctrl Pts',(-18.9187937407615,21.3199676381122,
9.4759158264876));
#198204=CARTESIAN_POINT('Ctrl Pts',(-18.9045533366357,21.3211670002328,
9.4767838544749));
#198205=CARTESIAN_POINT('Ctrl Pts',(-18.7737124064208,21.3308536736132,
9.48479486767219));
#198206=CARTESIAN_POINT('Ctrl Pts',(-18.6566272837034,21.3298115341273,
9.4922399577738));
#198207=CARTESIAN_POINT('Ctrl Pts',(-18.3780207271946,21.30420470784,9.51051549157705));
#198208=CARTESIAN_POINT('Ctrl Pts',(-18.2180663795343,21.2706212740284,
9.52148645629154));
#198209=CARTESIAN_POINT('Ctrl Pts',(-18.0329148996013,21.2088016788044,
9.53388734209194));
#198210=CARTESIAN_POINT('Ctrl Pts',(-18.0025197840609,21.1978741336953,
9.53591104784495));
#198211=CARTESIAN_POINT('Ctrl Pts',(-17.9656436128781,21.1836554847918,
9.53834131470093));
#198212=CARTESIAN_POINT('Ctrl Pts',(-17.9589156906172,21.1810217044809,
9.53878367693989));
#198213=CARTESIAN_POINT('Ctrl Pts',(-17.9483851120989,21.1768370000413,
9.53947429480328));
#198214=CARTESIAN_POINT('Ctrl Pts',(-17.9445733340599,21.1753093958406,
9.53972391409476));
#198215=CARTESIAN_POINT('Ctrl Pts',(-17.9374538901133,21.1724321442594,
9.54018942343491));
#198216=CARTESIAN_POINT('Ctrl Pts',(-17.9341452321789,21.1710852308843,
9.54040546773772));
#198217=CARTESIAN_POINT('Ctrl Pts',(-17.9265965685278,21.1679899673576,
9.54089771428285));
#198218=CARTESIAN_POINT('Ctrl Pts',(-17.922358832866,21.1662362134057,9.54117358570328));
#198219=CARTESIAN_POINT('Ctrl Pts',(-17.9093381078825,21.1607980608227,
9.54201986875329));
#198220=CARTESIAN_POINT('Ctrl Pts',(-17.9005741171114,21.1570680922558,
9.54258758981504));
#198221=CARTESIAN_POINT('Ctrl Pts',(-17.782929025579,21.1060576408512,9.55018678117345));
#198222=CARTESIAN_POINT('Ctrl Pts',(-17.6781704763533,21.0497527415101,
9.55670838499721));
#198223=CARTESIAN_POINT('Ctrl Pts',(-17.4871215863486,20.9253279009855,
9.56912064420152));
#198224=CARTESIAN_POINT('Ctrl Pts',(-17.4003237687817,20.8587052971729,
9.57500415806185));
#198225=CARTESIAN_POINT('Ctrl Pts',(-17.2781503546985,20.7489257189789,
9.58413785601873));
#198226=CARTESIAN_POINT('Ctrl Pts',(-17.238692224888,20.7105891845749,9.58723927556134));
#198227=CARTESIAN_POINT('Ctrl Pts',(-17.1771518333463,20.6459516725265,
9.59237409329115));
#198228=CARTESIAN_POINT('Ctrl Pts',(-17.1541371778341,20.6205729083274,
9.59436828818859));
#198229=CARTESIAN_POINT('Ctrl Pts',(-17.1246885345662,20.5864716693302,
9.59702559973078));
#198230=CARTESIAN_POINT('Ctrl Pts',(-17.1176905695215,20.5782415749621,
9.59766526328236));
#198231=CARTESIAN_POINT('Ctrl Pts',(-17.1063287045608,20.5646700931405,
9.59871754990777));
#198232=CARTESIAN_POINT('Ctrl Pts',(-17.1019273197589,20.5593602381188,
9.59912863411235));
#198233=CARTESIAN_POINT('Ctrl Pts',(-17.0934554419456,20.5490374622768,
9.5999266597221));
#198234=CARTESIAN_POINT('Ctrl Pts',(-17.0893817791442,20.5440272328854,
9.60031346629392));
#198235=CARTESIAN_POINT('Ctrl Pts',(-17.0800254800757,20.5324116782775,
9.60120907135326));
#198236=CARTESIAN_POINT('Ctrl Pts',(-17.0747594054637,20.5257932089295,
9.60171852701432));
#198237=CARTESIAN_POINT('Ctrl Pts',(-17.0606963242318,20.5078995045333,
9.60309370329275));
#198238=CARTESIAN_POINT('Ctrl Pts',(-17.0519737926135,20.4965665436334,
9.60396235773285));
#198239=CARTESIAN_POINT('Ctrl Pts',(-16.972516591875,20.3911367566103,9.61202351569985));
#198240=CARTESIAN_POINT('Ctrl Pts',(-16.9096424763334,20.2913972480126,
9.61952253163762));
#198241=CARTESIAN_POINT('Ctrl Pts',(-16.7799847257009,20.0418221704587,
9.63789912037959));
#198242=CARTESIAN_POINT('Ctrl Pts',(-16.7216567648856,19.8884335690771,
9.64891538407312));
#198243=CARTESIAN_POINT('Ctrl Pts',(-16.6739757242247,19.6998239156768,
9.66125913182953));
#198244=CARTESIAN_POINT('Ctrl Pts',(-16.6670422527242,19.6696226584634,
9.66319881259296));
#198245=CARTESIAN_POINT('Ctrl Pts',(-16.6593309330688,19.6322934057461,
9.66554221773797));
#198246=CARTESIAN_POINT('Ctrl Pts',(-16.6579233039985,19.6253011304167,
9.6659788494655));
#198247=CARTESIAN_POINT('Ctrl Pts',(-16.6557648778657,19.6142920442681,
9.66666252092505));
#198248=CARTESIAN_POINT('Ctrl Pts',(-16.6549903411732,19.6102800207873,
9.66691088031755));
#198249=CARTESIAN_POINT('Ctrl Pts',(-16.6535598290674,19.6027530849862,
9.66737531317241));
#198250=CARTESIAN_POINT('Ctrl Pts',(-16.6529011500223,19.5992387941174,
9.66759153326132));
#198251=CARTESIAN_POINT('Ctrl Pts',(-16.6514121583734,19.5911818072088,
9.6680858421601));
#198252=CARTESIAN_POINT('Ctrl Pts',(-16.6505878051263,19.5866380595754,
9.66836358952008));
#198253=CARTESIAN_POINT('Ctrl Pts',(-16.6480803550525,19.5725550628477,
9.66922139368315));
#198254=CARTESIAN_POINT('Ctrl Pts',(-16.6464478293761,19.5630067778102,
9.66979865259885));
#198255=CARTESIAN_POINT('Ctrl Pts',(-16.6279609211413,19.4502263873174,
9.67656949773241));
#198256=CARTESIAN_POINT('Ctrl Pts',(-16.6187119317562,19.3458784281049,
9.68236860186208));
#198257=CARTESIAN_POINT('Ctrl Pts',(-16.6148005740982,19.0722859228046,
9.69731859862332));
#198258=CARTESIAN_POINT('Ctrl Pts',(-16.6326252356836,18.9036416198706,
9.70632881182754));
#198259=CARTESIAN_POINT('Ctrl Pts',(-16.6796530836691,18.6980637473473,
9.71838536827981));
#198260=CARTESIAN_POINT('Ctrl Pts',(-16.6902075756455,18.6575047175167,
9.72081453095264));
#198261=CARTESIAN_POINT('Ctrl Pts',(-16.7052112877906,18.6061529768218,
9.72396600025222));
#198262=CARTESIAN_POINT('Ctrl Pts',(-16.7085559212137,18.5950455894642,
9.7246522392589));
#198263=CARTESIAN_POINT('Ctrl Pts',(-16.7140865696057,18.5772107913768,
9.72576171661946));
#198264=CARTESIAN_POINT('Ctrl Pts',(-16.7162153410324,18.5704657734164,
9.72618307494958));
#198265=CARTESIAN_POINT('Ctrl Pts',(-16.7203354362771,18.5576356161355,
9.72698798052912));
#198266=CARTESIAN_POINT('Ctrl Pts',(-16.7223206461291,18.5515485847238,
9.72737132265636));
#198267=CARTESIAN_POINT('Ctrl Pts',(-16.7269175487943,18.537667540411,9.72824891014382));
#198268=CARTESIAN_POINT('Ctrl Pts',(-16.7295470723675,18.5298795811279,
9.72874374036002));
#198269=CARTESIAN_POINT('Ctrl Pts',(-16.7365144843569,18.5096337411346,
9.73003662642503));
#198270=CARTESIAN_POINT('Ctrl Pts',(-16.7409235266807,18.497200887219,9.73083703059558));
#198271=CARTESIAN_POINT('Ctrl Pts',(-16.7716690078757,18.4130094243426,
9.7363018639495));
#198272=CARTESIAN_POINT('Ctrl Pts',(-16.8017561228273,18.3426894667636,
9.74109128645236));
#198273=CARTESIAN_POINT('Ctrl Pts',(-16.921780172379,18.0994722372349,9.75846999541262));
#198274=CARTESIAN_POINT('Ctrl Pts',(-17.0316660862533,17.9375479685287,
9.77166726323247));
#198275=CARTESIAN_POINT('Ctrl Pts',(-17.1902366627887,17.7617778206229,
9.78683301440995));
#198276=CARTESIAN_POINT('Ctrl Pts',(-17.2192701516351,17.7314581116134,
9.78947996192508));
#198277=CARTESIAN_POINT('Ctrl Pts',(-17.2547430210394,17.6965533927764,
9.79254374545519));
#198278=CARTESIAN_POINT('Ctrl Pts',(-17.2603282817907,17.6911179627308,
9.7930213352587));
#198279=CARTESIAN_POINT('Ctrl Pts',(-17.2689913127958,17.6827799764446,
9.79375453963165));
#198280=CARTESIAN_POINT('Ctrl Pts',(-17.2720479121388,17.6798556607885,
9.79401180162807));
#198281=CARTESIAN_POINT('Ctrl Pts',(-17.2776933699718,17.6744868446462,
9.79448428436337));
#198282=CARTESIAN_POINT('Ctrl Pts',(-17.2802796124028,17.6720397301195,
9.79469970453727));
#198283=CARTESIAN_POINT('Ctrl Pts',(-17.2860908403172,17.6665688399374,
9.79518145660487));
#198284=CARTESIAN_POINT('Ctrl Pts',(-17.2893191197814,17.6635486443792,
9.79544751356641));
#198285=CARTESIAN_POINT('Ctrl Pts',(-17.2975687555384,17.6558790691032,
9.79612349225951));
#198286=CARTESIAN_POINT('Ctrl Pts',(-17.3026032819286,17.6512438433648,
9.79653235653453));
#198287=CARTESIAN_POINT('Ctrl Pts',(-17.3315053871257,17.6248918288508,
9.79885930004098));
#198288=CARTESIAN_POINT('Ctrl Pts',(-17.3558459481913,17.6036973111419,
9.80074054842719));
#198289=CARTESIAN_POINT('Ctrl Pts',(-17.3954616522374,17.5707639069678,
9.80369742715779));
#198290=CARTESIAN_POINT('Ctrl Pts',(-17.410427767966,17.5586634915258,9.80479154979167));
#198291=CARTESIAN_POINT('Ctrl Pts',(-17.426697316939,17.5458721375866,9.80595906110082));
#198292=CARTESIAN_POINT('Ctrl Pts',(-17.4278383477558,17.5449769384711,
9.8060408276413));
#198293=CARTESIAN_POINT('Ctrl Pts',(-17.4470195008386,17.5299601252104,
9.80741344965776));
#198294=CARTESIAN_POINT('Ctrl Pts',(-17.4652872283598,17.5161307361346,
9.80869245245463));
#198295=CARTESIAN_POINT('Ctrl Pts',(-17.5206370878767,17.4756251646983,
9.81249557890216));
#198296=CARTESIAN_POINT('Ctrl Pts',(-17.5583623569115,17.449849312523,9.8149932263107));
#198297=CARTESIAN_POINT('Ctrl Pts',(-17.6891293853963,17.3665781944157,
9.82343367022865));
#198298=CARTESIAN_POINT('Ctrl Pts',(-17.7857771714591,17.3150783291671,
9.82932176592834));
#198299=CARTESIAN_POINT('Ctrl Pts',(-17.9364617660584,17.2492000869357,
9.83846611489902));
#198300=CARTESIAN_POINT('Ctrl Pts',(-17.9877967539146,17.2291054004682,
9.84157363858167));
#198301=CARTESIAN_POINT('Ctrl Pts',(-18.0722656972139,17.1997879945636,
9.84671766068652));
#198302=CARTESIAN_POINT('Ctrl Pts',(-18.1049439105122,17.1893288452427,
9.84871477123229));
#198303=CARTESIAN_POINT('Ctrl Pts',(-18.1482320468893,17.1766249760926,
9.85137541687025));
#198304=CARTESIAN_POINT('Ctrl Pts',(-18.1586265732511,17.1736607435132,
9.85201542367111));
#198305=CARTESIAN_POINT('Ctrl Pts',(-18.1756912036971,17.1689353896586,
9.85306813107032));
#198306=CARTESIAN_POINT('Ctrl Pts',(-18.1823481036325,17.1671270175619,
9.85347929038108));
#198307=CARTESIAN_POINT('Ctrl Pts',(-18.1952528750725,17.163689025558,9.85427735893401));
#198308=CARTESIAN_POINT('Ctrl Pts',(-18.2014996045733,17.1620553892002,
9.85466413279845));
#198309=CARTESIAN_POINT('Ctrl Pts',(-18.2159429947749,17.1583486848286,
9.85555951225615));
#198310=CARTESIAN_POINT('Ctrl Pts',(-18.2241447551176,17.1562961020224,
9.85606877398238));
#198311=CARTESIAN_POINT('Ctrl Pts',(-18.2462414748078,17.1509065982363,
9.85744308747781));
#198312=CARTESIAN_POINT('Ctrl Pts',(-18.2601581038214,17.1476611900619,
9.85831106734732));
#198313=CARTESIAN_POINT('Ctrl Pts',(-18.3881653251675,17.119172758855,9.86631840861463));
#198314=CARTESIAN_POINT('Ctrl Pts',(-18.5041113482054,17.1032793757705,
9.87375955380936));
#198315=CARTESIAN_POINT('Ctrl Pts',(-18.7832498985648,17.0883266666903,
9.89201887790245));
#198316=CARTESIAN_POINT('Ctrl Pts',(-18.9461968238054,17.0983854555601,
9.90297711145388));
#198317=CARTESIAN_POINT('Ctrl Pts',(-19.1383850972074,17.1327270232927,
9.91538262627974));
#198318=CARTESIAN_POINT('Ctrl Pts',(-19.1702539013258,17.139182277625,9.917420184744));
#198319=CARTESIAN_POINT('Ctrl Pts',(-19.2090239435011,17.1479697852639,
9.91986473493801));
#198320=CARTESIAN_POINT('Ctrl Pts',(-19.2160764507605,17.1496063663328,
9.92030801579544));
#198321=CARTESIAN_POINT('Ctrl Pts',(-19.2271190429344,17.1522286433133,
9.92099974674368));
#198322=CARTESIAN_POINT('Ctrl Pts',(-19.2311148119395,17.1531898158401,
9.92124956761185));
#198323=CARTESIAN_POINT('Ctrl Pts',(-19.2385781685672,17.1550081152537,
9.92171525135607));
#198324=CARTESIAN_POINT('Ctrl Pts',(-19.2420463477369,17.1558623727062,
9.92193126970113));
#198325=CARTESIAN_POINT('Ctrl Pts',(-19.2499579841591,17.157832362697,9.92242319618484));
#198326=CARTESIAN_POINT('Ctrl Pts',(-19.2543999835046,17.1589537416619,
9.92269877515916));
#198327=CARTESIAN_POINT('Ctrl Pts',(-19.2680410713539,17.1624445650132,
9.92354327015164));
#198328=CARTESIAN_POINT('Ctrl Pts',(-19.2772280261641,17.164861550309,9.92410951206675));
#198329=CARTESIAN_POINT('Ctrl Pts',(-19.3595520277177,17.1871136227094,
9.92916361140246));
#198330=CARTESIAN_POINT('Ctrl Pts',(-19.4315996383471,17.210802823055,9.93344569392556));
#198331=CARTESIAN_POINT('Ctrl Pts',(-19.5420512036803,17.2538161595377,
9.94000648320762));
#198332=CARTESIAN_POINT('Ctrl Pts',(-19.5813960228866,17.2705269907126,
9.94234263424595));
#198333=CARTESIAN_POINT('Ctrl Pts',(-19.7194906226425,17.3341813100814,
9.95062123118651));
#198334=CARTESIAN_POINT('Ctrl Pts',(-19.8150773194542,17.3875661227974,
9.95650793123038));
#198335=CARTESIAN_POINT('Ctrl Pts',(-19.9519738974235,17.4785849429644,
9.96564903557837));
#198336=CARTESIAN_POINT('Ctrl Pts',(-19.9966274390109,17.5108548148603,
9.96875469954442));
#198337=CARTESIAN_POINT('Ctrl Pts',(-20.0669593696601,17.5659819849045,
9.97389591760056));
#198338=CARTESIAN_POINT('Ctrl Pts',(-20.0934295913258,17.5877883868564,
9.97589214010261));
#198339=CARTESIAN_POINT('Ctrl Pts',(-20.1275293159034,17.6172993255093,
9.97855177028231));
#198340=CARTESIAN_POINT('Ctrl Pts',(-20.1356467557165,17.6244338463876,
9.9791916725856));
#198341=CARTESIAN_POINT('Ctrl Pts',(-20.1488551336826,17.6362233396075,
9.98024425188442));
#198342=CARTESIAN_POINT('Ctrl Pts',(-20.1539786396014,17.6408416510526,
9.98065538832868));
#198343=CARTESIAN_POINT('Ctrl Pts',(-20.1638543627909,17.6498314652345,
9.98145344379378));
#198344=CARTESIAN_POINT('Ctrl Pts',(-20.168609335561,17.6541998376084,9.98184022760254));
#198345=CARTESIAN_POINT('Ctrl Pts',(-20.1795448213011,17.6643388644299,
9.98273567568082));
#198346=CARTESIAN_POINT('Ctrl Pts',(-20.1857108628382,17.6701249024822,
9.98324499639986));
#198347=CARTESIAN_POINT('Ctrl Pts',(-20.2022061769968,17.6857905324228,
9.98461957232397));
#198348=CARTESIAN_POINT('Ctrl Pts',(-20.2124701921566,17.6957379192579,
9.98548775736936));
#198349=CARTESIAN_POINT('Ctrl Pts',(-20.3058953903506,17.7881340820861,
9.99351092039735));
#198350=CARTESIAN_POINT('Ctrl Pts',(-20.382168567715,17.8772327582584,10.0009690673243));
#198351=CARTESIAN_POINT('Ctrl Pts',(-20.5463777362288,18.1047806390244,
10.0193001576771));
#198352=CARTESIAN_POINT('Ctrl Pts',(-20.6263877479788,18.2480341934771,
10.0303152960732));
#198353=CARTESIAN_POINT('Ctrl Pts',(-20.7012121906667,18.4282095779477,
10.042700831961));
#198354=CARTESIAN_POINT('Ctrl Pts',(-20.7126617678792,18.4576192839732,
10.0446771660736));
#198355=CARTESIAN_POINT('Ctrl Pts',(-20.7259025049934,18.4940168294528,
10.0470585100492));
#198356=CARTESIAN_POINT('Ctrl Pts',(-20.7283205544069,18.5007704695581,
10.0474976755916));
#198357=CARTESIAN_POINT('Ctrl Pts',(-20.7320650318759,18.5113987578401,
10.0481844190689));
#198358=CARTESIAN_POINT('Ctrl Pts',(-20.7334145988123,18.5152651134591,
10.0484333360482));
#198359=CARTESIAN_POINT('Ctrl Pts',(-20.7359210084947,18.5225132174356,
10.0488982423822));
#198360=CARTESIAN_POINT('Ctrl Pts',(-20.7370804931179,18.5258939408191,
10.0491143817466));
#198361=CARTESIAN_POINT('Ctrl Pts',(-20.7397139287311,18.5336361169858,
10.0496077645352));
#198362=CARTESIAN_POINT('Ctrl Pts',(-20.7411822155883,18.5379994440847,
10.0498846712711));
#198363=CARTESIAN_POINT('Ctrl Pts',(-20.7456726562695,18.5514891608176,
10.050737301678));
#198364=CARTESIAN_POINT('Ctrl Pts',(-20.748646934659,18.5606315201919,10.0513102759193));
#198365=CARTESIAN_POINT('Ctrl Pts',(-20.7774526056146,18.6512687556419,
10.0569455155612));
#198366=CARTESIAN_POINT('Ctrl Pts',(-20.7983905411972,18.7342475906723,
10.0617452393583));
#198367=CARTESIAN_POINT('Ctrl Pts',(-20.8385991839127,18.9472314285597,
10.0736796187252));
#198368=CARTESIAN_POINT('Ctrl Pts',(-20.8509009165662,19.0781722963637,
10.0806786689208));
#198369=CARTESIAN_POINT('Ctrl Pts',(-20.8510686215296,19.3016470631716,
10.0930379618485));
#198370=CARTESIAN_POINT('Ctrl Pts',(-20.8451100151077,19.3937783280465,
10.0982491651107));
#198371=CARTESIAN_POINT('Ctrl Pts',(-20.8313804909468,19.4988780661773,
10.1044628226863));
#198372=CARTESIAN_POINT('Ctrl Pts',(-20.8294631854275,19.5125173791607,
10.1052743194174));
#198373=CARTESIAN_POINT('Ctrl Pts',(-20.8261768233744,19.5343482583805,
10.1065817984235));
#198374=CARTESIAN_POINT('Ctrl Pts',(-20.8248923986009,19.5425523049788,
10.1070751037696));
#198375=CARTESIAN_POINT('Ctrl Pts',(-20.8225273356179,19.5570981837842,
10.1079532951721));
#198376=CARTESIAN_POINT('Ctrl Pts',(-20.8214659898445,19.5634430794814,
10.1083375644673));
#198377=CARTESIAN_POINT('Ctrl Pts',(-20.8191956392426,19.5766455016435,
10.1091396978766));
#198378=CARTESIAN_POINT('Ctrl Pts',(-20.8179816887034,19.5835020887657,
10.1095577151611));
#198379=CARTESIAN_POINT('Ctrl Pts',(-20.8147441170231,19.6012771145112,
10.1106451675106));
#198380=CARTESIAN_POINT('Ctrl Pts',(-20.8126683965908,19.6121857378977,
10.1113162553442));
#198381=CARTESIAN_POINT('Ctrl Pts',(-20.8033102345472,19.6593426322595,
10.1142337296146));
#198382=CARTESIAN_POINT('Ctrl Pts',(-20.7951650779569,19.695411203176,10.1165074902027));
#198383=CARTESIAN_POINT('Ctrl Pts',(-20.7710540774191,19.790515584671,10.1226195362212));
#198384=CARTESIAN_POINT('Ctrl Pts',(-20.7534685869628,19.8491012118838,
10.126506512534));
#198385=CARTESIAN_POINT('Ctrl Pts',(-20.7298520717044,19.916959144821,10.131146365902));
#198386=CARTESIAN_POINT('Ctrl Pts',(-20.7262541603358,19.9270496306836,
10.1318399254289));
#198387=CARTESIAN_POINT('Ctrl Pts',(-20.7225805927058,19.9371103403161,
10.1325349747556));
#198388=CARTESIAN_POINT('Origin',(-18.734,19.211,0.));
#198389=CARTESIAN_POINT('',(-20.7225806899004,19.9371100741315,11.1558808822554));
#198390=CARTESIAN_POINT('',(-20.7225806064498,19.9371103026755,10.9336112484111));
#198391=CARTESIAN_POINT('',(-20.7225806064498,19.9371103026755,0.));
#198392=CARTESIAN_POINT('',(-20.8509995968923,19.2096935705332,11.1109437209282));
#198393=CARTESIAN_POINT('Ctrl Pts',(-20.7225806899004,19.9371100741315,
11.1558808822554));
#198394=CARTESIAN_POINT('Ctrl Pts',(-20.7445653673935,19.8769011516913,
11.1523876403128));
#198395=CARTESIAN_POINT('Ctrl Pts',(-20.763823629495,19.8156719423086,11.1488667470025));
#198396=CARTESIAN_POINT('Ctrl Pts',(-20.7906145513329,19.7146376108668,
11.1430184534343));
#198397=CARTESIAN_POINT('Ctrl Pts',(-20.799831825771,19.6753843887736,11.1407374126506));
#198398=CARTESIAN_POINT('Ctrl Pts',(-20.8091426808549,19.6299377205522,
11.1380746344932));
#198399=CARTESIAN_POINT('Ctrl Pts',(-20.810337188784,19.6239767996495,11.137724952832));
#198400=CARTESIAN_POINT('Ctrl Pts',(-20.8121465849177,19.6147410968476,
11.1371824640975));
#198401=CARTESIAN_POINT('Ctrl Pts',(-20.812779451429,19.6114698413517,11.1369901805635));
#198402=CARTESIAN_POINT('Ctrl Pts',(-20.8188276074304,19.5798065618939,
11.1351276632203));
#198403=CARTESIAN_POINT('Ctrl Pts',(-20.8236684176471,19.5513090037321,
11.1334407399127));
#198404=CARTESIAN_POINT('Ctrl Pts',(-20.829467698782,19.5123536362169,11.1311168047545));
#198405=CARTESIAN_POINT('Ctrl Pts',(-20.8309342155032,19.5019738485889,
11.1304958634879));
#198406=CARTESIAN_POINT('Ctrl Pts',(-20.8331379328417,19.4854935205726,
11.1295070910953));
#198407=CARTESIAN_POINT('Ctrl Pts',(-20.8339257795473,19.4793998381151,
11.1291408638761));
#198408=CARTESIAN_POINT('Ctrl Pts',(-20.8354516395268,19.4671797870958,
11.1284051599387));
#198409=CARTESIAN_POINT('Ctrl Pts',(-20.8361894175406,19.4610534505192,
11.128035679647));
#198410=CARTESIAN_POINT('Ctrl Pts',(-20.837616391639,19.4487513233087,11.1272924070941));
#198411=CARTESIAN_POINT('Ctrl Pts',(-20.8383052007998,19.4425755503276,
11.1269186065157));
#198412=CARTESIAN_POINT('Ctrl Pts',(-20.839817318421,19.4284539825217,11.1260623031829));
#198413=CARTESIAN_POINT('Ctrl Pts',(-20.8406228594108,19.4205064164719,
11.1255792453081));
#198414=CARTESIAN_POINT('Ctrl Pts',(-20.8425678109608,19.4001706896508,
11.124340258937));
#198415=CARTESIAN_POINT('Ctrl Pts',(-20.8436430281583,19.3877768271365,
11.1235823280557));
#198416=CARTESIAN_POINT('Ctrl Pts',(-20.8489047513553,19.3202149734588,
11.1194348915391));
#198417=CARTESIAN_POINT('Ctrl Pts',(-20.851036203119,19.2649135578119,11.1159820029749));
#198418=CARTESIAN_POINT('Ctrl Pts',(-20.8509995348902,19.2095966915971,
11.1124693680802));
#198419=CARTESIAN_POINT('Ctrl Pts',(-20.7225806064498,19.9371103026755,
10.3555828687981));
#198420=CARTESIAN_POINT('Ctrl Pts',(-20.6978477139366,20.0048456731998,
10.3599055461406));
#198421=CARTESIAN_POINT('Ctrl Pts',(-20.6696397182687,20.071343807373,10.3642282234831));
#198422=CARTESIAN_POINT('Ctrl Pts',(-20.6381130431754,20.1362256583177,
10.3685509008256));
#198423=CARTESIAN_POINT('Ctrl Pts',(-20.6065863063599,20.2011076362865,
10.3728735866309));
#198424=CARTESIAN_POINT('Ctrl Pts',(-20.5717410957585,20.2643728810197,
10.3771962724362));
#198425=CARTESIAN_POINT('Ctrl Pts',(-20.5337806062108,20.3256653172623,
10.3815189582415));
#198426=CARTESIAN_POINT('Ctrl Pts',(-20.495782105661,20.3870191275007,10.3858459724846));
#198427=CARTESIAN_POINT('Ctrl Pts',(-20.4546623619949,20.4463957658043,
10.3901729867278));
#198428=CARTESIAN_POINT('Ctrl Pts',(-20.4106683247005,20.5034675349679,
10.3945000009709));
#198429=CARTESIAN_POINT('Ctrl Pts',(-20.3666497254667,20.560571167389,10.3988294309929));
#198430=CARTESIAN_POINT('Ctrl Pts',(-20.3197539628617,20.6153669959171,
10.4031588610148));
#198431=CARTESIAN_POINT('Ctrl Pts',(-20.2702669159773,20.6675620353674,
10.4074882910367));
#198432=CARTESIAN_POINT('Ctrl Pts',(-20.2206957718595,20.719845773956,10.4118250783998));
#198433=CARTESIAN_POINT('Ctrl Pts',(-20.1685249152318,20.7695195646485,
10.4161618657629));
#198434=CARTESIAN_POINT('Ctrl Pts',(-20.114074862226,20.816329366408,10.420498653126));
#198435=CARTESIAN_POINT('Ctrl Pts',(-20.0868592195423,20.839726200175,10.4226662994138));
#198436=CARTESIAN_POINT('Ctrl Pts',(-20.0590746522195,20.8624081912211,
10.4248339457017));
#198437=CARTESIAN_POINT('Ctrl Pts',(-20.0307638001157,20.8843477363386,
10.4270015919895));
#198438=CARTESIAN_POINT('Ctrl Pts',(-19.9734509743371,20.9287624124624,
10.4313898009204));
#198439=CARTESIAN_POINT('Ctrl Pts',(-19.9137418045025,20.9703158984433,
10.4357780098513));
#198440=CARTESIAN_POINT('Ctrl Pts',(-19.8519537768691,21.0087397900653,
10.4401662187821));
#198441=CARTESIAN_POINT('Ctrl Pts',(-19.7902574529134,21.0471066542614,
10.4445479148834));
#198442=CARTESIAN_POINT('Ctrl Pts',(-19.7264888022841,21.0823528921034,
10.4489296109847));
#198443=CARTESIAN_POINT('Ctrl Pts',(-19.6609970987611,21.1142512653059,
10.4533113070859));
#198444=CARTESIAN_POINT('Ctrl Pts',(-19.5955823532016,21.1461121553814,
10.4576878543455));
#198445=CARTESIAN_POINT('Ctrl Pts',(-19.5284490083968,21.1746327855719,
10.4620644016052));
#198446=CARTESIAN_POINT('Ctrl Pts',(-19.4599724698909,21.199630929298,10.4664409488648));
#198447=CARTESIAN_POINT('Ctrl Pts',(-19.3915393582105,21.2246132195646,
10.4708147205818));
#198448=CARTESIAN_POINT('Ctrl Pts',(-19.3217651949909,21.2460772907209,
10.4751884922988));
#198449=CARTESIAN_POINT('Ctrl Pts',(-19.2510456730823,21.2638888844618,
10.4795622640157));
#198450=CARTESIAN_POINT('Ctrl Pts',(-19.1803476713616,21.281695058075,10.4839347047793));
#198451=CARTESIAN_POINT('Ctrl Pts',(-19.1087053495654,21.295850843123,10.4883071455428));
#198452=CARTESIAN_POINT('Ctrl Pts',(-19.0365282611626,21.3062722141044,
10.4926795863064));
#198453=CARTESIAN_POINT('Ctrl Pts',(-18.9643493271836,21.3166938515614,
10.4970521388737));
#198454=CARTESIAN_POINT('Ctrl Pts',(-18.8916360771621,21.3233808184121,
10.5014246914411));
#198455=CARTESIAN_POINT('Ctrl Pts',(-18.8188052520575,21.3263007042081,
10.5057972440084));
#198456=CARTESIAN_POINT('Ctrl Pts',(-18.7458988403756,21.3292236203718,
10.5101743345757));
#198457=CARTESIAN_POINT('Ctrl Pts',(-18.6728750930034,21.3283716302984,
10.5145514251431));
#198458=CARTESIAN_POINT('Ctrl Pts',(-18.6001519939633,21.3237644713219,
10.5189285157104));
#198459=CARTESIAN_POINT('Ctrl Pts',(-18.5273891781396,21.3191547962048,
10.5233079967693));
#198460=CARTESIAN_POINT('Ctrl Pts',(-18.4549278170834,21.3107859243705,
10.5276874778283));
#198461=CARTESIAN_POINT('Ctrl Pts',(-18.3831792948549,21.2987293485606,
10.5320669588872));
#198462=CARTESIAN_POINT('Ctrl Pts',(-18.3113035988522,21.2866514025511,
10.5364542025469));
#198463=CARTESIAN_POINT('Ctrl Pts',(-18.2401437361938,21.2708728040954,
10.5408414462066));
#198464=CARTESIAN_POINT('Ctrl Pts',(-18.1700988737775,21.2515157484923,
10.5452286898664));
#198465=CARTESIAN_POINT('Ctrl Pts',(-18.1224751168409,21.2383548159235,
10.5482115928012));
#198466=CARTESIAN_POINT('Ctrl Pts',(-18.0753664841794,21.2235407241658,
10.551194495736));
#198467=CARTESIAN_POINT('Ctrl Pts',(-18.0288930166915,21.2071245307068,
10.5541773986709));
#198468=CARTESIAN_POINT('Ctrl Pts',(-17.960524957276,21.1829743359732,10.5585656076018));
#198469=CARTESIAN_POINT('Ctrl Pts',(-17.8932656103902,21.1552604871605,
10.5629538165327));
#198470=CARTESIAN_POINT('Ctrl Pts',(-17.8275125107933,21.1241046578564,
10.5673420254636));
#198471=CARTESIAN_POINT('Ctrl Pts',(-17.7618569996982,21.0929950689686,
10.5717237215649));
#198472=CARTESIAN_POINT('Ctrl Pts',(-17.6977037303933,21.0584538454431,
10.5761054176661));
#198473=CARTESIAN_POINT('Ctrl Pts',(-17.6354328295881,21.0206516714808,
10.5804871137674));
#198474=CARTESIAN_POINT('Ctrl Pts',(-17.5732351020472,20.9828939180814,
10.5848636610271));
#198475=CARTESIAN_POINT('Ctrl Pts',(-17.5129157592863,20.9418830753682,
10.5892402082867));
#198476=CARTESIAN_POINT('Ctrl Pts',(-17.4548312249217,20.8978361642035,
10.5936167555463));
#198477=CARTESIAN_POINT('Ctrl Pts',(-17.3967835269247,20.8538171869497,
10.5979905272633));
#198478=CARTESIAN_POINT('Ctrl Pts',(-17.3409682086661,20.8067662523013,
10.6023642989803));
#198479=CARTESIAN_POINT('Ctrl Pts',(-17.2877123411685,20.7569434038514,
10.6067380706973));
#198480=CARTESIAN_POINT('Ctrl Pts',(-17.2344726796103,20.7071357166617,
10.6111105114608));
#198481=CARTESIAN_POINT('Ctrl Pts',(-17.1837912746023,20.654558119635,10.6154829522244));
#198482=CARTESIAN_POINT('Ctrl Pts',(-17.135960461819,20.5995095010155,10.6198553929879));
#198483=CARTESIAN_POINT('Ctrl Pts',(-17.0881284259965,20.5444594747966,
10.6242279455553));
#198484=CARTESIAN_POINT('Ctrl Pts',(-17.0431474419898,20.4869386669777,
10.6286004981226));
#198485=CARTESIAN_POINT('Ctrl Pts',(-17.0012703358341,20.4272799475941,
10.63297305069));
#198486=CARTESIAN_POINT('Ctrl Pts',(-16.9593497680381,20.3675593121413,
10.6373501412573));
#198487=CARTESIAN_POINT('Ctrl Pts',(-16.9205397874118,20.3056967307924,
10.6417272318246));
#198488=CARTESIAN_POINT('Ctrl Pts',(-16.8850500448046,20.2420543454071,
10.6461043223919));
#198489=CARTESIAN_POINT('Ctrl Pts',(-16.8495409199318,20.1783772025532,
10.6504838034509));
#198490=CARTESIAN_POINT('Ctrl Pts',(-16.8173558563405,20.1129187535682,
10.6548632845098));
#198491=CARTESIAN_POINT('Ctrl Pts',(-16.7886574143382,20.0460636050089,
10.6592427655688));
#198492=CARTESIAN_POINT('Ctrl Pts',(-16.75990810454,19.9790899561476,10.6636300092285));
#198493=CARTESIAN_POINT('Ctrl Pts',(-16.7346579248205,19.9107151168649,
10.6680172528882));
#198494=CARTESIAN_POINT('Ctrl Pts',(-16.7130201897423,19.8413408653503,
10.6724044965479));
#198495=CARTESIAN_POINT('Ctrl Pts',(-16.6983086148963,19.7941730592073,
10.6753873994827));
#198496=CARTESIAN_POINT('Ctrl Pts',(-16.68526591231,19.7465435673453,10.6783703024176));
#198497=CARTESIAN_POINT('Ctrl Pts',(-16.673914126578,19.6985809616125,10.6813532053524));
#198498=CARTESIAN_POINT('Ctrl Pts',(-16.6572142846389,19.6280222007594,
10.6857414142833));
#198499=CARTESIAN_POINT('Ctrl Pts',(-16.6441110368839,19.5564667533231,
10.6901296232142));
#198500=CARTESIAN_POINT('Ctrl Pts',(-16.6347172531062,19.4843147427305,
10.6945178321451));
#198501=CARTESIAN_POINT('Ctrl Pts',(-16.6253374112611,19.4122698176846,
10.6988995282463));
#198502=CARTESIAN_POINT('Ctrl Pts',(-16.6196561660671,19.3396305615062,
10.7032812243476));
#198503=CARTESIAN_POINT('Ctrl Pts',(-16.6177357545009,19.2668089887221,
10.7076629204489));
#198504=CARTESIAN_POINT('Ctrl Pts',(-16.6158175995711,19.1940729870813,
10.7120394677085));
#198505=CARTESIAN_POINT('Ctrl Pts',(-16.6176515119966,19.1211555742338,
10.7164160149681));
#198506=CARTESIAN_POINT('Ctrl Pts',(-16.6232479369201,19.0484739153123,
10.7207925622278));
#198507=CARTESIAN_POINT('Ctrl Pts',(-16.6288408126722,18.9758383500427,
10.7251663339447));
#198508=CARTESIAN_POINT('Ctrl Pts',(-16.6381914295875,18.9034387218191,
10.7295401056617));
#198509=CARTESIAN_POINT('Ctrl Pts',(-16.6512581694981,18.8316908022766,
10.7339138773787));
#198510=CARTESIAN_POINT('Ctrl Pts',(-16.6643209331558,18.7599647158668,
10.7382863181422));
#198511=CARTESIAN_POINT('Ctrl Pts',(-16.6810974883882,18.6888904187038,
10.7426587589058));
#198512=CARTESIAN_POINT('Ctrl Pts',(-16.701494753238,18.6188755013641,10.7470311996693));
#198513=CARTESIAN_POINT('Ctrl Pts',(-16.7218925396481,18.5488587937351,
10.7514037522367));
#198514=CARTESIAN_POINT('Ctrl Pts',(-16.7459110826477,18.4799019822764,
10.755776304804));
#198515=CARTESIAN_POINT('Ctrl Pts',(-16.7734073411523,18.4123978299098,
10.7601488573714));
#198516=CARTESIAN_POINT('Ctrl Pts',(-16.8009321363112,18.3448236191879,
10.7645259479387));
#198517=CARTESIAN_POINT('Ctrl Pts',(-16.8319416708364,18.2787055253263,
10.768903038506));
#198518=CARTESIAN_POINT('Ctrl Pts',(-16.8662449207624,18.2144158520314,
10.7732801290733));
#198519=CARTESIAN_POINT('Ctrl Pts',(-16.9005669049664,18.1500910677599,
10.7776596101323));
#198520=CARTESIAN_POINT('Ctrl Pts',(-16.9381859370547,18.0875971057585,
10.7820390911912));
#198521=CARTESIAN_POINT('Ctrl Pts',(-16.9788666145896,18.0272788337544,
10.7864185722502));
#198522=CARTESIAN_POINT('Ctrl Pts',(-17.0196193983523,17.9668536480182,
10.7908058159099));
#198523=CARTESIAN_POINT('Ctrl Pts',(-17.0634443742614,17.9086122391294,
10.7951930595696));
#198524=CARTESIAN_POINT('Ctrl Pts',(-17.1100650454662,17.8528673616163,
10.7995803032293));
#198525=CARTESIAN_POINT('Ctrl Pts',(-17.1417626095282,17.814966216471,10.8025632061641));
#198526=CARTESIAN_POINT('Ctrl Pts',(-17.1747517071182,17.7782184270681,
10.8055461090989));
#198527=CARTESIAN_POINT('Ctrl Pts',(-17.2089361619795,17.7427121229261,
10.8085290120338));
#198528=CARTESIAN_POINT('Ctrl Pts',(-17.259225605987,17.6904780796656,10.8129172209647));
#198529=CARTESIAN_POINT('Ctrl Pts',(-17.3122998738987,17.6407287153967,
10.8173054298956));
#198530=CARTESIAN_POINT('Ctrl Pts',(-17.3678836195123,17.5937755149754,
10.8216936388265));
#198531=CARTESIAN_POINT('Ctrl Pts',(-17.4233848696313,17.5468920008886,
10.8260753349277));
#198532=CARTESIAN_POINT('Ctrl Pts',(-17.4813878383957,17.5027967211001,
10.830457031029));
#198533=CARTESIAN_POINT('Ctrl Pts',(-17.5415797744861,17.461765022707,10.8348387271302));
#198534=CARTESIAN_POINT('Ctrl Pts',(-17.6017009802613,17.4207815398249,
10.8392152743899));
#198535=CARTESIAN_POINT('Ctrl Pts',(-17.6640056470483,17.3828547573656,
10.8435918216495));
#198536=CARTESIAN_POINT('Ctrl Pts',(-17.7281486587458,17.3482192616153,
10.8479683689091));
#198537=CARTESIAN_POINT('Ctrl Pts',(-17.7922509918775,17.313605731193,10.8523421406261));
#198538=CARTESIAN_POINT('Ctrl Pts',(-17.8581889333117,17.2822795746618,
10.8567159123431));
#198539=CARTESIAN_POINT('Ctrl Pts',(-17.9255903577758,17.2544308470287,
10.8610896840601));
#198540=CARTESIAN_POINT('Ctrl Pts',(-17.9929712717601,17.2265905938569,
10.8654621248236));
#198541=CARTESIAN_POINT('Ctrl Pts',(-18.0618143390775,17.2022258528362,
10.8698345655872));
#198542=CARTESIAN_POINT('Ctrl Pts',(-18.1317264570577,17.1814789778197,
10.8742070063507));
#198543=CARTESIAN_POINT('Ctrl Pts',(-18.2016403626988,17.1607315723032,
10.8785795589181));
#198544=CARTESIAN_POINT('Ctrl Pts',(-18.2726229102616,17.1436023517758,
10.8829521114854));
#198545=CARTESIAN_POINT('Ctrl Pts',(-18.3442664228591,17.1301836364424,
10.8873246640528));
#198546=CARTESIAN_POINT('Ctrl Pts',(-18.4159842897961,17.1167509946602,
10.8917017546201));
#198547=CARTESIAN_POINT('Ctrl Pts',(-18.4883640162146,17.1070366356522,
10.8960788451874));
#198548=CARTESIAN_POINT('Ctrl Pts',(-18.5609891559666,17.1010814594286,
10.9004559357548));
#198549=CARTESIAN_POINT('Ctrl Pts',(-18.6336539590027,17.0951230308623,
10.9048354168137));
#198550=CARTESIAN_POINT('Ctrl Pts',(-18.70656395973,17.092927887168,10.9092148978726));
#198551=CARTESIAN_POINT('Ctrl Pts',(-18.7793017600913,17.0944847625087,
10.9135943789316));
#198552=CARTESIAN_POINT('Ctrl Pts',(-18.8521684877156,17.0960443974006,
10.9179816225913));
#198553=CARTESIAN_POINT('Ctrl Pts',(-18.9248619239415,17.1013692966915,
10.922368866251));
#198554=CARTESIAN_POINT('Ctrl Pts',(-18.9969694292041,17.1103962583809,
10.9267561099107));
#198555=CARTESIAN_POINT('Ctrl Pts',(-19.04599558452,17.1165337224938,10.9297390128456));
#198556=CARTESIAN_POINT('Ctrl Pts',(-19.0947510327818,17.1243814515022,
10.9327219157804));
#198557=CARTESIAN_POINT('Ctrl Pts',(-19.1431096126277,17.1339062792316,
10.9357048187152));
#198558=CARTESIAN_POINT('Ctrl Pts',(-19.2142508990198,17.1479184462449,
10.9400930276461));
#198559=CARTESIAN_POINT('Ctrl Pts',(-19.2848103359499,17.1656171190662,
10.944481236577));
#198560=CARTESIAN_POINT('Ctrl Pts',(-19.3543769742706,17.1869393759586,
10.9488694455079));
#198561=CARTESIAN_POINT('Ctrl Pts',(-19.4238403641655,17.2082299870864,
10.9532511416092));
#198562=CARTESIAN_POINT('Ctrl Pts',(-19.4923134231172,17.2331333660321,
10.9576328377104));
#198563=CARTESIAN_POINT('Ctrl Pts',(-19.5593953414341,17.2615355785911,
10.9620145338117));
#198564=CARTESIAN_POINT('Ctrl Pts',(-19.6263984331584,17.2899044162902,
10.9663910810713));
#198565=CARTESIAN_POINT('Ctrl Pts',(-19.6920131895935,17.3217637331238,
10.970767628331));
#198566=CARTESIAN_POINT('Ctrl Pts',(-19.7558555559969,17.3569503181742,
10.9751441755906));
#198567=CARTESIAN_POINT('Ctrl Pts',(-19.8196574344994,17.3921145884038,
10.9795179473076));
#198568=CARTESIAN_POINT('Ctrl Pts',(-19.8816887317569,17.4306017078617,
10.9838917190246));
#198569=CARTESIAN_POINT('Ctrl Pts',(-19.941588217233,17.4722016512545,10.9882654907415));
#198570=CARTESIAN_POINT('Ctrl Pts',(-20.0014694750944,17.5137889356447,
10.9926379315051));
#198571=CARTESIAN_POINT('Ctrl Pts',(-20.0592198131158,17.5584868884064,
10.9970103722686));
#198572=CARTESIAN_POINT('Ctrl Pts',(-20.1145067552151,17.6060420258444,
11.0013828130322));
#198573=CARTESIAN_POINT('Ctrl Pts',(-20.1697951110076,17.6535983792726,
11.0057553655995));
#198574=CARTESIAN_POINT('Ctrl Pts',(-20.2226195814183,17.7040117463509,
11.0101279181669));
#198575=CARTESIAN_POINT('Ctrl Pts',(-20.2726818719981,17.7569893065096,
11.0145004707342));
#198576=CARTESIAN_POINT('Ctrl Pts',(-20.3227961191113,17.8100218487785,
11.0188775613015));
#198577=CARTESIAN_POINT('Ctrl Pts',(-20.3701421308266,17.8656235460727,
11.0232546518688));
#198578=CARTESIAN_POINT('Ctrl Pts',(-20.4144601023066,17.9234663714854,
11.0276317424362));
#198579=CARTESIAN_POINT('Ctrl Pts',(-20.4588022774757,17.9813407870121,
11.0320112234951));
#198580=CARTESIAN_POINT('Ctrl Pts',(-20.5001128464797,18.0414583697185,
11.036390704554));
#198581=CARTESIAN_POINT('Ctrl Pts',(-20.5381753524532,18.1034620559095,
11.040770185613));
#198582=CARTESIAN_POINT('Ctrl Pts',(-20.576305323963,18.165575643218,11.0451574292727));
#198583=CARTESIAN_POINT('Ctrl Pts',(-20.611175504632,18.2295815860898,11.0495446729324));
#198584=CARTESIAN_POINT('Ctrl Pts',(-20.6426156833706,18.2950987099081,
11.0539319165921));
#198585=CARTESIAN_POINT('Ctrl Pts',(-20.6639919753445,18.3396440408898,
11.056914819527));
#198586=CARTESIAN_POINT('Ctrl Pts',(-20.6837836766024,18.3848874840296,
11.0598977224618));
#198587=CARTESIAN_POINT('Ctrl Pts',(-20.7019503858964,18.4307050053664,
11.0628806253966));
#198588=CARTESIAN_POINT('Ctrl Pts',(-20.7321363776461,18.5068358719245,
11.0678370477142));
#198589=CARTESIAN_POINT('Ctrl Pts',(-20.7579328257801,18.5848010792849,
11.0727934700317));
#198590=CARTESIAN_POINT('Ctrl Pts',(-20.7791414399035,18.6641129085547,
11.0777498923493));
#198591=CARTESIAN_POINT('Ctrl Pts',(-20.8002681015216,18.7431182678655,
11.0826871624853));
#198592=CARTESIAN_POINT('Ctrl Pts',(-20.8168421753556,18.8234596442832,
11.0876244326214));
#198593=CARTESIAN_POINT('Ctrl Pts',(-20.8287143558564,18.904632953193,11.0925617027575));
#198594=CARTESIAN_POINT('Ctrl Pts',(-20.840509956428,18.9852826644165,11.097467125686));
#198595=CARTESIAN_POINT('Ctrl Pts',(-20.8476640072495,19.0667533747692,
11.1023725486145));
#198596=CARTESIAN_POINT('Ctrl Pts',(-20.8500781623712,19.1485323224719,
11.1072779715431));
#198597=CARTESIAN_POINT('Ctrl Pts',(-20.8506795164088,19.1689030517394,
11.1084998880048));
#198598=CARTESIAN_POINT('Ctrl Pts',(-20.8509870073137,19.1892928268125,
11.1097218044665));
#198599=CARTESIAN_POINT('Ctrl Pts',(-20.8509995968923,19.2096935705332,
11.1109437209282));
#198600=CARTESIAN_POINT('',(-20.8509995968923,19.2123064294671,10.8890562790718));
#198601=CARTESIAN_POINT('Ctrl Pts',(-20.7225805927058,19.9371103403161,
10.1325349747556));
#198602=CARTESIAN_POINT('Ctrl Pts',(-20.6722700068885,20.0748947086263,
10.1420538790795));
#198603=CARTESIAN_POINT('Ctrl Pts',(-20.6077708800263,20.2070921693553,
10.151890455237));
#198604=CARTESIAN_POINT('Ctrl Pts',(-20.4974383372554,20.3839378624421,
10.1654299576843));
#198605=CARTESIAN_POINT('Ctrl Pts',(-20.4624925057593,20.4348517776986,
10.1693726388878));
#198606=CARTESIAN_POINT('Ctrl Pts',(-20.4198757026397,20.4914669170025,
10.173746424394));
#198607=CARTESIAN_POINT('Ctrl Pts',(-20.4143358602232,20.4987281599882,
10.1743071704144));
#198608=CARTESIAN_POINT('Ctrl Pts',(-20.405991196218,20.5095202221887,10.1751399668579));
#198609=CARTESIAN_POINT('Ctrl Pts',(-20.403221888764,20.5130781906646,10.1754144254421));
#198610=CARTESIAN_POINT('Ctrl Pts',(-20.3982421237061,20.5194341281866,
10.1759044939734));
#198611=CARTESIAN_POINT('Ctrl Pts',(-20.3960359528224,20.5222353740848,
10.1761204008213));
#198612=CARTESIAN_POINT('Ctrl Pts',(-20.3912401647724,20.5282931893853,
10.1765871284904));
#198613=CARTESIAN_POINT('Ctrl Pts',(-20.3886480299972,20.5315476924542,
10.1768377652364));
#198614=CARTESIAN_POINT('Ctrl Pts',(-20.3813738080093,20.5406256504569,
10.1775366433218));
#198615=CARTESIAN_POINT('Ctrl Pts',(-20.3766704055904,20.5464320559437,
10.1779833835897));
#198616=CARTESIAN_POINT('Ctrl Pts',(-20.3490477356145,20.5801658143092,
10.1805780413002));
#198617=CARTESIAN_POINT('Ctrl Pts',(-20.3254458485314,20.6075295120245,
10.1826795773869));
#198618=CARTESIAN_POINT('Ctrl Pts',(-20.2470258197943,20.6938768565625,
10.1893509428739));
#198619=CARTESIAN_POINT('Ctrl Pts',(-20.1895377961755,20.7503448783542,
10.1937780257805));
#198620=CARTESIAN_POINT('Ctrl Pts',(-20.0272911806018,20.8924751985434,
10.205535102627));
#198621=CARTESIAN_POINT('Ctrl Pts',(-19.9173224873183,20.9715985056218,
10.2127866121133));
#198622=CARTESIAN_POINT('Ctrl Pts',(-19.7460918468844,21.0714664705331,
10.2239370092751));
#198623=CARTESIAN_POINT('Ctrl Pts',(-19.6902329837888,21.1007837892465,
10.2275506563067));
#198624=CARTESIAN_POINT('Ctrl Pts',(-19.6218463304284,21.1328672852451,
10.2319868157594));
#198625=CARTESIAN_POINT('Ctrl Pts',(-19.6104934947065,21.1380713822479,
10.2327235935239));
#198626=CARTESIAN_POINT('Ctrl Pts',(-19.5917883596035,21.1464462604983,
10.2339383599015));
#198627=CARTESIAN_POINT('Ctrl Pts',(-19.5844628406245,21.1496763657643,
10.2344143091388));
#198628=CARTESIAN_POINT('Ctrl Pts',(-19.5712677747777,21.1554054021022,
10.2352720590958));
#198629=CARTESIAN_POINT('Ctrl Pts',(-19.565404894644,21.1579195140505,10.2356533355446));
#198630=CARTESIAN_POINT('Ctrl Pts',(-19.5529028188346,21.1632138667234,
10.2364667493653));
#198631=CARTESIAN_POINT('Ctrl Pts',(-19.5462606410044,21.165986817655,10.2368991288974));
#198632=CARTESIAN_POINT('Ctrl Pts',(-19.528356405446,21.1733544137094,10.2380652907038));
#198633=CARTESIAN_POINT('Ctrl Pts',(-19.5170688042838,21.177885909746,10.2388011971044));
#198634=CARTESIAN_POINT('Ctrl Pts',(-19.4607287147891,21.1999422332628,
10.2424783379126));
#198635=CARTESIAN_POINT('Ctrl Pts',(-19.4151272682136,21.2160164281905,
10.2454677186487));
#198636=CARTESIAN_POINT('Ctrl Pts',(-19.282560450199,21.2577008790079,10.2542017717621));
#198637=CARTESIAN_POINT('Ctrl Pts',(-19.1944550767868,21.2793039049885,
10.2600638133215));
#198638=CARTESIAN_POINT('Ctrl Pts',(-18.9466759619437,21.323439323219,10.2765860700516));
#198639=CARTESIAN_POINT('Ctrl Pts',(-18.7853982408565,21.3334969258075,
10.2874121703723));
#198640=CARTESIAN_POINT('Ctrl Pts',(-18.6045529745864,21.3241334235593,
10.2987722432675));
#198641=CARTESIAN_POINT('Ctrl Pts',(-18.5845846127825,21.3228154529584,
10.3000151640786));
#198642=CARTESIAN_POINT('Ctrl Pts',(-18.5582752748694,21.3207039021706,
10.3016350769499));
#198643=CARTESIAN_POINT('Ctrl Pts',(-18.5519156706789,21.3201645344263,
10.3020252822205));
#198644=CARTESIAN_POINT('Ctrl Pts',(-18.5416547912929,21.3192475379835,
10.3026525440244));
#198645=CARTESIAN_POINT('Ctrl Pts',(-18.5377520124521,21.3188878264005,
10.3028905856347));
#198646=CARTESIAN_POINT('Ctrl Pts',(-18.5302461106706,21.3181749949476,
10.3033473220732));
#198647=CARTESIAN_POINT('Ctrl Pts',(-18.5266428913036,21.3178234706212,
10.3035661008765));
#198648=CARTESIAN_POINT('Ctrl Pts',(-18.5181207875851,21.3169699932925,
10.3040824415807));
#198649=CARTESIAN_POINT('Ctrl Pts',(-18.5132026915968,21.3164600439652,
10.3043795545946));
#198650=CARTESIAN_POINT('Ctrl Pts',(-18.4968956579324,21.3147114277419,
10.3053619562062));
#198651=CARTESIAN_POINT('Ctrl Pts',(-18.485514762443,21.3133975218965,10.3060431477741));
#198652=CARTESIAN_POINT('Ctrl Pts',(-18.4583813967461,21.3100416079543,
10.3076577749112));
#198653=CARTESIAN_POINT('Ctrl Pts',(-18.4426399379007,21.3079145503646,
10.3085869153626));
#198654=CARTESIAN_POINT('Ctrl Pts',(-18.3847298137794,21.2994247416996,
10.3119819533344));
#198655=CARTESIAN_POINT('Ctrl Pts',(-18.3427300801996,21.2919651269961,
10.3143990293684));
#198656=CARTESIAN_POINT('Ctrl Pts',(-18.1521714016529,21.2521457566835,
10.3252730197185));
#198657=CARTESIAN_POINT('Ctrl Pts',(-18.0071385216096,21.2051107556225,
10.3333207048918));
#198658=CARTESIAN_POINT('Ctrl Pts',(-17.7812050228889,21.1038807677603,
10.3469912183704));
#198659=CARTESIAN_POINT('Ctrl Pts',(-17.6967756912564,21.0589659910465,
10.3523802563669));
#198660=CARTESIAN_POINT('Ctrl Pts',(-17.6039048668715,21.0011860524091,
10.3587916159442));
#198661=CARTESIAN_POINT('Ctrl Pts',(-17.5922086031033,20.9937488618731,
10.3596081753665));
#198662=CARTESIAN_POINT('Ctrl Pts',(-17.573601717547,20.9816592579012,10.360922257278));
#198663=CARTESIAN_POINT('Ctrl Pts',(-17.5666439412484,20.9770798992629,
10.3614170590713));
#198664=CARTESIAN_POINT('Ctrl Pts',(-17.5543575432001,20.968889105883,10.3622969749089));
#198665=CARTESIAN_POINT('Ctrl Pts',(-17.5490179991131,20.9652941858845,
10.3626814638666));
#198666=CARTESIAN_POINT('Ctrl Pts',(-17.5379462395731,20.957766363201,10.3634831108117));
#198667=CARTESIAN_POINT('Ctrl Pts',(-17.5322168420308,20.9538294709666,
10.3639004172791));
#198668=CARTESIAN_POINT('Ctrl Pts',(-17.5174292233435,20.9435607315022,
10.3649839676944));
#198669=CARTESIAN_POINT('Ctrl Pts',(-17.5084010956056,20.9371861027277,
10.3656518422405));
#198670=CARTESIAN_POINT('Ctrl Pts',(-17.4697850913289,20.90946424837,10.3685363102943));
#198671=CARTESIAN_POINT('Ctrl Pts',(-17.4407033050697,20.8874258221909,
10.3707795165235));
#198672=CARTESIAN_POINT('Ctrl Pts',(-17.3653248046872,20.8271743133028,
10.3767886303896));
#198673=CARTESIAN_POINT('Ctrl Pts',(-17.3200613581114,20.787726887068,10.3806012202841));
#198674=CARTESIAN_POINT('Ctrl Pts',(-17.1553520348191,20.6313796017348,
10.3952543022437));
#198675=CARTESIAN_POINT('Ctrl Pts',(-17.0482235207344,20.5024171305579,
10.4065010679343));
#198676=CARTESIAN_POINT('Ctrl Pts',(-16.9463728577249,20.3452342862648,
10.4186131048079));
#198677=CARTESIAN_POINT('Ctrl Pts',(-16.9356159839769,20.3281003508967,
10.4199133111844));
#198678=CARTESIAN_POINT('Ctrl Pts',(-16.906553162828,20.2802999568463,10.4234804164344));
#198679=CARTESIAN_POINT('Ctrl Pts',(-16.8887740686995,20.2493188094764,
10.4257251613407));
#198680=CARTESIAN_POINT('Ctrl Pts',(-16.868421535263,20.2116777888174,10.428359848409));
#198681=CARTESIAN_POINT('Ctrl Pts',(-16.8650879914422,20.2054380084342,
10.4287936100046));
#198682=CARTESIAN_POINT('Ctrl Pts',(-16.8596890920909,20.1952092235228,
10.4294996437514));
#198683=CARTESIAN_POINT('Ctrl Pts',(-16.8576050739897,20.1912302064707,
10.4297730563891));
#198684=CARTESIAN_POINT('Ctrl Pts',(-16.8538899700927,20.1840816928529,
10.430262002301));
#198685=CARTESIAN_POINT('Ctrl Pts',(-16.8522542177986,20.1809146958789,
10.4304778266448));
#198686=CARTESIAN_POINT('Ctrl Pts',(-16.848720678445,20.1740307865896,10.430945227638));
#198687=CARTESIAN_POINT('Ctrl Pts',(-16.8468258868471,20.1703124014303,
10.4311966156227));
#198688=CARTESIAN_POINT('Ctrl Pts',(-16.8415429403344,20.1598687921114,
10.4318997135726));
#198689=CARTESIAN_POINT('Ctrl Pts',(-16.8381796162148,20.1531309800705,
10.4323498930077));
#198690=CARTESIAN_POINT('Ctrl Pts',(-16.8184564931481,20.1130859558023,
10.4350060078636));
#198691=CARTESIAN_POINT('Ctrl Pts',(-16.8029376883378,20.0793690030319,
10.4371629580768));
#198692=CARTESIAN_POINT('Ctrl Pts',(-16.7551226905858,19.9678532451521,
10.444095560181));
#198693=CARTESIAN_POINT('Ctrl Pts',(-16.7265791073742,19.8885292138496,
10.4487153085571));
#198694=CARTESIAN_POINT('Ctrl Pts',(-16.652240803465,19.6354862292233,10.4630752647893));
#198695=CARTESIAN_POINT('Ctrl Pts',(-16.6237589320657,19.457548301185,10.4727058102398));
#198696=CARTESIAN_POINT('Ctrl Pts',(-16.6173461289145,19.2554918041819,
10.4844566424849));
#198697=CARTESIAN_POINT('Ctrl Pts',(-16.6169910278957,19.2328193531069,
10.4857853182322));
#198698=CARTESIAN_POINT('Ctrl Pts',(-16.6170040011973,19.2006521637118,
10.4876864661778));
#198699=CARTESIAN_POINT('Ctrl Pts',(-16.6170716964181,19.1911583848314,
10.488249548472));
#198700=CARTESIAN_POINT('Ctrl Pts',(-16.6172857986382,19.1757086291063,
10.489169223374));
#198701=CARTESIAN_POINT('Ctrl Pts',(-16.6173934925153,19.1697521823283,
10.4895245996546));
#198702=CARTESIAN_POINT('Ctrl Pts',(-16.6176719965794,19.1572648832638,
10.4902713500743));
#198703=CARTESIAN_POINT('Ctrl Pts',(-16.6178478989413,19.1507342175656,
10.490662880035));
#198704=CARTESIAN_POINT('Ctrl Pts',(-16.6183394476929,19.1351629437227,
10.4915988261956));
#198705=CARTESIAN_POINT('Ctrl Pts',(-16.6186828158395,19.1261233947551,
10.4921441058168));
#198706=CARTESIAN_POINT('Ctrl Pts',(-16.6200426342039,19.0955005407325,
10.4939980398286));
#198707=CARTESIAN_POINT('Ctrl Pts',(-16.621331551719,19.0739312478338,10.4953151913678));
#198708=CARTESIAN_POINT('Ctrl Pts',(-16.6302341083521,18.9554439302184,
10.5026154383313));
#198709=CARTESIAN_POINT('Ctrl Pts',(-16.6441856191071,18.8591318388708,
10.5087958059423));
#198710=CARTESIAN_POINT('Ctrl Pts',(-16.6897931054439,18.6479397843144,
10.5228491338026));
#198711=CARTESIAN_POINT('Ctrl Pts',(-16.7246257532691,18.5340719590099,
10.5307724833707));
#198712=CARTESIAN_POINT('Ctrl Pts',(-16.780172889355,18.3954146033851,10.5405693270477));
#198713=CARTESIAN_POINT('Ctrl Pts',(-16.7921305131261,18.3673395680752,
10.5425599972482));
#198714=CARTESIAN_POINT('Ctrl Pts',(-16.8269256299967,18.2903080193825,
10.5480251827271));
#198715=CARTESIAN_POINT('Ctrl Pts',(-16.8510379405187,18.2419482316065,
10.551460127144));
#198716=CARTESIAN_POINT('Ctrl Pts',(-16.8811748334136,18.1868884918671,
10.5553323094483));
#198717=CARTESIAN_POINT('Ctrl Pts',(-16.8854212788035,18.1792431504343,
10.5558690833038));
#198718=CARTESIAN_POINT('Ctrl Pts',(-16.8919188084727,18.1677138306035,
10.5566769275715));
#198719=CARTESIAN_POINT('Ctrl Pts',(-16.8941350092539,18.1638104449919,
10.5569501494967));
#198720=CARTESIAN_POINT('Ctrl Pts',(-16.8981332843079,18.1568201736699,
10.5574388913103));
#198721=CARTESIAN_POINT('Ctrl Pts',(-16.8999107469432,18.153730726618,10.5576547012042));
#198722=CARTESIAN_POINT('Ctrl Pts',(-16.9037875130085,18.147031631927,10.5581222276757));
#198723=CARTESIAN_POINT('Ctrl Pts',(-16.905889689162,18.143423713312,10.5583737547417));
#198724=CARTESIAN_POINT('Ctrl Pts',(-16.9118183201517,18.1333173956787,
10.5590776348027));
#198725=CARTESIAN_POINT('Ctrl Pts',(-16.9156688871746,18.1268331133806,
10.5595284517789));
#198726=CARTESIAN_POINT('Ctrl Pts',(-16.9387666874942,18.088406068743,10.5621961689107));
#198727=CARTESIAN_POINT('Ctrl Pts',(-16.9588218820822,18.0569537208418,
10.5643635838444));
#198728=CARTESIAN_POINT('Ctrl Pts',(-17.0272410746549,17.9556604896947,
10.5713463289452));
#198729=CARTESIAN_POINT('Ctrl Pts',(-17.0789799731119,17.8881945334714,
10.5760031617327));
#198730=CARTESIAN_POINT('Ctrl Pts',(-17.2515555507291,17.6891936876925,
10.5903425370995));
#198731=CARTESIAN_POINT('Ctrl Pts',(-17.3850369160179,17.5697114664087,
10.599922140173));
#198732=CARTESIAN_POINT('Ctrl Pts',(-17.5506555430493,17.4554650386797,
10.6116163000165));
#198733=CARTESIAN_POINT('Ctrl Pts',(-17.5695986876368,17.4428437204718,
10.6129500225172));
#198734=CARTESIAN_POINT('Ctrl Pts',(-17.5967380789285,17.4253867345281,
10.6148571440337));
#198735=CARTESIAN_POINT('Ctrl Pts',(-17.60476948835,17.4202968258187,10.6154210712554));
#198736=CARTESIAN_POINT('Ctrl Pts',(-17.6178904033551,17.4121048139558,
10.6163417468393));
#198737=CARTESIAN_POINT('Ctrl Pts',(-17.6229592570245,17.4089697592922,
10.6166972734818));
#198738=CARTESIAN_POINT('Ctrl Pts',(-17.6336098992516,17.4024444227025,
10.6174440290005));
#198739=CARTESIAN_POINT('Ctrl Pts',(-17.6391942645076,17.3990584860299,
10.6178354123248));
#198740=CARTESIAN_POINT('Ctrl Pts',(-17.6525400345069,17.3910508407939,
10.6187704304607));
#198741=CARTESIAN_POINT('Ctrl Pts',(-17.6603154816009,17.3864528917959,
10.6193149242252));
#198742=CARTESIAN_POINT('Ctrl Pts',(-17.6867224743011,17.3710645805184,
10.6211634016877));
#198743=CARTESIAN_POINT('Ctrl Pts',(-17.7054886494271,17.360509007938,10.6224758148469));
#198744=CARTESIAN_POINT('Ctrl Pts',(-17.8832637637862,17.2640539088817,
10.6349012482034));
#198745=CARTESIAN_POINT('Ctrl Pts',(-18.052469355787,17.1985782316151,10.6467698980266));
#198746=CARTESIAN_POINT('Ctrl Pts',(-18.2356545022221,17.1534760584398,
10.6592326475943));
#198747=CARTESIAN_POINT('Ctrl Pts',(-18.2434336302385,17.1516074578773,
10.6597610031951));
#198748=CARTESIAN_POINT('Ctrl Pts',(-18.309188922122,17.1362062988076,10.6642188771182));
#198749=CARTESIAN_POINT('Ctrl Pts',(-18.3677041653715,17.1250802210653,
10.668133044275));
#198750=CARTESIAN_POINT('Ctrl Pts',(-18.4787586326482,17.1087824571137,
10.6753842595395));
#198751=CARTESIAN_POINT('Ctrl Pts',(-18.5311770082509,17.1030790832728,
10.6787333620628));
#198752=CARTESIAN_POINT('Ctrl Pts',(-18.5924273327954,17.0987212026948,
10.6825210895039));
#198753=CARTESIAN_POINT('Ctrl Pts',(-18.6011005454764,17.0981577724346,
10.6830545093525));
#198754=CARTESIAN_POINT('Ctrl Pts',(-18.6142463991786,17.097385059127,10.6838583131789));
#198755=CARTESIAN_POINT('Ctrl Pts',(-18.6187165169945,17.0971365317057,
10.6841308173092));
#198756=CARTESIAN_POINT('Ctrl Pts',(-18.6267460610666,17.0967156550779,
10.6846187926298));
#198757=CARTESIAN_POINT('Ctrl Pts',(-18.6303051474642,17.0965381117797,
10.6848345498182));
#198758=CARTESIAN_POINT('Ctrl Pts',(-18.6380446201953,17.0961716203004,
10.6853025562256));
#198759=CARTESIAN_POINT('Ctrl Pts',(-18.6422251101187,17.0959860802398,
10.6855546127155));
#198760=CARTESIAN_POINT('Ctrl Pts',(-18.6539820310099,17.0954992042487,
10.6862614724676));
#198761=CARTESIAN_POINT('Ctrl Pts',(-18.6615596585811,17.0952261715717,
10.6867147187176));
#198762=CARTESIAN_POINT('Ctrl Pts',(-18.7071304135825,17.0938293053316,
10.6894272656464));
#198763=CARTESIAN_POINT('Ctrl Pts',(-18.7451492822725,17.0936880665798,
10.6916351238748));
#198764=CARTESIAN_POINT('Ctrl Pts',(-18.8708799898052,17.0966081520467,
10.6988141803918));
#198765=CARTESIAN_POINT('Ctrl Pts',(-18.9584018316481,17.1040981807423,
10.7036165147389));
#198766=CARTESIAN_POINT('Ctrl Pts',(-19.2177353966039,17.1426405451631,
10.7178796716451));
#198767=CARTESIAN_POINT('Ctrl Pts',(-19.3864078837211,17.1894985842783,
10.7272618008282));
#198768=CARTESIAN_POINT('Ctrl Pts',(-19.5687178602881,17.2653722641146,
10.7387355062578));
#198769=CARTESIAN_POINT('Ctrl Pts',(-19.589869326526,17.2745835088188,10.7400869644461));
#198770=CARTESIAN_POINT('Ctrl Pts',(-19.6195659215021,17.2880976692996,
10.7420150709314));
#198771=CARTESIAN_POINT('Ctrl Pts',(-19.6282393648511,17.2921158637025,
10.7425819568808));
#198772=CARTESIAN_POINT('Ctrl Pts',(-19.6422842675964,17.2987384278177,
10.7435061392012));
#198773=CARTESIAN_POINT('Ctrl Pts',(-19.6476725097027,17.3013070469057,
10.7438621949091));
#198774=CARTESIAN_POINT('Ctrl Pts',(-19.6588079452328,17.3066733155458,
10.7446011689023));
#198775=CARTESIAN_POINT('Ctrl Pts',(-19.6645534694456,17.3094742715908,
10.7449841995308));
#198776=CARTESIAN_POINT('Ctrl Pts',(-19.6780797279655,17.3161443388437,
10.7458901059798));
#198777=CARTESIAN_POINT('Ctrl Pts',(-19.6858494548944,17.320035399308,10.7464137458434));
#198778=CARTESIAN_POINT('Ctrl Pts',(-19.7022696337834,17.3283854280613,
10.7475274206143));
#198779=CARTESIAN_POINT('Ctrl Pts',(-19.7109137135204,17.3328564214751,
10.7481178706126));
#198780=CARTESIAN_POINT('Ctrl Pts',(-19.7342780068654,17.3451461146347,
10.7497253096375));
#198781=CARTESIAN_POINT('Ctrl Pts',(-19.7489369729805,17.3530791920708,
10.7507463139337));
#198782=CARTESIAN_POINT('Ctrl Pts',(-19.7944990681235,17.3784364195429,
10.7539595370732));
#198783=CARTESIAN_POINT('Ctrl Pts',(-19.8250576274806,17.3964640893429,
10.7561727821335));
#198784=CARTESIAN_POINT('Ctrl Pts',(-19.9432250861952,17.4702400403586,
10.7649637045216));
#198785=CARTESIAN_POINT('Ctrl Pts',(-20.0271281137687,17.5316293211403,
10.7717300905263));
#198786=CARTESIAN_POINT('Ctrl Pts',(-20.2183047072959,17.6943561393415,
10.7882834518899));
#198787=CARTESIAN_POINT('Ctrl Pts',(-20.3201729473132,17.8012373385352,
10.7981192223337));
#198788=CARTESIAN_POINT('Ctrl Pts',(-20.4195999587139,17.9301088253,10.8082704714047));
#198789=CARTESIAN_POINT('Ctrl Pts',(-20.4289366735445,17.9424894060122,
10.8092296568668));
#198790=CARTESIAN_POINT('Ctrl Pts',(-20.4415555985968,17.9596103399693,
10.8105330107739));
#198791=CARTESIAN_POINT('Ctrl Pts',(-20.4449554683245,17.9642628221124,
10.8108848812677));
#198792=CARTESIAN_POINT('Ctrl Pts',(-20.4503344450374,17.9716870166139,
10.8114426432439));
#198793=CARTESIAN_POINT('Ctrl Pts',(-20.4523259040171,17.9744496832011,
10.8116493782275));
#198794=CARTESIAN_POINT('Ctrl Pts',(-20.4564306277032,17.9801730567957,
10.8120759591988));
#198795=CARTESIAN_POINT('Ctrl Pts',(-20.4585429301364,17.9831344073394,
10.8122957338488));
#198796=CARTESIAN_POINT('Ctrl Pts',(-20.46356691152,17.9902163356042,10.8128190985874));
#198797=CARTESIAN_POINT('Ctrl Pts',(-20.4664715352662,17.9943419390099,
10.8131222051367));
#198798=CARTESIAN_POINT('Ctrl Pts',(-20.4762589505169,18.0083496864062,
10.8141454751634));
#198799=CARTESIAN_POINT('Ctrl Pts',(-20.4830723057312,18.018280371614,10.8148610591661));
#198800=CARTESIAN_POINT('Ctrl Pts',(-20.4992636167786,18.0423168715611,
10.8165708966984));
#198801=CARTESIAN_POINT('Ctrl Pts',(-20.5085578820493,18.0564783450655,
10.8175601478));
#198802=CARTESIAN_POINT('Ctrl Pts',(-20.5429253103041,18.1102389772883,
10.8212539188106));
#198803=CARTESIAN_POINT('Ctrl Pts',(-20.5668525036089,18.1505576994599,
10.8238998568287));
#198804=CARTESIAN_POINT('Ctrl Pts',(-20.6721509071704,18.3422201706049,
10.836064728062));
#198805=CARTESIAN_POINT('Ctrl Pts',(-20.7362418679452,18.502311299053,10.8451123316752));
#198806=CARTESIAN_POINT('Ctrl Pts',(-20.79061455188,18.7073623913048,10.8569815544184));
#198807=CARTESIAN_POINT('Ctrl Pts',(-20.7998318264488,18.7466156141736,
10.8592625952486));
#198808=CARTESIAN_POINT('Ctrl Pts',(-20.8091426817149,18.7920622836997,
10.8619253734846));
#198809=CARTESIAN_POINT('Ctrl Pts',(-20.8103371897353,18.7980232051254,
10.8622750551767));
#198810=CARTESIAN_POINT('Ctrl Pts',(-20.8121465851799,18.8072589045349,
10.8628175437125));
#198811=CARTESIAN_POINT('Ctrl Pts',(-20.8127794509336,18.8105301561102,
10.863009827016));
#198812=CARTESIAN_POINT('Ctrl Pts',(-20.8188276065779,18.8421934331642,
10.8648723442165));
#198813=CARTESIAN_POINT('Ctrl Pts',(-20.8236684171136,18.8706909928592,
10.8665592676138));
#198814=CARTESIAN_POINT('Ctrl Pts',(-20.8294676985616,18.9096463622397,
10.8688832028828));
#198815=CARTESIAN_POINT('Ctrl Pts',(-20.8309342153355,18.920026150191,10.8695041441686));
#198816=CARTESIAN_POINT('Ctrl Pts',(-20.8331379327419,18.936506478661,10.8704929165883));
#198817=CARTESIAN_POINT('Ctrl Pts',(-20.8339257794662,18.9426001612473,
10.8708591438151));
#198818=CARTESIAN_POINT('Ctrl Pts',(-20.8354516394795,18.9548202125136,
10.8715948477674));
#198819=CARTESIAN_POINT('Ctrl Pts',(-20.8361894175088,18.9609465492099,
10.8719643280663));
#198820=CARTESIAN_POINT('Ctrl Pts',(-20.8376163916313,18.9732486766209,
10.8727076006313));
#198821=CARTESIAN_POINT('Ctrl Pts',(-20.8383052008012,18.9794244496828,
10.8730814012146));
#198822=CARTESIAN_POINT('Ctrl Pts',(-20.839817318438,18.9935460176408,10.8739377045565));
#198823=CARTESIAN_POINT('Ctrl Pts',(-20.8406228594342,19.0014935837608,
10.8744207624356));
#198824=CARTESIAN_POINT('Ctrl Pts',(-20.8425678109941,19.0218293107162,
10.8756597488149));
#198825=CARTESIAN_POINT('Ctrl Pts',(-20.8436430281949,19.034223173295,10.8764176797));
#198826=CARTESIAN_POINT('Ctrl Pts',(-20.8489047513554,19.1017850267102,
10.8805651162004));
#198827=CARTESIAN_POINT('Ctrl Pts',(-20.8510362031063,19.1570864420282,
10.8840180047431));
#198828=CARTESIAN_POINT('Ctrl Pts',(-20.8509995348906,19.2124033079146,
10.8875306396154));
#198829=CARTESIAN_POINT('Ctrl Pts',(-20.7225806064498,19.9371103026755,
10.9336112484111));
#198830=CARTESIAN_POINT('Ctrl Pts',(-20.7506609592852,19.8602073240716,
10.9286590708807));
#198831=CARTESIAN_POINT('Ctrl Pts',(-20.7743084251627,19.7815858993868,
10.9237068933503));
#198832=CARTESIAN_POINT('Ctrl Pts',(-20.7933361082647,19.7017380087145,
10.9187547158199));
#198833=CARTESIAN_POINT('Ctrl Pts',(-20.8123544235949,19.6219294290199,
10.9138049763619));
#198834=CARTESIAN_POINT('Ctrl Pts',(-20.826757334099,19.5408958015685,10.9088552369039));
#198835=CARTESIAN_POINT('Ctrl Pts',(-20.8364059223804,19.4591498288124,
10.9039054974458));
#198836=CARTESIAN_POINT('Ctrl Pts',(-20.8460545106619,19.3774038560563,
10.8989557579878));
#198837=CARTESIAN_POINT('Ctrl Pts',(-20.8509485990248,19.2949457663871,
10.8940060185298));
#198838=CARTESIAN_POINT('Ctrl Pts',(-20.8509995968923,19.2123064294671,
10.8890562790718));
#198839=CARTESIAN_POINT('Origin',(-18.734,19.211,0.));
#198840=CARTESIAN_POINT('',(-20.7225806064515,19.9371103026709,11.953538761502));
#198841=CARTESIAN_POINT('',(-20.72197304927,19.9368789336484,11.7337477349807));
#198842=CARTESIAN_POINT('',(-20.7225806064498,19.9371103026755,0.));
#198843=CARTESIAN_POINT('Ctrl Pts',(-20.7225806064515,19.9371103026709,
11.953538761502));
#198844=CARTESIAN_POINT('Ctrl Pts',(-20.7228709525551,19.9363151388665,
11.9534866621657));
#198845=CARTESIAN_POINT('Ctrl Pts',(-20.7231608231142,19.9355197970987,
11.9534345886039));
#198846=CARTESIAN_POINT('Ctrl Pts',(-20.7259025051468,19.9279831701196,
11.9529414976273));
#198847=CARTESIAN_POINT('Ctrl Pts',(-20.7283205545219,19.9212295301179,
11.9525023320917));
#198848=CARTESIAN_POINT('Ctrl Pts',(-20.7320650319312,19.9106012420015,
11.9518155886252));
#198849=CARTESIAN_POINT('Ctrl Pts',(-20.7334145988461,19.9067348864431,
11.9515666716498));
#198850=CARTESIAN_POINT('Ctrl Pts',(-20.7359210084883,19.8994867825828,
11.9511017653232));
#198851=CARTESIAN_POINT('Ctrl Pts',(-20.7370804930927,19.8961060592543,
11.9508856259623));
#198852=CARTESIAN_POINT('Ctrl Pts',(-20.7397139286616,19.8883638832195,
11.9503922431821));
#198853=CARTESIAN_POINT('Ctrl Pts',(-20.7411822154934,19.8840005561975,
11.950115336451));
#198854=CARTESIAN_POINT('Ctrl Pts',(-20.7456726560905,19.8705108397258,
11.9492627060604));
#198855=CARTESIAN_POINT('Ctrl Pts',(-20.7486469344233,19.8613684805354,
11.9486897318306));
#198856=CARTESIAN_POINT('Ctrl Pts',(-20.7774526028783,19.7707312530957,
11.9430544926844));
#198857=CARTESIAN_POINT('Ctrl Pts',(-20.7983905369682,19.6877524261686,
11.9382547693229));
#198858=CARTESIAN_POINT('Ctrl Pts',(-20.8385991823417,19.4747685882942,
11.9263203898874));
#198859=CARTESIAN_POINT('Ctrl Pts',(-20.8509009165884,19.3438277118629,
11.9193213392548));
#198860=CARTESIAN_POINT('Ctrl Pts',(-20.8510686215101,19.1203529362414,
11.9069620458454));
#198861=CARTESIAN_POINT('Ctrl Pts',(-20.8451100150514,19.0282216712388,
11.9017508425771));
#198862=CARTESIAN_POINT('Ctrl Pts',(-20.8313804908501,18.9231219331247,
11.8955371850017));
#198863=CARTESIAN_POINT('Ctrl Pts',(-20.8294631853462,18.9094826202811,
11.8947256882788));
#198864=CARTESIAN_POINT('Ctrl Pts',(-20.8261768233257,18.8876517413073,
11.8934182092873));
#198865=CARTESIAN_POINT('Ctrl Pts',(-20.8248923985681,18.8794476948169,
11.8929249039477));
#198866=CARTESIAN_POINT('Ctrl Pts',(-20.8225273356177,18.8649018162163,
11.8920467125576));
#198867=CARTESIAN_POINT('Ctrl Pts',(-20.8214659898609,18.8585569206174,
11.8916624432684));
#198868=CARTESIAN_POINT('Ctrl Pts',(-20.8191956392982,18.8453544986756,
11.8908603098725));
#198869=CARTESIAN_POINT('Ctrl Pts',(-20.8179816887819,18.8384979116754,
11.8904422925955));
#198870=CARTESIAN_POINT('Ctrl Pts',(-20.814744117171,18.8207228862841,11.8893548402678));
#198871=CARTESIAN_POINT('Ctrl Pts',(-20.8126683967876,18.8098142631284,
11.8886837524485));
#198872=CARTESIAN_POINT('Ctrl Pts',(-20.8033102350445,18.7626573701317,
11.8857662782635));
#198873=CARTESIAN_POINT('Ctrl Pts',(-20.7951650787619,18.7265888003379,
11.8834925177482));
#198874=CARTESIAN_POINT('Ctrl Pts',(-20.7710540793184,18.6314844222602,
11.8773804719579));
#198875=CARTESIAN_POINT('Ctrl Pts',(-20.7534685897906,18.5728987972974,
11.8734934958043));
#198876=CARTESIAN_POINT('Ctrl Pts',(-20.6816192585597,18.3664522857742,
11.8593775111725));
#198877=CARTESIAN_POINT('Ctrl Pts',(-20.6134417266214,18.2239972898535,
11.8488054516846));
#198878=CARTESIAN_POINT('Ctrl Pts',(-20.4974382960959,18.0380620774467,
11.8345700453692));
#198879=CARTESIAN_POINT('Ctrl Pts',(-20.4624924823144,17.9871481908861,
11.8306273663894));
#198880=CARTESIAN_POINT('Ctrl Pts',(-20.4198756999732,17.9305330794949,
11.8262535830398));
#198881=CARTESIAN_POINT('Ctrl Pts',(-20.4143358582464,17.9232718374406,
11.8256928370914));
#198882=CARTESIAN_POINT('Ctrl Pts',(-20.4059911951109,17.9124797763867,
11.8248600407364));
#198883=CARTESIAN_POINT('Ctrl Pts',(-20.4032218878214,17.9089218081279,
11.824585582169));
#198884=CARTESIAN_POINT('Ctrl Pts',(-20.3982421229723,17.9025658708802,
11.8240955136588));
#198885=CARTESIAN_POINT('Ctrl Pts',(-20.396035952132,17.8997646250404,11.8238796068155));
#198886=CARTESIAN_POINT('Ctrl Pts',(-20.3912401640744,17.8937068097363,
11.8234128791462));
#198887=CARTESIAN_POINT('Ctrl Pts',(-20.3886480292473,17.8904523066059,
11.8231622423955));
#198888=CARTESIAN_POINT('Ctrl Pts',(-20.3813738068635,17.8813743481205,
11.822463364273));
#198889=CARTESIAN_POINT('Ctrl Pts',(-20.3766704040939,17.8755679422125,
11.8220166239727));
#198890=CARTESIAN_POINT('Ctrl Pts',(-20.3490477271098,17.8418341753833,
11.8194219656118));
#198891=CARTESIAN_POINT('Ctrl Pts',(-20.3254458329638,17.8144704699649,
11.8173204289346));
#198892=CARTESIAN_POINT('Ctrl Pts',(-20.2470257693653,17.7281230898476,
11.8106490606755));
#198893=CARTESIAN_POINT('Ctrl Pts',(-20.1895377151286,17.6716550429534,
11.8062219757253));
#198894=CARTESIAN_POINT('Ctrl Pts',(-20.027291082339,17.5295247282931,11.794464898527));
#198895=CARTESIAN_POINT('Ctrl Pts',(-19.9173224095994,17.4504014444491,
11.7872133905136));
#198896=CARTESIAN_POINT('Ctrl Pts',(-19.7460918076039,17.3505335087033,
11.7760629959117));
#198897=CARTESIAN_POINT('Ctrl Pts',(-19.6902329598429,17.3212161992322,
11.7724493498698));
#198898=CARTESIAN_POINT('Ctrl Pts',(-19.621846323873,17.2891327117363,11.7680131915447));
#198899=CARTESIAN_POINT('Ctrl Pts',(-19.6104934895084,17.2839286153976,
11.7672764138682));
#198900=CARTESIAN_POINT('Ctrl Pts',(-19.5917883562531,17.2755537380189,
11.7660616476105));
#198901=CARTESIAN_POINT('Ctrl Pts',(-19.5844628377545,17.2723236329788,
11.7655856984044));
#198902=CARTESIAN_POINT('Ctrl Pts',(-19.571267772515,17.266594596924,11.7647279484868));
#198903=CARTESIAN_POINT('Ctrl Pts',(-19.5654048925079,17.2640804850378,
11.7643466720462));
#198904=CARTESIAN_POINT('Ctrl Pts',(-19.5529028166928,17.2587861323776,
11.763533258225));
#198905=CARTESIAN_POINT('Ctrl Pts',(-19.5462606387296,17.2560131813993,
11.7631008786842));
#198906=CARTESIAN_POINT('Ctrl Pts',(-19.5283564021436,17.2486455849479,
11.7619347168106));
#198907=CARTESIAN_POINT('Ctrl Pts',(-19.5170688000802,17.2441140885745,
11.7611988103511));
#198908=CARTESIAN_POINT('Ctrl Pts',(-19.4607286971292,17.2220577599582,
11.7575216686631));
#198909=CARTESIAN_POINT('Ctrl Pts',(-19.4151272376851,17.205983561115,11.7545322870777));
#198910=CARTESIAN_POINT('Ctrl Pts',(-19.282560368219,17.1642990972677,11.7457982305456));
#198911=CARTESIAN_POINT('Ctrl Pts',(-19.1944549551949,17.1426960662093,
11.739936186302));
#198912=CARTESIAN_POINT('Ctrl Pts',(-18.9466754574159,17.0985605996105,
11.7234139040057));
#198913=CARTESIAN_POINT('Ctrl Pts',(-18.7853973843949,17.0885030271862,
11.71258777986));
#198914=CARTESIAN_POINT('Ctrl Pts',(-18.6045520986102,17.0978666331439,
11.7012277098679));
#198915=CARTESIAN_POINT('Ctrl Pts',(-18.5845840578884,17.0991845893463,
11.6999848093547));
#198916=CARTESIAN_POINT('Ctrl Pts',(-18.5582750803121,17.1012961141556,
11.6983649188088));
#198917=CARTESIAN_POINT('Ctrl Pts',(-18.551915515977,17.10183547905,11.6979747160094));
#198918=CARTESIAN_POINT('Ctrl Pts',(-18.5416546853507,17.1027524716987,
11.6973474572141));
#198919=CARTESIAN_POINT('Ctrl Pts',(-18.5377519154395,17.1031121826482,
11.6971094161579));
#198920=CARTESIAN_POINT('Ctrl Pts',(-18.5302460191488,17.1038250138962,
11.6966526800697));
#198921=CARTESIAN_POINT('Ctrl Pts',(-18.526642796348,17.1041765387186,11.6964339010661));
#198922=CARTESIAN_POINT('Ctrl Pts',(-18.5181206678648,17.1050300189295,
11.6959175588815));
#198923=CARTESIAN_POINT('Ctrl Pts',(-18.5132025505647,17.1055399707743,
11.6956204445952));
#198924=CARTESIAN_POINT('Ctrl Pts',(-18.4968953736618,17.1072886036292,
11.6946380344148));
#198925=CARTESIAN_POINT('Ctrl Pts',(-18.4855143564462,17.1086025254199,
11.6939568356486));
#198926=CARTESIAN_POINT('Ctrl Pts',(-18.4045622378447,17.1186148809229,
11.6891396129952));
#198927=CARTESIAN_POINT('Ctrl Pts',(-18.3354431371683,17.1306732948523,
11.6851738507996));
#198928=CARTESIAN_POINT('Ctrl Pts',(-18.1364691604697,17.1756701737503,
11.6738643124207));
#198929=CARTESIAN_POINT('Ctrl Pts',(-18.0089876523703,17.217518084213,11.6667362053494));
#198930=CARTESIAN_POINT('Ctrl Pts',(-17.7930239356027,17.31189053747,11.6537590749683));
#198931=CARTESIAN_POINT('Ctrl Pts',(-17.7028124307309,17.3593247980837,
11.6480338559666));
#198932=CARTESIAN_POINT('Ctrl Pts',(-17.6044694274327,17.4204565056723,
11.6412477181595));
#198933=CARTESIAN_POINT('Ctrl Pts',(-17.5926436740793,17.4279713847902,
11.6404223877528));
#198934=CARTESIAN_POINT('Ctrl Pts',(-17.5738710901486,17.4401640303468,
11.6390968730311));
#198935=CARTESIAN_POINT('Ctrl Pts',(-17.5668757855613,17.444766667768,11.6385994860182));
#198936=CARTESIAN_POINT('Ctrl Pts',(-17.5545460456886,17.4529843878896,
11.6377165824833));
#198937=CARTESIAN_POINT('Ctrl Pts',(-17.5492004352257,17.4565825717185,
11.6373317054563));
#198938=CARTESIAN_POINT('Ctrl Pts',(-17.5381383541914,17.4641021841157,
11.6365308565426));
#198939=CARTESIAN_POINT('Ctrl Pts',(-17.532424557653,17.4680273927488,11.6361147441348));
#198940=CARTESIAN_POINT('Ctrl Pts',(-17.517724169298,17.4782327616776,11.6350377538351));
#198941=CARTESIAN_POINT('Ctrl Pts',(-17.5087669834297,17.4845547368719,
11.6343752823735));
#198942=CARTESIAN_POINT('Ctrl Pts',(-17.4708707668758,17.5117453108734,
11.6315454664862));
#198943=CARTESIAN_POINT('Ctrl Pts',(-17.4424140301682,17.5332731457457,
11.6293527447546));
#198944=CARTESIAN_POINT('Ctrl Pts',(-17.3690205726399,17.5917702736534,
11.623512295077));
#198945=CARTESIAN_POINT('Ctrl Pts',(-17.3250426906431,17.6298889701344,
11.6198210715812));
#198946=CARTESIAN_POINT('Ctrl Pts',(-17.16236303672,17.7830768316281,11.6054232915186));
#198947=CARTESIAN_POINT('Ctrl Pts',(-17.0557295954231,17.9100741052188,
11.5943090586917));
#198948=CARTESIAN_POINT('Ctrl Pts',(-16.9327538503364,18.0971605956071,
11.5797921147241));
#198949=CARTESIAN_POINT('Ctrl Pts',(-16.9025977377251,18.147471442423,11.5760536559104));
#198950=CARTESIAN_POINT('Ctrl Pts',(-16.8703032960898,18.2068072227535,
11.5718848024811));
#198951=CARTESIAN_POINT('Ctrl Pts',(-16.8660893302217,18.2146675885096,
11.5713372678744));
#198952=CARTESIAN_POINT('Ctrl Pts',(-16.8598120079354,18.2265565775295,
11.5705164760147));
#198953=CARTESIAN_POINT('Ctrl Pts',(-16.8577117519602,18.2305654571611,
11.5702409652391));
#198954=CARTESIAN_POINT('Ctrl Pts',(-16.8539791506287,18.2377460098456,
11.56974976198));
#198955=CARTESIAN_POINT('Ctrl Pts',(-16.8523419560362,18.2409150915381,
11.5695337667376));
#198956=CARTESIAN_POINT('Ctrl Pts',(-16.8488181234957,18.247778582184,11.5690676917523));
#198957=CARTESIAN_POINT('Ctrl Pts',(-16.8469343376717,18.2514743911809,
11.5688177915615));
#198958=CARTESIAN_POINT('Ctrl Pts',(-16.841713439,18.2617921425662,11.5681230434265));
#198959=CARTESIAN_POINT('Ctrl Pts',(-16.8384001992717,18.2684261913638,
11.567679667975));
#198960=CARTESIAN_POINT('Ctrl Pts',(-16.8195604469863,18.3066498680522,
11.5651433593889));
#198961=CARTESIAN_POINT('Ctrl Pts',(-16.8047878635503,18.3386074148869,
11.5630944049475));
#198962=CARTESIAN_POINT('Ctrl Pts',(-16.7602204144,18.4416960640825,11.5566645509209));
#198963=CARTESIAN_POINT('Ctrl Pts',(-16.7335097351966,18.5140961741071,
11.5524147678487));
#198964=CARTESIAN_POINT('Ctrl Pts',(-16.6547947039527,18.769640079198,11.5378226612765));
#198965=CARTESIAN_POINT('Ctrl Pts',(-16.6235566710767,18.9581825625041,
11.5276699631841));
#198966=CARTESIAN_POINT('Ctrl Pts',(-16.6172876560822,19.1699552799707,
11.5153414775381));
#198967=CARTESIAN_POINT('Ctrl Pts',(-16.6169790180816,19.1915596473639,
11.5140744879302));
#198968=CARTESIAN_POINT('Ctrl Pts',(-16.6170096727442,19.2215431645967,
11.5123018237538));
#198969=CARTESIAN_POINT('Ctrl Pts',(-16.6170679819039,19.2299217257715,
11.5118049275352));
#198970=CARTESIAN_POINT('Ctrl Pts',(-16.6172541346972,19.2443560862753,
11.5109461411231));
#198971=CARTESIAN_POINT('Ctrl Pts',(-16.6173582330624,19.2504121307511,
11.5105849976694));
#198972=CARTESIAN_POINT('Ctrl Pts',(-16.6176270766693,19.2629267712989,
11.5098369482988));
#198973=CARTESIAN_POINT('Ctrl Pts',(-16.6177954010009,19.2693852200894,
11.5094499340261));
#198974=CARTESIAN_POINT('Ctrl Pts',(-16.6182575183143,19.28446544812,11.5085439679263));
#198975=CARTESIAN_POINT('Ctrl Pts',(-16.6185744523904,19.2930863566998,
11.5080242959635));
#198976=CARTESIAN_POINT('Ctrl Pts',(-16.619766877102,19.3208912767179,11.5063424035464));
#198977=CARTESIAN_POINT('Ctrl Pts',(-16.6208506943456,19.3400649624337,
11.505173683693));
#198978=CARTESIAN_POINT('Ctrl Pts',(-16.6276561703373,19.4370273330098,
11.4992166016647));
#198979=CARTESIAN_POINT('Ctrl Pts',(-16.6374123056662,19.5144638800302,
11.4943031743117));
#198980=CARTESIAN_POINT('Ctrl Pts',(-16.6778959968728,19.7362297481452,
11.4797925704699));
#198981=CARTESIAN_POINT('Ctrl Pts',(-16.7194566174206,19.8781120566393,
11.4699322484873));
#198982=CARTESIAN_POINT('Ctrl Pts',(-16.8048782625093,20.086331582315,11.4552023150989));
#198983=CARTESIAN_POINT('Ctrl Pts',(-16.8382764015838,20.1564897065807,
11.4501988740954));
#198984=CARTESIAN_POINT('Ctrl Pts',(-16.8800160265032,20.2330191122241,
11.4448146552489));
#198985=CARTESIAN_POINT('Ctrl Pts',(-16.8846310518782,20.2413466121835,
11.4442298160458));
#198986=CARTESIAN_POINT('Ctrl Pts',(-16.8915519164469,20.2536385211883,
11.443368427247));
#198987=CARTESIAN_POINT('Ctrl Pts',(-16.893814636686,20.2576268943674,11.4430892251613));
#198988=CARTESIAN_POINT('Ctrl Pts',(-16.8978631249317,20.2647092278751,
11.4425940010038));
#198989=CARTESIAN_POINT('Ctrl Pts',(-16.8996437794134,20.2678060453785,
11.4423776556722));
#198990=CARTESIAN_POINT('Ctrl Pts',(-16.9034884891663,20.2744535606612,
11.4419136874145));
#198991=CARTESIAN_POINT('Ctrl Pts',(-16.9055550344743,20.2780027533611,
11.441666228862));
#198992=CARTESIAN_POINT('Ctrl Pts',(-16.911286643476,20.2877809677476,11.4409851225405));
#198993=CARTESIAN_POINT('Ctrl Pts',(-16.9149733362137,20.2939973372153,
11.440552854627));
#198994=CARTESIAN_POINT('Ctrl Pts',(-16.9353240135401,20.3279148239308,
11.4381976880994));
#198995=CARTESIAN_POINT('Ctrl Pts',(-16.9525899622241,20.3552519664713,
11.436311738785));
#198996=CARTESIAN_POINT('Ctrl Pts',(-17.0605740209722,20.5178501204822,
11.425102100913));
#198997=CARTESIAN_POINT('Ctrl Pts',(-17.1660346205669,20.6426802134523,
11.4164943786594));
#198998=CARTESIAN_POINT('Ctrl Pts',(-17.3700262245264,20.8342502160882,
11.4011747407821));
#198999=CARTESIAN_POINT('Ctrl Pts',(-17.4617509395734,20.9070963351511,
11.3946462198658));
#199000=CARTESIAN_POINT('Ctrl Pts',(-17.5708760650445,20.9799078817012,
11.386960603818));
#199001=CARTESIAN_POINT('Ctrl Pts',(-17.5828184775738,20.987702977319,11.3861207623949));
#199002=CARTESIAN_POINT('Ctrl Pts',(-17.6019578141564,20.9999216950296,
11.3847763512077));
#199003=CARTESIAN_POINT('Ctrl Pts',(-17.6091041613893,21.0044240130542,
11.3842747076628));
#199004=CARTESIAN_POINT('Ctrl Pts',(-17.6217595539072,21.0122917207251,
11.3833868623902));
#199005=CARTESIAN_POINT('Ctrl Pts',(-17.6272574387829,21.0156749222072,
11.3830013239591));
#199006=CARTESIAN_POINT('Ctrl Pts',(-17.6386649836771,21.0226229833315,
11.3822016777864));
#199007=CARTESIAN_POINT('Ctrl Pts',(-17.644576767613,21.0261841919482,11.3817874422534));
#199008=CARTESIAN_POINT('Ctrl Pts',(-17.6598050531408,21.0352563919834,
11.3807207806086));
#199009=CARTESIAN_POINT('Ctrl Pts',(-17.6691465147597,21.0407249016469,
11.380066818611));
#199010=CARTESIAN_POINT('Ctrl Pts',(-17.7083860721731,21.0632935443514,
11.3773209924109));
#199011=CARTESIAN_POINT('Ctrl Pts',(-17.7386559173632,21.0797335930151,
11.3752055880742));
#199012=CARTESIAN_POINT('Ctrl Pts',(-17.8186342981646,21.120676636333,11.3696201204907));
#199013=CARTESIAN_POINT('Ctrl Pts',(-17.8689251941597,21.1439780055794,
11.366111135662));
#199014=CARTESIAN_POINT('Ctrl Pts',(-18.0212889993912,21.207435511519,11.355499555825));
#199015=CARTESIAN_POINT('Ctrl Pts',(-18.1256246289486,21.2416618800848,
11.3482487140524));
#199016=CARTESIAN_POINT('Ctrl Pts',(-18.2934918689496,21.2826251689456,
11.3368351360873));
#199017=CARTESIAN_POINT('Ctrl Pts',(-18.3554938271188,21.2948454769652,
11.3326745932652));
#199018=CARTESIAN_POINT('Ctrl Pts',(-18.4215225606767,21.3048146748482,
11.3283530534595));
#199019=CARTESIAN_POINT('Ctrl Pts',(-18.4250949455776,21.3053446971034,
11.3281195818666));
#199020=CARTESIAN_POINT('Ctrl Pts',(-18.480170370975,21.3133720627818,11.3245255314925));
#199021=CARTESIAN_POINT('Ctrl Pts',(-18.531936183015,21.3189774561398,11.3212195601482));
#199022=CARTESIAN_POINT('Ctrl Pts',(-18.5925088602089,21.3232841743815,
11.3174738996854));
#199023=CARTESIAN_POINT('Ctrl Pts',(-18.6011613031151,21.3238459627956,
11.3169417738591));
#199024=CARTESIAN_POINT('Ctrl Pts',(-18.6142818875039,21.3246169417625,
11.3161395295049));
#199025=CARTESIAN_POINT('Ctrl Pts',(-18.6187475211981,21.3248651494228,
11.3158673028685));
#199026=CARTESIAN_POINT('Ctrl Pts',(-18.626772299796,21.3252856753279,11.3153796231478));
#199027=CARTESIAN_POINT('Ctrl Pts',(-18.6303311058605,21.3254631606039,
11.3151638856158));
#199028=CARTESIAN_POINT('Ctrl Pts',(-18.6380737937486,21.3258297101021,
11.3146956903862));
#199029=CARTESIAN_POINT('Ctrl Pts',(-18.642257780132,21.3260153440501,11.3144434266741));
#199030=CARTESIAN_POINT('Ctrl Pts',(-18.6540343106212,21.3265028304012,
11.3137353995251));
#199031=CARTESIAN_POINT('Ctrl Pts',(-18.6616280572531,21.3267762270104,
11.313281201361));
#199032=CARTESIAN_POINT('Ctrl Pts',(-18.707500191893,21.3281804973007,11.3105508139893));
#199033=CARTESIAN_POINT('Ctrl Pts',(-18.7458046282492,21.3283135247564,
11.3083268572928));
#199034=CARTESIAN_POINT('Ctrl Pts',(-18.872959702434,21.3253038348203,11.3010685126954));
#199035=CARTESIAN_POINT('Ctrl Pts',(-18.9616119178651,21.3176052850084,
11.2962072710144));
#199036=CARTESIAN_POINT('Ctrl Pts',(-19.2204010022461,21.2785989859009,
11.2819730642575));
#199037=CARTESIAN_POINT('Ctrl Pts',(-19.38746128238,21.2320227716173,11.2726699152892));
#199038=CARTESIAN_POINT('Ctrl Pts',(-19.5684013417516,21.1567648026964,
11.2612846863707));
#199039=CARTESIAN_POINT('Ctrl Pts',(-19.5896546695879,21.1475126621208,
11.2599269005634));
#199040=CARTESIAN_POINT('Ctrl Pts',(-19.61946836711,21.1339473449959,11.2579913033342));
#199041=CARTESIAN_POINT('Ctrl Pts',(-19.6281584055849,21.129921953056,11.2574233589185));
#199042=CARTESIAN_POINT('Ctrl Pts',(-19.6422228599753,21.1232907485736,
11.2564979211355));
#199043=CARTESIAN_POINT('Ctrl Pts',(-19.6476141498304,21.1207208839424,
11.2561416752308));
#199044=CARTESIAN_POINT('Ctrl Pts',(-19.6587502178289,21.1153547085741,
11.255402680866));
#199045=CARTESIAN_POINT('Ctrl Pts',(-19.6644933498556,21.1125551388084,
11.255019821718));
#199046=CARTESIAN_POINT('Ctrl Pts',(-19.6780039477084,21.105893347004,11.2541149944336));
#199047=CARTESIAN_POINT('Ctrl Pts',(-19.6857604778694,21.1020093175536,
11.2535922672215));
#199048=CARTESIAN_POINT('Ctrl Pts',(-19.7021492214513,21.0936763902196,
11.2524807864139));
#199049=CARTESIAN_POINT('Ctrl Pts',(-19.710775111216,21.08921555804,11.2518916208867));
#199050=CARTESIAN_POINT('Ctrl Pts',(-19.7340764993085,21.0769614403632,
11.2502886491783));
#199051=CARTESIAN_POINT('Ctrl Pts',(-19.7486911975887,21.069054587536,11.2492708561578));
#199052=CARTESIAN_POINT('Ctrl Pts',(-19.7940791437828,21.0438035813068,
11.2460704430737));
#199053=CARTESIAN_POINT('Ctrl Pts',(-19.8245111230161,21.0258614326853,
11.2438669874616));
#199054=CARTESIAN_POINT('Ctrl Pts',(-19.9426842944749,20.9521430616556,
11.2350791291115));
#199055=CARTESIAN_POINT('Ctrl Pts',(-20.0267073626804,20.8907024097566,
11.2283050634107));
#199056=CARTESIAN_POINT('Ctrl Pts',(-20.2180933636188,20.7278610628081,
11.2117366713103));
#199057=CARTESIAN_POINT('Ctrl Pts',(-20.3200485882068,20.6209137489345,
11.2018932674048));
#199058=CARTESIAN_POINT('Ctrl Pts',(-20.4195599670587,20.4919440703462,
11.1917336419008));
#199059=CARTESIAN_POINT('Ctrl Pts',(-20.4289104268596,20.47954593575,11.1907730569111));
#199060=CARTESIAN_POINT('Ctrl Pts',(-20.441544763451,20.4624044603584,11.1894681178351));
#199061=CARTESIAN_POINT('Ctrl Pts',(-20.444946669146,20.4577492689874,11.1891160379487));
#199062=CARTESIAN_POINT('Ctrl Pts',(-20.4503280637915,20.4503218225994,
11.1885580266811));
#199063=CARTESIAN_POINT('Ctrl Pts',(-20.4523199244401,20.4475586278791,
11.188351250476));
#199064=CARTESIAN_POINT('Ctrl Pts',(-20.4564248077126,20.4418350864301,
11.1879246537967));
#199065=CARTESIAN_POINT('Ctrl Pts',(-20.4585368723974,20.4388740994531,
11.1877049043681));
#199066=CARTESIAN_POINT('Ctrl Pts',(-20.4635592093266,20.4317945663319,
11.1871817122292));
#199067=CARTESIAN_POINT('Ctrl Pts',(-20.4664624389261,20.4276710034597,
11.1868787522052));
#199068=CARTESIAN_POINT('Ctrl Pts',(-20.4762402075636,20.4136773198074,
11.1858564953932));
#199069=CARTESIAN_POINT('Ctrl Pts',(-20.483045500209,20.4037587894231,11.1851417657773));
#199070=CARTESIAN_POINT('Ctrl Pts',(-20.4992145917481,20.3797567930537,
11.1834343070271));
#199071=CARTESIAN_POINT('Ctrl Pts',(-20.5084950230396,20.3656178789156,
11.1824465619013));
#199072=CARTESIAN_POINT('Ctrl Pts',(-20.542793561286,20.3119729054226,11.1787603976243));
#199073=CARTESIAN_POINT('Ctrl Pts',(-20.5666712987927,20.2717506580328,
11.17612030076));
#199074=CARTESIAN_POINT('Ctrl Pts',(-20.6411063548543,20.1363357441531,
11.1675235763867));
#199075=CARTESIAN_POINT('Ctrl Pts',(-20.6856834273888,20.0381597446355,
11.1617436503133));
#199076=CARTESIAN_POINT('Ctrl Pts',(-20.7225806899004,19.9371100741315,
11.1558808822554));
#199077=CARTESIAN_POINT('',(-20.851016007326,19.2120754280517,11.6890562438271));
#199078=CARTESIAN_POINT('Ctrl Pts',(-20.8509997268492,19.2120754163999,
11.6890562436229));
#199079=CARTESIAN_POINT('Ctrl Pts',(-20.8510361609233,19.140353500128,11.6847206650321));
#199080=CARTESIAN_POINT('Ctrl Pts',(-20.8474235543273,19.0684835617338,
11.6803850864412));
#199081=CARTESIAN_POINT('Ctrl Pts',(-20.8401430852414,18.9968731579421,
11.6760495078504));
#199082=CARTESIAN_POINT('Ctrl Pts',(-20.8328737172071,18.92537194365,11.671720540026));
#199083=CARTESIAN_POINT('Ctrl Pts',(-20.8219476405689,18.8541299663453,
11.6673915722017));
#199084=CARTESIAN_POINT('Ctrl Pts',(-20.8073980430273,18.7835546173248,
11.6630626043773));
#199085=CARTESIAN_POINT('Ctrl Pts',(-20.7928607647276,18.7130390249256,
11.658737301919));
#199086=CARTESIAN_POINT('Ctrl Pts',(-20.7747061465212,18.6431894241743,
11.6544119994608));
#199087=CARTESIAN_POINT('Ctrl Pts',(-20.7530189912436,18.5744064774147,
11.6500866970025));
#199088=CARTESIAN_POINT('Ctrl Pts',(-20.7313426460971,18.5056578160493,
11.6457635505248));
#199089=CARTESIAN_POINT('Ctrl Pts',(-20.7061374043778,18.4379752252391,
11.6414404040472));
#199090=CARTESIAN_POINT('Ctrl Pts',(-20.6775383611331,18.3717457841607,
11.6371172575695));
#199091=CARTESIAN_POINT('Ctrl Pts',(-20.6489436148164,18.3055262938746,
11.6327947606328));
#199092=CARTESIAN_POINT('Ctrl Pts',(-20.6169562761199,18.2407599735633,
11.6284722636961));
#199093=CARTESIAN_POINT('Ctrl Pts',(-20.5817594783855,18.1778137099067,
11.6241497667594));
#199094=CARTESIAN_POINT('Ctrl Pts',(-20.5465310340247,18.1148108491444,
11.6198233833201));
#199095=CARTESIAN_POINT('Ctrl Pts',(-20.5080876068594,18.0536317475177,
11.6154969998808));
#199096=CARTESIAN_POINT('Ctrl Pts',(-20.4666577218297,17.9946175687786,
11.6111706164415));
#199097=CARTESIAN_POINT('Ctrl Pts',(-20.4252103606638,17.9355784964193,
11.6068424080281));
#199098=CARTESIAN_POINT('Ctrl Pts',(-20.3807743381433,17.878706555747,11.6025141996147));
#199099=CARTESIAN_POINT('Ctrl Pts',(-20.3336191165842,17.8243105315686,
11.5981859912013));
#199100=CARTESIAN_POINT('Ctrl Pts',(-20.2863774057356,17.7698147374533,
11.5938498442467));
#199101=CARTESIAN_POINT('Ctrl Pts',(-20.2364068761987,17.7178042891277,
11.5895136972921));
#199102=CARTESIAN_POINT('Ctrl Pts',(-20.184014156115,17.6685513146085,11.5851775503375));
#199103=CARTESIAN_POINT('Ctrl Pts',(-20.1349615139514,17.6224382567118,
11.5811178362285));
#199104=CARTESIAN_POINT('Ctrl Pts',(-20.0837862726332,17.578742122906,11.5770581221195));
#199105=CARTESIAN_POINT('Ctrl Pts',(-20.0307638001155,17.5376522636612,
11.5729984080105));
#199106=CARTESIAN_POINT('Ctrl Pts',(-19.9734509743369,17.4932375875374,
11.5686101990796));
#199107=CARTESIAN_POINT('Ctrl Pts',(-19.9137418045022,17.4516841015565,
11.5642219901487));
#199108=CARTESIAN_POINT('Ctrl Pts',(-19.8519537768687,17.4132602099344,
11.5598337812178));
#199109=CARTESIAN_POINT('Ctrl Pts',(-19.7902574529129,17.3748933457383,
11.5554520851166));
#199110=CARTESIAN_POINT('Ctrl Pts',(-19.7264888022835,17.3396471078962,
11.5510703890153));
#199111=CARTESIAN_POINT('Ctrl Pts',(-19.6609970987603,17.3077487346937,
11.546688692914));
#199112=CARTESIAN_POINT('Ctrl Pts',(-19.5955823532007,17.2758878446183,
11.5423121456544));
#199113=CARTESIAN_POINT('Ctrl Pts',(-19.5284490083959,17.2473672144277,
11.5379355983948));
#199114=CARTESIAN_POINT('Ctrl Pts',(-19.45997246989,17.2223690707017,11.5335590511351));
#199115=CARTESIAN_POINT('Ctrl Pts',(-19.3915393582096,17.1973867804351,
11.5291852794182));
#199116=CARTESIAN_POINT('Ctrl Pts',(-19.32176519499,17.1759227092788,11.5248115077012));
#199117=CARTESIAN_POINT('Ctrl Pts',(-19.2510456730813,17.1581111155379,
11.5204377359842));
#199118=CARTESIAN_POINT('Ctrl Pts',(-19.1803476713606,17.1403049419248,
11.5160652952207));
#199119=CARTESIAN_POINT('Ctrl Pts',(-19.1087053495643,17.1261491568768,
11.5116928544571));
#199120=CARTESIAN_POINT('Ctrl Pts',(-19.0365282611614,17.1157277858954,
11.5073204136936));
#199121=CARTESIAN_POINT('Ctrl Pts',(-18.9643493271828,17.1053061484385,
11.5029478611262));
#199122=CARTESIAN_POINT('Ctrl Pts',(-18.8916360771615,17.0986191815879,
11.4985753085589));
#199123=CARTESIAN_POINT('Ctrl Pts',(-18.8188052520572,17.0956992957918,
11.4942027559916));
#199124=CARTESIAN_POINT('Ctrl Pts',(-18.7458988403753,17.0927763796282,
11.4898256654243));
#199125=CARTESIAN_POINT('Ctrl Pts',(-18.6728750930031,17.0936283697016,
11.4854485748569));
#199126=CARTESIAN_POINT('Ctrl Pts',(-18.6001519939629,17.0982355286781,
11.4810714842896));
#199127=CARTESIAN_POINT('Ctrl Pts',(-18.5273891781392,17.1028452037952,
11.4766920032307));
#199128=CARTESIAN_POINT('Ctrl Pts',(-18.4549278170831,17.1112140756296,
11.4723125221717));
#199129=CARTESIAN_POINT('Ctrl Pts',(-18.3831792948545,17.1232706514394,
11.4679330411128));
#199130=CARTESIAN_POINT('Ctrl Pts',(-18.3113035988519,17.135348597449,11.4635457974531));
#199131=CARTESIAN_POINT('Ctrl Pts',(-18.2401437361935,17.1511271959047,
11.4591585537934));
#199132=CARTESIAN_POINT('Ctrl Pts',(-18.1700988737773,17.1704842515078,
11.4547713101336));
#199133=CARTESIAN_POINT('Ctrl Pts',(-18.1224751168407,17.1836451840766,
11.4517884071988));
#199134=CARTESIAN_POINT('Ctrl Pts',(-18.0753664841793,17.1984592758342,
11.448805504264));
#199135=CARTESIAN_POINT('Ctrl Pts',(-18.0288930166915,17.2148754692932,
11.4458226013291));
#199136=CARTESIAN_POINT('Ctrl Pts',(-17.960524957276,17.2390256640268,11.4414343923982));
#199137=CARTESIAN_POINT('Ctrl Pts',(-17.8932656103902,17.2667395128395,
11.4370461834673));
#199138=CARTESIAN_POINT('Ctrl Pts',(-17.8275125107934,17.2978953421436,
11.4326579745364));
#199139=CARTESIAN_POINT('Ctrl Pts',(-17.7618569996983,17.3290049310313,
11.4282762784352));
#199140=CARTESIAN_POINT('Ctrl Pts',(-17.6977037303935,17.3635461545568,
11.4238945823339));
#199141=CARTESIAN_POINT('Ctrl Pts',(-17.6354328295884,17.401348328519,11.4195128862326));
#199142=CARTESIAN_POINT('Ctrl Pts',(-17.5732351020475,17.4391060819184,
11.415136338973));
#199143=CARTESIAN_POINT('Ctrl Pts',(-17.5129157592866,17.4801169246316,
11.4107597917133));
#199144=CARTESIAN_POINT('Ctrl Pts',(-17.454831224922,17.5241638357963,11.4063832444537));
#199145=CARTESIAN_POINT('Ctrl Pts',(-17.3967835269249,17.5681828130501,
11.4020094727367));
#199146=CARTESIAN_POINT('Ctrl Pts',(-17.3409682086663,17.6152337476986,
11.3976357010197));
#199147=CARTESIAN_POINT('Ctrl Pts',(-17.2877123411686,17.6650565961484,
11.3932619293028));
#199148=CARTESIAN_POINT('Ctrl Pts',(-17.2344726796103,17.7148642833382,
11.3888894885392));
#199149=CARTESIAN_POINT('Ctrl Pts',(-17.1837912746023,17.7674418803649,
11.3845170477757));
#199150=CARTESIAN_POINT('Ctrl Pts',(-17.135960461819,17.8224904989845,11.3801446070121));
#199151=CARTESIAN_POINT('Ctrl Pts',(-17.0881284259965,17.8775405252034,
11.3757720544447));
#199152=CARTESIAN_POINT('Ctrl Pts',(-17.0431474419897,17.9350613330224,
11.3713995018774));
#199153=CARTESIAN_POINT('Ctrl Pts',(-17.001270335834,17.994720052406,11.36702694931));
#199154=CARTESIAN_POINT('Ctrl Pts',(-16.959349768038,18.0544406878589,11.3626498587427));
#199155=CARTESIAN_POINT('Ctrl Pts',(-16.9205397874117,18.1163032692078,
11.3582727681754));
#199156=CARTESIAN_POINT('Ctrl Pts',(-16.8850500448045,18.179945654593,11.3538956776081));
#199157=CARTESIAN_POINT('Ctrl Pts',(-16.8495409199317,18.2436227974469,
11.3495161965491));
#199158=CARTESIAN_POINT('Ctrl Pts',(-16.8173558563405,18.3090812464319,
11.3451367154902));
#199159=CARTESIAN_POINT('Ctrl Pts',(-16.7886574143382,18.3759363949911,
11.3407572344312));
#199160=CARTESIAN_POINT('Ctrl Pts',(-16.75990810454,18.4429100438524,11.3363699907715));
#199161=CARTESIAN_POINT('Ctrl Pts',(-16.7346579248205,18.511284883135,11.3319827471118));
#199162=CARTESIAN_POINT('Ctrl Pts',(-16.7130201897423,18.5806591346496,
11.3275955034521));
#199163=CARTESIAN_POINT('Ctrl Pts',(-16.6983086148963,18.6278269407927,
11.3246126005173));
#199164=CARTESIAN_POINT('Ctrl Pts',(-16.68526591231,18.6754564326548,11.3216296975824));
#199165=CARTESIAN_POINT('Ctrl Pts',(-16.6739141265779,18.7234190383877,
11.3186467946476));
#199166=CARTESIAN_POINT('Ctrl Pts',(-16.6572142846389,18.7939777992408,
11.3142585857167));
#199167=CARTESIAN_POINT('Ctrl Pts',(-16.6441110368838,18.8655332466771,
11.3098703767858));
#199168=CARTESIAN_POINT('Ctrl Pts',(-16.6347172531061,18.9376852572698,
11.3054821678549));
#199169=CARTESIAN_POINT('Ctrl Pts',(-16.6253374112611,19.0097301823155,
11.3011004717537));
#199170=CARTESIAN_POINT('Ctrl Pts',(-16.6196561660671,19.0823694384939,
11.2967187756524));
#199171=CARTESIAN_POINT('Ctrl Pts',(-16.6177357545009,19.1551910112778,
11.2923370795512));
#199172=CARTESIAN_POINT('Ctrl Pts',(-16.6158175995711,19.2279270129186,
11.2879605322915));
#199173=CARTESIAN_POINT('Ctrl Pts',(-16.6176515119966,19.3008444257661,
11.2835839850319));
#199174=CARTESIAN_POINT('Ctrl Pts',(-16.6232479369201,19.3735260846875,
11.2792074377722));
#199175=CARTESIAN_POINT('Ctrl Pts',(-16.6288408126722,19.4461616499572,
11.2748336660553));
#199176=CARTESIAN_POINT('Ctrl Pts',(-16.6381914295875,19.5185612781807,
11.2704598943383));
#199177=CARTESIAN_POINT('Ctrl Pts',(-16.6512581694981,19.5903091977233,
11.2660861226213));
#199178=CARTESIAN_POINT('Ctrl Pts',(-16.6643209331558,19.6620352841331,
11.2617136818578));
#199179=CARTESIAN_POINT('Ctrl Pts',(-16.6810974883882,19.7331095812962,
11.2573412410942));
#199180=CARTESIAN_POINT('Ctrl Pts',(-16.701494753238,19.803124498636,11.2529688003307));
#199181=CARTESIAN_POINT('Ctrl Pts',(-16.7218925396482,19.873141206265,11.2485962477633));
#199182=CARTESIAN_POINT('Ctrl Pts',(-16.7459110826477,19.9420980177238,
11.244223695196));
#199183=CARTESIAN_POINT('Ctrl Pts',(-16.7734073411525,20.0096021700904,
11.2398511426286));
#199184=CARTESIAN_POINT('Ctrl Pts',(-16.8009321363113,20.0771763808124,
11.2354740520613));
#199185=CARTESIAN_POINT('Ctrl Pts',(-16.8319416708365,20.143294474674,11.231096961494));
#199186=CARTESIAN_POINT('Ctrl Pts',(-16.8662449207626,20.2075841479689,
11.2267198709266));
#199187=CARTESIAN_POINT('Ctrl Pts',(-16.9005669049666,20.2719089322405,
11.2223403898677));
#199188=CARTESIAN_POINT('Ctrl Pts',(-16.938185937055,20.3344028942419,11.2179609088088));
#199189=CARTESIAN_POINT('Ctrl Pts',(-16.9788666145899,20.394721166246,11.2135814277498));
#199190=CARTESIAN_POINT('Ctrl Pts',(-17.0196193983526,20.4551463519822,
11.2091941840901));
#199191=CARTESIAN_POINT('Ctrl Pts',(-17.0634443742617,20.5133877608711,
11.2048069404304));
#199192=CARTESIAN_POINT('Ctrl Pts',(-17.1100650454665,20.5691326383841,
11.2004196967707));
#199193=CARTESIAN_POINT('Ctrl Pts',(-17.1417626095285,20.6070337835293,
11.1974367938359));
#199194=CARTESIAN_POINT('Ctrl Pts',(-17.1747517071183,20.643781572932,11.194453890901));
#199195=CARTESIAN_POINT('Ctrl Pts',(-17.2089361619795,20.6792878770739,
11.1914709879662));
#199196=CARTESIAN_POINT('Ctrl Pts',(-17.259225605987,20.7315219203344,11.1870827790353));
#199197=CARTESIAN_POINT('Ctrl Pts',(-17.3122998738988,20.7812712846034,
11.1826945701044));
#199198=CARTESIAN_POINT('Ctrl Pts',(-17.3678836195123,20.8282244850246,
11.1783063611735));
#199199=CARTESIAN_POINT('Ctrl Pts',(-17.4233848696314,20.8751079991114,
11.1739246650723));
#199200=CARTESIAN_POINT('Ctrl Pts',(-17.4813878383958,20.9192032789,11.169542968971));
#199201=CARTESIAN_POINT('Ctrl Pts',(-17.5415797744862,20.9602349772931,
11.1651612728698));
#199202=CARTESIAN_POINT('Ctrl Pts',(-17.6017009802615,21.0012184601752,
11.1607847256101));
#199203=CARTESIAN_POINT('Ctrl Pts',(-17.6640056470485,21.0391452426346,
11.1564081783505));
#199204=CARTESIAN_POINT('Ctrl Pts',(-17.7281486587461,21.0737807383849,
11.1520316310908));
#199205=CARTESIAN_POINT('Ctrl Pts',(-17.7922509918778,21.1083942688071,
11.1476578593739));
#199206=CARTESIAN_POINT('Ctrl Pts',(-17.8581889333121,21.1397204253384,
11.1432840876569));
#199207=CARTESIAN_POINT('Ctrl Pts',(-17.9255903577763,21.1675691529715,
11.1389103159399));
#199208=CARTESIAN_POINT('Ctrl Pts',(-17.9929712717607,21.1954094061433,
11.1345378751764));
#199209=CARTESIAN_POINT('Ctrl Pts',(-18.0618143390783,21.2197741471641,
11.1301654344128));
#199210=CARTESIAN_POINT('Ctrl Pts',(-18.1317264570587,21.2405210221806,
11.1257929936492));
#199211=CARTESIAN_POINT('Ctrl Pts',(-18.2016403626996,21.261268427697,11.1214204410819));
#199212=CARTESIAN_POINT('Ctrl Pts',(-18.2726229102623,21.2783976482244,
11.1170478885146));
#199213=CARTESIAN_POINT('Ctrl Pts',(-18.3442664228596,21.2918163635577,
11.1126753359472));
#199214=CARTESIAN_POINT('Ctrl Pts',(-18.4159842897966,21.3052490053399,
11.1082982453799));
#199215=CARTESIAN_POINT('Ctrl Pts',(-18.4883640162152,21.3149633643478,
11.1039211548125));
#199216=CARTESIAN_POINT('Ctrl Pts',(-18.5609891559671,21.3209185405714,
11.0995440642452));
#199217=CARTESIAN_POINT('Ctrl Pts',(-18.6336539590034,21.3268769691377,
11.0951645831863));
#199218=CARTESIAN_POINT('Ctrl Pts',(-18.7065639597306,21.329072112832,11.0907851021273));
#199219=CARTESIAN_POINT('Ctrl Pts',(-18.779301760092,21.3275152374912,11.0864056210684));
#199220=CARTESIAN_POINT('Ctrl Pts',(-18.8521684877163,21.3259556025994,
11.0820183774087));
#199221=CARTESIAN_POINT('Ctrl Pts',(-18.9248619239423,21.3206307033084,
11.077631133749));
#199222=CARTESIAN_POINT('Ctrl Pts',(-18.9969694292048,21.311603741619,11.0732438900892));
#199223=CARTESIAN_POINT('Ctrl Pts',(-19.0459955845206,21.3054662775061,
11.0702609871544));
#199224=CARTESIAN_POINT('Ctrl Pts',(-19.0947510327821,21.2976185484977,
11.0672780842196));
#199225=CARTESIAN_POINT('Ctrl Pts',(-19.1431096126279,21.2880937207684,
11.0642951812848));
#199226=CARTESIAN_POINT('Ctrl Pts',(-19.21425089902,21.2740815537551,11.0599069723539));
#199227=CARTESIAN_POINT('Ctrl Pts',(-19.2848103359501,21.2563828809337,
11.055518763423));
#199228=CARTESIAN_POINT('Ctrl Pts',(-19.3543769742709,21.2350606240413,
11.0511305544921));
#199229=CARTESIAN_POINT('Ctrl Pts',(-19.4238403641662,21.2137700129134,
11.0467488583908));
#199230=CARTESIAN_POINT('Ctrl Pts',(-19.4923134231182,21.1888666339676,
11.0423671622895));
#199231=CARTESIAN_POINT('Ctrl Pts',(-19.5593953414354,21.1604644214083,
11.0379854661882));
#199232=CARTESIAN_POINT('Ctrl Pts',(-19.6263984331598,21.1320955837092,
11.0336089189286));
#199233=CARTESIAN_POINT('Ctrl Pts',(-19.6920131895949,21.1002362668755,
11.029232371669));
#199234=CARTESIAN_POINT('Ctrl Pts',(-19.7558555559983,21.065049681825,11.0248558244093));
#199235=CARTESIAN_POINT('Ctrl Pts',(-19.8196574345007,21.0298854115954,
11.0204820526924));
#199236=CARTESIAN_POINT('Ctrl Pts',(-19.881688731758,20.9913982921376,11.0161082809754));
#199237=CARTESIAN_POINT('Ctrl Pts',(-19.9415882172339,20.9497983487448,
11.0117345092584));
#199238=CARTESIAN_POINT('Ctrl Pts',(-20.0014694750955,20.9082110643544,
11.0073620684949));
#199239=CARTESIAN_POINT('Ctrl Pts',(-20.059219813117,20.8635131115926,11.0029896277313));
#199240=CARTESIAN_POINT('Ctrl Pts',(-20.1145067552164,20.8159579741544,
10.9986171869677));
#199241=CARTESIAN_POINT('Ctrl Pts',(-20.1697951110089,20.7684016207262,
10.9942446344004));
#199242=CARTESIAN_POINT('Ctrl Pts',(-20.2226195814197,20.7179882536478,
10.989872081833));
#199243=CARTESIAN_POINT('Ctrl Pts',(-20.2726818719995,20.665010693489,10.9854995292657));
#199244=CARTESIAN_POINT('Ctrl Pts',(-20.3227961191127,20.61197815122,10.9811224386984));
#199245=CARTESIAN_POINT('Ctrl Pts',(-20.370142130828,20.5563764539256,10.976745348131));
#199246=CARTESIAN_POINT('Ctrl Pts',(-20.4144601023079,20.4985336285127,
10.9723682575637));
#199247=CARTESIAN_POINT('Ctrl Pts',(-20.4588022774771,20.4406592129859,
10.9679887765048));
#199248=CARTESIAN_POINT('Ctrl Pts',(-20.5001128464811,20.3805416302794,
10.9636092954458));
#199249=CARTESIAN_POINT('Ctrl Pts',(-20.5381753524546,20.3185379440883,
10.9592298143869));
#199250=CARTESIAN_POINT('Ctrl Pts',(-20.5763053239643,20.2564243567798,
10.9548425707271));
#199251=CARTESIAN_POINT('Ctrl Pts',(-20.6111755046332,20.192418413908,10.9504553270674));
#199252=CARTESIAN_POINT('Ctrl Pts',(-20.6426156833716,20.1269012900897,
10.9460680834077));
#199253=CARTESIAN_POINT('Ctrl Pts',(-20.6639919753451,20.0823559591087,
10.9430851804729));
#199254=CARTESIAN_POINT('Ctrl Pts',(-20.6837836766027,20.0371125159695,
10.9401022775381));
#199255=CARTESIAN_POINT('Ctrl Pts',(-20.7019503858965,19.9912949946334,
10.9371193746033));
#199256=CARTESIAN_POINT('Ctrl Pts',(-20.7090722076132,19.9733333366809,
10.9359499992059));
#199257=CARTESIAN_POINT('Ctrl Pts',(-20.7159498922732,19.955269678145,10.9347806238085));
#199258=CARTESIAN_POINT('Ctrl Pts',(-20.7225806064498,19.9371103026755,
10.9336112484111));
#199259=CARTESIAN_POINT('Ctrl Pts',(-20.7219730492699,19.9368789336487,
11.7337477349808));
#199260=CARTESIAN_POINT('Ctrl Pts',(-20.7875398502892,19.7626326972607,
11.7225565615512));
#199261=CARTESIAN_POINT('Ctrl Pts',(-20.8444161920097,19.5201105099742,
11.7076594095651));
#199262=CARTESIAN_POINT('Ctrl Pts',(-20.8542040955766,19.273466074897,11.692762257579));
#199263=CARTESIAN_POINT('Ctrl Pts',(-20.853822991173,19.2120774369757,11.6890562790225));
#199264=CARTESIAN_POINT('Origin',(-18.734,19.211,0.));
#199265=CARTESIAN_POINT('',(-20.7225806071911,19.9371103006456,12.75653014821));
#199266=CARTESIAN_POINT('',(-20.7225806018034,19.9371103154006,12.5316746994897));
#199267=CARTESIAN_POINT('',(-20.7225806064498,19.9371103026755,0.));
#199268=CARTESIAN_POINT('',(-20.850999901999,19.2116441554391,12.7090270029862));
#199269=CARTESIAN_POINT('Ctrl Pts',(-20.7225806071911,19.9371103006456,
12.75653014821));
#199270=CARTESIAN_POINT('Ctrl Pts',(-20.7242579214128,19.9325166810117,
12.7562119943992));
#199271=CARTESIAN_POINT('Ctrl Pts',(-20.725919378386,19.927917086162,12.7558935117464));
#199272=CARTESIAN_POINT('Ctrl Pts',(-20.7864431000032,19.7585277763737,
12.7441682245227));
#199273=CARTESIAN_POINT('Ctrl Pts',(-20.8246620318631,19.5870863820778,
12.7323482183352));
#199274=CARTESIAN_POINT('Ctrl Pts',(-20.8438467742753,19.3868429567836,
12.7196400581752));
#199275=CARTESIAN_POINT('Ctrl Pts',(-20.8458598061736,19.3607413110147,
12.7180060566353));
#199276=CARTESIAN_POINT('Ctrl Pts',(-20.8477953021789,19.3276490835098,
12.715968468761));
#199277=CARTESIAN_POINT('Ctrl Pts',(-20.8481679338033,19.320688372186,12.7155417813462));
#199278=CARTESIAN_POINT('Ctrl Pts',(-20.8487046765667,19.3096400718763,
12.7148676844595));
#199279=CARTESIAN_POINT('Ctrl Pts',(-20.8488913284795,19.3055537003482,
12.7146190451098));
#199280=CARTESIAN_POINT('Ctrl Pts',(-20.8492163340247,19.2979552396666,
12.7141580150344));
#199281=CARTESIAN_POINT('Ctrl Pts',(-20.8493577841497,19.2944433860608,
12.7139454585469));
#199282=CARTESIAN_POINT('Ctrl Pts',(-20.8496218268413,19.2874551214259,
12.713523515112));
#199283=CARTESIAN_POINT('Ctrl Pts',(-20.849744596623,19.2839787781355,12.7133141197207));
#199284=CARTESIAN_POINT('Ctrl Pts',(-20.850006252835,19.2760131563302,12.7128354340013));
#199285=CARTESIAN_POINT('Ctrl Pts',(-20.8501394227246,19.2715236891833,
12.7125664580095));
#199286=CARTESIAN_POINT('Ctrl Pts',(-20.8504746952252,19.2588612713493,
12.711810028741));
#199287=CARTESIAN_POINT('Ctrl Pts',(-20.8506437465308,19.2506874266378,
12.7113243345654));
#199288=CARTESIAN_POINT('Ctrl Pts',(-20.8509186141132,19.2322240492644,
12.7102326836416));
#199289=CARTESIAN_POINT('Ctrl Pts',(-20.8509967709478,19.2219342726963,
12.7096281222256));
#199290=CARTESIAN_POINT('Ctrl Pts',(-20.850999901999,19.2116441554391,12.7090270029862));
#199291=CARTESIAN_POINT('Ctrl Pts',(-20.8509999014158,19.2116460691223,
12.7090271147781));
#199292=CARTESIAN_POINT('Ctrl Pts',(-20.8510612404263,19.0106541402446,
12.6972857323756));
#199293=CARTESIAN_POINT('Ctrl Pts',(-20.8224997951858,18.810633809048,12.6868413446637));
#199294=CARTESIAN_POINT('Ctrl Pts',(-20.7414593028743,18.533101317908,12.6708787977931));
#199295=CARTESIAN_POINT('Ctrl Pts',(-20.7115380387582,18.4502239235883,
12.6659224450404));
#199296=CARTESIAN_POINT('Ctrl Pts',(-20.6684004803174,18.3506490097334,
12.6595976067165));
#199297=CARTESIAN_POINT('Ctrl Pts',(-20.6599809133746,18.3319627297392,
12.6583942611593));
#199298=CARTESIAN_POINT('Ctrl Pts',(-20.6475366195967,18.3053814065272,
12.6566576095812));
#199299=CARTESIAN_POINT('Ctrl Pts',(-20.643731405833,18.2973844433655,12.6561318752003));
#199300=CARTESIAN_POINT('Ctrl Pts',(-20.6370469607357,18.2835607822067,
12.6552173071385));
#199301=CARTESIAN_POINT('Ctrl Pts',(-20.6341908486712,18.277722991476,12.6548292816806));
#199302=CARTESIAN_POINT('Ctrl Pts',(-20.6286469714142,18.2665224533086,
12.6540812987143));
#199303=CARTESIAN_POINT('Ctrl Pts',(-20.6259632017933,18.2611577897345,
12.6537214839144));
#199304=CARTESIAN_POINT('Ctrl Pts',(-20.6188714145975,18.2471311235001,
12.6527765706384));
#199305=CARTESIAN_POINT('Ctrl Pts',(-20.614426520458,18.238488017101,12.6521901792748));
#199306=CARTESIAN_POINT('Ctrl Pts',(-20.5987859039375,18.2085829492576,
12.6501466443006));
#199307=CARTESIAN_POINT('Ctrl Pts',(-20.5872881357366,18.1874818406939,
12.6486788520719));
#199308=CARTESIAN_POINT('Ctrl Pts',(-20.503482796716,18.0397230352569,12.6382123895947));
#199309=CARTESIAN_POINT('Ctrl Pts',(-20.4186277887561,17.9206611186917,
12.6287469226873));
#199310=CARTESIAN_POINT('Ctrl Pts',(-20.2316748408658,17.7085295413942,
12.6100860236023));
#199311=CARTESIAN_POINT('Ctrl Pts',(-20.1313546897213,17.6148004864574,
12.6009623563512));
#199312=CARTESIAN_POINT('Ctrl Pts',(-20.0125946991022,17.5236808059512,
12.5915883312335));
#199313=CARTESIAN_POINT('Ctrl Pts',(-20.0024435423399,17.5160364416838,
12.590797638063));
#199314=CARTESIAN_POINT('Ctrl Pts',(-19.9868049689495,17.5044789444255,
12.5895963507252));
#199315=CARTESIAN_POINT('Ctrl Pts',(-19.9813668578717,17.5004999772129,
12.5891816906442));
#199316=CARTESIAN_POINT('Ctrl Pts',(-19.9723753383292,17.4939867302626,
12.5885012513126));
#199317=CARTESIAN_POINT('Ctrl Pts',(-19.9688329714792,17.4914373869045,
12.5882344921829));
#199318=CARTESIAN_POINT('Ctrl Pts',(-19.9619704832989,17.4865307856064,
12.5877202811318));
#199319=CARTESIAN_POINT('Ctrl Pts',(-19.9586513981957,17.4841721183665,
12.5874727348678));
#199320=CARTESIAN_POINT('Ctrl Pts',(-19.9553158056823,17.4818161743379,
12.5872251308145));
#199321=CARTESIAN_POINT('Ctrl Pts',(-19.9553061150038,17.4818093298901,
12.5872244114766));
#199322=CARTESIAN_POINT('Ctrl Pts',(-19.9552866993953,17.4817956170476,
12.5872229702781));
#199323=CARTESIAN_POINT('Ctrl Pts',(-19.9552769742806,17.4817887485233,
12.5872222484039));
#199324=CARTESIAN_POINT('Ctrl Pts',(-19.9552574896208,17.481774987404,12.5872208021199));
#199325=CARTESIAN_POINT('Ctrl Pts',(-19.9552477298694,17.4817680946641,
12.5872200776947));
#199326=CARTESIAN_POINT('Ctrl Pts',(-19.9552275533345,17.4817538454172,
12.5872185800965));
#199327=CARTESIAN_POINT('Ctrl Pts',(-19.9552171369376,17.4817464892004,
12.5872178069536));
#199328=CARTESIAN_POINT('Ctrl Pts',(-19.9551961361628,17.4817316584205,
12.5872162482226));
#199329=CARTESIAN_POINT('Ctrl Pts',(-19.9551855518082,17.4817241838784,
12.5872154626366));
#199330=CARTESIAN_POINT('Ctrl Pts',(-19.9551642116505,17.4817091140131,
12.5872138787634));
#199331=CARTESIAN_POINT('Ctrl Pts',(-19.9551534559073,17.4817015187369,
12.587213080481));
#199332=CARTESIAN_POINT('Ctrl Pts',(-19.955131769556,17.481686205005,12.5872114709625));
#199333=CARTESIAN_POINT('Ctrl Pts',(-19.9551208386152,17.4816784863193,
12.5872106597021));
#199334=CARTESIAN_POINT('Ctrl Pts',(-19.9550987979607,17.481662923024,12.5872090239387));
#199335=CARTESIAN_POINT('Ctrl Pts',(-19.9550876883188,17.4816550784701,
12.5872081994415));
#199336=CARTESIAN_POINT('Ctrl Pts',(-19.9550652861652,17.4816392605609,
12.5872065369018));
#199337=CARTESIAN_POINT('Ctrl Pts',(-19.9550539938539,17.4816312873523,
12.5872056988745));
#199338=CARTESIAN_POINT('Ctrl Pts',(-19.955031222665,17.4816152095399,12.5872040090017));
#199339=CARTESIAN_POINT('Ctrl Pts',(-19.9550197434877,17.4816071047299,
12.5872031571343));
#199340=CARTESIAN_POINT('Ctrl Pts',(-19.9549965942264,17.4815907606666,
12.5872014392605));
#199341=CARTESIAN_POINT('Ctrl Pts',(-19.9549849244509,17.4815825216369,
12.5872005732774));
#199342=CARTESIAN_POINT('Ctrl Pts',(-19.9549613899256,17.4815659062798,
12.5871988268716));
#199343=CARTESIAN_POINT('Ctrl Pts',(-19.9549495249503,17.4815575297991,
12.5871979464327));
#199344=CARTESIAN_POINT('Ctrl Pts',(-19.9549255955538,17.4815406364012,
12.587196170785));
#199345=CARTESIAN_POINT('Ctrl Pts',(-19.9549135313658,17.4815321196547,
12.5871952755941));
#199346=CARTESIAN_POINT('Ctrl Pts',(-19.9548891993164,17.4815149427595,
12.5871934701301));
#199347=CARTESIAN_POINT('Ctrl Pts',(-19.9548769310923,17.4815062823612,
12.5871925598306));
#199348=CARTESIAN_POINT('Ctrl Pts',(-19.9548521861696,17.4814888147924,
12.5871907237951));
#199349=CARTESIAN_POINT('Ctrl Pts',(-19.9548397097018,17.4814800077916,
12.5871897980766));
#199350=CARTESIAN_POINT('Ctrl Pts',(-19.9519913099692,17.4794694000664,
12.5869784586612));
#199351=CARTESIAN_POINT('Ctrl Pts',(-19.9491505071673,17.4774746050912,
12.5867685355329));
#199352=CARTESIAN_POINT('Ctrl Pts',(-19.94255546995,17.4728677863359,12.5862831463832));
#199353=CARTESIAN_POINT('Ctrl Pts',(-19.9387976744691,17.4702609383892,
12.5860080348999));
#199354=CARTESIAN_POINT('Ctrl Pts',(-19.9272418710299,17.4622998218784,
12.5851663937687));
#199355=CARTESIAN_POINT('Ctrl Pts',(-19.9194162781616,17.4569855386215,
12.5846025120512));
#199356=CARTESIAN_POINT('Ctrl Pts',(-19.8494529408243,17.4101562300247,
12.5796125709236));
#199357=CARTESIAN_POINT('Ctrl Pts',(-19.7851860079688,17.3719013005707,
12.575386643219));
#199358=CARTESIAN_POINT('Ctrl Pts',(-19.5990860785352,17.2740759124247,
12.5637419663062));
#199359=CARTESIAN_POINT('Ctrl Pts',(-19.4733711743142,17.2226887999682,
12.5565299566913));
#199360=CARTESIAN_POINT('Ctrl Pts',(-19.2568625606815,17.1575862411018,
12.5440641699188));
#199361=CARTESIAN_POINT('Ctrl Pts',(-19.1685460712486,17.1371002164304,
12.5389719551515));
#199362=CARTESIAN_POINT('Ctrl Pts',(-19.0586647937198,17.1189400600132,
12.5324828739332));
#199363=CARTESIAN_POINT('Ctrl Pts',(-19.0380857978338,17.1158499331011,
12.5312613540816));
#199364=CARTESIAN_POINT('Ctrl Pts',(-19.0086348516524,17.111870633958,12.5295030791257));
#199365=CARTESIAN_POINT('Ctrl Pts',(-18.9997972453777,17.1107332984181,
12.5289741616074));
#199366=CARTESIAN_POINT('Ctrl Pts',(-18.9844923597262,17.1088618172458,
12.5280558443821));
#199367=CARTESIAN_POINT('Ctrl Pts',(-18.9780283432306,17.1081016363325,
12.5276672715735));
#199368=CARTESIAN_POINT('Ctrl Pts',(-18.965612626409,17.1066995401261,12.5269194990817));
#199369=CARTESIAN_POINT('Ctrl Pts',(-18.9596614994,17.1060530361355,12.5265604481554));
#199370=CARTESIAN_POINT('Ctrl Pts',(-18.9441079262473,17.1044300819816,
12.5256203752755));
#199371=CARTESIAN_POINT('Ctrl Pts',(-18.9345014838396,17.1034940544986,
12.5250380859469));
#199372=CARTESIAN_POINT('Ctrl Pts',(-18.9013560507739,17.1004931186363,
12.5230230691564));
#199373=CARTESIAN_POINT('Ctrl Pts',(-18.8777897678921,17.0987566959106,
12.5215800839237));
#199374=CARTESIAN_POINT('Ctrl Pts',(-18.6899012424729,17.0880714299837,
12.5099892867828));
#199375=CARTESIAN_POINT('Ctrl Pts',(-18.5251026446632,17.0979186449067,
12.4992323462443));
#199376=CARTESIAN_POINT('Ctrl Pts',(-18.2370095520701,17.149179824324,12.4798950751947));
#199377=CARTESIAN_POINT('Ctrl Pts',(-18.1131619060435,17.1830284032977,
12.4714194782576));
#199378=CARTESIAN_POINT('Ctrl Pts',(-17.9819496658706,17.2320478461235,
12.4627331353316));
#199379=CARTESIAN_POINT('Ctrl Pts',(-17.9708089840001,17.2363175393153,
12.4619981516652));
#199380=CARTESIAN_POINT('Ctrl Pts',(-17.9550266066247,17.2425196935959,
12.4609611649867));
#199381=CARTESIAN_POINT('Ctrl Pts',(-17.9503550170327,17.2443747672336,
12.4606547457596));
#199382=CARTESIAN_POINT('Ctrl Pts',(-17.9423172603459,17.2475997233052,
12.460128501367));
#199383=CARTESIAN_POINT('Ctrl Pts',(-17.9389479469103,17.2489616618302,
12.4599082021403));
#199384=CARTESIAN_POINT('Ctrl Pts',(-17.9324232046092,17.2516186500808,
12.4594821804507));
#199385=CARTESIAN_POINT('Ctrl Pts',(-17.9292673986513,17.2529126490303,
12.4592763940596));
#199386=CARTESIAN_POINT('Ctrl Pts',(-17.9207641087769,17.2564233465748,
12.4587225883768));
#199387=CARTESIAN_POINT('Ctrl Pts',(-17.915422521203,17.2586543794999,12.4583754303163));
#199388=CARTESIAN_POINT('Ctrl Pts',(-17.8956466524546,17.2670096410848,
12.4570926423709));
#199389=CARTESIAN_POINT('Ctrl Pts',(-17.8812709872245,17.2732724355222,
12.4561650528904));
#199390=CARTESIAN_POINT('Ctrl Pts',(-17.7430903583886,17.3353068164049,
12.4472842084464));
#199391=CARTESIAN_POINT('Ctrl Pts',(-17.6248348617212,17.4027163594933,
12.4399460763045));
#199392=CARTESIAN_POINT('Ctrl Pts',(-17.3869268745972,17.5705115265166,
12.4241364496277));
#199393=CARTESIAN_POINT('Ctrl Pts',(-17.2702647311286,17.6737036667616,
12.4156781380246));
#199394=CARTESIAN_POINT('Ctrl Pts',(-17.1516501821509,17.8044757174082,
12.4053962458497));
#199395=CARTESIAN_POINT('Ctrl Pts',(-17.1375974593144,17.8204460157528,
12.4041479530037));
#199396=CARTESIAN_POINT('Ctrl Pts',(-17.117952018687,17.8434625288588,12.4023578734839));
#199397=CARTESIAN_POINT('Ctrl Pts',(-17.1121595738175,17.8503371317314,
12.401824324488));
#199398=CARTESIAN_POINT('Ctrl Pts',(-17.1022400721328,17.8622631523878,
12.4009005352025));
#199399=CARTESIAN_POINT('Ctrl Pts',(-17.0980922228448,17.8672971721862,
12.4005111491311));
#199400=CARTESIAN_POINT('Ctrl Pts',(-17.0901933116631,17.8769744376842,
12.3997636115105));
#199401=CARTESIAN_POINT('Ctrl Pts',(-17.0864384881928,17.8816145430272,
12.3994056173556));
#199402=CARTESIAN_POINT('Ctrl Pts',(-17.076722222468,17.8937260239067,12.398472291294));
#199403=CARTESIAN_POINT('Ctrl Pts',(-17.0707917163883,17.9012219422236,
12.397895727346));
#199404=CARTESIAN_POINT('Ctrl Pts',(-17.0507243607571,17.9269423297956,
12.3959208854994));
#199405=CARTESIAN_POINT('Ctrl Pts',(-17.0368350628012,17.9453570456137,
12.3945128903651));
#199406=CARTESIAN_POINT('Ctrl Pts',(-16.9204468115025,18.105028527019,12.3823500964375));
#199407=CARTESIAN_POINT('Ctrl Pts',(-16.8354969553638,18.2582087384392,
12.3709003220424));
#199408=CARTESIAN_POINT('Ctrl Pts',(-16.7375521487364,18.5013704792442,
12.3535792629893));
#199409=CARTESIAN_POINT('Ctrl Pts',(-16.7098729182018,18.5846697592452,
12.3477984751274));
#199410=CARTESIAN_POINT('Ctrl Pts',(-16.6777196923027,18.7061794436123,
12.3397724386492));
#199411=CARTESIAN_POINT('Ctrl Pts',(-16.6689904029987,18.7431663997934,
12.337382282039));
#199412=CARTESIAN_POINT('Ctrl Pts',(-16.6597186930948,18.7877937404118,
12.3345774078427));
#199413=CARTESIAN_POINT('Ctrl Pts',(-16.6582163734147,18.7952250393248,
12.334112953271));
#199414=CARTESIAN_POINT('Ctrl Pts',(-16.6559468864146,18.8067701570194,
12.333395603268));
#199415=CARTESIAN_POINT('Ctrl Pts',(-16.6551519572504,18.8108783626274,
12.333141168883));
#199416=CARTESIAN_POINT('Ctrl Pts',(-16.6537025994971,18.8184895869389,
12.3326713460469));
#199417=CARTESIAN_POINT('Ctrl Pts',(-16.6530448407578,18.8219918710046,
12.3324557746841));
#199418=CARTESIAN_POINT('Ctrl Pts',(-16.651580614975,18.8298982414754,12.3319705026637));
#199419=CARTESIAN_POINT('Ctrl Pts',(-16.6507792761641,18.8343032225971,
12.3317010960942));
#199420=CARTESIAN_POINT('Ctrl Pts',(-16.6484632857467,18.847267719656,12.3309109264659));
#199421=CARTESIAN_POINT('Ctrl Pts',(-16.6469873492618,18.8558341798744,
12.3303923115206));
#199422=CARTESIAN_POINT('Ctrl Pts',(-16.6369266417622,18.9164565890559,
12.3267453933397));
#199423=CARTESIAN_POINT('Ctrl Pts',(-16.6302369607937,18.9688129747234,
12.323716234339));
#199424=CARTESIAN_POINT('Ctrl Pts',(-16.6241263825108,19.0367559453065,
12.3198779382673));
#199425=CARTESIAN_POINT('Ctrl Pts',(-16.6229109796364,19.0521578235637,
12.3190139730767));
#199426=CARTESIAN_POINT('Ctrl Pts',(-16.6088148094335,19.2597393350508,
12.3074364942488));
#199427=CARTESIAN_POINT('Ctrl Pts',(-16.6220498949103,19.4527862645305,
12.2973487796074));
#199428=CARTESIAN_POINT('Ctrl Pts',(-16.6722361451746,19.6944870069274,
12.2833673376024));
#199429=CARTESIAN_POINT('Ctrl Pts',(-16.6852965369748,19.7471373608193,
12.2802433641807));
#199430=CARTESIAN_POINT('Ctrl Pts',(-16.7038666652338,19.8113387842336,
12.2763119385533));
#199431=CARTESIAN_POINT('Ctrl Pts',(-16.7074785647983,19.8234205051229,
12.2755667300639));
#199432=CARTESIAN_POINT('Ctrl Pts',(-16.7133503992139,19.8424407556411,
12.2743847595165));
#199433=CARTESIAN_POINT('Ctrl Pts',(-16.7155386777619,19.8494012262096,
12.2739503480734));
#199434=CARTESIAN_POINT('Ctrl Pts',(-16.7197038804549,19.8624143725247,
12.273134619844));
#199435=CARTESIAN_POINT('Ctrl Pts',(-16.721672218605,19.8684697261473,12.272753589508));
#199436=CARTESIAN_POINT('Ctrl Pts',(-16.7261319786537,19.8819819825727,
12.2719000492049));
#199437=CARTESIAN_POINT('Ctrl Pts',(-16.7286376740101,19.8894340432063,
12.2714270719034));
#199438=CARTESIAN_POINT('Ctrl Pts',(-16.7350795554196,19.9082449875085,
12.2702273846959));
#199439=CARTESIAN_POINT('Ctrl Pts',(-16.7390710537003,19.9195845088839,
12.2694988503244));
#199440=CARTESIAN_POINT('Ctrl Pts',(-16.7621577476356,19.98343035874,12.2653661441093));
#199441=CARTESIAN_POINT('Ctrl Pts',(-16.7832275648349,20.0351944647441,
12.2618965246258));
#199442=CARTESIAN_POINT('Ctrl Pts',(-16.816529360096,20.1085553443587,12.2568019291525));
#199443=CARTESIAN_POINT('Ctrl Pts',(-16.8271330774761,20.1308683169119,
12.255228055829));
#199444=CARTESIAN_POINT('Ctrl Pts',(-16.9240137138269,20.3258530013913,
12.2412626563793));
#199445=CARTESIAN_POINT('Ctrl Pts',(-17.0331261948717,20.4861325231692,
12.2281887719511));
#199446=CARTESIAN_POINT('Ctrl Pts',(-17.1904552002863,20.6604508922759,
12.2131470363264));
#199447=CARTESIAN_POINT('Ctrl Pts',(-17.2193953186728,20.6906660564634,
12.2105091550339));
#199448=CARTESIAN_POINT('Ctrl Pts',(-17.2547639797147,20.7254670424927,
12.207454467003));
#199449=CARTESIAN_POINT('Ctrl Pts',(-17.2603442726056,20.7308975057357,
12.2069773127093));
#199450=CARTESIAN_POINT('Ctrl Pts',(-17.2690012142695,20.7392295112354,
12.2062446335026));
#199451=CARTESIAN_POINT('Ctrl Pts',(-17.2720567400587,20.7421527639776,
12.20598746481));
#199452=CARTESIAN_POINT('Ctrl Pts',(-17.2777011869994,20.747520564473,12.20551507117));
#199453=CARTESIAN_POINT('Ctrl Pts',(-17.2802874985051,20.7499677193296,
12.2052996473295));
#199454=CARTESIAN_POINT('Ctrl Pts',(-17.2861001113746,20.7554398567681,
12.2048177851147));
#199455=CARTESIAN_POINT('Ctrl Pts',(-17.2893297141327,20.7584612514064,
12.2045516222799));
#199456=CARTESIAN_POINT('Ctrl Pts',(-17.2975849567799,20.7661359209603,
12.2038751937367));
#199457=CARTESIAN_POINT('Ctrl Pts',(-17.3026237972977,20.770775008866,12.2034659879044));
#199458=CARTESIAN_POINT('Ctrl Pts',(-17.3315905409576,20.7971851154393,
12.2011339065317));
#199459=CARTESIAN_POINT('Ctrl Pts',(-17.3559938654293,20.8184311371059,
12.1992480505197));
#199460=CARTESIAN_POINT('Ctrl Pts',(-17.3956018123434,20.8513493296863,
12.1962923396516));
#199461=CARTESIAN_POINT('Ctrl Pts',(-17.4104933713668,20.8633879316851,
12.1952037595441));
#199462=CARTESIAN_POINT('Ctrl Pts',(-17.4266898551028,20.876122007533,12.1940414813639));
#199463=CARTESIAN_POINT('Ctrl Pts',(-17.4278340242785,20.8770196753955,
12.1939594895363));
#199464=CARTESIAN_POINT('Ctrl Pts',(-17.447019000192,20.8920395034338,12.1925865926441));
#199465=CARTESIAN_POINT('Ctrl Pts',(-17.4652874247353,20.9058694227012,
12.1913075409787));
#199466=CARTESIAN_POINT('Ctrl Pts',(-17.5206377176417,20.9463752660136,
12.1875043870956));
#199467=CARTESIAN_POINT('Ctrl Pts',(-17.5583626918446,20.9721509015813,
12.1850067597534));
#199468=CARTESIAN_POINT('Ctrl Pts',(-17.689129410271,21.0554218194558,12.1765663359542));
#199469=CARTESIAN_POINT('Ctrl Pts',(-17.7857771936881,21.1069216817362,
12.1706782404404));
#199470=CARTESIAN_POINT('Ctrl Pts',(-17.9364617815969,21.1727999192604,
12.1615338918867));
#199471=CARTESIAN_POINT('Ctrl Pts',(-17.987796765582,21.1928946038052,12.1584263684373));
#199472=CARTESIAN_POINT('Ctrl Pts',(-18.0722657029889,21.2222120073014,
12.1532823466898));
#199473=CARTESIAN_POINT('Ctrl Pts',(-18.1049439143532,21.2326711559176,
12.1512852362614));
#199474=CARTESIAN_POINT('Ctrl Pts',(-18.1482320484398,21.245375024352,12.1486245907639));
#199475=CARTESIAN_POINT('Ctrl Pts',(-18.1586265744733,21.2483392568301,
12.1479845839832));
#199476=CARTESIAN_POINT('Ctrl Pts',(-18.1756912044482,21.2530646105462,
12.146931876613));
#199477=CARTESIAN_POINT('Ctrl Pts',(-18.1823481042419,21.2548729826021,
12.146520717311));
#199478=CARTESIAN_POINT('Ctrl Pts',(-18.1952528754523,21.2583109745416,
12.1457226487722));
#199479=CARTESIAN_POINT('Ctrl Pts',(-18.2014996048667,21.2599446108758,
12.1453358749131));
#199480=CARTESIAN_POINT('Ctrl Pts',(-18.2159429949385,21.2636513152125,
12.1444404954634));
#199481=CARTESIAN_POINT('Ctrl Pts',(-18.2241447552368,21.265703898007,12.1439312337399));
#199482=CARTESIAN_POINT('Ctrl Pts',(-18.2462414749576,21.2710934017997,
12.1425569202425));
#199483=CARTESIAN_POINT('Ctrl Pts',(-18.2601581040461,21.2743388099902,
12.1416889403682));
#199484=CARTESIAN_POINT('Ctrl Pts',(-18.3881653422859,21.3028272449374,
12.1336815980427));
#199485=CARTESIAN_POINT('Ctrl Pts',(-18.5041113826693,21.3187206289427,
12.1262404516991));
#199486=CARTESIAN_POINT('Ctrl Pts',(-18.7832499910539,21.3336733342703,
12.1079811237119));
#199487=CARTESIAN_POINT('Ctrl Pts',(-18.9461969566186,21.3236145342229,
12.0970228873341));
#199488=CARTESIAN_POINT('Ctrl Pts',(-19.1383852166641,21.2892729526618,
12.084617373784));
#199489=CARTESIAN_POINT('Ctrl Pts',(-19.1702539702209,21.2828177070633,
12.0825798186054));
#199490=CARTESIAN_POINT('Ctrl Pts',(-19.2090239588168,21.274030211197,12.0801352718031));
#199491=CARTESIAN_POINT('Ctrl Pts',(-19.2160764625761,21.2723936308914,
12.0796919911676));
#199492=CARTESIAN_POINT('Ctrl Pts',(-19.2271190504475,21.2697713548855,
12.0790002604906));
#199493=CARTESIAN_POINT('Ctrl Pts',(-19.231114818645,21.2688101825384,12.0787504396736));
#199494=CARTESIAN_POINT('Ctrl Pts',(-19.2385781745122,21.2669918832874,
12.0782847559777));
#199495=CARTESIAN_POINT('Ctrl Pts',(-19.2420463537293,21.2661376258125,
12.0780687376301));
#199496=CARTESIAN_POINT('Ctrl Pts',(-19.2499579912323,21.2641676355279,
12.0775768110802));
#199497=CARTESIAN_POINT('Ctrl Pts',(-19.2543999916097,21.2630462562851,
12.0773012320426));
#199498=CARTESIAN_POINT('Ctrl Pts',(-19.2680410859687,21.2595554312031,
12.0764567366496));
#199499=CARTESIAN_POINT('Ctrl Pts',(-19.2772280462382,21.2571384443878,
12.0758904944011));
#199500=CARTESIAN_POINT('Ctrl Pts',(-19.3595522765203,21.2348863090597,
12.0708363810609));
#199501=CARTESIAN_POINT('Ctrl Pts',(-19.4316001034628,21.2111970235066,
12.066554286132));
#199502=CARTESIAN_POINT('Ctrl Pts',(-19.5420516518056,21.1681836503344,
12.0599934978968));
#199503=CARTESIAN_POINT('Ctrl Pts',(-19.5813962524043,21.1514729039001,
12.0576573597134));
#199504=CARTESIAN_POINT('Ctrl Pts',(-19.7194906370005,21.0878186822561,
12.0493787756542));
#199505=CARTESIAN_POINT('Ctrl Pts',(-19.8150773315717,21.0344338698914,
12.0434920757181));
#199506=CARTESIAN_POINT('Ctrl Pts',(-19.9519739052804,20.9434150514362,
12.0343509716056));
#199507=CARTESIAN_POINT('Ctrl Pts',(-19.99662744481,20.911145180756,12.0312453077688));
#199508=CARTESIAN_POINT('Ctrl Pts',(-20.0669593725278,20.8560180127472,
12.0261040899131));
#199509=CARTESIAN_POINT('Ctrl Pts',(-20.0934295932457,20.8342116115107,
12.0241078674788));
#199510=CARTESIAN_POINT('Ctrl Pts',(-20.1275293167234,20.8047006737721,
12.0214482373828));
#199511=CARTESIAN_POINT('Ctrl Pts',(-20.13564675635,20.7975661530511,12.0208083350939));
#199512=CARTESIAN_POINT('Ctrl Pts',(-20.1488551340384,20.7857766600723,
12.0197557558168));
#199513=CARTESIAN_POINT('Ctrl Pts',(-20.1539786398635,20.7811583487098,
12.0193446193799));
#199514=CARTESIAN_POINT('Ctrl Pts',(-20.1638543628842,20.7721685346796,
12.0185465639283));
#199515=CARTESIAN_POINT('Ctrl Pts',(-20.1686093355817,20.7678001623721,
12.0181597801255));
#199516=CARTESIAN_POINT('Ctrl Pts',(-20.1795448211767,20.7576611356858,
12.0172643320591));
#199517=CARTESIAN_POINT('Ctrl Pts',(-20.1857108626406,20.7518750977034,
12.0167550113461));
#199518=CARTESIAN_POINT('Ctrl Pts',(-20.2022061766497,20.7362094679103,
12.0153804354348));
#199519=CARTESIAN_POINT('Ctrl Pts',(-20.2124701917325,20.7262620811548,
12.0145122503961));
#199520=CARTESIAN_POINT('Ctrl Pts',(-20.3058953921581,20.6338659161811,
12.0064890871795));
#199521=CARTESIAN_POINT('Ctrl Pts',(-20.3821685714459,20.5447672374127,
11.9990309400375));
#199522=CARTESIAN_POINT('Ctrl Pts',(-20.5463777395271,20.3172193552303,
11.9806998495973));
#199523=CARTESIAN_POINT('Ctrl Pts',(-20.6263877497714,20.1739658026081,
11.9696847113564));
#199524=CARTESIAN_POINT('Ctrl Pts',(-20.7008875653749,19.9945721115513,
11.9573529102966));
#199525=CARTESIAN_POINT('Ctrl Pts',(-20.7120470405025,19.965958323262,11.9554288912061));
#199526=CARTESIAN_POINT('Ctrl Pts',(-20.7225806064515,19.9371103026709,
11.953538761502));
#199527=CARTESIAN_POINT('',(-20.8516474773841,19.2091064840258,12.4890562790225));
#199528=CARTESIAN_POINT('Ctrl Pts',(-20.8516474773841,19.2091064840258,
12.4890562790225));
#199529=CARTESIAN_POINT('Ctrl Pts',(-20.8529701850388,19.0661177649361,
12.4804472042752));
#199530=CARTESIAN_POINT('Ctrl Pts',(-20.7745205055235,18.2204815862945,
12.4294461939675));
#199531=CARTESIAN_POINT('Ctrl Pts',(-19.6371491691806,16.8763368280626,
12.336053248099));
#199532=CARTESIAN_POINT('Ctrl Pts',(-17.2597752565566,17.1878855805931,
12.2088774414178));
#199533=CARTESIAN_POINT('Ctrl Pts',(-16.2349110453346,19.3555162442872,
12.0817016347362));
#199534=CARTESIAN_POINT('Ctrl Pts',(-17.5028058390645,21.3905622235373,
11.9545258280549));
#199535=CARTESIAN_POINT('Ctrl Pts',(-19.6892758345617,21.4228771276963,
11.838541194803));
#199536=CARTESIAN_POINT('Ctrl Pts',(-20.5391741519826,20.4226738690892,
11.7649484971116));
#199537=CARTESIAN_POINT('Ctrl Pts',(-20.7219730492699,19.9368789336487,
11.7337477349808));
#199538=CARTESIAN_POINT('Ctrl Pts',(-20.8509991358365,19.209087183383,12.489429393495));
#199539=CARTESIAN_POINT('Ctrl Pts',(-20.8511371264887,19.3618075690115,
12.4977330855385));
#199540=CARTESIAN_POINT('Ctrl Pts',(-20.8347500521367,19.5140860427722,
12.5059642009009));
#199541=CARTESIAN_POINT('Ctrl Pts',(-20.7967940657989,19.6876464450794,
12.5161562698567));
#199542=CARTESIAN_POINT('Ctrl Pts',(-20.7910349565221,19.7119174639306,
12.5175993915336));
#199543=CARTESIAN_POINT('Ctrl Pts',(-20.7816382558835,19.7486189113664,
12.5198116649265));
#199544=CARTESIAN_POINT('Ctrl Pts',(-20.7783131362579,19.7611275404856,
12.5205709996961));
#199545=CARTESIAN_POINT('Ctrl Pts',(-20.7719302797975,19.7842816365704,
12.5219869115254));
#199546=CARTESIAN_POINT('Ctrl Pts',(-20.7689032850522,19.7949351621357,
12.5226424844955));
#199547=CARTESIAN_POINT('Ctrl Pts',(-20.7638390421021,19.8122411000255,
12.5237142877202));
#199548=CARTESIAN_POINT('Ctrl Pts',(-20.7618523246356,19.818908171434,12.5241288655344));
#199549=CARTESIAN_POINT('Ctrl Pts',(-20.7579646561404,19.8317233543802,
12.5249290164279));
#199550=CARTESIAN_POINT('Ctrl Pts',(-20.7560684601301,19.8378728364728,
12.5253144298941));
#199551=CARTESIAN_POINT('Ctrl Pts',(-20.7516570332761,19.8519510801957,
12.5262001515466));
#199552=CARTESIAN_POINT('Ctrl Pts',(-20.7491230627168,19.8598738168205,
12.5267010712896));
#199553=CARTESIAN_POINT('Ctrl Pts',(-20.7422545061787,19.8809207944706,
12.5280384508754));
#199554=CARTESIAN_POINT('Ctrl Pts',(-20.7378380266801,19.8940177018656,
12.528877598968));
#199555=CARTESIAN_POINT('Ctrl Pts',(-20.7297977044651,19.9171115879249,
12.5303698152429));
#199556=CARTESIAN_POINT('Ctrl Pts',(-20.7262265520042,19.9271252405564,
12.5310210574263));
#199557=CARTESIAN_POINT('Ctrl Pts',(-20.7225806018034,19.9371103154006,
12.5316746994897));
#199558=CARTESIAN_POINT('Origin',(-18.734,19.211,0.));
#199559=CARTESIAN_POINT('',(-20.722580608645,19.9371102966638,13.5571445218548));
#199560=CARTESIAN_POINT('',(-20.7225805710824,19.9371103995355,13.3344633171505));
#199561=CARTESIAN_POINT('',(-20.7225806064498,19.9371103026755,0.));
#199562=CARTESIAN_POINT('Ctrl Pts',(-20.722580608645,19.9371102966638,13.5571445218548));
#199563=CARTESIAN_POINT('Ctrl Pts',(-20.7282459073958,19.9215948807692,
13.5562052644303));
#199564=CARTESIAN_POINT('Ctrl Pts',(-20.7337298132394,19.9060126420946,
13.5552608856393));
#199565=CARTESIAN_POINT('Ctrl Pts',(-20.750223161395,19.8573354325802,13.5523054576032));
#199566=CARTESIAN_POINT('Ctrl Pts',(-20.7605967221015,19.8240341325958,
13.5502759196125));
#199567=CARTESIAN_POINT('Ctrl Pts',(-20.773119092699,19.780034764304,13.5475782150195));
#199568=CARTESIAN_POINT('Ctrl Pts',(-20.7760149188631,19.7695537589714,
13.5469344214741));
#199569=CARTESIAN_POINT('Ctrl Pts',(-20.7806193225015,19.7523742976286,
13.545877071117));
#199570=CARTESIAN_POINT('Ctrl Pts',(-20.7823760846193,19.7456888773732,
13.5454650823657));
#199571=CARTESIAN_POINT('Ctrl Pts',(-20.7857090367791,19.7327476847868,
13.544666531175));
#199572=CARTESIAN_POINT('Ctrl Pts',(-20.7872894372499,19.7264930684602,
13.5442801100892));
#199573=CARTESIAN_POINT('Ctrl Pts',(-20.7908666323442,19.7120584358001,
13.5433871819095));
#199574=CARTESIAN_POINT('Ctrl Pts',(-20.7928432517009,19.7038735751324,
13.5428800299894));
#199575=CARTESIAN_POINT('Ctrl Pts',(-20.7980153378751,19.6818826823534,
13.5415150903552));
#199576=CARTESIAN_POINT('Ctrl Pts',(-20.801121053926,19.6680561766484,13.5406544363613));
#199577=CARTESIAN_POINT('Ctrl Pts',(-20.835418189784,19.5078618821578,13.5306528589752));
#199578=CARTESIAN_POINT('Ctrl Pts',(-20.851137506266,19.3586426934896,13.521001335935));
#199579=CARTESIAN_POINT('Ctrl Pts',(-20.8508605240914,19.0592697719238,
13.5012717751918));
#199580=CARTESIAN_POINT('Ctrl Pts',(-20.8348287881357,18.9099266958755,
13.4912566176988));
#199581=CARTESIAN_POINT('Ctrl Pts',(-20.799845502621,18.748162883075,13.4809318733944));
#199582=CARTESIAN_POINT('Ctrl Pts',(-20.7963536195627,18.7328437297549,
13.4799597814493));
#199583=CARTESIAN_POINT('Ctrl Pts',(-20.7913410449669,18.7119304769614,
13.4786418129792));
#199584=CARTESIAN_POINT('Ctrl Pts',(-20.7899675523549,18.7063020808353,
13.4782880141239));
#199585=CARTESIAN_POINT('Ctrl Pts',(-20.7877485339382,18.6973682262046,
13.4777279559423));
#199586=CARTESIAN_POINT('Ctrl Pts',(-20.7869181049378,18.6940590995997,
13.4775208409079));
#199587=CARTESIAN_POINT('Ctrl Pts',(-20.785186732014,18.6872298278594,13.4770941107266));
#199588=CARTESIAN_POINT('Ctrl Pts',(-20.784284724454,18.683709992855,13.4768745642414));
#199589=CARTESIAN_POINT('Ctrl Pts',(-20.7821142198579,18.6753299779801,
13.4763527700331));
#199590=CARTESIAN_POINT('Ctrl Pts',(-20.7808374691826,18.6704719193154,
13.4760509980924));
#199591=CARTESIAN_POINT('Ctrl Pts',(-20.7764750782533,18.6541100545507,
13.4750369304475));
#199592=CARTESIAN_POINT('Ctrl Pts',(-20.7733095867119,18.6426275157399,
13.4743291031207));
#199593=CARTESIAN_POINT('Ctrl Pts',(-20.735765065069,18.5107911399019,13.4662399460591));
#199594=CARTESIAN_POINT('Ctrl Pts',(-20.6908688888608,18.3936696445328,
13.459408366111));
#199595=CARTESIAN_POINT('Ctrl Pts',(-20.5622080644684,18.1305007323441,
13.4434862170804));
#199596=CARTESIAN_POINT('Ctrl Pts',(-20.470900901101,17.9891196006906,13.4344327670586));
#199597=CARTESIAN_POINT('Ctrl Pts',(-20.3488895819459,17.8419229993028,
13.4233283739655));
#199598=CARTESIAN_POINT('Ctrl Pts',(-20.3336077748065,17.8240987426217,
13.4219533731892));
#199599=CARTESIAN_POINT('Ctrl Pts',(-20.3116466034115,17.7993297599487,
13.419997374714));
#199600=CARTESIAN_POINT('Ctrl Pts',(-20.3052111006416,17.7921704314923,
13.4194265313305));
#199601=CARTESIAN_POINT('Ctrl Pts',(-20.2946981094222,17.7806342461468,
13.4184976525528));
#199602=CARTESIAN_POINT('Ctrl Pts',(-20.2906504602041,17.7762302895008,
13.4181408833058));
#199603=CARTESIAN_POINT('Ctrl Pts',(-20.2821571001986,17.7670675211936,
13.4173940172811));
#199604=CARTESIAN_POINT('Ctrl Pts',(-20.277707991829,17.7623119574112,13.4170037770794));
#199605=CARTESIAN_POINT('Ctrl Pts',(-20.2671051402753,17.7510830843432,
13.4160760788625));
#199606=CARTESIAN_POINT('Ctrl Pts',(-20.2609322705816,17.7446280795804,
13.4155377970484));
#199607=CARTESIAN_POINT('Ctrl Pts',(-20.2401569273135,17.7231766119986,
13.4137320446068));
#199608=CARTESIAN_POINT('Ctrl Pts',(-20.2253732794107,17.7083580547387,
13.4124566646547));
#199609=CARTESIAN_POINT('Ctrl Pts',(-20.1447384548318,17.629895070409,13.4055489437137));
#199610=CARTESIAN_POINT('Ctrl Pts',(-20.0750377426678,17.5703629982089,
13.3997422941687));
#199611=CARTESIAN_POINT('Ctrl Pts',(-19.9260796328734,17.4589860280167,
13.3876785533894));
#199612=CARTESIAN_POINT('Ctrl Pts',(-19.8467533944115,17.4075630111075,
13.3814262633459));
#199613=CARTESIAN_POINT('Ctrl Pts',(-19.6994150670681,17.3254832687996,
13.3702890413442));
#199614=CARTESIAN_POINT('Ctrl Pts',(-19.6327063786031,17.2927904984049,
13.3654069071643));
#199615=CARTESIAN_POINT('Ctrl Pts',(-19.5255532053833,17.2470963944471,
13.357938199605));
#199616=CARTESIAN_POINT('Ctrl Pts',(-19.4862011994339,17.2316900806288,
13.355271086146));
#199617=CARTESIAN_POINT('Ctrl Pts',(-19.4393956549596,17.214963557571,13.3522082005009));
#199618=CARTESIAN_POINT('Ctrl Pts',(-19.4323664137032,17.2124933411401,
13.3517510810436));
#199619=CARTESIAN_POINT('Ctrl Pts',(-19.4209708585323,17.2085561798213,
13.3510148095728));
#199620=CARTESIAN_POINT('Ctrl Pts',(-19.4166126125033,17.2070663095747,
13.3507343516266));
#199621=CARTESIAN_POINT('Ctrl Pts',(-19.4088636482934,17.2044455323962,
13.3502377462513));
#199622=CARTESIAN_POINT('Ctrl Pts',(-19.4054748984273,17.2033089787763,
13.3500212686018));
#199623=CARTESIAN_POINT('Ctrl Pts',(-19.3981986887382,17.2008890925199,
13.3495579564602));
#199624=CARTESIAN_POINT('Ctrl Pts',(-19.3943103912965,17.1996084552503,
13.3493112814047));
#199625=CARTESIAN_POINT('Ctrl Pts',(-19.3836044811085,17.1961167810974,
13.3486345380573));
#199626=CARTESIAN_POINT('Ctrl Pts',(-19.3767792439967,17.193929050697,13.3482058205599));
#199627=CARTESIAN_POINT('Ctrl Pts',(-19.3399295113016,17.182323440626,13.3459051370449));
#199628=CARTESIAN_POINT('Ctrl Pts',(-19.3097072577266,17.1735406636963,
13.3440681326239));
#199629=CARTESIAN_POINT('Ctrl Pts',(-19.1212225221389,17.1232951591185,
13.3328547613254));
#199630=CARTESIAN_POINT('Ctrl Pts',(-18.9587779444252,17.0996165893947,
13.324209424332));
#199631=CARTESIAN_POINT('Ctrl Pts',(-18.6781394236988,17.0914986017331,
13.3088409293912));
#199632=CARTESIAN_POINT('Ctrl Pts',(-18.5610028530007,17.0978333525961,
13.302303466778));
#199633=CARTESIAN_POINT('Ctrl Pts',(-18.4308397129408,17.1157703822688,
13.2946060493309));
#199634=CARTESIAN_POINT('Ctrl Pts',(-18.416700193534,17.1178649999192,13.2937643190609));
#199635=CARTESIAN_POINT('Ctrl Pts',(-18.3942316652004,17.1214263641796,
13.2924174498814));
#199636=CARTESIAN_POINT('Ctrl Pts',(-18.3858882083006,17.1228001345264,
13.2919152541721));
#199637=CARTESIAN_POINT('Ctrl Pts',(-18.3711884695595,17.1253110283683,
13.291026765892));
#199638=CARTESIAN_POINT('Ctrl Pts',(-18.3648287049276,17.1264273228128,
13.2906411397131));
#199639=CARTESIAN_POINT('Ctrl Pts',(-18.3516858575842,17.1287962455108,
13.289841639869));
#199640=CARTESIAN_POINT('Ctrl Pts',(-18.3449035985754,17.1300529638296,
13.2894276400311));
#199641=CARTESIAN_POINT('Ctrl Pts',(-18.3275113951464,17.1333636499252,
13.2883622771834));
#199642=CARTESIAN_POINT('Ctrl Pts',(-18.3169109137869,17.1354657371154,
13.2877093854886));
#199643=CARTESIAN_POINT('Ctrl Pts',(-18.2727439680525,17.144576110914,13.2849739480399));
#199644=CARTESIAN_POINT('Ctrl Pts',(-18.2393357166929,17.1523179344066,
13.2828680842396));
#199645=CARTESIAN_POINT('Ctrl Pts',(-18.1527992406153,17.1745993531266,
13.2773138060491));
#199646=CARTESIAN_POINT('Ctrl Pts',(-18.1000269379603,17.1904062124275,
13.2738270096537));
#199647=CARTESIAN_POINT('Ctrl Pts',(-17.9444686966766,17.2436945681668,
13.2632580291975));
#199648=CARTESIAN_POINT('Ctrl Pts',(-17.8439124039957,17.2871000686388,
13.256027452449));
#199649=CARTESIAN_POINT('Ctrl Pts',(-17.7067682895232,17.3593603919983,
13.2457874379338));
#199650=CARTESIAN_POINT('Ctrl Pts',(-17.6670671255388,17.3819487003336,
13.2427765413148));
#199651=CARTESIAN_POINT('Ctrl Pts',(-17.6086447268562,17.4177385859405,
13.2383012730214));
#199652=CARTESIAN_POINT('Ctrl Pts',(-17.5893566555011,17.4299883053796,
13.2368162492262));
#199653=CARTESIAN_POINT('Ctrl Pts',(-17.5696842356408,17.4429337419373,
13.2352964308223));
#199654=CARTESIAN_POINT('Ctrl Pts',(-17.5690984633031,17.4433196267881,
13.2352511714255));
#199655=CARTESIAN_POINT('Ctrl Pts',(-17.5591293207858,17.4498940314335,
13.2344808304781));
#199656=CARTESIAN_POINT('Ctrl Pts',(-17.5497950416684,17.4561569955931,
13.2337583344831));
#199657=CARTESIAN_POINT('Ctrl Pts',(-17.5073067497728,17.4851585057362,
13.230465528539));
#199658=CARTESIAN_POINT('Ctrl Pts',(-17.4747523302698,17.5087658851297,
13.2279309371078));
#199659=CARTESIAN_POINT('Ctrl Pts',(-17.4370703308376,17.5377647151626,
13.2250016017706));
#199660=CARTESIAN_POINT('Ctrl Pts',(-17.4312761266593,17.5422719219111,
13.2245513024591));
#199661=CARTESIAN_POINT('Ctrl Pts',(-17.4219107699467,17.5496355722622,
13.2238238468773));
#199662=CARTESIAN_POINT('Ctrl Pts',(-17.418325279334,17.5524735637678,13.2235454339716));
#199663=CARTESIAN_POINT('Ctrl Pts',(-17.411956117236,17.5575485418906,13.2230510744505));
#199664=CARTESIAN_POINT('Ctrl Pts',(-17.4091688891385,17.5597809713361,
13.2228348089525));
#199665=CARTESIAN_POINT('Ctrl Pts',(-17.4031816373139,17.5646013780041,
13.2223704131566));
#199666=CARTESIAN_POINT('Ctrl Pts',(-17.3999835167876,17.5671916291267,
13.2221224503915));
#199667=CARTESIAN_POINT('Ctrl Pts',(-17.3911600059624,17.5743807577062,
13.2214385327544));
#199668=CARTESIAN_POINT('Ctrl Pts',(-17.3855506458471,17.5789993454052,
13.2210039766082));
#199669=CARTESIAN_POINT('Ctrl Pts',(-17.3546780548679,17.6046868028498,
13.2186128536975));
#199670=CARTESIAN_POINT('Ctrl Pts',(-17.3298832676818,17.62631467228,13.2166945800168));
#199671=CARTESIAN_POINT('Ctrl Pts',(-17.1857539564765,17.7580752175109,
13.2054867681597));
#199672=CARTESIAN_POINT('Ctrl Pts',(-17.078897780358,17.8810734656102,13.1969034242001));
#199673=CARTESIAN_POINT('Ctrl Pts',(-16.9212025345497,18.1114174523548,
13.1816207316834));
#199674=CARTESIAN_POINT('Ctrl Pts',(-16.8633460336548,18.2130195810622,
13.1751035442016));
#199675=CARTESIAN_POINT('Ctrl Pts',(-16.8081394607258,18.3318217758328,
13.1674289498601));
#199676=CARTESIAN_POINT('Ctrl Pts',(-16.8022494467284,18.3448401119813,
13.1665875123647));
#199677=CARTESIAN_POINT('Ctrl Pts',(-16.7930849391628,18.365654388574,13.1652410241529));
#199678=CARTESIAN_POINT('Ctrl Pts',(-16.78972452393,18.3734121860173,13.1647389140015));
#199679=CARTESIAN_POINT('Ctrl Pts',(-16.7838798137614,18.3871298954707,
13.1638505253839));
#199680=CARTESIAN_POINT('Ctrl Pts',(-16.7813761337724,18.3930814676722,
13.16346491283));
#199681=CARTESIAN_POINT('Ctrl Pts',(-16.7762539527176,18.4054151185397,
13.1626653904539));
#199682=CARTESIAN_POINT('Ctrl Pts',(-16.7736393439993,18.4117987215101,
13.1622513542088));
#199683=CARTESIAN_POINT('Ctrl Pts',(-16.7670078690167,18.4282179076416,
13.1611857907113));
#199684=CARTESIAN_POINT('Ctrl Pts',(-16.7630366189024,18.4382715929561,
13.1605327336622));
#199685=CARTESIAN_POINT('Ctrl Pts',(-16.7467811521142,18.4803648781251,
13.1577956937372));
#199686=CARTESIAN_POINT('Ctrl Pts',(-16.7352003966803,18.5126688750892,
13.1556883586312));
#199687=CARTESIAN_POINT('Ctrl Pts',(-16.70707472939,18.5975657355916,13.1501292744112));
#199688=CARTESIAN_POINT('Ctrl Pts',(-16.6917908493953,18.6505460653424,
13.1466390604284));
#199689=CARTESIAN_POINT('Ctrl Pts',(-16.6523927377921,18.8102868827723,
13.1360635151584));
#199690=CARTESIAN_POINT('Ctrl Pts',(-16.6344692945024,18.9183788325335,
13.1288298130631));
#199691=CARTESIAN_POINT('Ctrl Pts',(-16.6206804354889,19.0767390065439,
13.1183294300833));
#199692=CARTESIAN_POINT('Ctrl Pts',(-16.6181162941577,19.1262533336285,
13.1150620266067));
#199693=CARTESIAN_POINT('Ctrl Pts',(-16.6170162590124,19.1924272790692,
13.1107467113952));
#199694=CARTESIAN_POINT('Ctrl Pts',(-16.6169356878532,19.2090444000759,
13.1096674498783));
#199695=CARTESIAN_POINT('Ctrl Pts',(-16.6174195000452,19.2789033939328,
13.1051526981619));
#199696=CARTESIAN_POINT('Ctrl Pts',(-16.6197967557899,19.3321179478195,
13.1017682289513));
#199697=CARTESIAN_POINT('Ctrl Pts',(-16.6248955339115,19.3938750486984,
13.0979456663442));
#199698=CARTESIAN_POINT('Ctrl Pts',(-16.6256661577767,19.4025550783555,
13.0974108378647));
#199699=CARTESIAN_POINT('Ctrl Pts',(-16.6269142732002,19.4156920293778,
13.0966053368395));
#199700=CARTESIAN_POINT('Ctrl Pts',(-16.627352348132,19.420152477174,13.0963325309955));
#199701=CARTESIAN_POINT('Ctrl Pts',(-16.6281641899434,19.4281571825308,
13.0958442338215));
#199702=CARTESIAN_POINT('Ctrl Pts',(-16.6285327425798,19.4317019015688,
13.0956284548083));
#199703=CARTESIAN_POINT('Ctrl Pts',(-16.6293531076128,19.4394030150423,
13.0951606516315));
#199704=CARTESIAN_POINT('Ctrl Pts',(-16.6298082800898,19.4435589935281,
13.094908818839));
#199705=CARTESIAN_POINT('Ctrl Pts',(-16.6311216474387,19.4552311673385,
13.0942032185742));
#199706=CARTESIAN_POINT('Ctrl Pts',(-16.632007832681,19.4627442376995,13.0937509992246));
#199707=CARTESIAN_POINT('Ctrl Pts',(-16.6375516847289,19.5076733950392,
13.0910575238554));
#199708=CARTESIAN_POINT('Ctrl Pts',(-16.6431683078155,19.5449668737488,
13.0888668727374));
#199709=CARTESIAN_POINT('Ctrl Pts',(-16.6649490001153,19.6672968481861,
13.0817718359432));
#199710=CARTESIAN_POINT('Ctrl Pts',(-16.6853312226077,19.7514974222934,
13.077031836201));
#199711=CARTESIAN_POINT('Ctrl Pts',(-16.7626652808814,20.0025507386355,
13.0627369267368));
#199712=CARTESIAN_POINT('Ctrl Pts',(-16.8353145540425,20.1637329397712,
13.0532706872202));
#199713=CARTESIAN_POINT('Ctrl Pts',(-16.9390353979865,20.3336386538017,
13.0417029093244));
#199714=CARTESIAN_POINT('Ctrl Pts',(-16.9513079978244,20.3530265471152,
13.0403586266725));
#199715=CARTESIAN_POINT('Ctrl Pts',(-16.969125019228,20.3801861641347,13.0384390109132));
#199716=CARTESIAN_POINT('Ctrl Pts',(-16.974410859894,20.3881261774568,13.0378733220956));
#199717=CARTESIAN_POINT('Ctrl Pts',(-16.9830894024727,20.4009733889527,
13.0369505591202));
#199718=CARTESIAN_POINT('Ctrl Pts',(-16.9864495435496,20.4059025014566,
13.0365947179496));
#199719=CARTESIAN_POINT('Ctrl Pts',(-16.9935290003468,20.4161938790851,
13.0358479457907));
#199720=CARTESIAN_POINT('Ctrl Pts',(-16.997252361775,20.4215532728706,13.0354568631987));
#199721=CARTESIAN_POINT('Ctrl Pts',(-17.0061733991523,20.4342683099771,
13.0345237557428));
#199722=CARTESIAN_POINT('Ctrl Pts',(-17.0113933222732,20.4416081223215,
13.0339808811173));
#199723=CARTESIAN_POINT('Ctrl Pts',(-17.0291578474941,20.4662525842667,
13.0321436092435));
#199724=CARTESIAN_POINT('Ctrl Pts',(-17.0419173099536,20.4834000678817,
13.0308409206414));
#199725=CARTESIAN_POINT('Ctrl Pts',(-17.1129411707734,20.5758913795751,
13.0236779279189));
#199726=CARTESIAN_POINT('Ctrl Pts',(-17.1759722637987,20.6474210901233,
13.0176285599478));
#199727=CARTESIAN_POINT('Ctrl Pts',(-17.3647447806782,20.8345545074701,
13.0003560112373));
#199728=CARTESIAN_POINT('Ctrl Pts',(-17.4999563804146,20.9395607566476,
12.9888459807993));
#199729=CARTESIAN_POINT('Ctrl Pts',(-17.6778502601351,21.0460992780768,
12.9756116400919));
#199730=CARTESIAN_POINT('Ctrl Pts',(-17.7098920808618,21.0641716003169,
12.9732981934057));
#199731=CARTESIAN_POINT('Ctrl Pts',(-17.7487000691313,21.0847459923291,
12.9705933106989));
#199732=CARTESIAN_POINT('Ctrl Pts',(-17.755026463378,21.0880590868298,12.9701553906861));
#199733=CARTESIAN_POINT('Ctrl Pts',(-17.7653773241287,21.0934132041429,
12.9694439645255));
#199734=CARTESIAN_POINT('Ctrl Pts',(-17.7693917053173,21.0954734537915,
12.9691692891368));
#199735=CARTESIAN_POINT('Ctrl Pts',(-17.7765904065161,21.0991389213428,
12.9686789872335));
#199736=CARTESIAN_POINT('Ctrl Pts',(-17.7797722117947,21.1007489369777,
12.9684630626108));
#199737=CARTESIAN_POINT('Ctrl Pts',(-17.786672952114,21.1042188868042,12.9679964714297));
#199738=CARTESIAN_POINT('Ctrl Pts',(-17.7903932914092,21.1060759006419,
12.967745988007));
#199739=CARTESIAN_POINT('Ctrl Pts',(-17.8008038820364,21.1112341071183,
12.9670479702103));
#199740=CARTESIAN_POINT('Ctrl Pts',(-17.8075062238379,21.114510951618,12.9666019309341));
#199741=CARTESIAN_POINT('Ctrl Pts',(-17.8465891774246,21.1333636830468,
12.964019571208));
#199742=CARTESIAN_POINT('Ctrl Pts',(-17.8793469039137,21.1481495887896,
12.9619291200903));
#199743=CARTESIAN_POINT('Ctrl Pts',(-17.9859982380772,21.1930564458303,
12.9553091718838));
#199744=CARTESIAN_POINT('Ctrl Pts',(-18.0612266799572,21.2198385793404,
12.950919902283));
#199745=CARTESIAN_POINT('Ctrl Pts',(-18.3163865067015,21.294730178849,12.9364216409884));
#199746=CARTESIAN_POINT('Ctrl Pts',(-18.5010916551091,21.3233636582702,
12.9264692745726));
#199747=CARTESIAN_POINT('Ctrl Pts',(-18.7092084766712,21.3279697344123,
12.9143615696649));
#199748=CARTESIAN_POINT('Ctrl Pts',(-18.7312649157707,21.3281131149387,
12.9130685803715));
#199749=CARTESIAN_POINT('Ctrl Pts',(-18.76176960561,21.3278347285684,12.9112652848019));
#199750=CARTESIAN_POINT('Ctrl Pts',(-18.7702196015889,21.327707007685,12.910764164821));
#199751=CARTESIAN_POINT('Ctrl Pts',(-18.7847430870114,21.3274004951778,
12.9099000314596));
#199752=CARTESIAN_POINT('Ctrl Pts',(-18.7908170301856,21.3272461437095,
12.9095377866375));
#199753=CARTESIAN_POINT('Ctrl Pts',(-18.8033375603729,21.3268740293785,
12.9087892828695));
#199754=CARTESIAN_POINT('Ctrl Pts',(-18.8097839787012,21.3266529471114,
12.9084029236745));
#199755=CARTESIAN_POINT('Ctrl Pts',(-18.8247832047746,21.3260699020969,
12.9075016400214));
#199756=CARTESIAN_POINT('Ctrl Pts',(-18.8333349827925,21.3256855177204,
12.9069860176908));
#199757=CARTESIAN_POINT('Ctrl Pts',(-18.8607003270948,21.3242891424224,
12.9053302986479));
#199758=CARTESIAN_POINT('Ctrl Pts',(-18.8795024029744,21.3230778837619,
12.9041839820261));
#199759=CARTESIAN_POINT('Ctrl Pts',(-18.9733442061239,21.3157734599182,
12.8984176063806));
#199760=CARTESIAN_POINT('Ctrl Pts',(-19.048029803229,21.3059319997079,12.8936813032008));
#199761=CARTESIAN_POINT('Ctrl Pts',(-19.2293127889757,21.2721319244407,
12.8818311209907));
#199762=CARTESIAN_POINT('Ctrl Pts',(-19.334884623808,21.2438634398422,12.8746173490601));
#199763=CARTESIAN_POINT('Ctrl Pts',(-19.5501841534604,21.1679702634865,
12.8595366994744));
#199764=CARTESIAN_POINT('Ctrl Pts',(-19.6590387362335,21.1189305852053,
12.8516978038089));
#199765=CARTESIAN_POINT('Ctrl Pts',(-19.7715148752033,21.0563570054044,
12.8437479826082));
#199766=CARTESIAN_POINT('Ctrl Pts',(-19.7798013167007,21.0516735743813,
12.8431632938848));
#199767=CARTESIAN_POINT('Ctrl Pts',(-19.7920323210489,21.0446514471727,
12.8423020832976));
#199768=CARTESIAN_POINT('Ctrl Pts',(-19.7960011937486,21.0423556420021,
12.8420229105033));
#199769=CARTESIAN_POINT('Ctrl Pts',(-19.8029497390453,21.03830605235,12.8415346875896));
#199770=CARTESIAN_POINT('Ctrl Pts',(-19.8059326018198,21.0365578466142,
12.8413252816192));
#199771=CARTESIAN_POINT('Ctrl Pts',(-19.8123348112572,21.0327845172184,
12.8408762189911));
#199772=CARTESIAN_POINT('Ctrl Pts',(-19.815752733244,21.0307570763876,12.8406367161229));
#199773=CARTESIAN_POINT('Ctrl Pts',(-19.8228011823922,21.0265492060836,
12.8401432586166));
#199774=CARTESIAN_POINT('Ctrl Pts',(-19.8264309199432,21.0243674807774,
12.8398893885877));
#199775=CARTESIAN_POINT('Ctrl Pts',(-19.8355517791909,21.0188478837424,
12.8392520159915));
#199776=CARTESIAN_POINT('Ctrl Pts',(-19.8410343380238,21.0154958491952,
12.8388693998814));
#199777=CARTESIAN_POINT('Ctrl Pts',(-19.8566123030061,21.0058737682743,
12.8377834505836));
#199778=CARTESIAN_POINT('Ctrl Pts',(-19.866670459463,20.9995435054228,12.837083739143));
#199779=CARTESIAN_POINT('Ctrl Pts',(-19.9003600331289,20.9779422408574,
12.834743099242));
#199780=CARTESIAN_POINT('Ctrl Pts',(-19.923741079198,20.9622843639021,12.8331237184737));
#199781=CARTESIAN_POINT('Ctrl Pts',(-20.1088252450054,20.8329186129527,
12.8202871227201));
#199782=CARTESIAN_POINT('Ctrl Pts',(-20.2541976856571,20.69753256102,12.8100063819662));
#199783=CARTESIAN_POINT('Ctrl Pts',(-20.4249763388468,20.4868108874827,
12.7948508453257));
#199784=CARTESIAN_POINT('Ctrl Pts',(-20.468256540685,20.4273251921819,12.7906592706563));
#199785=CARTESIAN_POINT('Ctrl Pts',(-20.515479317361,20.3547618483329,12.7855790060097));
#199786=CARTESIAN_POINT('Ctrl Pts',(-20.5225045500718,20.3437449787257,
12.7848086283983));
#199787=CARTESIAN_POINT('Ctrl Pts',(-20.5337623764292,20.3257247795402,
12.7835496938018));
#199788=CARTESIAN_POINT('Ctrl Pts',(-20.5380572057999,20.318760597359,12.7830634392869));
#199789=CARTESIAN_POINT('Ctrl Pts',(-20.5456382811619,20.3063066570861,
12.7821942958995));
#199790=CARTESIAN_POINT('Ctrl Pts',(-20.5489402313534,20.3008265412692,
12.7818119892106));
#199791=CARTESIAN_POINT('Ctrl Pts',(-20.5558505420021,20.289239268294,12.7810038924124));
#199792=CARTESIAN_POINT('Ctrl Pts',(-20.5594531446599,20.2831287850949,
12.7805778985502));
#199793=CARTESIAN_POINT('Ctrl Pts',(-20.5689125005315,20.2668985864276,
12.7794467442218));
#199794=CARTESIAN_POINT('Ctrl Pts',(-20.5747161808223,20.2567483648043,
12.7787396750558));
#199795=CARTESIAN_POINT('Ctrl Pts',(-20.6014164502777,20.209140536072,12.7754244834299));
#199796=CARTESIAN_POINT('Ctrl Pts',(-20.6212544197464,20.1711036731717,
12.7727788948518));
#199797=CARTESIAN_POINT('Ctrl Pts',(-20.670727062303,20.0687794470757,12.7656650187975));
#199798=CARTESIAN_POINT('Ctrl Pts',(-20.6983134548541,20.0035701600995,
12.7611331539509));
#199799=CARTESIAN_POINT('Ctrl Pts',(-20.7225806071911,19.9371103006456,
12.75653014821));
#199800=CARTESIAN_POINT('Ctrl Pts',(-20.7225806018034,19.9371103154006,
12.5316746994897));
#199801=CARTESIAN_POINT('Ctrl Pts',(-20.6939757378795,20.0154497581957,
12.5368029489854));
#199802=CARTESIAN_POINT('Ctrl Pts',(-20.6607669422471,20.0920298936055,
12.5420833733886));
#199803=CARTESIAN_POINT('Ctrl Pts',(-20.602665918439,20.2069075948999,12.5504105413036));
#199804=CARTESIAN_POINT('Ctrl Pts',(-20.5809117602758,20.2466934439469,
12.5533735281679));
#199805=CARTESIAN_POINT('Ctrl Pts',(-20.5316283424972,20.3303296579239,
12.5597563757112));
#199806=CARTESIAN_POINT('Ctrl Pts',(-20.503733307023,20.3739318282504,12.5631796257824));
#199807=CARTESIAN_POINT('Ctrl Pts',(-20.4264177596365,20.4855481664746,
12.5721484126384));
#199808=CARTESIAN_POINT('Ctrl Pts',(-20.3744922025269,20.5517229657316,
12.5776795961887));
#199809=CARTESIAN_POINT('Ctrl Pts',(-20.2942311408303,20.6423410473356,
12.5854031239243));
#199810=CARTESIAN_POINT('Ctrl Pts',(-20.2689713883223,20.6693969381936,
12.5877297341331));
#199811=CARTESIAN_POINT('Ctrl Pts',(-20.2377192153322,20.7011592211483,
12.5904716532237));
#199812=CARTESIAN_POINT('Ctrl Pts',(-20.2323960249063,20.7065117316206,
12.5909340877451));
#199813=CARTESIAN_POINT('Ctrl Pts',(-20.2240794077151,20.7147851734803,
12.5916492914583));
#199814=CARTESIAN_POINT('Ctrl Pts',(-20.2211058256541,20.7177258387908,
12.5919035813813));
#199815=CARTESIAN_POINT('Ctrl Pts',(-20.2155821701284,20.7231560678198,
12.5923732706561));
#199816=CARTESIAN_POINT('Ctrl Pts',(-20.2130345465443,20.7256479824414,
12.59258885207));
#199817=CARTESIAN_POINT('Ctrl Pts',(-20.2072698478499,20.731258210957,12.5930743144939));
#199818=CARTESIAN_POINT('Ctrl Pts',(-20.2040491682681,20.7343727437133,
12.5933439003935));
#199819=CARTESIAN_POINT('Ctrl Pts',(-20.1945407447006,20.743509554752,12.5941350839851));
#199820=CARTESIAN_POINT('Ctrl Pts',(-20.1882256212846,20.7495033801158,
12.5946545252993));
#199821=CARTESIAN_POINT('Ctrl Pts',(-20.1431281644156,20.7917806114516,
12.5983229332164));
#199822=CARTESIAN_POINT('Ctrl Pts',(-20.1030260998331,20.826635500588,12.6013714207977));
#199823=CARTESIAN_POINT('Ctrl Pts',(-20.0473217756002,20.8714858909613,
12.6053941466042));
#199824=CARTESIAN_POINT('Ctrl Pts',(-20.0328414662831,20.8828368201011,
12.6064215426));
#199825=CARTESIAN_POINT('Ctrl Pts',(-19.8674199937629,21.0090619993885,
12.6179757194447));
#199826=CARTESIAN_POINT('Ctrl Pts',(-19.7018490214765,21.1033374937958,
12.627926805568));
#199827=CARTESIAN_POINT('Ctrl Pts',(-19.4760477215584,21.1944179954608,
12.6417205209282));
#199828=CARTESIAN_POINT('Ctrl Pts',(-19.4254231080912,21.2126281219504,
12.644819304011));
#199829=CARTESIAN_POINT('Ctrl Pts',(-19.3621221137179,21.2327099653548,
12.6487257231115));
#199830=CARTESIAN_POINT('Ctrl Pts',(-19.3500475104601,21.2364219383133,
12.6494722283799));
#199831=CARTESIAN_POINT('Ctrl Pts',(-19.3309427553344,21.2421084794397,
12.6506557923751));
#199832=CARTESIAN_POINT('Ctrl Pts',(-19.3239342474494,21.2441551564098,
12.6510904896425));
#199833=CARTESIAN_POINT('Ctrl Pts',(-19.3107946833903,21.2479186113388,
12.651906473571));
#199834=CARTESIAN_POINT('Ctrl Pts',(-19.3046661830549,21.2496440695109,
12.6522874720648));
#199835=CARTESIAN_POINT('Ctrl Pts',(-19.2909590858506,21.2534366046774,
12.6531405760855));
#199836=CARTESIAN_POINT('Ctrl Pts',(-19.2833766082406,21.2554891897882,
12.6536131467591));
#199837=CARTESIAN_POINT('Ctrl Pts',(-19.264182588152,21.2605705460335,12.6548111167751));
#199838=CARTESIAN_POINT('Ctrl Pts',(-19.2525565055725,21.2635428475853,
12.6555383314942));
#199839=CARTESIAN_POINT('Ctrl Pts',(-19.1869372681565,21.2797258398991,
12.6596522577984));
#199840=CARTESIAN_POINT('Ctrl Pts',(-19.1324697176687,21.2909037837291,
12.6631037295946));
#199841=CARTESIAN_POINT('Ctrl Pts',(-19.0530007504076,21.3039764680535,
12.6681954863541));
#199842=CARTESIAN_POINT('Ctrl Pts',(-19.0283033276721,21.307591866153,12.6697855034202));
#199843=CARTESIAN_POINT('Ctrl Pts',(-18.843488752511,21.3313166036231,12.6817366843576));
#199844=CARTESIAN_POINT('Ctrl Pts',(-18.6816101315199,21.3334930032669,
12.6925566367374));
#199845=CARTESIAN_POINT('Ctrl Pts',(-18.472333969205,21.3123378243056,12.7062829712044));
#199846=CARTESIAN_POINT('Ctrl Pts',(-18.4237672321485,21.3057186034452,
12.709445010742));
#199847=CARTESIAN_POINT('Ctrl Pts',(-18.3495878328167,21.29297166385,12.7141979600806));
#199848=CARTESIAN_POINT('Ctrl Pts',(-18.3237882155467,21.2880424073911,
12.715836551287));
#199849=CARTESIAN_POINT('Ctrl Pts',(-18.2914704780547,21.2812420923089,
12.7178652404337));
#199850=CARTESIAN_POINT('Ctrl Pts',(-18.2848618724701,21.2798184173128,
12.7182788199608));
#199851=CARTESIAN_POINT('Ctrl Pts',(-18.2743504604813,21.2775012288611,
12.718934505566));
#199852=CARTESIAN_POINT('Ctrl Pts',(-18.2704432385511,21.276628271881,12.7191777603174));
#199853=CARTESIAN_POINT('Ctrl Pts',(-18.263034204319,21.2749508542315,12.7196381033074));
#199854=CARTESIAN_POINT('Ctrl Pts',(-18.2595320080105,21.2741485729621,
12.719855306579));
#199855=CARTESIAN_POINT('Ctrl Pts',(-18.251471154613,21.272280386078,12.7203543421141));
#199856=CARTESIAN_POINT('Ctrl Pts',(-18.2469139805637,21.271208272795,12.7206358146928));
#199857=CARTESIAN_POINT('Ctrl Pts',(-18.2347012131966,21.2682923292672,
12.7213884653357));
#199858=CARTESIAN_POINT('Ctrl Pts',(-18.2270522043401,21.2664208677057,
12.7218580995142));
#199859=CARTESIAN_POINT('Ctrl Pts',(-18.1696272410509,21.2520308002749,
12.725371848381));
#199860=CARTESIAN_POINT('Ctrl Pts',(-18.1203065314138,21.2377472915025,
12.7283217401319));
#199861=CARTESIAN_POINT('Ctrl Pts',(-18.0580582235636,21.2172386438953,
12.732013863888));
#199862=CARTESIAN_POINT('Ctrl Pts',(-18.0446114803329,21.2126578787571,
12.7328095396516));
#199863=CARTESIAN_POINT('Ctrl Pts',(-17.8962877784859,21.1604579811881,
12.7415753146879));
#199864=CARTESIAN_POINT('Ctrl Pts',(-17.7665194593634,21.0994208882194,
12.7491693486816));
#199865=CARTESIAN_POINT('Ctrl Pts',(-17.5641903077008,20.9778839800793,
12.7621677102766));
#199866=CARTESIAN_POINT('Ctrl Pts',(-17.4877365417385,20.9248139374791,
12.7673878531307));
#199867=CARTESIAN_POINT('Ctrl Pts',(-17.3985178372785,20.853748203897,12.7740317061341));
#199868=CARTESIAN_POINT('Ctrl Pts',(-17.3822105066157,20.8403555126228,
12.7752701264902));
#199869=CARTESIAN_POINT('Ctrl Pts',(-17.3592676960378,20.8209317949007,
12.7770484849225));
#199870=CARTESIAN_POINT('Ctrl Pts',(-17.3524657852365,20.8150986570243,
12.777580334009));
#199871=CARTESIAN_POINT('Ctrl Pts',(-17.3407808116132,20.8049484844647,
12.7785021126087));
#199872=CARTESIAN_POINT('Ctrl Pts',(-17.3358802400462,20.8006517270705,
12.7788911979519));
#199873=CARTESIAN_POINT('Ctrl Pts',(-17.3265250460994,20.792372491627,12.7796388122746));
#199874=CARTESIAN_POINT('Ctrl Pts',(-17.3220672838421,20.7883936436532,
12.7799971870084));
#199875=CARTESIAN_POINT('Ctrl Pts',(-17.3104974181208,20.7779784324989,
12.7809329499628));
#199876=CARTESIAN_POINT('Ctrl Pts',(-17.3034121681018,20.7715125629169,
12.7815115829568));
#199877=CARTESIAN_POINT('Ctrl Pts',(-17.2792898127184,20.749196592085,12.7835010102009));
#199878=CARTESIAN_POINT('Ctrl Pts',(-17.262470699414,20.7331142974793,12.7849217166165));
#199879=CARTESIAN_POINT('Ctrl Pts',(-17.1239847155411,20.596254278873,12.7969092641665));
#199880=CARTESIAN_POINT('Ctrl Pts',(-17.0171596501688,20.4614063083084,
12.8081436431408));
#199881=CARTESIAN_POINT('Ctrl Pts',(-16.8808936944311,20.2385043294495,
12.8254075461086));
#199882=CARTESIAN_POINT('Ctrl Pts',(-16.8389404070292,20.1589025540898,
12.831338628619));
#199883=CARTESIAN_POINT('Ctrl Pts',(-16.7864092042904,20.0417011885649,
12.8395436730425));
#199884=CARTESIAN_POINT('Ctrl Pts',(-16.7716079683765,20.0061052247659,
12.8419691279139));
#199885=CARTESIAN_POINT('Ctrl Pts',(-16.755056309783,19.9630165006175,12.8448097554097));
#199886=CARTESIAN_POINT('Ctrl Pts',(-16.7523649797786,19.9558956953316,
12.8452761189057));
#199887=CARTESIAN_POINT('Ctrl Pts',(-16.7482515231648,19.9448321003641,
12.8459957749163));
#199888=CARTESIAN_POINT('Ctrl Pts',(-16.7468026291136,19.9408994277454,
12.8462506219511));
#199889=CARTESIAN_POINT('Ctrl Pts',(-16.744143577396,19.9336154665655,12.8467208276092));
#199890=CARTESIAN_POINT('Ctrl Pts',(-16.7429302115117,19.9302654536225,
12.8469363715683));
#199891=CARTESIAN_POINT('Ctrl Pts',(-16.7402141009249,19.9227069323436,
12.8474211056352));
#199892=CARTESIAN_POINT('Ctrl Pts',(-16.7387162248005,19.918496732264,12.8476900045509));
#199893=CARTESIAN_POINT('Ctrl Pts',(-16.7343571669519,19.9061204288711,
12.8484773069793));
#199894=CARTESIAN_POINT('Ctrl Pts',(-16.7315326666444,19.8979413767105,
12.848993585663));
#199895=CARTESIAN_POINT('Ctrl Pts',(-16.7121522154832,19.8406849939106,
12.8525812003558));
#199896=CARTESIAN_POINT('Ctrl Pts',(-16.697350646471,19.7910275918559,12.8555570257175));
#199897=CARTESIAN_POINT('Ctrl Pts',(-16.6790045187347,19.7200624691352,
12.8596845669602));
#199898=CARTESIAN_POINT('Ctrl Pts',(-16.6739416291031,19.6991706437737,
12.8608845964973));
#199899=CARTESIAN_POINT('Ctrl Pts',(-16.6387807428172,19.5437778278176,
12.8697221449241));
#199900=CARTESIAN_POINT('Ctrl Pts',(-16.6215631961414,19.4066993693504,
12.8770523915137));
#199901=CARTESIAN_POINT('Ctrl Pts',(-16.6153091995141,19.1781827269612,
12.8896557718727));
#199902=CARTESIAN_POINT('Ctrl Pts',(-16.6186640135761,19.0873933246637,
12.894758101716));
#199903=CARTESIAN_POINT('Ctrl Pts',(-16.6299381261798,18.9763798403343,
12.9012594161225));
#199904=CARTESIAN_POINT('Ctrl Pts',(-16.6323487137071,18.9556868327892,
12.9024822797136));
#199905=CARTESIAN_POINT('Ctrl Pts',(-16.6362262989008,18.926194860731,12.9042421523431));
#199906=CARTESIAN_POINT('Ctrl Pts',(-16.6374441722094,18.9173639571992,
12.9047713039514));
#199907=CARTESIAN_POINT('Ctrl Pts',(-16.6396477629919,18.9020985946339,
12.9056898972832));
#199908=CARTESIAN_POINT('Ctrl Pts',(-16.6406074560659,18.8956604584905,
12.9060785107318));
#199909=CARTESIAN_POINT('Ctrl Pts',(-16.6425065486055,18.8833111746527,
12.9068262693715));
#199910=CARTESIAN_POINT('Ctrl Pts',(-16.6434413555057,18.877399376094,12.9071852653646));
#199911=CARTESIAN_POINT('Ctrl Pts',(-16.645948341716,18.8619694297522,12.9081249890012));
#199912=CARTESIAN_POINT('Ctrl Pts',(-16.647560521134,18.8524580040773,12.9087069821842));
#199913=CARTESIAN_POINT('Ctrl Pts',(-16.653340563729,18.8197171295186,12.9107199333799));
#199914=CARTESIAN_POINT('Ctrl Pts',(-16.6578317032633,18.7965472193741,
12.9121611210903));
#199915=CARTESIAN_POINT('Ctrl Pts',(-16.6968550101441,18.61181384599,12.9237896471893));
#199916=CARTESIAN_POINT('Ctrl Pts',(-16.749799376812,18.4547514101852,12.9345914681778));
#199917=CARTESIAN_POINT('Ctrl Pts',(-16.8749454905301,18.1902934768021,
12.9539259743473));
#199918=CARTESIAN_POINT('Ctrl Pts',(-16.9397426723322,18.0802600403464,
12.9623536335936));
#199919=CARTESIAN_POINT('Ctrl Pts',(-17.0210403983306,17.9669734079629,
12.9710016530801));
#199920=CARTESIAN_POINT('Ctrl Pts',(-17.0281137715218,17.9572915213666,
12.9717403588792));
#199921=CARTESIAN_POINT('Ctrl Pts',(-17.0382747652153,17.9436285885701,
12.9727816451745));
#199922=CARTESIAN_POINT('Ctrl Pts',(-17.0412947731577,17.9395978674631,
12.9730886908595));
#199923=CARTESIAN_POINT('Ctrl Pts',(-17.0465196709674,17.9326759570553,
12.9736156695249));
#199924=CARTESIAN_POINT('Ctrl Pts',(-17.0487176679126,17.9297796124108,
12.9738360800628));
#199925=CARTESIAN_POINT('Ctrl Pts',(-17.0529903479878,17.9241794358584,
12.9742620488415));
#199926=CARTESIAN_POINT('Ctrl Pts',(-17.0550640982262,17.9214749507782,
12.9744676722848));
#199927=CARTESIAN_POINT('Ctrl Pts',(-17.0606692089384,17.9142014769428,
12.9750204735018));
#199928=CARTESIAN_POINT('Ctrl Pts',(-17.0642127777655,17.9096418709828,
12.9753667956314));
#199929=CARTESIAN_POINT('Ctrl Pts',(-17.0773898736568,17.8928289817404,
12.9766432338783));
#199930=CARTESIAN_POINT('Ctrl Pts',(-17.0871402490518,17.8806673586254,
12.977565411901));
#199931=CARTESIAN_POINT('Ctrl Pts',(-17.1836998002703,17.7629175844823,
12.9864951176728));
#199932=CARTESIAN_POINT('Ctrl Pts',(-17.2804210886076,17.6658488378552,
12.9938785515231));
#199933=CARTESIAN_POINT('Ctrl Pts',(-17.5049801053808,17.4803708958351,
13.0096951467069));
#199934=CARTESIAN_POINT('Ctrl Pts',(-17.634519212944,17.3953178864269,13.0181145403484));
#199935=CARTESIAN_POINT('Ctrl Pts',(-17.7911005572384,17.3154573192619,
13.0283509471637));
#199936=CARTESIAN_POINT('Ctrl Pts',(-17.810192476547,17.3060797852058,13.0295991178271));
#199937=CARTESIAN_POINT('Ctrl Pts',(-17.8375492481597,17.2931507212595,
13.0313890523388));
#199938=CARTESIAN_POINT('Ctrl Pts',(-17.8457008263835,17.2893615374382,
13.0319225803579));
#199939=CARTESIAN_POINT('Ctrl Pts',(-17.8598084695829,17.2829126799852,
13.0328463448206));
#199940=CARTESIAN_POINT('Ctrl Pts',(-17.865753192453,17.2802283860666,13.0332357271702));
#199941=CARTESIAN_POINT('Ctrl Pts',(-17.8771616969699,17.2751403065064,
13.033983265684));
#199942=CARTESIAN_POINT('Ctrl Pts',(-17.8826234337851,17.2727320691405,
13.0343412644924));
#199943=CARTESIAN_POINT('Ctrl Pts',(-17.8968576561934,17.2665275614899,
13.0352746203802));
#199944=CARTESIAN_POINT('Ctrl Pts',(-17.9056457256159,17.2627675807693,
13.0358512096565));
#199945=CARTESIAN_POINT('Ctrl Pts',(-17.9357274150561,17.2501374412311,
13.0378262304455));
#199946=CARTESIAN_POINT('Ctrl Pts',(-17.957139819771,17.2415560966169,13.039234381576));
#199947=CARTESIAN_POINT('Ctrl Pts',(-18.1416935628958,17.1710713823248,
13.0513951759771));
#199948=CARTESIAN_POINT('Ctrl Pts',(-18.3117420517259,17.1292193075748,
13.0628424756846));
#199949=CARTESIAN_POINT('Ctrl Pts',(-18.5720579118163,17.0983814302608,
13.0801628680898));
#199950=CARTESIAN_POINT('Ctrl Pts',(-18.65972397661,17.0934855447209,13.0859453644604));
#199951=CARTESIAN_POINT('Ctrl Pts',(-18.7854445246833,17.0942840444705,
13.093973440362));
#199952=CARTESIAN_POINT('Ctrl Pts',(-18.823432873117,17.095548475591,13.0963640022605));
#199953=CARTESIAN_POINT('Ctrl Pts',(-18.8689372367757,17.0982912112943,
13.0991692872839));
#199954=CARTESIAN_POINT('Ctrl Pts',(-18.8765029324068,17.0987880309988,
13.0996337639773));
#199955=CARTESIAN_POINT('Ctrl Pts',(-18.8882398333895,17.0996221126282,
13.1003511407098));
#199956=CARTESIAN_POINT('Ctrl Pts',(-18.8924128941211,17.0999311083808,
13.1006055798826));
#199957=CARTESIAN_POINT('Ctrl Pts',(-18.9001380732722,17.1005261575976,
13.101075407153));
#199958=CARTESIAN_POINT('Ctrl Pts',(-18.9036903550988,17.1008088042685,
13.1012909781908));
#199959=CARTESIAN_POINT('Ctrl Pts',(-18.9117040920276,17.1014668051293,
13.1017762439332));
#199960=CARTESIAN_POINT('Ctrl Pts',(-18.9161650672885,17.1018473422507,
13.1020456445837));
#199961=CARTESIAN_POINT('Ctrl Pts',(-18.9292829712635,17.1030082753133,
13.1028357807427));
#199962=CARTESIAN_POINT('Ctrl Pts',(-18.9379364606399,17.1038278484904,
13.1033543684103));
#199963=CARTESIAN_POINT('Ctrl Pts',(-18.9990565036251,17.1099965794217,
13.1070000432727));
#199964=CARTESIAN_POINT('Ctrl Pts',(-19.0513167497674,17.1172518317035,
13.1100280650202));
#199965=CARTESIAN_POINT('Ctrl Pts',(-19.1187991609385,17.1292056337981,
13.1138841932025));
#199966=CARTESIAN_POINT('Ctrl Pts',(-19.1343115325991,17.1321327911846,
13.11476686249));
#199967=CARTESIAN_POINT('Ctrl Pts',(-19.1996418870996,17.1452188985015,
13.1184736259121));
#199968=CARTESIAN_POINT('Ctrl Pts',(-19.2491196316764,17.1569975561323,
13.1212551272408));
#199969=CARTESIAN_POINT('Ctrl Pts',(-19.4035795587739,17.1997012889708,
13.1299803500712));
#199970=CARTESIAN_POINT('Ctrl Pts',(-19.5066125565614,17.2369867652113,
13.1358713302348));
#199971=CARTESIAN_POINT('Ctrl Pts',(-19.656577437648,17.3048035658457,13.1450223857008));
#199972=CARTESIAN_POINT('Ctrl Pts',(-19.7059453396827,17.3294964567632,
13.1481337539049));
#199973=CARTESIAN_POINT('Ctrl Pts',(-19.784378457078,17.3726384136937,13.1532835721569));
#199974=CARTESIAN_POINT('Ctrl Pts',(-19.8140584661585,17.3899174270098,
13.1552825178229));
#199975=CARTESIAN_POINT('Ctrl Pts',(-19.8525132495497,17.4135757253279,
13.1579452617814));
#199976=CARTESIAN_POINT('Ctrl Pts',(-19.8616788873658,17.4193119040908,
13.1585854843885));
#199977=CARTESIAN_POINT('Ctrl Pts',(-19.8766199764073,17.4288226279258,
13.1596384563426));
#199978=CARTESIAN_POINT('Ctrl Pts',(-19.8824217011921,17.4325556824806,
13.1600496628807));
#199979=CARTESIAN_POINT('Ctrl Pts',(-19.8936175175815,17.439837133579,13.1608477585023));
#199980=CARTESIAN_POINT('Ctrl Pts',(-19.8990138331243,17.4433819831007,
13.161234511866));
#199981=CARTESIAN_POINT('Ctrl Pts',(-19.9114372723222,17.4516245658215,
13.1621297497777));
#199982=CARTESIAN_POINT('Ctrl Pts',(-19.9184526096969,17.4563397876542,
13.1626388898059));
#199983=CARTESIAN_POINT('Ctrl Pts',(-19.9372457769357,17.4691353075703,
13.164012661985));
#199984=CARTESIAN_POINT('Ctrl Pts',(-19.9489702236747,17.4772928891142,
13.1648802186487));
#199985=CARTESIAN_POINT('Ctrl Pts',(-20.07557807645,17.567298531444,13.174365196308));
#199986=CARTESIAN_POINT('Ctrl Pts',(-20.182067377199,17.6602989408211,13.1834323132249));
#199987=CARTESIAN_POINT('Ctrl Pts',(-20.3445945702494,17.8336791733927,
13.1990666910339));
#199988=CARTESIAN_POINT('Ctrl Pts',(-20.4057792373794,17.9086245128324,
13.2054948616771));
#199989=CARTESIAN_POINT('Ctrl Pts',(-20.4993339042067,18.0407260570813,
13.2160580007295));
#199990=CARTESIAN_POINT('Ctrl Pts',(-20.5345602872609,18.0956842678464,
13.220252126317));
#199991=CARTESIAN_POINT('Ctrl Pts',(-20.5737749589651,18.1635792676172,
13.2251235692587));
#199992=CARTESIAN_POINT('Ctrl Pts',(-20.5802489425307,18.1750333246347,
13.2259351580403));
#199993=CARTESIAN_POINT('Ctrl Pts',(-20.5891459476138,18.1911226310708,
13.2270601566078));
#199994=CARTESIAN_POINT('Ctrl Pts',(-20.5916590611624,18.1957073582334,
13.2273790413168));
#199995=CARTESIAN_POINT('Ctrl Pts',(-20.595907904763,18.2035272053478,13.2279200092904));
#199996=CARTESIAN_POINT('Ctrl Pts',(-20.5976522423857,18.2067575999996,
13.2281426366694));
#199997=CARTESIAN_POINT('Ctrl Pts',(-20.6009776730976,18.2129545761209,
13.2285680661442));
#199998=CARTESIAN_POINT('Ctrl Pts',(-20.6025601088534,18.2159203951753,
13.2287709563414));
#199999=CARTESIAN_POINT('Ctrl Pts',(-20.6067291659775,18.2237791020038,
13.2293067057554));
#200000=CARTESIAN_POINT('Ctrl Pts',(-20.6093036963967,18.2286784241424,
13.2296388023647));
#200001=CARTESIAN_POINT('Ctrl Pts',(-20.6183487944788,18.2460563736321,
13.2308102280235));
#200002=CARTESIAN_POINT('Ctrl Pts',(-20.6247144240707,18.2585895991702,
13.2316432121907));
#200003=CARTESIAN_POINT('Ctrl Pts',(-20.7038353716376,18.4182901562788,
13.2421192697334));
#200004=CARTESIAN_POINT('Ctrl Pts',(-20.7593686000765,18.5733959132647,
13.2508474686791));
#200005=CARTESIAN_POINT('Ctrl Pts',(-20.8270296516777,18.8655648132127,
13.2671777503762));
#200006=CARTESIAN_POINT('Ctrl Pts',(-20.8448588515676,19.0003662911015,
13.2746744668283));
#200007=CARTESIAN_POINT('Ctrl Pts',(-20.8502665612874,19.152784629548,13.2835990378356));
#200008=CARTESIAN_POINT('Ctrl Pts',(-20.8506630230942,19.1696380610564,
13.2845915396842));
#200009=CARTESIAN_POINT('Ctrl Pts',(-20.8509528940655,19.1946775469274,
13.2860752297776));
#200010=CARTESIAN_POINT('Ctrl Pts',(-20.8510001744507,19.2028614086608,
13.2865616003627));
#200011=CARTESIAN_POINT('Ctrl Pts',(-20.8509998627497,19.21744352008,13.28743087348));
#200012=CARTESIAN_POINT('Ctrl Pts',(-20.8509707194948,19.2238416995252,
13.2878131931752));
#200013=CARTESIAN_POINT('Ctrl Pts',(-20.8508481156851,19.237331668986,13.2886212368629));
#200014=CARTESIAN_POINT('Ctrl Pts',(-20.8507480205181,19.2444233062069,
13.2890471641999));
#200015=CARTESIAN_POINT('Ctrl Pts',(-20.8503886243228,19.2631994798068,
13.2901779541959));
#200016=CARTESIAN_POINT('Ctrl Pts',(-20.8500681972047,19.2748824784275,
13.2908847233622));
#200017=CARTESIAN_POINT('Ctrl Pts',(-20.8481220038479,19.3293736724638,
13.2941963673929));
#200018=CARTESIAN_POINT('Ctrl Pts',(-20.8452939286926,19.3721263518761,
13.2968386108037));
#200019=CARTESIAN_POINT('Ctrl Pts',(-20.8339020511185,19.4899338561121,
13.3042463940272));
#200020=CARTESIAN_POINT('Ctrl Pts',(-20.8226163055533,19.564656190052,13.3090902071202));
#200021=CARTESIAN_POINT('Ctrl Pts',(-20.7864357642242,19.7400858175658,
13.3207653363176));
#200022=CARTESIAN_POINT('Ctrl Pts',(-20.7580935696955,19.8398518296155,
13.3276520160473));
#200023=CARTESIAN_POINT('Ctrl Pts',(-20.7225805710824,19.9371103995355,
13.3344633171505));
#200024=CARTESIAN_POINT('Origin',(-18.734,19.211,0.));
#200025=CARTESIAN_POINT('',(-20.7249099185723,19.937940853899,14.355439970105));
#200026=CARTESIAN_POINT('',(-20.7225805809329,19.9371103725581,14.1348941200942));
#200027=CARTESIAN_POINT('',(-20.7225806064498,19.9371103026755,0.));
#200028=CARTESIAN_POINT('',(-20.8478642240166,19.211459512885,14.3110922513879));
#200029=CARTESIAN_POINT('Ctrl Pts',(-20.8476071148151,19.2114685807671,
14.310944106499));
#200030=CARTESIAN_POINT('Ctrl Pts',(-20.8480884069697,19.4590066998217,
14.3257760610343));
#200031=CARTESIAN_POINT('Ctrl Pts',(-20.80739811974,19.7063940898195,14.3406080155697));
#200032=CARTESIAN_POINT('Ctrl Pts',(-20.7249099185723,19.937940853899,14.355439970105));
#200033=CARTESIAN_POINT('Ctrl Pts',(-20.8509999712459,19.2113489194644,
14.3128990514644));
#200034=CARTESIAN_POINT('Ctrl Pts',(-20.8510014361084,19.2024611552748,
14.3123784859613));
#200035=CARTESIAN_POINT('Ctrl Pts',(-20.8509469309422,19.1935735497784,
14.3118562320931));
#200036=CARTESIAN_POINT('Ctrl Pts',(-20.8507292584551,19.1760624133584,
14.3108237614325));
#200037=CARTESIAN_POINT('Ctrl Pts',(-20.8505693533197,19.1674390332335,
14.3103136564554));
#200038=CARTESIAN_POINT('Ctrl Pts',(-20.8502036147191,19.1526059869016,
14.3094332672318));
#200039=CARTESIAN_POINT('Ctrl Pts',(-20.8500231310319,19.1463957633363,
14.3090637777332));
#200040=CARTESIAN_POINT('Ctrl Pts',(-20.8496088606873,19.1340179085138,
14.3083255149905));
#200041=CARTESIAN_POINT('Ctrl Pts',(-20.8493754334206,19.1278503261407,
14.3079567565876));
#200042=CARTESIAN_POINT('Ctrl Pts',(-20.848855723496,19.1155429558949,14.3072190705556));
#200043=CARTESIAN_POINT('Ctrl Pts',(-20.8485696657352,19.1094032186219,
14.3068501535266));
#200044=CARTESIAN_POINT('Ctrl Pts',(-20.8477228781531,19.0927853673251,
14.3058491347497));
#200045=CARTESIAN_POINT('Ctrl Pts',(-20.8471109809795,19.082310136904,14.30521543353));
#200046=CARTESIAN_POINT('Ctrl Pts',(-20.8445147257632,19.042899487298,14.3028208683896));
#200047=CARTESIAN_POINT('Ctrl Pts',(-20.8420137560137,19.0140023769774,
14.3010439012303));
#200048=CARTESIAN_POINT('Ctrl Pts',(-20.8144782635763,18.7573526849457,
14.2850653343867));
#200049=CARTESIAN_POINT('Ctrl Pts',(-20.753211591893,18.5350388691164,14.269604433014));
#200050=CARTESIAN_POINT('Ctrl Pts',(-20.6340839915613,18.2758348938444,
14.2510838378801));
#200051=CARTESIAN_POINT('Ctrl Pts',(-20.6085646358542,18.2256769524415,
14.2474877607192));
#200052=CARTESIAN_POINT('Ctrl Pts',(-20.5751286687195,18.1659725642482,
14.2432425645308));
#200053=CARTESIAN_POINT('Ctrl Pts',(-20.5690903961147,18.1554052054487,
14.2424925974347));
#200054=CARTESIAN_POINT('Ctrl Pts',(-20.560409458869,18.1405126516654,14.2414383174952));
#200055=CARTESIAN_POINT('Ctrl Pts',(-20.5578420111671,18.1361441985472,
14.2411293897551));
#200056=CARTESIAN_POINT('Ctrl Pts',(-20.5534026131307,18.1286523709495,
14.2406002011725));
#200057=CARTESIAN_POINT('Ctrl Pts',(-20.5515382512226,18.1255245443153,
14.2403794522541));
#200058=CARTESIAN_POINT('Ctrl Pts',(-20.5479175144887,18.1194855429855,
14.2399536264843));
#200059=CARTESIAN_POINT('Ctrl Pts',(-20.5461621961086,18.1165737874974,
14.2397484806425));
#200060=CARTESIAN_POINT('Ctrl Pts',(-20.5414281368992,18.1087634562195,
14.2391986301067));
#200061=CARTESIAN_POINT('Ctrl Pts',(-20.5384364741632,18.1038726898179,
14.2388547647149));
#200062=CARTESIAN_POINT('Ctrl Pts',(-20.5273808238152,18.0859627814456,
14.2375969485602));
#200063=CARTESIAN_POINT('Ctrl Pts',(-20.5191952827764,18.073018736953,14.2366906394999));
#200064=CARTESIAN_POINT('Ctrl Pts',(-20.4329200664155,17.9398113524507,
14.2273801595364));
#200065=CARTESIAN_POINT('Ctrl Pts',(-20.3429326823567,17.8276716575317,
14.2196650392277));
#200066=CARTESIAN_POINT('Ctrl Pts',(-20.143065965183,17.6247417878619,14.204193749349));
#200067=CARTESIAN_POINT('Ctrl Pts',(-20.0340165922372,17.5342076098945,
14.1964684471925));
#200068=CARTESIAN_POINT('Ctrl Pts',(-19.9021332799011,17.4453655951087,
14.1872528265992));
#200069=CARTESIAN_POINT('Ctrl Pts',(-19.8873798999456,17.4356929869136,
14.1862240528257));
#200070=CARTESIAN_POINT('Ctrl Pts',(-19.8639721957415,17.4207613745174,
14.1845942123657));
#200071=CARTESIAN_POINT('Ctrl Pts',(-19.8553978859257,17.4153780254611,
14.1839976996536));
#200072=CARTESIAN_POINT('Ctrl Pts',(-19.8408083615995,17.406363301082,14.1829833922676));
#200073=CARTESIAN_POINT('Ctrl Pts',(-19.8348130293989,17.4026999593859,
14.1825667722271));
#200074=CARTESIAN_POINT('Ctrl Pts',(-19.8230017557086,17.395563395887,14.1817463193197));
#200075=CARTESIAN_POINT('Ctrl Pts',(-19.8171871566711,17.3920881083811,
14.1813425682413));
#200076=CARTESIAN_POINT('Ctrl Pts',(-19.8059706291668,17.3854570371514,
14.1805639657056));
#200077=CARTESIAN_POINT('Ctrl Pts',(-19.800571187759,17.3822971703578,14.1801892682528));
#200078=CARTESIAN_POINT('Ctrl Pts',(-19.7879859654366,17.3750067316828,
14.1793161207764));
#200079=CARTESIAN_POINT('Ctrl Pts',(-19.7807898114373,17.3708943551351,
14.1788170194299));
#200080=CARTESIAN_POINT('Ctrl Pts',(-19.7616178673035,17.3600870472655,
14.1774876453664));
#200081=CARTESIAN_POINT('Ctrl Pts',(-19.7496009762144,17.3534661825408,
14.1766547350752));
#200082=CARTESIAN_POINT('Ctrl Pts',(-19.6575661445073,17.3039184250284,
14.1702772305848));
#200083=CARTESIAN_POINT('Ctrl Pts',(-19.5749355579623,17.2660685982982,
14.1645541765244));
#200084=CARTESIAN_POINT('Ctrl Pts',(-19.3564459783098,17.1825183701739,
14.149447690927));
#200085=CARTESIAN_POINT('Ctrl Pts',(-19.2179152282854,17.1450867253631,
14.1398743484975));
#200086=CARTESIAN_POINT('Ctrl Pts',(-19.0250550073876,17.1134506217828,
14.1270950656102));
#200087=CARTESIAN_POINT('Ctrl Pts',(-18.9731248713825,17.106897710058,14.1237108504651));
#200088=CARTESIAN_POINT('Ctrl Pts',(-18.8936566373678,17.0998504524788,
14.1186666159142));
#200089=CARTESIAN_POINT('Ctrl Pts',(-18.8662650649588,17.0979574606686,
14.1169522408766));
#200090=CARTESIAN_POINT('Ctrl Pts',(-18.8319910100657,17.0962579763324,
14.1148437913913));
#200091=CARTESIAN_POINT('Ctrl Pts',(-18.8251373351981,17.0959515244726,
14.1144240031113));
#200092=CARTESIAN_POINT('Ctrl Pts',(-18.8142595621251,17.0955181140307,
14.1137607740516));
#200093=CARTESIAN_POINT('Ctrl Pts',(-18.8102364521885,17.0953693112551,
14.1135161394941));
#200094=CARTESIAN_POINT('Ctrl Pts',(-18.8026275322974,17.0951096125571,
14.1130547382518));
#200095=CARTESIAN_POINT('Ctrl Pts',(-18.7990419100372,17.0949963563436,
14.1128378478732));
#200096=CARTESIAN_POINT('Ctrl Pts',(-18.7908167627642,17.0947574818597,
14.1123415337505));
#200097=CARTESIAN_POINT('Ctrl Pts',(-18.7861771046747,17.0946380057271,
14.112062456411));
#200098=CARTESIAN_POINT('Ctrl Pts',(-18.7738027239945,17.0943600700649,
14.1113204025284));
#200099=CARTESIAN_POINT('Ctrl Pts',(-18.7660673796609,17.0942287470952,
14.1108589024566));
#200100=CARTESIAN_POINT('Ctrl Pts',(-18.7105206704841,17.0935902888748,
14.1075607924631));
#200101=CARTESIAN_POINT('Ctrl Pts',(-18.6627010439702,17.0946606180976,
14.1048058391841));
#200102=CARTESIAN_POINT('Ctrl Pts',(-18.5863863887302,17.0989588134262,
14.1004866742263));
#200103=CARTESIAN_POINT('Ctrl Pts',(-18.5578524533513,17.101146948829,14.0988891270869));
#200104=CARTESIAN_POINT('Ctrl Pts',(-18.4860611086704,17.1081189464573,
14.0948948962025));
#200105=CARTESIAN_POINT('Ctrl Pts',(-18.4428902215796,17.1136593708419,
14.0925160463929));
#200106=CARTESIAN_POINT('Ctrl Pts',(-18.2919610675702,17.1377794793268,
14.0841946673857));
#200107=CARTESIAN_POINT('Ctrl Pts',(-18.1855021437519,17.1633694276856,
14.0783076130399));
#200108=CARTESIAN_POINT('Ctrl Pts',(-18.0290972439073,17.2140434629985,
14.0691656850162));
#200109=CARTESIAN_POINT('Ctrl Pts',(-17.9773802934524,17.2330593332276,
14.0660595489563));
#200110=CARTESIAN_POINT('Ctrl Pts',(-17.8947632612499,17.2671515186741,
14.0609176190743));
#200111=CARTESIAN_POINT('Ctrl Pts',(-17.8633843627988,17.2810017000321,
14.0589211711253));
#200112=CARTESIAN_POINT('Ctrl Pts',(-17.8225786124641,17.300210409725,14.0562612831552));
#200113=CARTESIAN_POINT('Ctrl Pts',(-17.8128357915825,17.3048881726049,
14.0556213543255));
#200114=CARTESIAN_POINT('Ctrl Pts',(-17.7969340937783,17.3126733505018,
14.0545687425131));
#200115=CARTESIAN_POINT('Ctrl Pts',(-17.7907537556867,17.3157366669364,
14.0541576002687));
#200116=CARTESIAN_POINT('Ctrl Pts',(-17.7788173466281,17.3217258560732,
14.0533595414941));
#200117=CARTESIAN_POINT('Ctrl Pts',(-17.7730594671969,17.3246479694405,
14.052972760218));
#200118=CARTESIAN_POINT('Ctrl Pts',(-17.7597926517222,17.3314573595997,
14.0520773295852));
#200119=CARTESIAN_POINT('Ctrl Pts',(-17.7522934943752,17.3353633539261,
14.0515680238594));
#200120=CARTESIAN_POINT('Ctrl Pts',(-17.7321817606472,17.3459923621472,
14.0501935146202));
#200121=CARTESIAN_POINT('Ctrl Pts',(-17.7196137044144,17.352798261342,14.0493253817085));
#200122=CARTESIAN_POINT('Ctrl Pts',(-17.604967392435,17.4163916537719,14.041320236642));
#200123=CARTESIAN_POINT('Ctrl Pts',(-17.5077005723999,17.481400144653,14.0338816548519));
#200124=CARTESIAN_POINT('Ctrl Pts',(-17.2890242455132,17.655307404964,14.0156317693971));
#200125=CARTESIAN_POINT('Ctrl Pts',(-17.1738359726383,17.7708532554101,
14.0046806493747));
#200126=CARTESIAN_POINT('Ctrl Pts',(-17.0527786490054,17.9240467969068,
13.9922725077672));
#200127=CARTESIAN_POINT('Ctrl Pts',(-17.0331405496458,17.9501149221383,
13.9902271697918));
#200128=CARTESIAN_POINT('Ctrl Pts',(-17.0098856677209,17.9825166655757,
13.987774602756));
#200129=CARTESIAN_POINT('Ctrl Pts',(-17.0056897218789,17.9884268448191,
13.9873308091675));
#200130=CARTESIAN_POINT('Ctrl Pts',(-16.9991612511879,17.9977232713858,
13.9866384570032));
#200131=CARTESIAN_POINT('Ctrl Pts',(-16.9968081429046,18.0010948975714,
13.9863885236746));
#200132=CARTESIAN_POINT('Ctrl Pts',(-16.9924293000988,18.0074081864139,
13.9859227423806));
#200133=CARTESIAN_POINT('Ctrl Pts',(-16.9904012094102,18.0103480878408,
13.9857067382689));
#200134=CARTESIAN_POINT('Ctrl Pts',(-16.9857901705053,18.0170685299058,
13.9852149892101));
#200135=CARTESIAN_POINT('Ctrl Pts',(-16.98321204571,18.0208523187268,13.9849395725074));
#200136=CARTESIAN_POINT('Ctrl Pts',(-16.9753306568642,18.0325004823382,
13.9840960687318));
#200137=CARTESIAN_POINT('Ctrl Pts',(-16.9700678716026,18.0403922836419,
13.9835306466567));
#200138=CARTESIAN_POINT('Ctrl Pts',(-16.8985026535371,18.149286346342,13.9758077734178));
#200139=CARTESIAN_POINT('Ctrl Pts',(-16.8409021112143,18.2557642630198,
13.9691788512222));
#200140=CARTESIAN_POINT('Ctrl Pts',(-16.7212417796211,18.5308637742304,
13.9528531364415));
#200141=CARTESIAN_POINT('Ctrl Pts',(-16.6709342707907,18.7035221969101,
13.9432269751985));
#200142=CARTESIAN_POINT('Ctrl Pts',(-16.6396109529109,18.9016698411859,
13.931546709493));
#200143=CARTESIAN_POINT('Ctrl Pts',(-16.6365795287003,18.9229410749684,
13.9302860809617));
#200144=CARTESIAN_POINT('Ctrl Pts',(-16.6327352125529,18.9532079221095,
13.9284813669376));
#200145=CARTESIAN_POINT('Ctrl Pts',(-16.6316552496936,18.9621687129683,
13.9279457068064));
#200146=CARTESIAN_POINT('Ctrl Pts',(-16.6298928385996,18.9776232975215,
13.927019416919));
#200147=CARTESIAN_POINT('Ctrl Pts',(-16.6291830660321,18.9841138943763,
13.9266296538938));
#200148=CARTESIAN_POINT('Ctrl Pts',(-16.6278827007965,18.9965368039438,
13.9258821966779));
#200149=CARTESIAN_POINT('Ctrl Pts',(-16.6272871174503,19.0024685399363,
13.9255246637581));
#200150=CARTESIAN_POINT('Ctrl Pts',(-16.6258058221287,19.0178759935954,
13.9245943025838));
#200151=CARTESIAN_POINT('Ctrl Pts',(-16.6249589458899,19.0273552317331,
13.924020257734));
#200152=CARTESIAN_POINT('Ctrl Pts',(-16.6222991901077,19.0595762244486,
13.9220632342899));
#200153=CARTESIAN_POINT('Ctrl Pts',(-16.6207900662452,19.08234082903,13.9206707744085));
#200154=CARTESIAN_POINT('Ctrl Pts',(-16.610755260275,19.2827379019803,13.9083226741322));
#200155=CARTESIAN_POINT('Ctrl Pts',(-16.6242786936108,19.4607322600714,
13.8966418568998));
#200156=CARTESIAN_POINT('Ctrl Pts',(-16.6769703053261,19.7185506508725,
13.8792575885286));
#200157=CARTESIAN_POINT('Ctrl Pts',(-16.6991126331987,19.8010966920309,
13.8736345038582));
#200158=CARTESIAN_POINT('Ctrl Pts',(-16.7380394344089,19.9175618845139,
13.8657971684818));
#200159=CARTESIAN_POINT('Ctrl Pts',(-16.7508364498547,19.9527216506691,
13.8634448258777));
#200160=CARTESIAN_POINT('Ctrl Pts',(-16.7673280142462,19.9945478734847,
13.8606783139092));
#200161=CARTESIAN_POINT('Ctrl Pts',(-16.7701341729209,20.0015548600593,
13.8602159435152));
#200162=CARTESIAN_POINT('Ctrl Pts',(-16.7745514351743,20.0124161026467,
13.8595011119499));
#200163=CARTESIAN_POINT('Ctrl Pts',(-16.7761365392633,20.0162807694132,
13.8592471287445));
#200164=CARTESIAN_POINT('Ctrl Pts',(-16.7790953530739,20.0234343202682,
13.8587777222644));
#200165=CARTESIAN_POINT('Ctrl Pts',(-16.7804659177088,20.0267243976635,
13.8585621187336));
#200166=CARTESIAN_POINT('Ctrl Pts',(-16.7835806055966,20.0341484170485,
13.8580762485064));
#200167=CARTESIAN_POINT('Ctrl Pts',(-16.7853295608258,20.0382802734836,
13.8578062791063));
#200168=CARTESIAN_POINT('Ctrl Pts',(-16.7905227264005,20.050441131481,13.8570129250961));
#200169=CARTESIAN_POINT('Ctrl Pts',(-16.794003565405,20.0584545214519,13.8564917146073));
#200170=CARTESIAN_POINT('Ctrl Pts',(-16.8191828177947,20.1154525671578,
13.8527940658262));
#200171=CARTESIAN_POINT('Ctrl Pts',(-16.8426861647177,20.1636239002871,
13.8497198783941));
#200172=CARTESIAN_POINT('Ctrl Pts',(-16.8687418804884,20.2122510445528,
13.846617966454));
#200173=CARTESIAN_POINT('Ctrl Pts',(-16.8694912047369,20.2136457295714,
13.8465290012217));
#200174=CARTESIAN_POINT('Ctrl Pts',(-16.9499448449609,20.3629885559826,
13.8370026142969));
#200175=CARTESIAN_POINT('Ctrl Pts',(-17.0469830877593,20.5009270442499,
13.8281568217718));
#200176=CARTESIAN_POINT('Ctrl Pts',(-17.1986287364124,20.6696922788584,
13.8155775117368));
#200177=CARTESIAN_POINT('Ctrl Pts',(-17.2397418358419,20.7117797506953,
13.8122701236083));
#200178=CARTESIAN_POINT('Ctrl Pts',(-17.3087280757825,20.7767528411853,
13.8068257553542));
#200179=CARTESIAN_POINT('Ctrl Pts',(-17.3355272421349,20.8007344865888,
13.8047344763484));
#200180=CARTESIAN_POINT('Ctrl Pts',(-17.3713000663059,20.83114158881,13.8019663225418));
#200181=CARTESIAN_POINT('Ctrl Pts',(-17.3797323372157,20.8381966592026,
13.8013154720447));
#200182=CARTESIAN_POINT('Ctrl Pts',(-17.3935755057102,20.8495967547373,
13.8002494647671));
#200183=CARTESIAN_POINT('Ctrl Pts',(-17.3989535550439,20.8539814781596,
13.7998359263978));
#200184=CARTESIAN_POINT('Ctrl Pts',(-17.4093653563391,20.8623853433021,
13.7990364339964));
#200185=CARTESIAN_POINT('Ctrl Pts',(-17.4143960922524,20.8664081117642,
13.7986506323148));
#200186=CARTESIAN_POINT('Ctrl Pts',(-17.4259965408285,20.875597791774,13.7977620949432));
#200187=CARTESIAN_POINT('Ctrl Pts',(-17.432578618685,20.8807488561788,13.7972587346905));
#200188=CARTESIAN_POINT('Ctrl Pts',(-17.4502337558508,20.8943977707451,
13.7959105854448));
#200189=CARTESIAN_POINT('Ctrl Pts',(-17.4613605031513,20.9028252039088,
13.7950630392939));
#200190=CARTESIAN_POINT('Ctrl Pts',(-17.5524254343221,20.9703913757237,
13.7881422545663));
#200191=CARTESIAN_POINT('Ctrl Pts',(-17.636344870651,21.0239326422511,13.7818535544323));
#200192=CARTESIAN_POINT('Ctrl Pts',(-17.8752652868229,21.153680747242,13.7642222294857));
#200193=CARTESIAN_POINT('Ctrl Pts',(-18.0363028913904,21.2171525569805,
13.7525823078525));
#200194=CARTESIAN_POINT('Ctrl Pts',(-18.2419618706716,21.2704141600095,
13.7389940113692));
#200195=CARTESIAN_POINT('Ctrl Pts',(-18.2809540346393,21.2793418563952,
13.7364749385332));
#200196=CARTESIAN_POINT('Ctrl Pts',(-18.3277213637619,21.2886635495839,
13.7335397442831));
#200197=CARTESIAN_POINT('Ctrl Pts',(-18.3352725227154,21.2901259121459,
13.7330684823386));
#200198=CARTESIAN_POINT('Ctrl Pts',(-18.346967287639,21.2923246714394,13.7323429118898));
#200199=CARTESIAN_POINT('Ctrl Pts',(-18.3511053107049,21.2930899034384,
13.7320870086122));
#200200=CARTESIAN_POINT('Ctrl Pts',(-18.358749955898,21.2944800432895,13.7316158145563));
#200201=CARTESIAN_POINT('Ctrl Pts',(-18.3622558463511,21.2951084355035,
13.7314003322577));
#200202=CARTESIAN_POINT('Ctrl Pts',(-18.3701428439712,21.296501557907,13.7309169365973));
#200203=CARTESIAN_POINT('Ctrl Pts',(-18.3745247710316,21.2972613303741,
13.7306493071747));
#200204=CARTESIAN_POINT('Ctrl Pts',(-18.3857402754254,21.2991695764505,
13.7299666399164));
#200205=CARTESIAN_POINT('Ctrl Pts',(-18.3925772171162,21.3002983276923,
13.7295526957684));
#200206=CARTESIAN_POINT('Ctrl Pts',(-18.4324961258276,21.3066875941387,
13.7271480225704));
#200207=CARTESIAN_POINT('Ctrl Pts',(-18.4656956689786,21.3111962162708,
13.7251970334994));
#200208=CARTESIAN_POINT('Ctrl Pts',(-18.517213677266,21.3169508367706,13.7222257543013));
#200209=CARTESIAN_POINT('Ctrl Pts',(-18.5354632608623,21.3187496139726,
13.721184070428));
#200210=CARTESIAN_POINT('Ctrl Pts',(-18.5848602084064,21.3229711683156,
13.7183883942142));
#200211=CARTESIAN_POINT('Ctrl Pts',(-18.6160421535645,21.3249420445597,
13.7166492099635));
#200212=CARTESIAN_POINT('Ctrl Pts',(-18.6857207844649,21.3277994823183,
13.7127984913676));
#200213=CARTESIAN_POINT('Ctrl Pts',(-18.7242210427121,21.3283274266283,
13.7106949694213));
#200214=CARTESIAN_POINT('Ctrl Pts',(-18.871990195673,21.3263228986546,13.7026493649938));
#200215=CARTESIAN_POINT('Ctrl Pts',(-18.9809854365671,21.3163810967737,
13.6967644339791));
#200216=CARTESIAN_POINT('Ctrl Pts',(-19.1429757713918,21.2888489755441,
13.6876274419331));
#200217=CARTESIAN_POINT('Ctrl Pts',(-19.1968464670634,21.2775164048774,
13.6845241347417));
#200218=CARTESIAN_POINT('Ctrl Pts',(-19.283449812941,21.2557416712581,13.6793864704477));
#200219=CARTESIAN_POINT('Ctrl Pts',(-19.3164783870537,21.2465791145829,
13.6773913736653));
#200220=CARTESIAN_POINT('Ctrl Pts',(-19.3596071730437,21.2334790258985,
13.6747330307718));
#200221=CARTESIAN_POINT('Ctrl Pts',(-19.3699213050779,21.2302597238493,
13.6740932610015));
#200222=CARTESIAN_POINT('Ctrl Pts',(-19.3867782972178,21.2248562677711,
13.6730408441732));
#200223=CARTESIAN_POINT('Ctrl Pts',(-19.3933360067944,21.2227188175719,
13.6726297367327));
#200224=CARTESIAN_POINT('Ctrl Pts',(-19.4060125452849,21.2185183272665,
13.6718316978604));
#200225=CARTESIAN_POINT('Ctrl Pts',(-19.412132617633,21.2164592608179,13.6714449014303));
#200226=CARTESIAN_POINT('Ctrl Pts',(-19.4262461205299,21.2116388549707,
13.6705493662661));
#200227=CARTESIAN_POINT('Ctrl Pts',(-19.4342325760768,21.2088575663861,
13.6700399706809));
#200228=CARTESIAN_POINT('Ctrl Pts',(-19.4556758291152,21.2012455669553,
13.6686650616762));
#200229=CARTESIAN_POINT('Ctrl Pts',(-19.4691005277455,21.196326325187,13.6677966162071));
#200230=CARTESIAN_POINT('Ctrl Pts',(-19.5923288068216,21.1497503007377,
13.6597527064958));
#200231=CARTESIAN_POINT('Ctrl Pts',(-19.6985198484934,21.0991669976578,
13.6522722506534));
#200232=CARTESIAN_POINT('Ctrl Pts',(-19.9414512566245,20.9575884534316,
13.6339020086518));
#200233=CARTESIAN_POINT('Ctrl Pts',(-20.0728962327269,20.8589887583509,
13.6228709691785));
#200234=CARTESIAN_POINT('Ctrl Pts',(-20.2141768510264,20.7248459152367,
13.6105089203488));
#200235=CARTESIAN_POINT('Ctrl Pts',(-20.2362207476064,20.7029738693543,
13.6085649811454));
#200236=CARTESIAN_POINT('Ctrl Pts',(-20.2627314377079,20.675486302712,13.6062171643345));
#200237=CARTESIAN_POINT('Ctrl Pts',(-20.2676601523895,20.6703239804051,
13.6057802354619));
#200238=CARTESIAN_POINT('Ctrl Pts',(-20.2753701244454,20.6621663736319,
13.6050962036969));
#200239=CARTESIAN_POINT('Ctrl Pts',(-20.2781689230392,20.6591878477137,
13.604847778877));
#200240=CARTESIAN_POINT('Ctrl Pts',(-20.2833998752318,20.6535885795356,
13.6043832907146));
#200241=CARTESIAN_POINT('Ctrl Pts',(-20.2858339874894,20.6509698117177,
13.6041670803481));
#200242=CARTESIAN_POINT('Ctrl Pts',(-20.2913956817454,20.6449557174504,
13.6036728812598));
#200243=CARTESIAN_POINT('Ctrl Pts',(-20.2945187951976,20.6415563253114,
13.6033952334243));
#200244=CARTESIAN_POINT('Ctrl Pts',(-20.3041550095504,20.6309985589258,
13.6025380427304));
#200245=CARTESIAN_POINT('Ctrl Pts',(-20.3106302672645,20.6238056022485,
13.6019612919911));
#200246=CARTESIAN_POINT('Ctrl Pts',(-20.3791741512318,20.5466063575582,
13.5958448863841));
#200247=CARTESIAN_POINT('Ctrl Pts',(-20.4365943402133,20.472593958169,13.5906201605121));
#200248=CARTESIAN_POINT('Ctrl Pts',(-20.5627793897382,20.2855640012514,
13.578242942316));
#200249=CARTESIAN_POINT('Ctrl Pts',(-20.6262219468887,20.1694457514907,
13.5711935484779));
#200250=CARTESIAN_POINT('Ctrl Pts',(-20.6941947322286,20.0115708805455,
13.5616457046566));
#200251=CARTESIAN_POINT('Ctrl Pts',(-20.7089153611662,19.9745349775608,
13.5594101014325));
#200252=CARTESIAN_POINT('Ctrl Pts',(-20.722580608645,19.9371102966638,13.5571445218548));
#200253=CARTESIAN_POINT('',(-20.8509992001769,19.2129106825237,14.0892704698819));
#200254=CARTESIAN_POINT('Ctrl Pts',(-20.7225805710824,19.9371103995355,
13.3344633171505));
#200255=CARTESIAN_POINT('Ctrl Pts',(-20.714099989437,19.9603359584895,13.336089870733));
#200256=CARTESIAN_POINT('Ctrl Pts',(-20.7052104669082,19.9834185567835,
13.3377116194092));
#200257=CARTESIAN_POINT('Ctrl Pts',(-20.6896745200346,20.0217416997203,
13.3404079023461));
#200258=CARTESIAN_POINT('Ctrl Pts',(-20.6832526751649,20.0370623226433,
13.3414868207997));
#200259=CARTESIAN_POINT('Ctrl Pts',(-20.6554930751894,20.1011617266236,
13.3460010150011));
#200260=CARTESIAN_POINT('Ctrl Pts',(-20.6324975938024,20.1492065098487,
13.3493852707072));
#200261=CARTESIAN_POINT('Ctrl Pts',(-20.6036571521101,20.2040493757279,
13.353207619908));
#200262=CARTESIAN_POINT('Ctrl Pts',(-20.5995537730845,20.2117367559937,
13.3537424368348));
#200263=CARTESIAN_POINT('Ctrl Pts',(-20.5932681278435,20.2233394269715,
13.354547923945));
#200264=CARTESIAN_POINT('Ctrl Pts',(-20.5911207589636,20.2272733756704,
13.3548207273185));
#200265=CARTESIAN_POINT('Ctrl Pts',(-20.5872434542799,20.2343232138439,
13.3553090218582));
#200266=CARTESIAN_POINT('Ctrl Pts',(-20.5855181368739,20.2374415668869,
13.3555248006939));
#200267=CARTESIAN_POINT('Ctrl Pts',(-20.5817516686177,20.2442087157465,
13.3559926055366));
#200268=CARTESIAN_POINT('Ctrl Pts',(-20.5797075877119,20.2478558147259,
13.3562444401614));
#200269=CARTESIAN_POINT('Ctrl Pts',(-20.5739344739495,20.2580851744219,
13.3569500507283));
#200270=CARTESIAN_POINT('Ctrl Pts',(-20.5701809002478,20.2646536131018,
13.3574022784752));
#200271=CARTESIAN_POINT('Ctrl Pts',(-20.5475082460105,20.3038397277491,
13.3600959089861));
#200272=CARTESIAN_POINT('Ctrl Pts',(-20.5277543971108,20.3359695052267,
13.362286700065));
#200273=CARTESIAN_POINT('Ctrl Pts',(-20.4598655160041,20.4400519771557,
13.3693824172442));
#200274=CARTESIAN_POINT('Ctrl Pts',(-20.408174207836,20.509585243042,13.3741229213973));
#200275=CARTESIAN_POINT('Ctrl Pts',(-20.2388262196164,20.7104019699307,
13.3884175678289));
#200276=CARTESIAN_POINT('Ctrl Pts',(-20.1089430818994,20.8303310563656,
13.3978831230899));
#200277=CARTESIAN_POINT('Ctrl Pts',(-19.9470525241611,20.9461423837107,
13.4094501372104));
#200278=CARTESIAN_POINT('Ctrl Pts',(-19.9281749115875,20.9591881300637,
13.4107944810016));
#200279=CARTESIAN_POINT('Ctrl Pts',(-19.9011551667847,20.9772187871638,
13.4127141691007));
#200280=CARTESIAN_POINT('Ctrl Pts',(-19.8931852369537,20.9824597284118,
13.4132798681161));
#200281=CARTESIAN_POINT('Ctrl Pts',(-19.8801738311297,20.9908904843162,
13.4142026431836));
#200282=CARTESIAN_POINT('Ctrl Pts',(-19.8751537551993,20.9941132025755,
13.4145584861831));
#200283=CARTESIAN_POINT('Ctrl Pts',(-19.8646136993918,21.0008168200143,
13.4153052584736));
#200284=CARTESIAN_POINT('Ctrl Pts',(-19.8590911190167,21.0042934949104,
13.415696339352));
#200285=CARTESIAN_POINT('Ctrl Pts',(-19.8459085367891,21.0125075697508,
13.4166294358663));
#200286=CARTESIAN_POINT('Ctrl Pts',(-19.8382342505364,21.0172217012531,
13.4171723012111));
#200287=CARTESIAN_POINT('Ctrl Pts',(-19.8122482612514,21.0329567678506,
13.4190095089672));
#200288=CARTESIAN_POINT('Ctrl Pts',(-19.7938002763088,21.043749054994,13.4203121419455));
#200289=CARTESIAN_POINT('Ctrl Pts',(-19.6922717085249,21.1010989660828,
13.4274746095074));
#200290=CARTESIAN_POINT('Ctrl Pts',(-19.6062958858279,21.1422831036723,
13.4335234769039));
#200291=CARTESIAN_POINT('Ctrl Pts',(-19.3593924826863,21.2406973185158,
13.4507950654043));
#200292=CARTESIAN_POINT('Ctrl Pts',(-19.1938926996427,21.2844711270082,
13.462304652001));
#200293=CARTESIAN_POINT('Ctrl Pts',(-18.988496630972,21.3129690980325,13.4755396085012));
#200294=CARTESIAN_POINT('Ctrl Pts',(-18.9519258567018,21.3170748615545,
13.4778539234984));
#200295=CARTESIAN_POINT('Ctrl Pts',(-18.9081483700512,21.3208370445699,
13.4805596920531));
#200296=CARTESIAN_POINT('Ctrl Pts',(-18.9010293445624,21.3214125688606,
13.480997663745));
#200297=CARTESIAN_POINT('Ctrl Pts',(-18.8894079323888,21.3222929062983,
13.4817091568979));
#200298=CARTESIAN_POINT('Ctrl Pts',(-18.8849073101776,21.3226193658521,
13.4819838479591));
#200299=CARTESIAN_POINT('Ctrl Pts',(-18.8768482013101,21.3231780482486,
13.482474166745));
#200300=CARTESIAN_POINT('Ctrl Pts',(-18.873290153154,21.3234156716807,13.4826900926648));
#200301=CARTESIAN_POINT('Ctrl Pts',(-18.8655821738045,21.3239108876134,
13.4831566740311));
#200302=CARTESIAN_POINT('Ctrl Pts',(-18.8614320922034,21.3241652443711,
13.4834071464096));
#200303=CARTESIAN_POINT('Ctrl Pts',(-18.849834436901,21.3248417696012,13.484105102238));
#200304=CARTESIAN_POINT('Ctrl Pts',(-18.8423852568591,21.3252368087648,
13.4845510910201));
#200305=CARTESIAN_POINT('Ctrl Pts',(-18.7990570790752,21.3273049553139,
13.4871325677332));
#200306=CARTESIAN_POINT('Ctrl Pts',(-18.763139931681,21.3281042245254,13.4892222229809));
#200307=CARTESIAN_POINT('Ctrl Pts',(-18.6474865241204,21.327733690139,13.4958384900428));
#200308=CARTESIAN_POINT('Ctrl Pts',(-18.5678270879652,21.3229741107929,
13.5002250538236));
#200309=CARTESIAN_POINT('Ctrl Pts',(-18.3036688515648,21.2921480309304,
13.5147250553068));
#200310=CARTESIAN_POINT('Ctrl Pts',(-18.1223943214257,21.2462627739796,
13.5246812615265));
#200311=CARTESIAN_POINT('Ctrl Pts',(-17.9289826328832,21.1690914577697,
13.5367932104503));
#200312=CARTESIAN_POINT('Ctrl Pts',(-17.9086339339583,21.1606014776153,
13.538085731516));
#200313=CARTESIAN_POINT('Ctrl Pts',(-17.8806756847399,21.1484204526868,
13.5398884767732));
#200314=CARTESIAN_POINT('Ctrl Pts',(-17.8729496384795,21.1449991389044,
13.5403895221042));
#200315=CARTESIAN_POINT('Ctrl Pts',(-17.8597039230959,21.1390384546708,
13.5412535608802));
#200316=CARTESIAN_POINT('Ctrl Pts',(-17.8541742843991,21.1365213895884,
13.5416157861537));
#200317=CARTESIAN_POINT('Ctrl Pts',(-17.8427963618096,21.1312829695245,
13.5423642814023));
#200318=CARTESIAN_POINT('Ctrl Pts',(-17.8369495330777,21.1285586213036,
13.5427506517684));
#200319=CARTESIAN_POINT('Ctrl Pts',(-17.8233714229143,21.122156167156,13.5436520162441));
#200320=CARTESIAN_POINT('Ctrl Pts',(-17.8156498622229,21.1184578165047,
13.5441677086104));
#200321=CARTESIAN_POINT('Ctrl Pts',(-17.7910029068766,21.1064684618992,
13.5458238780106));
#200322=CARTESIAN_POINT('Ctrl Pts',(-17.7741660771847,21.0979984134206,
13.5469705797089));
#200323=CARTESIAN_POINT('Ctrl Pts',(-17.6906066949246,21.0545548102838,
13.5527402077935));
#200324=CARTESIAN_POINT('Ctrl Pts',(-17.6256781307248,21.0162657399933,
13.5574795258667));
#200325=CARTESIAN_POINT('Ctrl Pts',(-17.4719916056283,20.9142148557906,
13.56933492155));
#200326=CARTESIAN_POINT('Ctrl Pts',(-17.3858631201174,20.8468879893223,
13.5765508349481));
#200327=CARTESIAN_POINT('Ctrl Pts',(-17.2948305625363,20.7636371976547,
13.5847000357109));
#200328=CARTESIAN_POINT('Ctrl Pts',(-17.2844408245612,20.7539417154176,
13.5856382940039));
#200329=CARTESIAN_POINT('Ctrl Pts',(-17.1984073358917,20.6720210528694,
13.5934725087206));
#200330=CARTESIAN_POINT('Ctrl Pts',(-17.1281043658413,20.5943769405515,
13.6003057273877));
#200331=CARTESIAN_POINT('Ctrl Pts',(-17.0578711603,20.5042033629754,13.6073674632274));
#200332=CARTESIAN_POINT('Ctrl Pts',(-17.0519715232657,20.4965205315062,
13.6079626175343));
#200333=CARTESIAN_POINT('Ctrl Pts',(-17.0433374320107,20.4851155385267,
13.6088362114199));
#200334=CARTESIAN_POINT('Ctrl Pts',(-17.040562187945,20.4814246148239,13.6091174113764));
#200335=CARTESIAN_POINT('Ctrl Pts',(-17.0356595919814,20.4748598191969,
13.6096148357817));
#200336=CARTESIAN_POINT('Ctrl Pts',(-17.0335274236828,20.4719896121543,
13.6098313945607));
#200337=CARTESIAN_POINT('Ctrl Pts',(-17.028974171406,20.4658277251645,13.6102943326234));
#200338=CARTESIAN_POINT('Ctrl Pts',(-17.0265553493484,20.462534442844,13.6105405553369));
#200339=CARTESIAN_POINT('Ctrl Pts',(-17.0199405679013,20.4534733943254,
13.6112147826908));
#200340=CARTESIAN_POINT('Ctrl Pts',(-17.0157641537798,20.4476913327236,
13.6116414531712));
#200341=CARTESIAN_POINT('Ctrl Pts',(-16.9936027444247,20.4166808511105,
13.6139114216754));
#200342=CARTESIAN_POINT('Ctrl Pts',(-16.976142973047,20.3910795833401,13.6157208529884));
#200343=CARTESIAN_POINT('Ctrl Pts',(-16.8700919879331,20.2279971119139,
13.6269095658083));
#200344=CARTESIAN_POINT('Ctrl Pts',(-16.7971117252015,20.08100710477,13.6355534560693));
#200345=CARTESIAN_POINT('Ctrl Pts',(-16.7019663340167,19.8162959932826,
13.6509482649424));
#200346=CARTESIAN_POINT('Ctrl Pts',(-16.6714648710796,19.702413833633,13.6575165039292));
#200347=CARTESIAN_POINT('Ctrl Pts',(-16.6480480843424,19.5725219542311,
13.665248561539));
#200348=CARTESIAN_POINT('Ctrl Pts',(-16.6456535449103,19.558422777603,13.6660907125647));
#200349=CARTESIAN_POINT('Ctrl Pts',(-16.6420704654663,19.5359482403451,
13.6674381292322));
#200350=CARTESIAN_POINT('Ctrl Pts',(-16.6407889321607,19.5275879951391,
13.6679404478851));
#200351=CARTESIAN_POINT('Ctrl Pts',(-16.6386173999257,19.5128318352392,
13.6688290793997));
#200352=CARTESIAN_POINT('Ctrl Pts',(-16.6377064969351,19.5064390716212,
13.6692147251802));
#200353=CARTESIAN_POINT('Ctrl Pts',(-16.6358832057738,19.4932100011355,
13.6700141927525));
#200354=CARTESIAN_POINT('Ctrl Pts',(-16.634974950105,19.4863732106015,13.6704281403574));
#200355=CARTESIAN_POINT('Ctrl Pts',(-16.6327298117594,19.4688164098904,
13.6714932152976));
#200356=CARTESIAN_POINT('Ctrl Pts',(-16.6314415602274,19.4580904809252,
13.6721458697233));
#200357=CARTESIAN_POINT('Ctrl Pts',(-16.626410871443,19.4133130466284,13.6748790093008));
#200358=CARTESIAN_POINT('Ctrl Pts',(-16.6234133010094,19.3791846434934,
13.6769827635283));
#200359=CARTESIAN_POINT('Ctrl Pts',(-16.6177639888532,19.2901129386877,
13.6825301532353));
#200360=CARTESIAN_POINT('Ctrl Pts',(-16.616423234907,19.2351151293326,13.68601205213));
#200361=CARTESIAN_POINT('Ctrl Pts',(-16.6188189115814,19.0708366898491,
13.6965716227702));
#200362=CARTESIAN_POINT('Ctrl Pts',(-16.6288749874301,18.9618373954453,
13.7037977181733));
#200363=CARTESIAN_POINT('Ctrl Pts',(-16.6538425841158,18.8158536983178,
13.7135812115727));
#200364=CARTESIAN_POINT('Ctrl Pts',(-16.6614368350322,18.7777823795572,
13.7161412133366));
#200365=CARTESIAN_POINT('Ctrl Pts',(-16.6764912378106,18.7118221375845,
13.7205728943199));
#200366=CARTESIAN_POINT('Ctrl Pts',(-16.6834830384574,18.6838367104809,
13.7224519500333));
#200367=CARTESIAN_POINT('Ctrl Pts',(-16.7047152055288,18.6056807940748,
13.7276820630421));
#200368=CARTESIAN_POINT('Ctrl Pts',(-16.7202415782594,18.5558770246373,
13.7309945093287));
#200369=CARTESIAN_POINT('Ctrl Pts',(-16.7404765866114,18.4985194529803,
13.7347461132353));
#200370=CARTESIAN_POINT('Ctrl Pts',(-16.743410493025,18.4903630940372,13.7352780729219));
#200371=CARTESIAN_POINT('Ctrl Pts',(-16.7479339129004,18.4780262654958,
13.7360801170336));
#200372=CARTESIAN_POINT('Ctrl Pts',(-16.7494866725608,18.4738325482864,
13.736352308023));
#200373=CARTESIAN_POINT('Ctrl Pts',(-16.7523005262892,18.466306175514,13.7368399498039));
#200374=CARTESIAN_POINT('Ctrl Pts',(-16.7535567499692,18.462971771712,13.737055684844));
#200375=CARTESIAN_POINT('Ctrl Pts',(-16.7563079875154,18.4557246546391,
13.7375239044768));
#200376=CARTESIAN_POINT('Ctrl Pts',(-16.7578061915396,18.4518132142513,
13.7377761949221));
#200377=CARTESIAN_POINT('Ctrl Pts',(-16.7620557074149,18.4408165962108,
13.7384843727062));
#200378=CARTESIAN_POINT('Ctrl Pts',(-16.7648336130568,18.4337416690485,
13.7389386937051));
#200379=CARTESIAN_POINT('Ctrl Pts',(-16.7818510285622,18.3910776088956,
13.7416713945337));
#200380=CARTESIAN_POINT('Ctrl Pts',(-16.7970178564852,18.3558632130923,
13.7438974389364));
#200381=CARTESIAN_POINT('Ctrl Pts',(-16.8505630681125,18.2402877311501,
13.7511661148448));
#200382=CARTESIAN_POINT('Ctrl Pts',(-16.8930552414599,18.1619328442462,
13.7560350381166));
#200383=CARTESIAN_POINT('Ctrl Pts',(-17.0320404974686,17.9402470947443,
13.7702655157221));
#200384=CARTESIAN_POINT('Ctrl Pts',(-17.1412483627253,17.8057902296815,
13.7795583728622));
#200385=CARTESIAN_POINT('Ctrl Pts',(-17.2822664521819,17.6699949292943,
13.7909320811994));
#200386=CARTESIAN_POINT('Ctrl Pts',(-17.2992356712801,17.6541833183271,
13.7922906819857));
#200387=CARTESIAN_POINT('Ctrl Pts',(-17.3235756328385,17.6322397680457,
13.7942272443052));
#200388=CARTESIAN_POINT('Ctrl Pts',(-17.3307338664818,17.6258738474745,
13.7947953253153));
#200389=CARTESIAN_POINT('Ctrl Pts',(-17.3424250660992,17.6156179520643,
13.7957209251555));
#200390=CARTESIAN_POINT('Ctrl Pts',(-17.3469317748016,17.6116981482359,
13.7960771956445));
#200391=CARTESIAN_POINT('Ctrl Pts',(-17.3563921587688,17.6035398483496,
13.7968240031664));
#200392=CARTESIAN_POINT('Ctrl Pts',(-17.3613489390923,17.5993050639532,
13.797214687981));
#200393=CARTESIAN_POINT('Ctrl Pts',(-17.3731730123563,17.5892973776681,
13.7981452520512));
#200394=CARTESIAN_POINT('Ctrl Pts',(-17.3800575552127,17.583545134909,13.7986859688505));
#200395=CARTESIAN_POINT('Ctrl Pts',(-17.4033060344955,17.5643699500663,
13.800508383325));
#200396=CARTESIAN_POINT('Ctrl Pts',(-17.4198342468994,17.5511490206937,
13.8017981910926));
#200397=CARTESIAN_POINT('Ctrl Pts',(-17.5837507900191,17.4240151353829,
13.8145374047678));
#200398=CARTESIAN_POINT('Ctrl Pts',(-17.7453418021745,17.3297996082595,
13.8267959554362));
#200399=CARTESIAN_POINT('Ctrl Pts',(-17.985069458636,17.2295317459592,13.8439543901627));
#200400=CARTESIAN_POINT('Ctrl Pts',(-18.0544568764968,17.2046760562962,
13.8487976709831));
#200401=CARTESIAN_POINT('Ctrl Pts',(-18.165646234112,17.1712784552811,13.8562423375453));
#200402=CARTESIAN_POINT('Ctrl Pts',(-18.2066515294104,17.1602942353662,
13.8589218089182));
#200403=CARTESIAN_POINT('Ctrl Pts',(-18.2552234349893,17.1488366557899,
13.8619971148717));
#200404=CARTESIAN_POINT('Ctrl Pts',(-18.2624936686226,17.1471622058291,
13.8624548502572));
#200405=CARTESIAN_POINT('Ctrl Pts',(-18.2742693389211,17.1445155552961,
13.8631919173556));
#200406=CARTESIAN_POINT('Ctrl Pts',(-18.2787692913511,17.1435195904749,
13.8634725594934));
#200407=CARTESIAN_POINT('Ctrl Pts',(-18.2867651039416,17.1417772654529,
13.8639693679803));
#200408=CARTESIAN_POINT('Ctrl Pts',(-18.2902596332116,17.1410250569211,
13.8641858655702));
#200409=CARTESIAN_POINT('Ctrl Pts',(-18.2977584812327,17.1394307686739,
13.8646490839349));
#200410=CARTESIAN_POINT('Ctrl Pts',(-18.3017633297011,17.1385914484894,
13.864895645988));
#200411=CARTESIAN_POINT('Ctrl Pts',(-18.3127811107521,17.1363157129291,
13.8655717605959));
#200412=CARTESIAN_POINT('Ctrl Pts',(-18.3197990095529,17.1349032328616,
13.8659999665215));
#200413=CARTESIAN_POINT('Ctrl Pts',(-18.3575837602118,17.1274975833521,
13.8682929269956));
#200414=CARTESIAN_POINT('Ctrl Pts',(-18.3884754364149,17.1221523469643,
13.8701229969894));
#200415=CARTESIAN_POINT('Ctrl Pts',(-18.5813618835597,17.0931734967987,
13.8813369939068));
#200416=CARTESIAN_POINT('Ctrl Pts',(-18.7455393716564,17.0877085388961,
13.8899877300423));
#200417=CARTESIAN_POINT('Ctrl Pts',(-19.0254742134598,17.1108912785544,
13.9053635781708));
#200418=CARTESIAN_POINT('Ctrl Pts',(-19.141208036955,17.1302332706494,13.9119026743156));
#200419=CARTESIAN_POINT('Ctrl Pts',(-19.2685946818074,17.1625611192414,
13.9196019305026));
#200420=CARTESIAN_POINT('Ctrl Pts',(-19.2824133907115,17.1662173562977,
13.9204436838361));
#200421=CARTESIAN_POINT('Ctrl Pts',(-19.3043460798495,17.1722587579597,
13.9217905830302));
#200422=CARTESIAN_POINT('Ctrl Pts',(-19.3124847735985,17.1745531270505,
13.922292785483));
#200423=CARTESIAN_POINT('Ctrl Pts',(-19.3268136050104,17.1786853779578,
13.9231812816236));
#200424=CARTESIAN_POINT('Ctrl Pts',(-19.3330095236222,17.1805029469522,
13.9235669088817));
#200425=CARTESIAN_POINT('Ctrl Pts',(-19.3458068012147,17.1843206923529,
13.9243664069672));
#200426=CARTESIAN_POINT('Ctrl Pts',(-19.3524068863343,17.1863248410572,
13.9247804039474));
#200427=CARTESIAN_POINT('Ctrl Pts',(-19.3693219965263,17.1915516235456,
13.9258457510259));
#200428=CARTESIAN_POINT('Ctrl Pts',(-19.3796222597459,17.194821020997,13.9264986297217));
#200429=CARTESIAN_POINT('Ctrl Pts',(-19.4218508079554,17.2085815278659,
13.9291926508531));
#200430=CARTESIAN_POINT('Ctrl Pts',(-19.4535506985597,17.2197528881829,
13.9312560907756));
#200431=CARTESIAN_POINT('Ctrl Pts',(-19.5353266317394,17.2507792325233,
13.9366900412467));
#200432=CARTESIAN_POINT('Ctrl Pts',(-19.5849322295837,17.2717982573215,
13.9400972212999));
#200433=CARTESIAN_POINT('Ctrl Pts',(-19.7592183513054,17.3536227888732,
13.9524604745935));
#200434=CARTESIAN_POINT('Ctrl Pts',(-19.8786546037046,17.4247518687682,
13.9617005146233));
#200435=CARTESIAN_POINT('Ctrl Pts',(-20.0634095985323,17.5609643854179,
13.9767909036667));
#200436=CARTESIAN_POINT('Ctrl Pts',(-20.133015894145,17.6195522910692,13.982688180589));
#200437=CARTESIAN_POINT('Ctrl Pts',(-20.2056224655865,17.6891229876435,
13.9889007028638));
#200438=CARTESIAN_POINT('Ctrl Pts',(-20.2125519416844,17.6958543021151,
13.9894942389475));
#200439=CARTESIAN_POINT('Ctrl Pts',(-20.2227218545077,17.7058696011461,
13.990365919543));
#200440=CARTESIAN_POINT('Ctrl Pts',(-20.2259979113813,17.7091170115463,
13.9906468073772));
#200441=CARTESIAN_POINT('Ctrl Pts',(-20.2317940786145,17.7149001776599,
13.9911438870016));
#200442=CARTESIAN_POINT('Ctrl Pts',(-20.2343184032069,17.7174316319589,
13.9913604113936));
#200443=CARTESIAN_POINT('Ctrl Pts',(-20.2397164879855,17.7228724584363,
13.991823505609));
#200444=CARTESIAN_POINT('Ctrl Pts',(-20.242588226541,17.7257837579852,13.992069917661));
#200445=CARTESIAN_POINT('Ctrl Pts',(-20.2484651363593,17.7317762592988,
13.9925743398287));
#200446=CARTESIAN_POINT('Ctrl Pts',(-20.251469385212,17.7348583435255,13.9928322786039));
#200447=CARTESIAN_POINT('Ctrl Pts',(-20.2652668859293,17.7490999516008,
13.9940173986629));
#200448=CARTESIAN_POINT('Ctrl Pts',(-20.2759468995372,17.7603691654818,
13.994936146573));
#200449=CARTESIAN_POINT('Ctrl Pts',(-20.3410501612763,17.8305955550524,
14.0005530642606));
#200450=CARTESIAN_POINT('Ctrl Pts',(-20.3922148590281,17.8924959727615,
14.0050404365917));
#200451=CARTESIAN_POINT('Ctrl Pts',(-20.4809417866774,18.0132014549934,
14.0132761495103));
#200452=CARTESIAN_POINT('Ctrl Pts',(-20.5193513602725,18.071242185948,14.0170383228645));
#200453=CARTESIAN_POINT('Ctrl Pts',(-20.6313102356392,18.2600122713974,
14.0289664352486));
#200454=CARTESIAN_POINT('Ctrl Pts',(-20.6938625840409,18.396694031845,14.0371981702937));
#200455=CARTESIAN_POINT('Ctrl Pts',(-20.745951993975,18.5522596433864,14.0468106106721));
#200456=CARTESIAN_POINT('Ctrl Pts',(-20.7503149288445,18.5657374358616,
14.0476449383686));
#200457=CARTESIAN_POINT('Ctrl Pts',(-20.7570544842117,18.5872929930894,
14.0489821722094));
#200458=CARTESIAN_POINT('Ctrl Pts',(-20.7595187957101,18.5953430487196,
14.049482201439));
#200459=CARTESIAN_POINT('Ctrl Pts',(-20.7637864754445,18.6095870973499,
14.0503681693453));
#200460=CARTESIAN_POINT('Ctrl Pts',(-20.7656096811759,18.6157750699929,
14.0507534537642));
#200461=CARTESIAN_POINT('Ctrl Pts',(-20.7693280079652,18.6286112216265,
14.0515535403252));
#200462=CARTESIAN_POINT('Ctrl Pts',(-20.7712189024992,18.6352605357287,
14.0519684750335));
#200463=CARTESIAN_POINT('Ctrl Pts',(-20.7760008794889,18.652394861015,14.0530389870521));
#200464=CARTESIAN_POINT('Ctrl Pts',(-20.7788437624975,18.6628930093539,
14.0536961216643));
#200465=CARTESIAN_POINT('Ctrl Pts',(-20.7848190523309,18.6856521613353,
14.0551235603184));
#200466=CARTESIAN_POINT('Ctrl Pts',(-20.7879226552397,18.6979202280657,
14.0558947687061));
#200467=CARTESIAN_POINT('Ctrl Pts',(-20.79663370116,18.7336998467524,14.0581493586585));
#200468=CARTESIAN_POINT('Ctrl Pts',(-20.8019485569284,18.7572799187343,
14.0596419606873));
#200469=CARTESIAN_POINT('Ctrl Pts',(-20.8363441724377,18.9230662790745,
14.0701853687219));
#200470=CARTESIAN_POINT('Ctrl Pts',(-20.8511300495927,19.0678165918601,
14.0796831108336));
#200471=CARTESIAN_POINT('Ctrl Pts',(-20.8509991383142,19.2129100724755,
14.0892705377863));
#200472=CARTESIAN_POINT('Ctrl Pts',(-20.8509991377702,19.2129106753478,
14.0892705776226));
#200473=CARTESIAN_POINT('Ctrl Pts',(-20.8508884782116,19.3355197780962,
14.0973722912252));
#200474=CARTESIAN_POINT('Ctrl Pts',(-20.840126423568,19.4579019518155,14.1054939843093));
#200475=CARTESIAN_POINT('Ctrl Pts',(-20.8166444881502,19.5910510982751,
14.1139586039406));
#200476=CARTESIAN_POINT('Ctrl Pts',(-20.814351877406,19.6034066563032,14.1147403450995));
#200477=CARTESIAN_POINT('Ctrl Pts',(-20.8106712450187,19.6223030872299,
14.1159294515346));
#200478=CARTESIAN_POINT('Ctrl Pts',(-20.8093620687928,19.6288587985602,
14.116340787568));
#200479=CARTESIAN_POINT('Ctrl Pts',(-20.8071513247562,19.6396623843232,
14.1170165517433));
#200480=CARTESIAN_POINT('Ctrl Pts',(-20.8062677127861,19.6439138278879,
14.1172819409962));
#200481=CARTESIAN_POINT('Ctrl Pts',(-20.8045210246822,19.6521900148307,
14.1177974780946));
#200482=CARTESIAN_POINT('Ctrl Pts',(-20.803659279343,19.6562150165181,14.1180476988373));
#200483=CARTESIAN_POINT('Ctrl Pts',(-20.8020280139603,19.6637271643379,
14.1185137302678));
#200484=CARTESIAN_POINT('Ctrl Pts',(-20.8012614185717,19.6672148390563,
14.1187296988306));
#200485=CARTESIAN_POINT('Ctrl Pts',(-20.7994932703674,19.6751631714775,
14.1192209982101));
#200486=CARTESIAN_POINT('Ctrl Pts',(-20.7984860931349,19.6796225259647,
14.1194960031171));
#200487=CARTESIAN_POINT('Ctrl Pts',(-20.7953527020391,19.6932896856474,
14.1203369943829));
#200488=CARTESIAN_POINT('Ctrl Pts',(-20.7931792402637,19.702486690609,14.1209003387533));
#200489=CARTESIAN_POINT('Ctrl Pts',(-20.7723521707152,19.7880524400293,
14.1261200192409));
#200490=CARTESIAN_POINT('Ctrl Pts',(-20.749526058459,19.8633154573807,14.1305523841898));
#200491=CARTESIAN_POINT('Ctrl Pts',(-20.7225805809329,19.9371103725581,
14.1348941200942));
#200492=CARTESIAN_POINT('Origin',(-18.734,19.211,0.));
#200493=CARTESIAN_POINT('',(-20.7225806064499,19.9371103026755,15.1555945416419));
#200494=CARTESIAN_POINT('',(-20.7225805830531,19.9371103667517,14.9318515409431));
#200495=CARTESIAN_POINT('',(-20.7225806064498,19.9371103026755,0.));
#200496=CARTESIAN_POINT('',(-20.8523540121835,19.2127405753659,15.110942953294));
#200497=CARTESIAN_POINT('Ctrl Pts',(-20.8509992748742,19.2127521935257,
15.1109437209775));
#200498=CARTESIAN_POINT('Ctrl Pts',(-20.8509006165464,19.3319511321298,
15.1181312937192));
#200499=CARTESIAN_POINT('Ctrl Pts',(-20.8407310772906,19.4507453566806,
15.1253188664609));
#200500=CARTESIAN_POINT('Ctrl Pts',(-20.8207141748805,19.5678094061999,
15.1325064392026));
#200501=CARTESIAN_POINT('Ctrl Pts',(-20.8084963315169,19.6392625307264,
15.1368935634501));
#200502=CARTESIAN_POINT('Ctrl Pts',(-20.7925803619098,19.7102268266174,
15.1412806876976));
#200503=CARTESIAN_POINT('Ctrl Pts',(-20.7730188005824,19.7802901991706,
15.145667811945));
#200504=CARTESIAN_POINT('Ctrl Pts',(-20.75826484326,19.8331342432225,15.148976721844));
#200505=CARTESIAN_POINT('Ctrl Pts',(-20.7414381049983,19.8854657305472,
15.152285631743));
#200506=CARTESIAN_POINT('Ctrl Pts',(-20.7225806064499,19.9371103026755,
15.1555945416419));
#200507=CARTESIAN_POINT('Ctrl Pts',(-20.7249099185723,19.937940853899,14.355439970105));
#200508=CARTESIAN_POINT('Ctrl Pts',(-20.6989346035943,20.0108543135692,
14.360110513108));
#200509=CARTESIAN_POINT('Ctrl Pts',(-20.3954319215272,20.7297352208536,
14.4071729916714));
#200510=CARTESIAN_POINT('Ctrl Pts',(-19.0148744787979,21.6984565315259,
14.4966274057954));
#200511=CARTESIAN_POINT('Ctrl Pts',(-16.7944747336859,20.7935840294885,
14.6238032124768));
#200512=CARTESIAN_POINT('Ctrl Pts',(-16.3534690399024,18.4367889066407,
14.7509790191583));
#200513=CARTESIAN_POINT('Ctrl Pts',(-18.0964527495933,16.7902844089888,
14.8781548258396));
#200514=CARTESIAN_POINT('Ctrl Pts',(-20.2927766449214,17.3321745234098,
14.9981428038849));
#200515=CARTESIAN_POINT('Ctrl Pts',(-20.8471440588156,18.6285361211804,
15.0757388463697));
#200516=CARTESIAN_POINT('Ctrl Pts',(-20.8523540121835,19.2127405753659,
15.110942953294));
#200517=CARTESIAN_POINT('Ctrl Pts',(-20.7225805809329,19.9371103725581,
14.1348941200942));
#200518=CARTESIAN_POINT('Ctrl Pts',(-20.7075027445907,19.9784036713261,
14.1373236180813));
#200519=CARTESIAN_POINT('Ctrl Pts',(-20.6911350749698,20.0192372971913,
14.1397245483283));
#200520=CARTESIAN_POINT('Ctrl Pts',(-20.6449226516951,20.1248631733796,
14.1459967998668));
#200521=CARTESIAN_POINT('Ctrl Pts',(-20.6130668885677,20.1886905292902,
14.1498508365716));
#200522=CARTESIAN_POINT('Ctrl Pts',(-20.5342698885964,20.3284360931426,
14.158640741542));
#200523=CARTESIAN_POINT('Ctrl Pts',(-20.4856308923035,20.4032340607066,
14.1635990977973));
#200524=CARTESIAN_POINT('Ctrl Pts',(-20.4120570099747,20.5021150089675,
14.1706900328253));
#200525=CARTESIAN_POINT('Ctrl Pts',(-20.39103012142,20.5289925183535,14.172676241559));
#200526=CARTESIAN_POINT('Ctrl Pts',(-20.3624522619252,20.5637566990417,
14.1753300352325));
#200527=CARTESIAN_POINT('Ctrl Pts',(-20.3554761641233,20.5721107591439,
14.1759744171542));
#200528=CARTESIAN_POINT('Ctrl Pts',(-20.3439632380515,20.5856836669195,
14.177032489082));
#200529=CARTESIAN_POINT('Ctrl Pts',(-20.3394646543371,20.5909348005986,
14.1774446068526));
#200530=CARTESIAN_POINT('Ctrl Pts',(-20.3307199602477,20.6010417172682,
14.1782432344864));
#200531=CARTESIAN_POINT('Ctrl Pts',(-20.326477218989,20.6059003235973,14.1786296020724));
#200532=CARTESIAN_POINT('Ctrl Pts',(-20.3166485363715,20.6170524245627,
14.1795221554944));
#200533=CARTESIAN_POINT('Ctrl Pts',(-20.3110471704809,20.6233321242477,
14.1800289844274));
#200534=CARTESIAN_POINT('Ctrl Pts',(-20.2959249753151,20.6400835076497,
14.1813924909934));
#200535=CARTESIAN_POINT('Ctrl Pts',(-20.2863364528878,20.6504932518482,
14.1822520255119));
#200536=CARTESIAN_POINT('Ctrl Pts',(-20.2021775981613,20.7400412337915,
14.1897542468199));
#200537=CARTESIAN_POINT('Ctrl Pts',(-20.1217285188347,20.8134093595933,
14.196656521211));
#200538=CARTESIAN_POINT('Ctrl Pts',(-19.9589779544846,20.9403532531287,
14.2100961836297));
#200539=CARTESIAN_POINT('Ctrl Pts',(-19.8778787207691,20.9950329876922,
14.2165813580757));
#200540=CARTESIAN_POINT('Ctrl Pts',(-19.7310563154312,21.0798862323185,
14.2277585212487));
#200541=CARTESIAN_POINT('Ctrl Pts',(-19.6670177360556,21.1126667382505,
14.2324626464547));
#200542=CARTESIAN_POINT('Ctrl Pts',(-19.5707240266837,21.1559203325036,
14.2391778324342));
#200543=CARTESIAN_POINT('Ctrl Pts',(-19.5396899638316,21.1689801262702,
14.2412894979581));
#200544=CARTESIAN_POINT('Ctrl Pts',(-19.5015751173138,21.1839598365988,
14.2438083954485));
#200545=CARTESIAN_POINT('Ctrl Pts',(-19.4947807280694,21.1865897258538,
14.2442545711192));
#200546=CARTESIAN_POINT('Ctrl Pts',(-19.4840926108851,21.190663435538,14.2449518292703));
#200547=CARTESIAN_POINT('Ctrl Pts',(-19.4802080551625,21.1921309350987,
14.2452042927434));
#200548=CARTESIAN_POINT('Ctrl Pts',(-19.4729790589859,21.1948376119825,
14.2456723144294));
#200549=CARTESIAN_POINT('Ctrl Pts',(-19.4696358374338,21.1960797553975,
14.2458880439109));
#200550=CARTESIAN_POINT('Ctrl Pts',(-19.4620487015655,21.1988768865442,
14.2463760091694));
#200551=CARTESIAN_POINT('Ctrl Pts',(-19.457802947611,21.2004267319526,14.2466479365073));
#200552=CARTESIAN_POINT('Ctrl Pts',(-19.445190966769,21.2049848170869,14.2474524144538));
#200553=CARTESIAN_POINT('Ctrl Pts',(-19.4368105974676,21.2079540085681,
14.2479826988741));
#200554=CARTESIAN_POINT('Ctrl Pts',(-19.3737718093276,21.2298428602992,
14.2519413590458));
#200555=CARTESIAN_POINT('Ctrl Pts',(-19.3183720860012,21.2465699437743,
14.2552503475475));
#200556=CARTESIAN_POINT('Ctrl Pts',(-19.1043072086437,21.3017412218326,
14.2676373541398));
#200557=CARTESIAN_POINT('Ctrl Pts',(-18.9420769950573,21.324063329741,14.2762437750213));
#200558=CARTESIAN_POINT('Ctrl Pts',(-18.7188478806076,21.3287973145088,
14.2886115840558));
#200559=CARTESIAN_POINT('Ctrl Pts',(-18.6587878699798,21.3275153878792,
14.2919854993993));
#200560=CARTESIAN_POINT('Ctrl Pts',(-18.5747286589263,21.3221387123029,
14.2968224145711));
#200561=CARTESIAN_POINT('Ctrl Pts',(-18.5506197109285,21.3201812688754,
14.2982228471611));
#200562=CARTESIAN_POINT('Ctrl Pts',(-18.5085712708542,21.316040917951,14.3006913188793));
#200563=CARTESIAN_POINT('Ctrl Pts',(-18.4906161078813,21.3140405676679,
14.301753686834));
#200564=CARTESIAN_POINT('Ctrl Pts',(-18.4642184900994,21.3107570809678,
14.3033286556341));
#200565=CARTESIAN_POINT('Ctrl Pts',(-18.4557543798612,21.3096522422203,
14.3038356368359));
#200566=CARTESIAN_POINT('Ctrl Pts',(-18.4409102064075,21.3076232207399,
14.3047283447093));
#200567=CARTESIAN_POINT('Ctrl Pts',(-18.4345272129133,21.3067210227579,
14.30511337166));
#200568=CARTESIAN_POINT('Ctrl Pts',(-18.4221291229341,21.3049108293485,
14.3058635331603));
#200569=CARTESIAN_POINT('Ctrl Pts',(-18.4161136177958,21.3040060324884,
14.3062285627946));
#200570=CARTESIAN_POINT('Ctrl Pts',(-18.4017234817992,21.3017781326947,
14.3071043381384));
#200571=CARTESIAN_POINT('Ctrl Pts',(-18.3933527848819,21.3004306296843,
14.307615853762));
#200572=CARTESIAN_POINT('Ctrl Pts',(-18.3630621143995,21.2953676195601,
14.309474522269));
#200573=CARTESIAN_POINT('Ctrl Pts',(-18.3411935150339,21.2913572516898,
14.310830997205));
#200574=CARTESIAN_POINT('Ctrl Pts',(-18.1386282032922,21.2509020932711,
14.3235359568818));
#200575=CARTESIAN_POINT('Ctrl Pts',(-17.9633851786215,21.1913519550015,
14.3356714120186));
#200576=CARTESIAN_POINT('Ctrl Pts',(-17.7254648935146,21.0740901273226,
14.3531857352959));
#200577=CARTESIAN_POINT('Ctrl Pts',(-17.6549310632739,21.0341455939937,
14.3585088996915));
#200578=CARTESIAN_POINT('Ctrl Pts',(-17.5563846289528,20.970609467035,14.3659848135715));
#200579=CARTESIAN_POINT('Ctrl Pts',(-17.5264210921241,20.9501828496055,
14.368262971875));
#200580=CARTESIAN_POINT('Ctrl Pts',(-17.4909249822137,20.9246246522119,
14.3709540367914));
#200581=CARTESIAN_POINT('Ctrl Pts',(-17.4848779903975,20.9202217987955,
14.3714121961819));
#200582=CARTESIAN_POINT('Ctrl Pts',(-17.4755025499349,20.9133191512315,
14.3721219370661));
#200583=CARTESIAN_POINT('Ctrl Pts',(-17.4721579929903,20.910841485111,14.3723750066527));
#200584=CARTESIAN_POINT('Ctrl Pts',(-17.465961969051,20.9062230724059,14.3728435773018));
#200585=CARTESIAN_POINT('Ctrl Pts',(-17.463108629678,20.9040850062153,14.3730592532255));
#200586=CARTESIAN_POINT('Ctrl Pts',(-17.4566612144526,20.8992283418441,
14.3735463677906));
#200587=CARTESIAN_POINT('Ctrl Pts',(-17.4530704185527,20.8965054777441,
14.3738175025004));
#200588=CARTESIAN_POINT('Ctrl Pts',(-17.4422376509934,20.888236488411,14.3746350825371));
#200589=CARTESIAN_POINT('Ctrl Pts',(-17.4350226952681,20.8826549204064,
14.3751790954352));
#200590=CARTESIAN_POINT('Ctrl Pts',(-17.3795538997159,20.839167680719,14.379359391647));
#200591=CARTESIAN_POINT('Ctrl Pts',(-17.3329278455319,20.7992230759704,
14.3828612289333));
#200592=CARTESIAN_POINT('Ctrl Pts',(-17.1808303155901,20.6570015085998,
14.3944981721722));
#200593=CARTESIAN_POINT('Ctrl Pts',(-17.0842857608965,20.5458048286567,
14.4022854888115));
#200594=CARTESIAN_POINT('Ctrl Pts',(-16.946810279657,20.3495280655668,14.4154839112159));
#200595=CARTESIAN_POINT('Ctrl Pts',(-16.8986517639734,20.2701445724771,
14.4206924526458));
#200596=CARTESIAN_POINT('Ctrl Pts',(-16.8461314902584,20.1691678592443,
14.4273222647719));
#200597=CARTESIAN_POINT('Ctrl Pts',(-16.8366866789988,20.1503270310562,
14.4285591608391));
#200598=CARTESIAN_POINT('Ctrl Pts',(-16.8236313879887,20.1232833866047,
14.4303357088599));
#200599=CARTESIAN_POINT('Ctrl Pts',(-16.8197890746599,20.1151934200088,
14.4308672946605));
#200600=CARTESIAN_POINT('Ctrl Pts',(-16.8132398763448,20.1011752719942,
14.4317887620705));
#200601=CARTESIAN_POINT('Ctrl Pts',(-16.8105087979129,20.0952584811709,
14.4321778010639));
#200602=CARTESIAN_POINT('Ctrl Pts',(-16.8053256295102,20.0838916813101,
14.4329254282378));
#200603=CARTESIAN_POINT('Ctrl Pts',(-16.8028692096263,20.0784437065406,
14.4332838626625));
#200604=CARTESIAN_POINT('Ctrl Pts',(-16.7965281041514,20.0642196452384,
14.4342200070783));
#200605=CARTESIAN_POINT('Ctrl Pts',(-16.7926800043324,20.0554274864664,
14.4347989638389));
#200606=CARTESIAN_POINT('Ctrl Pts',(-16.7796943185482,20.0251997776535,
14.436790666187));
#200607=CARTESIAN_POINT('Ctrl Pts',(-16.7708511825201,20.0036402884189,
14.43821335448));
#200608=CARTESIAN_POINT('Ctrl Pts',(-16.7001112797976,19.8227270908541,
14.4501735258314));
#200609=CARTESIAN_POINT('Ctrl Pts',(-16.6573818896966,19.6565882069872,
14.461374321672));
#200610=CARTESIAN_POINT('Ctrl Pts',(-16.6233195846727,19.3977037016305,
14.4786292814234));
#200611=CARTESIAN_POINT('Ctrl Pts',(-16.617279810624,19.3075801299548,14.4845839137008));
#200612=CARTESIAN_POINT('Ctrl Pts',(-16.6168937955224,19.1787164502282,
14.492816935175));
#200613=CARTESIAN_POINT('Ctrl Pts',(-16.6178351962036,19.1400925501234,
14.4952478567591));
#200614=CARTESIAN_POINT('Ctrl Pts',(-16.6202270324269,19.0939066198248,
14.498094016606));
#200615=CARTESIAN_POINT('Ctrl Pts',(-16.6206620228555,19.0863018984478,
14.4985606726401));
#200616=CARTESIAN_POINT('Ctrl Pts',(-16.6214000360126,19.0745156949966,
14.4992806819838));
#200617=CARTESIAN_POINT('Ctrl Pts',(-16.6216744450782,19.0703325763396,
14.4995355922054));
#200618=CARTESIAN_POINT('Ctrl Pts',(-16.6222050645947,19.0625956694284,
14.5000058566502));
#200619=CARTESIAN_POINT('Ctrl Pts',(-16.6224578188473,19.0590417423849,
14.5002213965798));
#200620=CARTESIAN_POINT('Ctrl Pts',(-16.6230477153701,19.0510330994009,
14.5007060490312));
#200621=CARTESIAN_POINT('Ctrl Pts',(-16.6233899857452,19.0465788157189,
14.5009748708014));
#200622=CARTESIAN_POINT('Ctrl Pts',(-16.6244361134988,19.0335064084795,
14.5017617379335));
#200623=CARTESIAN_POINT('Ctrl Pts',(-16.6251786836259,19.0248913552421,
14.5022776619906));
#200624=CARTESIAN_POINT('Ctrl Pts',(-16.6307250371006,18.9648466096778,
14.5058565896829));
#200625=CARTESIAN_POINT('Ctrl Pts',(-16.6373573233712,18.9135987862299,
14.5088246083189));
#200626=CARTESIAN_POINT('Ctrl Pts',(-16.6494417926672,18.8411618435247,
14.5129605195427));
#200627=CARTESIAN_POINT('Ctrl Pts',(-16.6533563331053,18.8197390150789,
14.5141762236957));
#200628=CARTESIAN_POINT('Ctrl Pts',(-16.6665987112314,18.7531003226135,
14.5179446567348));
#200629=CARTESIAN_POINT('Ctrl Pts',(-16.677075593898,18.7081258244164,14.5204691137869));
#200630=CARTESIAN_POINT('Ctrl Pts',(-16.71729483546,18.5578937437471,14.52893643587));
#200631=CARTESIAN_POINT('Ctrl Pts',(-16.7537170532173,18.4546098425893,
14.5348247787239));
#200632=CARTESIAN_POINT('Ctrl Pts',(-16.8202492865064,18.3042006774433,
14.5439697023021));
#200633=CARTESIAN_POINT('Ctrl Pts',(-16.8445041512232,18.254688546192,14.5470775553507));
#200634=CARTESIAN_POINT('Ctrl Pts',(-16.8869471151252,18.1759821992873,
14.5522220740495));
#200635=CARTESIAN_POINT('Ctrl Pts',(-16.9039633383107,18.146184604005,14.5542193418497));
#200636=CARTESIAN_POINT('Ctrl Pts',(-16.9272822628123,18.1075613484377,
14.5568801673014));
#200637=CARTESIAN_POINT('Ctrl Pts',(-16.9329397966025,18.0983509192882,
14.5575201926022));
#200638=CARTESIAN_POINT('Ctrl Pts',(-16.9423229767659,18.0833342559912,
14.5585729226801));
#200639=CARTESIAN_POINT('Ctrl Pts',(-16.946006951958,18.0775021198882,14.5589840860392));
#200640=CARTESIAN_POINT('Ctrl Pts',(-16.9531942095638,18.0662461281677,
14.5597821569104));
#200641=CARTESIAN_POINT('Ctrl Pts',(-16.9566939348696,18.0608200837504,
14.5601689290155));
#200642=CARTESIAN_POINT('Ctrl Pts',(-16.9648334169415,18.0483263222915,
14.5610642963304));
#200643=CARTESIAN_POINT('Ctrl Pts',(-16.969490776313,18.0412702552592,14.5615735476171));
#200644=CARTESIAN_POINT('Ctrl Pts',(-16.9821331267667,18.0223639562508,
14.5629478146742));
#200645=CARTESIAN_POINT('Ctrl Pts',(-16.9901959324398,18.0105665181789,
14.5638157582371));
#200646=CARTESIAN_POINT('Ctrl Pts',(-17.0652574946945,17.9030891097816,
14.5718203439441));
#200647=CARTESIAN_POINT('Ctrl Pts',(-17.1399371142987,17.8130414299508,
14.5792585290705));
#200648=CARTESIAN_POINT('Ctrl Pts',(-17.3354199716359,17.6134713819786,
14.5975058499753));
#200649=CARTESIAN_POINT('Ctrl Pts',(-17.4621895610557,17.5108170568064,
14.6084547013722));
#200650=CARTESIAN_POINT('Ctrl Pts',(-17.6270395097253,17.4061745833797,
14.6208636871663));
#200651=CARTESIAN_POINT('Ctrl Pts',(-17.6550249474443,17.3893058929064,
14.6229115124145));
#200652=CARTESIAN_POINT('Ctrl Pts',(-17.6896861242341,17.3694924380092,
14.62536664193));
#200653=CARTESIAN_POINT('Ctrl Pts',(-17.695999451984,17.3659264410847,14.6258105989811));
#200654=CARTESIAN_POINT('Ctrl Pts',(-17.7059218470725,17.3603889601486,
14.6265031491889));
#200655=CARTESIAN_POINT('Ctrl Pts',(-17.7095184801269,17.3583954751621,
14.6267531183667));
#200656=CARTESIAN_POINT('Ctrl Pts',(-17.7162497645866,17.3546901621181,
14.6272189307998));
#200657=CARTESIAN_POINT('Ctrl Pts',(-17.7193829050965,17.3529758056304,
14.6274349304174));
#200658=CARTESIAN_POINT('Ctrl Pts',(-17.7265418266783,17.349082175748,14.62792662311));
#200659=CARTESIAN_POINT('Ctrl Pts',(-17.7305703391558,17.3469080301924,
14.628201988233));
#200660=CARTESIAN_POINT('Ctrl Pts',(-17.7429638644626,17.3402711939668,
14.62904517706));
#200661=CARTESIAN_POINT('Ctrl Pts',(-17.7513519619008,17.3358515449577,
14.629610338656));
#200662=CARTESIAN_POINT('Ctrl Pts',(-17.8671857826812,17.2758099794782,
14.6373430419722));
#200663=CARTESIAN_POINT('Ctrl Pts',(-17.9791940981658,17.2294339722747,
14.6439805394056));
#200664=CARTESIAN_POINT('Ctrl Pts',(-18.2651920541203,17.1388165594462,
14.6603064926629));
#200665=CARTESIAN_POINT('Ctrl Pts',(-18.4419635492511,17.1066158183815,
14.6699251819398));
#200666=CARTESIAN_POINT('Ctrl Pts',(-18.6421236112204,17.0958855459716,
14.6815961476636));
#200667=CARTESIAN_POINT('Ctrl Pts',(-18.6635892524944,17.0950622170958,
14.6828565027497));
#200668=CARTESIAN_POINT('Ctrl Pts',(-18.694085586048,17.0943570713107,14.6846608925073));
#200669=CARTESIAN_POINT('Ctrl Pts',(-18.7031091628754,17.0942061507193,
14.6851965060007));
#200670=CARTESIAN_POINT('Ctrl Pts',(-18.7186621421395,17.0940454940806,
14.68612274061));
#200671=CARTESIAN_POINT('Ctrl Pts',(-18.7251911802201,17.0940082585807,
14.6865124952718));
#200672=CARTESIAN_POINT('Ctrl Pts',(-18.7376819722161,17.0939948074014,
14.6872599541023));
#200673=CARTESIAN_POINT('Ctrl Pts',(-18.7436436666921,17.0940135709052,
14.6876174970851));
#200674=CARTESIAN_POINT('Ctrl Pts',(-18.759122807348,17.0941276762233,14.6885479230633));
#200675=CARTESIAN_POINT('Ctrl Pts',(-18.7686397536842,17.0942620205944,
14.6891220229911));
#200676=CARTESIAN_POINT('Ctrl Pts',(-18.8009696848581,17.094936489212,14.6910794357538));
#200677=CARTESIAN_POINT('Ctrl Pts',(-18.8237740953053,17.0957812717743,
14.6924722350018));
#200678=CARTESIAN_POINT('Ctrl Pts',(-19.0240757495337,17.1064462853124,
14.7048165381823));
#200679=CARTESIAN_POINT('Ctrl Pts',(-19.1996626756419,17.1382182413091,
14.7164925876397));
#200680=CARTESIAN_POINT('Ctrl Pts',(-19.4506665592065,17.21716552418,14.7338755326956));
#200681=CARTESIAN_POINT('Ctrl Pts',(-19.5305375956243,17.2477077121202,
14.7395018360911));
#200682=CARTESIAN_POINT('Ctrl Pts',(-19.642427065061,17.2984494911567,14.7473430319348));
#200683=CARTESIAN_POINT('Ctrl Pts',(-19.6760922456736,17.3148059751004,
14.7496961544111));
#200684=CARTESIAN_POINT('Ctrl Pts',(-19.7160080817448,17.3355250981281,
14.7524634582063));
#200685=CARTESIAN_POINT('Ctrl Pts',(-19.722689272465,17.3390385937155,14.7529258720062));
#200686=CARTESIAN_POINT('Ctrl Pts',(-19.733038341259,17.3445518111275,14.7536407560317));
#200687=CARTESIAN_POINT('Ctrl Pts',(-19.7367192565435,17.3465267386462,
14.7538947486429));
#200688=CARTESIAN_POINT('Ctrl Pts',(-19.7435300028927,17.3502069227107,
14.7543641637826));
#200689=CARTESIAN_POINT('Ctrl Pts',(-19.7466613454354,17.3519091730141,
14.7545797666228));
#200690=CARTESIAN_POINT('Ctrl Pts',(-19.7537247522056,17.3557721006553,
14.7550656242847));
#200691=CARTESIAN_POINT('Ctrl Pts',(-19.7576542446953,17.3579373683178,
14.7553355818773));
#200692=CARTESIAN_POINT('Ctrl Pts',(-19.7692143336081,17.364355314756,14.7561288690103));
#200693=CARTESIAN_POINT('Ctrl Pts',(-19.7768256325251,17.368642809837,14.7566500249774));
#200694=CARTESIAN_POINT('Ctrl Pts',(-19.8310962808917,17.3996579064673,
14.7603593128213));
#200695=CARTESIAN_POINT('Ctrl Pts',(-19.8767530756473,17.4281099643231,
14.763444415524));
#200696=CARTESIAN_POINT('Ctrl Pts',(-20.060828040386,17.5528005500119,14.7759434955053));
#200697=CARTESIAN_POINT('Ctrl Pts',(-20.1885934942876,17.6636591893677,
14.784813366385));
#200698=CARTESIAN_POINT('Ctrl Pts',(-20.3564535217846,17.8486734027204,
14.7986577457812));
#200699=CARTESIAN_POINT('Ctrl Pts',(-20.4075288885854,17.9119279615835,
14.8032488516325));
#200700=CARTESIAN_POINT('Ctrl Pts',(-20.4662740171239,17.9939128733161,
14.8091327019448));
#200701=CARTESIAN_POINT('Ctrl Pts',(-20.4774848031288,18.0100274577334,
14.8102859877114));
#200702=CARTESIAN_POINT('Ctrl Pts',(-20.4933402564473,18.0335083378921,
14.8119629356255));
#200703=CARTESIAN_POINT('Ctrl Pts',(-20.4981663235767,18.040751337707,14.8124797351089));
#200704=CARTESIAN_POINT('Ctrl Pts',(-20.5065035623441,18.0534327133854,
14.8133838357586));
#200705=CARTESIAN_POINT('Ctrl Pts',(-20.5100347317634,18.0588578509156,
14.8137703807055));
#200706=CARTESIAN_POINT('Ctrl Pts',(-20.5168105272164,18.0693730644883,
14.8145191879849));
#200707=CARTESIAN_POINT('Ctrl Pts',(-20.5200583773066,18.0744609960414,
14.8148813251217));
#200708=CARTESIAN_POINT('Ctrl Pts',(-20.5277198435358,18.0865770382444,
14.8157432930968));
#200709=CARTESIAN_POINT('Ctrl Pts',(-20.5321139550627,18.093617310158,14.8162438398055));
#200710=CARTESIAN_POINT('Ctrl Pts',(-20.5475456171176,18.1186687666544,
14.8180239379527));
#200711=CARTESIAN_POINT('Ctrl Pts',(-20.5583545759495,18.1368186562927,
14.8193118195202));
#200712=CARTESIAN_POINT('Ctrl Pts',(-20.6657649922623,18.3234757962044,
14.8325424656076));
#200713=CARTESIAN_POINT('Ctrl Pts',(-20.7389930069559,18.5043270849297,
14.8453729429948));
#200714=CARTESIAN_POINT('Ctrl Pts',(-20.8048202111708,18.7649445267654,
14.8631017993519));
#200715=CARTESIAN_POINT('Ctrl Pts',(-20.8192617635743,18.8382443946001,
14.8679935684156));
#200716=CARTESIAN_POINT('Ctrl Pts',(-20.8346727882789,18.946323213088,14.8749434265609));
#200717=CARTESIAN_POINT('Ctrl Pts',(-20.8387085621401,18.980604359859,14.8771093787115));
#200718=CARTESIAN_POINT('Ctrl Pts',(-20.8425871754926,19.0223111894511,
14.8796858371126));
#200719=CARTESIAN_POINT('Ctrl Pts',(-20.843231455777,19.0296549876144,14.8801373014638));
#200720=CARTESIAN_POINT('Ctrl Pts',(-20.8441775334707,19.0411267947871,
14.8808389426141));
#200721=CARTESIAN_POINT('Ctrl Pts',(-20.844505601445,19.0452524945572,14.881090554214));
#200722=CARTESIAN_POINT('Ctrl Pts',(-20.8450939760331,19.052936861581,14.8815578121315));
#200723=CARTESIAN_POINT('Ctrl Pts',(-20.8453573820908,19.0564951886913,
14.8817736246496));
#200724=CARTESIAN_POINT('Ctrl Pts',(-20.8459354331728,19.0645816665432,
14.8822628208867));
#200725=CARTESIAN_POINT('Ctrl Pts',(-20.8462445117251,19.0691101630434,
14.8825358896815));
#200726=CARTESIAN_POINT('Ctrl Pts',(-20.8470081049079,19.0808538765501,
14.8832418226054));
#200727=CARTESIAN_POINT('Ctrl Pts',(-20.8474402335298,19.0880705586828,
14.8836734627217));
#200728=CARTESIAN_POINT('Ctrl Pts',(-20.8499256632875,19.1334751345946,
14.8863763467585));
#200729=CARTESIAN_POINT('Ctrl Pts',(-20.8509809805369,19.1717131791939,
14.8885955874458));
#200730=CARTESIAN_POINT('Ctrl Pts',(-20.8510792905107,19.3720991524381,
14.9000237387125));
#200731=CARTESIAN_POINT('Ctrl Pts',(-20.8325322797143,19.5337232380872,
14.9085853799334));
#200732=CARTESIAN_POINT('Ctrl Pts',(-20.7763041605286,19.7749056753729,
14.9221736593812));
#200733=CARTESIAN_POINT('Ctrl Pts',(-20.7518791101994,19.8568712118476,
14.9269356407186));
#200734=CARTESIAN_POINT('Ctrl Pts',(-20.7225805830531,19.9371103667517,
14.9318515409431));
#200735=CARTESIAN_POINT('Origin',(-18.734,19.211,0.));
#200736=CARTESIAN_POINT('',(-20.7225806064913,19.9371103025619,15.9575278864865));
#200737=CARTESIAN_POINT('',(-20.7225806013824,19.9371103165536,15.7328936098053));
#200738=CARTESIAN_POINT('',(-20.7225806064498,19.9371103026755,0.));
#200739=CARTESIAN_POINT('',(-20.8509995343428,19.2095958660383,15.9109437209775));
#200740=CARTESIAN_POINT('Ctrl Pts',(-20.7225806064913,19.9371103025619,
15.9575278864865));
#200741=CARTESIAN_POINT('Ctrl Pts',(-20.7279986629112,19.9222720033623,
15.9565688725157));
#200742=CARTESIAN_POINT('Ctrl Pts',(-20.7332504094381,19.907373693078,15.9556043363318));
#200743=CARTESIAN_POINT('Ctrl Pts',(-20.7683512912222,19.804127365591,15.9489076438136));
#200744=CARTESIAN_POINT('Ctrl Pts',(-20.7924972887047,19.7139614040123,
15.9429901615334));
#200745=CARTESIAN_POINT('Ctrl Pts',(-20.8375635127319,19.4865404276235,
15.9279396372871));
#200746=CARTESIAN_POINT('Ctrl Pts',(-20.8510859005584,19.3482705920783,
15.918664069312));
#200747=CARTESIAN_POINT('Ctrl Pts',(-20.8509995894496,19.2096815653012,
15.9096291633589));
#200748=CARTESIAN_POINT('Ctrl Pts',(-20.7225806064499,19.9371103026755,
15.1555945416419));
#200749=CARTESIAN_POINT('Ctrl Pts',(-20.6976334977237,20.0054323419264,
15.1599719904749));
#200750=CARTESIAN_POINT('Ctrl Pts',(-20.6691305497313,20.0725514062275,
15.1643494393079));
#200751=CARTESIAN_POINT('Ctrl Pts',(-20.6372132630012,20.1380751186049,
15.1687268881409));
#200752=CARTESIAN_POINT('Ctrl Pts',(-20.605318799863,20.2035519759197,15.1731012067233));
#200753=CARTESIAN_POINT('Ctrl Pts',(-20.570015052495,20.2674353123198,15.1774755253057));
#200754=CARTESIAN_POINT('Ctrl Pts',(-20.5314915547277,20.3293528560712,
15.1818498438881));
#200755=CARTESIAN_POINT('Ctrl Pts',(-20.4929828962544,20.3912465491161,
15.1862224774781));
#200756=CARTESIAN_POINT('Ctrl Pts',(-20.4512572037269,20.4511755433295,
15.1905951110682));
#200757=CARTESIAN_POINT('Ctrl Pts',(-20.4065490386169,20.5087937869406,
15.1949677446582));
#200758=CARTESIAN_POINT('Ctrl Pts',(-20.3618433470109,20.5664088427907,
15.1993401363299));
#200759=CARTESIAN_POINT('Ctrl Pts',(-20.3141558073646,20.6217130217184,
15.2037125280016));
#200760=CARTESIAN_POINT('Ctrl Pts',(-20.2637622094331,20.6743921492854,
15.2080849196733));
#200761=CARTESIAN_POINT('Ctrl Pts',(-20.2133189270891,20.7271232146306,
15.2124616222043));
#200762=CARTESIAN_POINT('Ctrl Pts',(-20.1601645909933,20.7772237090099,
15.2168383247353));
#200763=CARTESIAN_POINT('Ctrl Pts',(-20.1046123748413,20.824415853998,15.2212150272663));
#200764=CARTESIAN_POINT('Ctrl Pts',(-20.0490338494289,20.8716303489571,
15.2255938025824));
#200765=CARTESIAN_POINT('Ctrl Pts',(-19.9910555653989,20.9159334570895,
15.2299725778985));
#200766=CARTESIAN_POINT('Ctrl Pts',(-19.9310221853144,20.9570890263286,
15.2343513532146));
#200767=CARTESIAN_POINT('Ctrl Pts',(-19.8708776387445,20.9983208051694,
15.2387382369042));
#200768=CARTESIAN_POINT('Ctrl Pts',(-19.8086708046917,21.0363931464871,
15.2431251205937));
#200769=CARTESIAN_POINT('Ctrl Pts',(-19.7447732573725,21.0711146260864,
15.2475120042832));
#200770=CARTESIAN_POINT('Ctrl Pts',(-19.6856843426586,21.1032231284133,
15.2515687514834));
#200771=CARTESIAN_POINT('Ctrl Pts',(-19.6251501510711,21.1324665213767,
15.2556254986837));
#200772=CARTESIAN_POINT('Ctrl Pts',(-19.5634785608969,21.1587305555473,
15.2596822458839));
#200773=CARTESIAN_POINT('Ctrl Pts',(-19.496768014386,21.1871405262996,15.2640704548148));
#200774=CARTESIAN_POINT('Ctrl Pts',(-19.4284659821155,21.2121746938962,
15.2684586637457));
#200775=CARTESIAN_POINT('Ctrl Pts',(-19.358947687674,21.2336540454736,15.2728468726766));
#200776=CARTESIAN_POINT('Ctrl Pts',(-19.2895325699079,21.255101518132,15.2772285687779));
#200777=CARTESIAN_POINT('Ctrl Pts',(-19.2189052304801,21.273004507002,15.2816102648792));
#200778=CARTESIAN_POINT('Ctrl Pts',(-19.1474611885822,21.2872318862632,
15.2859919609804));
#200779=CARTESIAN_POINT('Ctrl Pts',(-19.0761010991192,21.3014425472216,
15.2903685082401));
#200780=CARTESIAN_POINT('Ctrl Pts',(-19.0039266843577,21.3119860848152,
15.2947450554997));
#200781=CARTESIAN_POINT('Ctrl Pts',(-18.9313473123127,21.31878154426,15.2991216027594));
#200782=CARTESIAN_POINT('Ctrl Pts',(-18.8588139690506,21.3255726941231,
15.3034953744764));
#200783=CARTESIAN_POINT('Ctrl Pts',(-18.7858766571609,21.3286204372107,
15.3078691461933));
#200784=CARTESIAN_POINT('Ctrl Pts',(-18.7129521899224,21.3278953657871,
15.3122429179103));
#200785=CARTESIAN_POINT('Ctrl Pts',(-18.6400499138441,21.3271705150052,
15.3166153586739));
#200786=CARTESIAN_POINT('Ctrl Pts',(-18.567160956721,21.3226751337981,15.3209877994374));
#200787=CARTESIAN_POINT('Ctrl Pts',(-18.4947027860641,21.3144319203156,
15.325360240201));
#200788=CARTESIAN_POINT('Ctrl Pts',(-18.4222427626439,21.3061884960532,
15.3297327927683));
#200789=CARTESIAN_POINT('Ctrl Pts',(-18.3502140266197,21.294197105762,15.3341053453357));
#200790=CARTESIAN_POINT('Ctrl Pts',(-18.2790278943158,21.2785321963755,
15.338477897903));
#200791=CARTESIAN_POINT('Ctrl Pts',(-18.2077678823586,21.2628510293552,
15.3428549884704));
#200792=CARTESIAN_POINT('Ctrl Pts',(-18.1373526922057,21.2434888351845,
15.3472320790377));
#200793=CARTESIAN_POINT('Ctrl Pts',(-18.0681816040659,21.2205708157803,
15.351609169605));
#200794=CARTESIAN_POINT('Ctrl Pts',(-17.9989727390276,21.197640279995,15.355988650664));
#200795=CARTESIAN_POINT('Ctrl Pts',(-17.9310097785368,21.1711502278389,
15.3603681317229));
#200796=CARTESIAN_POINT('Ctrl Pts',(-17.8646724802105,21.1412742456285,
15.3647476127819));
#200797=CARTESIAN_POINT('Ctrl Pts',(-17.7982175994683,21.1113453084402,
15.3691348564416));
#200798=CARTESIAN_POINT('Ctrl Pts',(-17.7333945644596,21.0780186771212,
15.3735221001013));
#200799=CARTESIAN_POINT('Ctrl Pts',(-17.670558444311,21.0415138780227,15.3779093437611));
#200800=CARTESIAN_POINT('Ctrl Pts',(-17.6278359374847,21.0166941322301,
15.3808922466959));
#200801=CARTESIAN_POINT('Ctrl Pts',(-17.5860313573347,20.9904061565717,
15.3838751496306));
#200802=CARTESIAN_POINT('Ctrl Pts',(-17.5452478505358,20.9627298099719,
15.3868580525654));
#200803=CARTESIAN_POINT('Ctrl Pts',(-17.4852504075478,20.9220145758597,
15.3912462614963));
#200804=CARTESIAN_POINT('Ctrl Pts',(-17.4272300397246,20.8781338958608,
15.3956344704272));
#200805=CARTESIAN_POINT('Ctrl Pts',(-17.3715403699668,20.831306377365,15.4000226793581));
#200806=CARTESIAN_POINT('Ctrl Pts',(-17.3159333529124,20.7845483586708,
15.4044043754594));
#200807=CARTESIAN_POINT('Ctrl Pts',(-17.2626505332034,20.7348524915492,
15.4087860715606));
#200808=CARTESIAN_POINT('Ctrl Pts',(-17.2120162539405,20.6824803691285,
15.4131677676619));
#200809=CARTESIAN_POINT('Ctrl Pts',(-17.1614414739853,20.6301697881196,
15.4175443149215));
#200810=CARTESIAN_POINT('Ctrl Pts',(-17.1135093856058,20.5751895440795,
15.4219208621812));
#200811=CARTESIAN_POINT('Ctrl Pts',(-17.0685096421063,20.5178400314358,
15.4262974094408));
#200812=CARTESIAN_POINT('Ctrl Pts',(-17.0235384367902,20.4605268890196,
15.4306711811578));
#200813=CARTESIAN_POINT('Ctrl Pts',(-16.981496183609,20.4008478378287,15.4350449528747));
#200814=CARTESIAN_POINT('Ctrl Pts',(-16.942633222937,20.3391374340189,15.4394187245917));
#200815=CARTESIAN_POINT('Ctrl Pts',(-16.9037820883944,20.2774458088923,
15.4437911653552));
#200816=CARTESIAN_POINT('Ctrl Pts',(-16.8681085825377,20.2137244662937,
15.4481636061188));
#200817=CARTESIAN_POINT('Ctrl Pts',(-16.835819587061,20.1483367164125,15.4525360468823));
#200818=CARTESIAN_POINT('Ctrl Pts',(-16.8035297659512,20.0829472945593,
15.4569085994497));
#200819=CARTESIAN_POINT('Ctrl Pts',(-16.7746248388306,20.0158918142278,
15.461281152017));
#200820=CARTESIAN_POINT('Ctrl Pts',(-16.7492648453346,19.9475564240677,
15.4656537045843));
#200821=CARTESIAN_POINT('Ctrl Pts',(-16.7238785322808,19.8791501128621,
15.4700307951517));
#200822=CARTESIAN_POINT('Ctrl Pts',(-16.7020446665446,19.8094616929176,
15.474407885719));
#200823=CARTESIAN_POINT('Ctrl Pts',(-16.6838740959316,19.7388946651254,
15.4787849762863));
#200824=CARTESIAN_POINT('Ctrl Pts',(-16.6656936016957,19.6682890980602,
15.4831644573452));
#200825=CARTESIAN_POINT('Ctrl Pts',(-16.6511804819231,19.5968044408508,
15.4875439384042));
#200826=CARTESIAN_POINT('Ctrl Pts',(-16.6403943335876,19.5248539685361,
15.4919234194631));
#200827=CARTESIAN_POINT('Ctrl Pts',(-16.6295890668765,19.4527759644922,
15.4963106631228));
#200828=CARTESIAN_POINT('Ctrl Pts',(-16.6225240103778,19.3802309770744,
15.5006979067825));
#200829=CARTESIAN_POINT('Ctrl Pts',(-16.6192067693547,19.3076363886775,
15.5050851504423));
#200830=CARTESIAN_POINT('Ctrl Pts',(-16.6169513651075,19.2582790637646,
15.5080680533771));
#200831=CARTESIAN_POINT('Ctrl Pts',(-16.6164273661252,19.2088988449423,
15.511050956312));
#200832=CARTESIAN_POINT('Ctrl Pts',(-16.6176234550289,19.1596256883618,
15.5140338592469));
#200833=CARTESIAN_POINT('Ctrl Pts',(-16.6193830456439,19.0871389496106,
15.5184220681777));
#200834=CARTESIAN_POINT('Ctrl Pts',(-16.6248744285954,19.014601222373,15.5228102771086));
#200835=CARTESIAN_POINT('Ctrl Pts',(-16.6341051990331,18.9424281755802,
15.5271984860395));
#200836=CARTESIAN_POINT('Ctrl Pts',(-16.643322269477,18.8703622455554,15.5315801821408));
#200837=CARTESIAN_POINT('Ctrl Pts',(-16.6562676494649,18.7986603960529,
15.5359618782421));
#200838=CARTESIAN_POINT('Ctrl Pts',(-16.6728969413427,18.7277369436906,
15.5403435743433));
#200839=CARTESIAN_POINT('Ctrl Pts',(-16.6895066924791,18.6568968320292,
15.544720121603));
#200840=CARTESIAN_POINT('Ctrl Pts',(-16.7097916465688,18.5868337678032,
15.5490966688626));
#200841=CARTESIAN_POINT('Ctrl Pts',(-16.7336560032764,18.5179539014094,
15.5534732161222));
#200842=CARTESIAN_POINT('Ctrl Pts',(-16.7575052255558,18.4491177176257,
15.5578469878392));
#200843=CARTESIAN_POINT('Ctrl Pts',(-16.7849291889402,18.3814636975243,
15.5622207595562));
#200844=CARTESIAN_POINT('Ctrl Pts',(-16.8157820891437,18.315383426644,15.5665945312732));
#200845=CARTESIAN_POINT('Ctrl Pts',(-16.846625600706,18.249323264212,15.5709669720367));
#200846=CARTESIAN_POINT('Ctrl Pts',(-16.8808957735917,18.1848363370635,
15.5753394128003));
#200847=CARTESIAN_POINT('Ctrl Pts',(-16.9183991025639,18.1222932528779,
15.5797118535638));
#200848=CARTESIAN_POINT('Ctrl Pts',(-16.9559033905003,18.0597485694587,
15.5840844061312));
#200849=CARTESIAN_POINT('Ctrl Pts',(-16.9966407488743,17.9991482403585,
15.5884569586985));
#200850=CARTESIAN_POINT('Ctrl Pts',(-17.0403731142,17.9408358485238,15.5928295112658));
#200851=CARTESIAN_POINT('Ctrl Pts',(-17.084150866624,17.8824629378893,15.5972066018332));
#200852=CARTESIAN_POINT('Ctrl Pts',(-17.1309295419548,17.8263830921187,
15.6015836924005));
#200853=CARTESIAN_POINT('Ctrl Pts',(-17.1804298596133,17.7729079240539,
15.6059607829678));
#200854=CARTESIAN_POINT('Ctrl Pts',(-17.2299572112324,17.7194035512151,
15.6103402640267));
#200855=CARTESIAN_POINT('Ctrl Pts',(-17.2822088187836,17.6685070251037,
15.6147197450857));
#200856=CARTESIAN_POINT('Ctrl Pts',(-17.3368694420728,17.6204921552831,
15.6190992261446));
#200857=CARTESIAN_POINT('Ctrl Pts',(-17.3916269509498,17.5723921794281,
15.6234864698043));
#200858=CARTESIAN_POINT('Ctrl Pts',(-17.4488016237918,17.5271843592174,
15.6278737134641));
#200859=CARTESIAN_POINT('Ctrl Pts',(-17.5080466246416,17.4851010106477,
15.6322609571238));
#200860=CARTESIAN_POINT('Ctrl Pts',(-17.548327516385,17.456488388762,15.6352438600586));
#200861=CARTESIAN_POINT('Ctrl Pts',(-17.5895648351145,17.4293192126642,
15.6382267629935));
#200862=CARTESIAN_POINT('Ctrl Pts',(-17.6316431823901,17.4036543090297,
15.6412096659283));
#200863=CARTESIAN_POINT('Ctrl Pts',(-17.6935454914314,17.3658981494093,
15.6455978748592));
#200864=CARTESIAN_POINT('Ctrl Pts',(-17.7575106221335,17.3312522374744,
15.6499860837901));
#200865=CARTESIAN_POINT('Ctrl Pts',(-17.8231931738166,17.2999479532525,
15.654374292721));
#200866=CARTESIAN_POINT('Ctrl Pts',(-17.8887782417026,17.2686901297788,
15.6587559888223));
#200867=CARTESIAN_POINT('Ctrl Pts',(-17.9560752387296,17.2407642944953,
15.6631376849235));
#200868=CARTESIAN_POINT('Ctrl Pts',(-18.0247117585807,17.2163573777279,
15.6675193810248));
#200869=CARTESIAN_POINT('Ctrl Pts',(-18.0932676250587,17.1919791410302,
15.6718959282845));
#200870=CARTESIAN_POINT('Ctrl Pts',(-18.1631594352667,17.1711117694416,
15.6762724755441));
#200871=CARTESIAN_POINT('Ctrl Pts',(-18.2339938260914,17.1538945515474,
15.6806490228038));
#200872=CARTESIAN_POINT('Ctrl Pts',(-18.3047832947748,17.1366882525626,
15.6850227945208));
#200873=CARTESIAN_POINT('Ctrl Pts',(-18.3765136904429,17.1231276279117,
15.6893965662377));
#200874=CARTESIAN_POINT('Ctrl Pts',(-18.4487768305323,17.1133020370895,
15.6937703379547));
#200875=CARTESIAN_POINT('Ctrl Pts',(-18.5210179807056,17.1034794362276,
15.6981427787183));
#200876=CARTESIAN_POINT('Ctrl Pts',(-18.593791075758,17.0973896776779,15.7025152194818));
#200877=CARTESIAN_POINT('Ctrl Pts',(-18.6666797525663,17.0950706570669,
15.7068876602454));
#200878=CARTESIAN_POINT('Ctrl Pts',(-18.7395702931461,17.0927515771582,
15.7112602128128));
#200879=CARTESIAN_POINT('Ctrl Pts',(-18.8125759391522,17.0942034399582,
15.7156327653801));
#200880=CARTESIAN_POINT('Ctrl Pts',(-18.8852789324501,17.0994120466822,
15.7200053179475));
#200881=CARTESIAN_POINT('Ctrl Pts',(-18.9580573796568,17.1046260590948,
15.7243824085148));
#200882=CARTESIAN_POINT('Ctrl Pts',(-19.0305320648508,17.113604565285,15.7287594990821));
#200883=CARTESIAN_POINT('Ctrl Pts',(-19.1022898016653,17.1262814046041,
15.7331365896495));
#200884=CARTESIAN_POINT('Ctrl Pts',(-19.1740867280431,17.1389651672157,
15.7375160707084));
#200885=CARTESIAN_POINT('Ctrl Pts',(-19.2451654560904,17.155351175915,15.7418955517674));
#200886=CARTESIAN_POINT('Ctrl Pts',(-19.3151251217573,17.1753225715103,
15.7462750328263));
#200887=CARTESIAN_POINT('Ctrl Pts',(-19.3852087904621,17.1953293662702,
15.750662276486));
#200888=CARTESIAN_POINT('Ctrl Pts',(-19.4541689789727,17.2189340823964,
15.7550495201458));
#200889=CARTESIAN_POINT('Ctrl Pts',(-19.5216226105752,17.2459708339796,
15.7594367638055));
#200890=CARTESIAN_POINT('Ctrl Pts',(-19.5674845802476,17.2643532198007,
15.7624196667403));
#200891=CARTESIAN_POINT('Ctrl Pts',(-19.61265053623,17.284321119187,15.765402569675));
#200892=CARTESIAN_POINT('Ctrl Pts',(-19.6570068699278,17.3058104246385,
15.7683854726098));
#200893=CARTESIAN_POINT('Ctrl Pts',(-19.7222603709406,17.3374237771891,
15.7727736815407));
#200894=CARTESIAN_POINT('Ctrl Pts',(-19.7860152120978,17.3724551543895,
15.7771618904716));
#200895=CARTESIAN_POINT('Ctrl Pts',(-19.8478898805759,17.4107393705492,
15.7815500994025));
#200896=CARTESIAN_POINT('Ctrl Pts',(-19.9096727167869,17.4489667665845,
15.7859317955037));
#200897=CARTESIAN_POINT('Ctrl Pts',(-19.9695805130033,17.4904371661198,
15.790313491605));
#200898=CARTESIAN_POINT('Ctrl Pts',(-20.0272545139271,17.5349386162174,
15.7946951877063));
#200899=CARTESIAN_POINT('Ctrl Pts',(-20.0848607433099,17.5793877735696,
15.7990717349659));
#200900=CARTESIAN_POINT('Ctrl Pts',(-20.1402380117453,17.6268606128758,
15.8034482822256));
#200901=CARTESIAN_POINT('Ctrl Pts',(-20.1930562795834,17.6771017722782,
15.8078248294852));
#200902=CARTESIAN_POINT('Ctrl Pts',(-20.2458410508437,17.7273110694674,
15.8121986012022));
#200903=CARTESIAN_POINT('Ctrl Pts',(-20.2960696928603,17.780284871717,15.8165723729192));
#200904=CARTESIAN_POINT('Ctrl Pts',(-20.3434461269599,17.8357283306874,
15.8209461446361));
#200905=CARTESIAN_POINT('Ctrl Pts',(-20.3908081442515,17.8911549180271,
15.8253185853997));
#200906=CARTESIAN_POINT('Ctrl Pts',(-20.4353193635675,17.9490493035726,
15.8296910261632));
#200907=CARTESIAN_POINT('Ctrl Pts',(-20.4767225512217,18.009081904012,15.8340634669268));
#200908=CARTESIAN_POINT('Ctrl Pts',(-20.5181267975599,18.0691160394917,
15.8384360194941));
#200909=CARTESIAN_POINT('Ctrl Pts',(-20.5564225822289,18.1312881001857,
15.8428085720615));
#200910=CARTESIAN_POINT('Ctrl Pts',(-20.5913957196047,18.1952391320817,
15.8471811246288));
#200911=CARTESIAN_POINT('Ctrl Pts',(-20.6264051534217,18.2592565347709,
15.8515582151961));
#200912=CARTESIAN_POINT('Ctrl Pts',(-20.6580848230995,18.3250561707613,
15.8559353057635));
#200913=CARTESIAN_POINT('Ctrl Pts',(-20.68626670933,18.3922548042024,15.8603123963308));
#200914=CARTESIAN_POINT('Ctrl Pts',(-20.7144639867346,18.4594901373112,
15.8646918773897));
#200915=CARTESIAN_POINT('Ctrl Pts',(-20.7391595139379,18.52812553487,15.8690713584487));
#200916=CARTESIAN_POINT('Ctrl Pts',(-20.7602345709197,18.597760679987,15.8734508395076));
#200917=CARTESIAN_POINT('Ctrl Pts',(-20.7813469832985,18.6675192529313,
15.8778380831673));
#200918=CARTESIAN_POINT('Ctrl Pts',(-20.7988259946711,18.7382806434225,
15.8822253268271));
#200919=CARTESIAN_POINT('Ctrl Pts',(-20.8126037366755,18.809632953671,15.8866125704868));
#200920=CARTESIAN_POINT('Ctrl Pts',(-20.8219712736183,18.8581456491475,
15.8895954734216));
#200921=CARTESIAN_POINT('Ctrl Pts',(-20.8296289055563,18.9069313156785,
15.8925783763564));
#200922=CARTESIAN_POINT('Ctrl Pts',(-20.8355690425742,18.9558597262409,
15.8955612792912));
#200923=CARTESIAN_POINT('Ctrl Pts',(-20.8457798800574,19.0399655384573,
15.9006887598533));
#200924=CARTESIAN_POINT('Ctrl Pts',(-20.850943223371,19.1246963446804,15.9058162404154));
#200925=CARTESIAN_POINT('Ctrl Pts',(-20.8509995343428,19.2095958660383,
15.9109437209775));
#200926=CARTESIAN_POINT('',(-20.8509995791044,19.2096650574301,15.6876314267646));
#200927=CARTESIAN_POINT('Ctrl Pts',(-20.7225805830531,19.9371103667517,
14.9318515409431));
#200928=CARTESIAN_POINT('Ctrl Pts',(-20.714010105929,19.9605821214281,14.9332895521512));
#200929=CARTESIAN_POINT('Ctrl Pts',(-20.7050225936995,19.983906167217,14.9347403770111));
#200930=CARTESIAN_POINT('Ctrl Pts',(-20.6902873330294,20.0202157299443,
14.9370363167659));
#200931=CARTESIAN_POINT('Ctrl Pts',(-20.6848211921425,20.0333058364495,
14.9378717579225));
#200932=CARTESIAN_POINT('Ctrl Pts',(-20.6758998546064,20.0540806160084,
14.9392104414492));
#200933=CARTESIAN_POINT('Ctrl Pts',(-20.6725295631085,20.0618014458346,
14.9397107969794));
#200934=CARTESIAN_POINT('Ctrl Pts',(-20.6664968926029,20.0753994372095,
14.9405971440495));
#200935=CARTESIAN_POINT('Ctrl Pts',(-20.6638535463858,20.0812849619796,
14.9409824795058));
#200936=CARTESIAN_POINT('Ctrl Pts',(-20.6583232643003,20.0934492798618,
14.9417824755278));
#200937=CARTESIAN_POINT('Ctrl Pts',(-20.6554324089197,20.0997261970076,
14.9421972676894));
#200938=CARTESIAN_POINT('Ctrl Pts',(-20.6479172869637,20.115835720989,14.9432669949786));
#200939=CARTESIAN_POINT('Ctrl Pts',(-20.6432480022968,20.1256469931882,
14.9439234830348));
#200940=CARTESIAN_POINT('Ctrl Pts',(-20.623305148899,20.1667334708388,14.9466939815646));
#200941=CARTESIAN_POINT('Ctrl Pts',(-20.6073377252505,20.1976640533919,
14.9488320641504));
#200942=CARTESIAN_POINT('Ctrl Pts',(-20.563605053731,20.2774870174198,14.9544919100229));
#200943=CARTESIAN_POINT('Ctrl Pts',(-20.5346432922634,20.3256892288278,
14.9580538990754));
#200944=CARTESIAN_POINT('Ctrl Pts',(-20.4347644591281,20.4778530934194,
14.9697637599371));
#200945=CARTESIAN_POINT('Ctrl Pts',(-20.3564950966972,20.5766579015057,
14.9781232382993));
#200946=CARTESIAN_POINT('Ctrl Pts',(-20.2011016309508,20.7404781432947,
14.9930007275872));
#200947=CARTESIAN_POINT('Ctrl Pts',(-20.1272124158796,20.8080768618124,
14.9995202713344));
#200948=CARTESIAN_POINT('Ctrl Pts',(-20.0412146256351,20.8762245784271,
15.0062996210402));
#200949=CARTESIAN_POINT('Ctrl Pts',(-20.0335754802509,20.8821931526325,
15.0068952528871));
#200950=CARTESIAN_POINT('Ctrl Pts',(-20.0222359707755,20.8909281001533,
15.0077694112859));
#200951=CARTESIAN_POINT('Ctrl Pts',(-20.0185672440217,20.8937350755852,
15.0080507032578));
#200952=CARTESIAN_POINT('Ctrl Pts',(-20.0120424371034,20.898693489401,15.0085482293783));
#200953=CARTESIAN_POINT('Ctrl Pts',(-20.0091900673703,20.9008497205265,
15.0087647983666));
#200954=CARTESIAN_POINT('Ctrl Pts',(-20.0030671636054,20.9054539600138,
15.0092276907257));
#200955=CARTESIAN_POINT('Ctrl Pts',(-19.9997950120221,20.9078997249504,
15.0094738578791));
#200956=CARTESIAN_POINT('Ctrl Pts',(-19.9907938675744,20.9145870938001,
15.0101477763432));
#200957=CARTESIAN_POINT('Ctrl Pts',(-19.98505043846,20.9188093030122,15.0105741955297));
#200958=CARTESIAN_POINT('Ctrl Pts',(-19.9542778836496,20.9411928116132,
15.0128404277134));
#200959=CARTESIAN_POINT('Ctrl Pts',(-19.9288730008383,20.9588340932724,
15.0146465059246));
#200960=CARTESIAN_POINT('Ctrl Pts',(-19.8508165748393,21.0105391382306,
15.0200319810482));
#200961=CARTESIAN_POINT('Ctrl Pts',(-19.7970274229189,21.0428281084345,
15.0235246284933));
#200962=CARTESIAN_POINT('Ctrl Pts',(-19.6236648553288,21.1366833539519,
15.0343590003749));
#200963=CARTESIAN_POINT('Ctrl Pts',(-19.4996236594439,21.1892772928256,
15.0415277489855));
#200964=CARTESIAN_POINT('Ctrl Pts',(-19.3325234617007,21.2420399883082,
15.0512527937098));
#200965=CARTESIAN_POINT('Ctrl Pts',(-19.2932699553191,21.253197502654,15.0535400264754));
#200966=CARTESIAN_POINT('Ctrl Pts',(-19.2066104697927,21.275143885851,15.0586207672228));
#200967=CARTESIAN_POINT('Ctrl Pts',(-19.1591071467,21.28544788283,15.0614260732125));
#200968=CARTESIAN_POINT('Ctrl Pts',(-19.0988926621608,21.2963539699619,
15.0650250902967));
#200969=CARTESIAN_POINT('Ctrl Pts',(-19.0864718539404,21.2984892614768,
15.065769734783));
#200970=CARTESIAN_POINT('Ctrl Pts',(-19.0667599268285,21.3016970436467,
15.0669553411896));
#200971=CARTESIAN_POINT('Ctrl Pts',(-19.0594808768274,21.3028426073513,
15.0673939803643));
#200972=CARTESIAN_POINT('Ctrl Pts',(-19.0459068920162,21.3049062917516,
15.0682135567924));
#200973=CARTESIAN_POINT('Ctrl Pts',(-19.0396134959049,21.3058340883414,
15.0685941824011));
#200974=CARTESIAN_POINT('Ctrl Pts',(-19.0256263735261,21.3078317519062,
15.0694415868103));
#200975=CARTESIAN_POINT('Ctrl Pts',(-19.0179307757519,21.3088876637252,
15.0699088019049));
#200976=CARTESIAN_POINT('Ctrl Pts',(-18.9955533400665,21.3118326859083,
15.0712703125729));
#200977=CARTESIAN_POINT('Ctrl Pts',(-18.9808575074943,21.3136101582108,
15.0721681164671));
#200978=CARTESIAN_POINT('Ctrl Pts',(-18.8639363523084,21.3265092061133,
15.0793414941781));
#200979=CARTESIAN_POINT('Ctrl Pts',(-18.7610577403731,21.3303218489948,
15.0858478890049));
#200980=CARTESIAN_POINT('Ctrl Pts',(-18.5026289384204,21.3210776411383,
15.1026341270099));
#200981=CARTESIAN_POINT('Ctrl Pts',(-18.348038087996,21.2983403900046,15.1131044691046));
#200982=CARTESIAN_POINT('Ctrl Pts',(-18.1465315252016,21.2455341593658,
15.12656034383));
#200983=CARTESIAN_POINT('Ctrl Pts',(-18.0962253255101,21.2303298180707,
15.1298980694134));
#200984=CARTESIAN_POINT('Ctrl Pts',(-18.0383148344007,21.2104465849901,
15.1336749021378));
#200985=CARTESIAN_POINT('Ctrl Pts',(-18.0301141804618,21.2075743799977,
15.1342081726498));
#200986=CARTESIAN_POINT('Ctrl Pts',(-18.0177156618509,21.2031460251375,
15.1350117965231));
#200987=CARTESIAN_POINT('Ctrl Pts',(-18.0135047821559,21.2016269566306,
15.1352842686453));
#200988=CARTESIAN_POINT('Ctrl Pts',(-18.0059505305127,21.1988746611253,
15.1357722098489));
#200989=CARTESIAN_POINT('Ctrl Pts',(-18.0026054413987,21.19764634462,15.1359879647496));
#200990=CARTESIAN_POINT('Ctrl Pts',(-17.9953385663123,21.1949571064528,
15.1364559928437));
#200991=CARTESIAN_POINT('Ctrl Pts',(-17.9914180185891,21.1934930051433,
15.1367080731634));
#200992=CARTESIAN_POINT('Ctrl Pts',(-17.9804047479368,21.1893429218316,
15.1374150671293));
#200993=CARTESIAN_POINT('Ctrl Pts',(-17.9733219974898,21.1866304059046,
15.1378684228144));
#200994=CARTESIAN_POINT('Ctrl Pts',(-17.9308014683579,21.1700835429774,
15.1405830127833));
#200995=CARTESIAN_POINT('Ctrl Pts',(-17.8957248758046,21.1553331585878,
15.1427927144636));
#200996=CARTESIAN_POINT('Ctrl Pts',(-17.7810017022344,21.1034074863403,
15.1499808166621));
#200997=CARTESIAN_POINT('Ctrl Pts',(-17.7032682728916,21.0622175463789,
15.1547898674582));
#200998=CARTESIAN_POINT('Ctrl Pts',(-17.4797360629945,20.9253125742143,
15.1690495330684));
#200999=CARTESIAN_POINT('Ctrl Pts',(-17.342976215466,20.8163322713576,15.1784224949014));
#201000=CARTESIAN_POINT('Ctrl Pts',(-17.2049682354818,20.6753373026759,
15.18988602955));
#201001=CARTESIAN_POINT('Ctrl Pts',(-17.1890924266148,20.6585781156718,
15.191238337592));
#201002=CARTESIAN_POINT('Ctrl Pts',(-17.1670331401775,20.6345151145433,
15.1931674499305));
#201003=CARTESIAN_POINT('Ctrl Pts',(-17.1606199011764,20.6274234822899,
15.1937344778527));
#201004=CARTESIAN_POINT('Ctrl Pts',(-17.1502810146679,20.6158340869886,
15.1946588285409));
#201005=CARTESIAN_POINT('Ctrl Pts',(-17.1463259194027,20.6113626848578,
15.1950149097325));
#201006=CARTESIAN_POINT('Ctrl Pts',(-17.1380892785461,20.6019710668898,
15.1957616999097));
#201007=CARTESIAN_POINT('Ctrl Pts',(-17.1338114588514,20.5970476799429,
15.1961525583538));
#201008=CARTESIAN_POINT('Ctrl Pts',(-17.1236935950338,20.5852936532444,
15.1970842349144));
#201009=CARTESIAN_POINT('Ctrl Pts',(-17.1178741955492,20.5784454810042,
15.1976258959164));
#201010=CARTESIAN_POINT('Ctrl Pts',(-17.0984378565033,20.5552757479446,
15.1994548008658));
#201011=CARTESIAN_POINT('Ctrl Pts',(-17.0850235146524,20.5387866209648,
15.2007502338299));
#201012=CARTESIAN_POINT('Ctrl Pts',(-17.0134819528044,20.4480901092409,
15.2078449111842));
#201013=CARTESIAN_POINT('Ctrl Pts',(-16.9601195976993,20.3702749881867,
15.2138292057618));
#201014=CARTESIAN_POINT('Ctrl Pts',(-16.8276109236315,20.1463642895075,
15.2307279303986));
#201015=CARTESIAN_POINT('Ctrl Pts',(-16.7601869832664,19.994124729502,15.2419104978843));
#201016=CARTESIAN_POINT('Ctrl Pts',(-16.698840707698,19.7954482201582,15.2552394432181));
#201017=CARTESIAN_POINT('Ctrl Pts',(-16.6876452440825,19.7549538801397,
15.2578905603053));
#201018=CARTESIAN_POINT('Ctrl Pts',(-16.6758936236268,19.7069258622046,
15.2609373606017));
#201019=CARTESIAN_POINT('Ctrl Pts',(-16.6741639831534,19.6996920346282,
15.2613936779627));
#201020=CARTESIAN_POINT('Ctrl Pts',(-16.6714259028112,19.6879677884871,
15.2621289131939));
#201021=CARTESIAN_POINT('Ctrl Pts',(-16.6703939360781,19.68348300659,15.2624091311566));
#201022=CARTESIAN_POINT('Ctrl Pts',(-16.6685865355233,19.6755094113196,
15.2629054721059));
#201023=CARTESIAN_POINT('Ctrl Pts',(-16.6678053051221,19.6720219690793,
15.2631219239834));
#201024=CARTESIAN_POINT('Ctrl Pts',(-16.6661476064176,19.6645330829273,
15.263585359257));
#201025=CARTESIAN_POINT('Ctrl Pts',(-16.6652739215586,19.6605310801099,
15.2638321822816));
#201026=CARTESIAN_POINT('Ctrl Pts',(-16.662901128459,19.649508830755,15.2645097490968));
#201027=CARTESIAN_POINT('Ctrl Pts',(-16.6614260867731,19.6424833808142,
15.2649391366288));
#201028=CARTESIAN_POINT('Ctrl Pts',(-16.6536456822026,19.6044656053513,
15.2672499832116));
#201029=CARTESIAN_POINT('Ctrl Pts',(-16.6479993385541,19.5733406581219,
15.2690961143121));
#201030=CARTESIAN_POINT('Ctrl Pts',(-16.6174875116691,19.3806531926838,
15.2803086994677));
#201031=CARTESIAN_POINT('Ctrl Pts',(-16.6107039351241,19.2167727713442,
15.2889469574216));
#201032=CARTESIAN_POINT('Ctrl Pts',(-16.6315476406607,18.9369726719341,
15.3043057823969));
#201033=CARTESIAN_POINT('Ctrl Pts',(-16.6499146963895,18.8211537964578,
15.3108410712198));
#201034=CARTESIAN_POINT('Ctrl Pts',(-16.6811576339985,18.6935722119373,
15.3185360417941));
#201035=CARTESIAN_POINT('Ctrl Pts',(-16.684697829224,18.6797242773819,15.3193777412692));
#201036=CARTESIAN_POINT('Ctrl Pts',(-16.6905550861813,18.6577429327706,
15.3207245703816));
#201037=CARTESIAN_POINT('Ctrl Pts',(-16.6927811637243,18.6495855741792,
15.3212267570963));
#201038=CARTESIAN_POINT('Ctrl Pts',(-16.6967932162291,18.6352229486684,
15.3221152349032));
#201039=CARTESIAN_POINT('Ctrl Pts',(-16.6985588333928,18.6290120718283,
15.3225008596541));
#201040=CARTESIAN_POINT('Ctrl Pts',(-16.702269315911,18.6161832156927,15.3233003618797));
#201041=CARTESIAN_POINT('Ctrl Pts',(-16.7042181655002,18.6095664773681,
15.3237143655532));
#201042=CARTESIAN_POINT('Ctrl Pts',(-16.7093033171964,18.5926076182379,
15.3247797495212));
#201043=CARTESIAN_POINT('Ctrl Pts',(-16.7124865111845,18.5822798691535,
15.3254326586177));
#201044=CARTESIAN_POINT('Ctrl Pts',(-16.7260999394291,18.5392840385424,
15.328168264609));
#201045=CARTESIAN_POINT('Ctrl Pts',(-16.73724361527,18.5068489436963,15.3302742831441));
#201046=CARTESIAN_POINT('Ctrl Pts',(-16.7683257266418,18.4230614422431,
15.3358290666946));
#201047=CARTESIAN_POINT('Ctrl Pts',(-16.7894882924941,18.3721937533858,
15.3393162224231));
#201048=CARTESIAN_POINT('Ctrl Pts',(-16.8585267494172,18.2229456383316,
15.3498858931871));
#201049=CARTESIAN_POINT('Ctrl Pts',(-16.9120655957312,18.12739356991,15.3571167986195));
#201050=CARTESIAN_POINT('Ctrl Pts',(-16.9983209755564,17.9980560792936,
15.3673861884883));
#201051=CARTESIAN_POINT('Ctrl Pts',(-17.0251482361426,17.9605438923364,
15.3704260515794));
#201052=CARTESIAN_POINT('Ctrl Pts',(-17.0664504489016,17.9066058976365,
15.3748626788361));
#201053=CARTESIAN_POINT('Ctrl Pts',(-17.0799889566774,17.88948080074,15.3762814686363));
#201054=CARTESIAN_POINT('Ctrl Pts',(-17.1264813801059,17.8325056876575,
15.3810289926653));
#201055=CARTESIAN_POINT('Ctrl Pts',(-17.1606324027548,17.7936510519272,
15.3843127762957));
#201056=CARTESIAN_POINT('Ctrl Pts',(-17.2021191584776,17.7498001868932,
15.3880361031336));
#201057=CARTESIAN_POINT('Ctrl Pts',(-17.208101832978,17.7435537160834,15.3885669035559));
#201058=CARTESIAN_POINT('Ctrl Pts',(-17.2172328403705,17.7341363146082,
15.3893675502721));
#201059=CARTESIAN_POINT('Ctrl Pts',(-17.2203531224792,17.7309384834479,
15.3896394923708));
#201060=CARTESIAN_POINT('Ctrl Pts',(-17.2259798705567,17.725208297314,15.3901268694201));
#201061=CARTESIAN_POINT('Ctrl Pts',(-17.2284826140154,17.7226723829591,
15.3903425872283));
#201062=CARTESIAN_POINT('Ctrl Pts',(-17.2339437067379,17.7171667807001,
15.3908109780318));
#201063=CARTESIAN_POINT('Ctrl Pts',(-17.2369044677119,17.714199566428,15.3910634557459));
#201064=CARTESIAN_POINT('Ctrl Pts',(-17.2452688903829,17.7058665595312,
15.3917726891239));
#201065=CARTESIAN_POINT('Ctrl Pts',(-17.2506927824817,17.7005210386077,
15.3922278709585));
#201066=CARTESIAN_POINT('Ctrl Pts',(-17.2837781783381,17.6682637774233,
15.3949768593752));
#201067=CARTESIAN_POINT('Ctrl Pts',(-17.3121443818488,17.6420814527203,
15.3972176029302));
#201068=CARTESIAN_POINT('Ctrl Pts',(-17.4090615902289,17.5574148150299,
15.4045593427285));
#201069=CARTESIAN_POINT('Ctrl Pts',(-17.4806308105671,17.5025287513374,
15.4094826296095));
#201070=CARTESIAN_POINT('Ctrl Pts',(-17.6976413966474,17.3571031522537,
15.4236874288174));
#201071=CARTESIAN_POINT('Ctrl Pts',(-17.8508055445381,17.2794375843642,
15.4329079072757));
#201072=CARTESIAN_POINT('Ctrl Pts',(-18.0335302010128,17.2131077798765,
15.4442003775982));
#201073=CARTESIAN_POINT('Ctrl Pts',(-18.0555481095039,17.2055239389201,
15.4455643641494));
#201074=CARTESIAN_POINT('Ctrl Pts',(-18.0868081545907,17.1953304395445,
15.4475073060515));
#201075=CARTESIAN_POINT('Ctrl Pts',(-18.0959502928806,17.1924179163705,
15.4480762913423));
#201076=CARTESIAN_POINT('Ctrl Pts',(-18.1108177556226,17.1877924971797,
15.4490029642072));
#201077=CARTESIAN_POINT('Ctrl Pts',(-18.116531154563,17.1860414984591,15.4493593976203));
#201078=CARTESIAN_POINT('Ctrl Pts',(-18.1284909091304,17.1824314866439,
15.4501062222404));
#201079=CARTESIAN_POINT('Ctrl Pts',(-18.1347385804405,17.1805770829557,
15.450496759796));
#201080=CARTESIAN_POINT('Ctrl Pts',(-18.1495942448935,17.1762422348056,
15.4514263774424));
#201081=CARTESIAN_POINT('Ctrl Pts',(-18.1582095642348,17.1737875368911,
15.4519662905354));
#201082=CARTESIAN_POINT('Ctrl Pts',(-18.1871568417086,17.1657380981198,
15.4537831933396));
#201083=CARTESIAN_POINT('Ctrl Pts',(-18.207556255928,17.1603926214685,15.4550682264372));
#201084=CARTESIAN_POINT('Ctrl Pts',(-18.3182055908662,17.133157853292,15.4620656072602));
#201085=CARTESIAN_POINT('Ctrl Pts',(-18.4097304674114,17.1169230415623,
15.4679573707977));
#201086=CARTESIAN_POINT('Ctrl Pts',(-18.6540655821775,17.0899861597897,
15.4839117914373));
#201087=CARTESIAN_POINT('Ctrl Pts',(-18.807473373259,17.089753396508,15.4941848570405));
#201088=CARTESIAN_POINT('Ctrl Pts',(-18.9638676732419,17.106512269825,15.5043643049148));
#201089=CARTESIAN_POINT('Ctrl Pts',(-18.9681721682654,17.1069868941303,
15.5046442125475));
#201090=CARTESIAN_POINT('Ctrl Pts',(-19.0235796242697,17.1132683989512,
15.5082435411218));
#201091=CARTESIAN_POINT('Ctrl Pts',(-19.074460688714,17.1209230423382,15.5115092579736));
#201092=CARTESIAN_POINT('Ctrl Pts',(-19.1327595734839,17.1318795430207,
15.5151679587037));
#201093=CARTESIAN_POINT('Ctrl Pts',(-19.1404945549523,17.1333779811331,
15.5156516791356));
#201094=CARTESIAN_POINT('Ctrl Pts',(-19.1528133496738,17.1358358363388,
15.516419132414));
#201095=CARTESIAN_POINT('Ctrl Pts',(-19.1574025703433,17.136767324429,15.5167043894806));
#201096=CARTESIAN_POINT('Ctrl Pts',(-19.1655075977397,17.1384404463791,
15.5172069892166));
#201097=CARTESIAN_POINT('Ctrl Pts',(-19.1690246550353,17.1391758133299,
15.5174246858046));
#201098=CARTESIAN_POINT('Ctrl Pts',(-19.1764559265738,17.1407493446699,
15.5178838029626));
#201099=CARTESIAN_POINT('Ctrl Pts',(-19.1803696336362,17.1415896555699,
15.5181250990765));
#201100=CARTESIAN_POINT('Ctrl Pts',(-19.1908835030481,17.1438782997365,
15.5187720356665));
#201101=CARTESIAN_POINT('Ctrl Pts',(-19.1974792178293,17.1453471548894,
15.5191765166686));
#201102=CARTESIAN_POINT('Ctrl Pts',(-19.2296418826757,17.1526715345459,
15.5211427177802));
#201103=CARTESIAN_POINT('Ctrl Pts',(-19.255106768312,17.1589705591677,15.5226804089078));
#201104=CARTESIAN_POINT('Ctrl Pts',(-19.3276967081876,17.1783650379128,
15.5270260421735));
#201105=CARTESIAN_POINT('Ctrl Pts',(-19.374495716819,17.1926227964102,15.5297818683856));
#201106=CARTESIAN_POINT('Ctrl Pts',(-19.5505236671568,17.2529916510873,
15.5401147113778));
#201107=CARTESIAN_POINT('Ctrl Pts',(-19.6756557403249,17.3100016040193,
15.5474115978392));
#201108=CARTESIAN_POINT('Ctrl Pts',(-19.8818239945251,17.4293174094384,
15.5605317142495));
#201109=CARTESIAN_POINT('Ctrl Pts',(-19.965508211468,17.4861010100236,15.5662145003484));
#201110=CARTESIAN_POINT('Ctrl Pts',(-20.055831543385,17.5573231187063,15.5729553902449));
#201111=CARTESIAN_POINT('Ctrl Pts',(-20.0667621388542,17.566119784323,15.5737818339964));
#201112=CARTESIAN_POINT('Ctrl Pts',(-20.0840796475392,17.5803424155024,
15.5751087993495));
#201113=CARTESIAN_POINT('Ctrl Pts',(-20.0905232966979,17.5856988725117,
15.5756065138542));
#201114=CARTESIAN_POINT('Ctrl Pts',(-20.1018663217547,17.5952425120317,
15.5764897966285));
#201115=CARTESIAN_POINT('Ctrl Pts',(-20.1067787224529,17.5994141003721,
15.5768747235754));
#201116=CARTESIAN_POINT('Ctrl Pts',(-20.1118623973303,17.6037712431229,
15.5772755922498));
#201117=CARTESIAN_POINT('Ctrl Pts',(-20.1120528087966,17.6039345006879,
15.5772906106666));
#201118=CARTESIAN_POINT('Ctrl Pts',(-20.1123584314734,17.6041966338607,
15.5773147221196));
#201119=CARTESIAN_POINT('Ctrl Pts',(-20.1124736596305,17.6042954867946,
15.5773238141534));
#201120=CARTESIAN_POINT('Ctrl Pts',(-20.1127006051659,17.6044902231886,
15.5773417238694));
#201121=CARTESIAN_POINT('Ctrl Pts',(-20.1128123241027,17.6045861067036,
15.577350541594));
#201122=CARTESIAN_POINT('Ctrl Pts',(-20.1130253202141,17.6047689506089,
15.577367355325));
#201123=CARTESIAN_POINT('Ctrl Pts',(-20.1131266017917,17.6048559111805,
15.5773753514527));
#201124=CARTESIAN_POINT('Ctrl Pts',(-20.113319853976,17.6050218696612,15.5773906106093));
#201125=CARTESIAN_POINT('Ctrl Pts',(-20.1134118267743,17.6051008665382,
15.577397873628));
#201126=CARTESIAN_POINT('Ctrl Pts',(-20.1135874428174,17.6052517321257,
15.5774117435363));
#201127=CARTESIAN_POINT('Ctrl Pts',(-20.1136710883106,17.6053236003969,
15.5774183504544));
#201128=CARTESIAN_POINT('Ctrl Pts',(-20.113830917418,17.6054609473987,15.5774309762642));
#201129=CARTESIAN_POINT('Ctrl Pts',(-20.1139070984954,17.6055264220136,
15.5774369948338));
#201130=CARTESIAN_POINT('Ctrl Pts',(-20.1140527497211,17.6056516214914,
15.5774485029204));
#201131=CARTESIAN_POINT('Ctrl Pts',(-20.1141222206594,17.6057113454474,
15.5774539924001));
#201132=CARTESIAN_POINT('Ctrl Pts',(-20.1142551174675,17.6058256114358,
15.5774644946323));
#201133=CARTESIAN_POINT('Ctrl Pts',(-20.1143185439812,17.6058801527177,
15.5774695073536));
#201134=CARTESIAN_POINT('Ctrl Pts',(-20.1144399406737,17.6059845558252,
15.5774791023592));
#201135=CARTESIAN_POINT('Ctrl Pts',(-20.1144979113635,17.6060344170146,
15.5774836846161));
#201136=CARTESIAN_POINT('Ctrl Pts',(-20.1146089183281,17.6061299057158,
15.5774924597509));
#201137=CARTESIAN_POINT('Ctrl Pts',(-20.1146619551019,17.6061755327672,
15.5774966526122));
#201138=CARTESIAN_POINT('Ctrl Pts',(-20.1147635586412,17.6062629501274,
15.5775046855067));
#201139=CARTESIAN_POINT('Ctrl Pts',(-20.1148121257641,17.6063047400058,
15.5775085255217));
#201140=CARTESIAN_POINT('Ctrl Pts',(-20.1149052038986,17.606384837011,15.5775158853136));
#201141=CARTESIAN_POINT('Ctrl Pts',(-20.1149497152654,17.6064231438297,
15.5775194050799));
#201142=CARTESIAN_POINT('Ctrl Pts',(-20.1150350525118,17.6064965918904,
15.5775261535694));
#201143=CARTESIAN_POINT('Ctrl Pts',(-20.1150758784476,17.6065317326691,
15.5775293822648));
#201144=CARTESIAN_POINT('Ctrl Pts',(-20.1151740831899,17.6066162685763,
15.5775371491405));
#201145=CARTESIAN_POINT('Ctrl Pts',(-20.1152314607782,17.6066656653034,
15.5775416873913));
#201146=CARTESIAN_POINT('Ctrl Pts',(-20.1153451301596,17.6067635346051,
15.5775506786807));
#201147=CARTESIAN_POINT('Ctrl Pts',(-20.1154014279276,17.6068120121257,
15.5775551321793));
#201148=CARTESIAN_POINT('Ctrl Pts',(-20.1155129909783,17.6069080883325,
15.5775639581452));
#201149=CARTESIAN_POINT('Ctrl Pts',(-20.1155682502987,17.6069556816954,
15.5775683301287));
#201150=CARTESIAN_POINT('Ctrl Pts',(-20.115677762143,17.6070500111515,15.5775769950612));
#201151=CARTESIAN_POINT('Ctrl Pts',(-20.1157320148557,17.6070967472287,
15.5775812880138));
#201152=CARTESIAN_POINT('Ctrl Pts',(-20.1158395463032,17.6071893898534,
15.5775897974481));
#201153=CARTESIAN_POINT('Ctrl Pts',(-20.1158928250621,17.607235296252,15.5775940139209));
#201154=CARTESIAN_POINT('Ctrl Pts',(-20.1159984397161,17.6073263058229,
15.5776023728261));
#201155=CARTESIAN_POINT('Ctrl Pts',(-20.1160507757332,17.6073714089389,
15.5776065152579));
#201156=CARTESIAN_POINT('Ctrl Pts',(-20.1161545350013,17.6074608374023,
15.5776147284331));
#201157=CARTESIAN_POINT('Ctrl Pts',(-20.1162059583187,17.6075051626533,
15.577618799172));
#201158=CARTESIAN_POINT('Ctrl Pts',(-20.1163079210326,17.6075930597933,
15.5776268712162));
#201159=CARTESIAN_POINT('Ctrl Pts',(-20.1163584605015,17.6076366315982,
15.5776308725179));
#201160=CARTESIAN_POINT('Ctrl Pts',(-20.1220936267825,17.6125815873703,
15.5780849658487));
#201161=CARTESIAN_POINT('Ctrl Pts',(-20.1277520904035,17.6175131168468,
15.578536307123));
#201162=CARTESIAN_POINT('Ctrl Pts',(-20.1436480051138,17.6315163496052,
15.5798137194793));
#201163=CARTESIAN_POINT('Ctrl Pts',(-20.1538237905432,17.6406572061432,
15.5806426799479));
#201164=CARTESIAN_POINT('Ctrl Pts',(-20.1765018938493,17.6614294584153,
15.5825158773276));
#201165=CARTESIAN_POINT('Ctrl Pts',(-20.1889533862617,17.6731147005853,
15.5835623715763));
#201166=CARTESIAN_POINT('Ctrl Pts',(-20.2277118941701,17.7103800883509,
15.5868777327349));
#201167=CARTESIAN_POINT('Ctrl Pts',(-20.2534949126171,17.7364932023779,
15.5891691783209));
#201168=CARTESIAN_POINT('Ctrl Pts',(-20.3343603276755,17.8227681462414,
15.596640886085));
#201169=CARTESIAN_POINT('Ctrl Pts',(-20.3866450157547,17.8854423435923,
15.6019238840865));
#201170=CARTESIAN_POINT('Ctrl Pts',(-20.4659357021339,17.992493632953,15.610667890851));
#201171=CARTESIAN_POINT('Ctrl Pts',(-20.4951598696652,18.0351280754042,
15.6140835312532));
#201172=CARTESIAN_POINT('Ctrl Pts',(-20.5894724938202,18.1841336649876,
15.6257362678925));
#201173=CARTESIAN_POINT('Ctrl Pts',(-20.6467221531686,18.295175949557,15.6339580316536));
#201174=CARTESIAN_POINT('Ctrl Pts',(-20.6974296624091,18.4193424496933,
15.6422406085192));
#201175=CARTESIAN_POINT('Ctrl Pts',(-20.7009325326663,18.4280861250016,
15.6428191325325));
#201176=CARTESIAN_POINT('Ctrl Pts',(-20.7060465160105,18.441102355905,15.6436730383389));
#201177=CARTESIAN_POINT('Ctrl Pts',(-20.7077022970713,18.4453570759616,
15.643951007541));
#201178=CARTESIAN_POINT('Ctrl Pts',(-20.7106284105698,18.4529486335987,
15.6444448820955));
#201179=CARTESIAN_POINT('Ctrl Pts',(-20.7119040751706,18.4562833527452,
15.644661103868));
#201180=CARTESIAN_POINT('Ctrl Pts',(-20.7146337326333,18.4634734157778,
15.6451257453601));
#201181=CARTESIAN_POINT('Ctrl Pts',(-20.7160849040996,18.4673297702814,
15.6453739957509));
#201182=CARTESIAN_POINT('Ctrl Pts',(-20.7200717134144,18.4780189191715,
15.64605951838));
#201183=CARTESIAN_POINT('Ctrl Pts',(-20.722583368006,18.4848606830103,15.646495381068));
#201184=CARTESIAN_POINT('Ctrl Pts',(-20.7363485352009,18.5229641947135,
15.648907340079));
#201185=CARTESIAN_POINT('Ctrl Pts',(-20.7469008883667,18.5544764152931,
15.6508443529585));
#201186=CARTESIAN_POINT('Ctrl Pts',(-20.8045488109645,18.7411117093909,
15.6620513335706));
#201187=CARTESIAN_POINT('Ctrl Pts',(-20.8344466713562,18.9009955576402,
15.670620709863));
#201188=CARTESIAN_POINT('Ctrl Pts',(-20.8492352643372,19.1116419049396,
15.6821816623415));
#201189=CARTESIAN_POINT('Ctrl Pts',(-20.8509686689526,19.160646635248,15.6848867256134));
#201190=CARTESIAN_POINT('Ctrl Pts',(-20.8509995791044,19.2096650574301,
15.6876314267646));
#201191=CARTESIAN_POINT('Ctrl Pts',(-20.8509995807897,19.2096677326801,
15.6876315765606));
#201192=CARTESIAN_POINT('Ctrl Pts',(-20.8510434871719,19.27943585758,15.6915381231541));
#201193=CARTESIAN_POINT('Ctrl Pts',(-20.8476384984025,19.3491589547705,
15.6955220276476));
#201194=CARTESIAN_POINT('Ctrl Pts',(-20.8397857342339,19.4288578015771,
15.7002212838235));
#201195=CARTESIAN_POINT('Ctrl Pts',(-20.838698304264,19.4391241385988,15.700829353884));
#201196=CARTESIAN_POINT('Ctrl Pts',(-20.8367354837038,19.4564445058437,
15.7018600347468));
#201197=CARTESIAN_POINT('Ctrl Pts',(-20.8358995712248,19.4635028920424,
15.7022814067909));
#201198=CARTESIAN_POINT('Ctrl Pts',(-20.8342941197586,19.4764984975953,
15.7030597630742));
#201199=CARTESIAN_POINT('Ctrl Pts',(-20.8335349079559,19.4824369371732,
15.7034164189799));
#201200=CARTESIAN_POINT('Ctrl Pts',(-20.8319155539216,19.4946898673831,
15.7041543748108));
#201201=CARTESIAN_POINT('Ctrl Pts',(-20.8310520687409,19.5010038480021,
15.7045357768828));
#201202=CARTESIAN_POINT('Ctrl Pts',(-20.8290496276841,19.5151693620982,
15.7053940391335));
#201203=CARTESIAN_POINT('Ctrl Pts',(-20.8278950218306,19.5230185542208,
15.7058713901581));
#201204=CARTESIAN_POINT('Ctrl Pts',(-20.824844961801,19.5429736274424,15.7070895838323));
#201205=CARTESIAN_POINT('Ctrl Pts',(-20.8228884926196,19.555069759064,15.7078323501742));
#201206=CARTESIAN_POINT('Ctrl Pts',(-20.8108297191291,19.6257273900897,
15.71219705076));
#201207=CARTESIAN_POINT('Ctrl Pts',(-20.7983710488112,19.6838546950599,
15.7158933385397));
#201208=CARTESIAN_POINT('Ctrl Pts',(-20.7680792322583,19.8009084968002,
15.7235578177454));
#201209=CARTESIAN_POINT('Ctrl Pts',(-20.7500878968257,19.8597364512723,
15.7275274295434));
#201210=CARTESIAN_POINT('Ctrl Pts',(-20.7272668328434,19.9241785542234,
15.7319934520378));
#201211=CARTESIAN_POINT('Ctrl Pts',(-20.7249393016113,19.9306506018069,
15.7324433106561));
#201212=CARTESIAN_POINT('Ctrl Pts',(-20.7225806013824,19.9371103165536,
15.7328936098053));
#201213=CARTESIAN_POINT('Origin',(-18.734,19.211,0.));
#201214=CARTESIAN_POINT('',(-20.7225806782305,19.9371101060915,16.7554729098499));
#201215=CARTESIAN_POINT('',(-20.7225806064499,19.9371103026755,16.5356516909487));
#201216=CARTESIAN_POINT('',(-20.7225806064498,19.9371103026755,0.));
#201217=CARTESIAN_POINT('Ctrl Pts',(-20.7225806782305,19.9371101060915,
16.7554729098499));
#201218=CARTESIAN_POINT('Ctrl Pts',(-20.7433303988069,19.8802833341313,
16.752186960848));
#201219=CARTESIAN_POINT('Ctrl Pts',(-20.7616463830241,19.8225613684717,
16.7488940370088));
#201220=CARTESIAN_POINT('Ctrl Pts',(-20.8031161608804,19.6693480182463,
16.7401351003016));
#201221=CARTESIAN_POINT('Ctrl Pts',(-20.8221382522373,19.5729387717263,
16.7345998955843));
#201222=CARTESIAN_POINT('Ctrl Pts',(-20.8362368147881,19.4610092278057,
16.727981283592));
#201223=CARTESIAN_POINT('Ctrl Pts',(-20.837918883443,19.446434821374,16.727115946789));
#201224=CARTESIAN_POINT('Ctrl Pts',(-20.8402567481903,19.4241464763026,
16.7257867843257));
#201225=CARTESIAN_POINT('Ctrl Pts',(-20.8410219631865,19.4164442841063,
16.7253264065544));
#201226=CARTESIAN_POINT('Ctrl Pts',(-20.8422815026815,19.4030185085638,
16.7245220094128));
#201227=CARTESIAN_POINT('Ctrl Pts',(-20.8427948028074,19.3972967547408,
16.7241785912338));
#201228=CARTESIAN_POINT('Ctrl Pts',(-20.8438966146394,19.3844264218433,
16.723404731499));
#201229=CARTESIAN_POINT('Ctrl Pts',(-20.8444720950485,19.3772768243325,
16.722973884264));
#201230=CARTESIAN_POINT('Ctrl Pts',(-20.8459169690324,19.3581085313088,
16.7218161322066));
#201231=CARTESIAN_POINT('Ctrl Pts',(-20.8467200885365,19.3460852403305,
16.7210871558742));
#201232=CARTESIAN_POINT('Ctrl Pts',(-20.8498276623789,19.292714307534,16.7178385212459));
#201233=CARTESIAN_POINT('Ctrl Pts',(-20.8510211083857,19.251313432386,16.7152843495757));
#201234=CARTESIAN_POINT('Ctrl Pts',(-20.8509121657265,19.0404276617498,
16.7020917268623));
#201235=CARTESIAN_POINT('Ctrl Pts',(-20.8304727774874,18.8715948023031,
16.6908605528484));
#201236=CARTESIAN_POINT('Ctrl Pts',(-20.7654397441084,18.6062621605717,
16.6728475888321));
#201237=CARTESIAN_POINT('Ctrl Pts',(-20.7333602027718,18.5074240000789,
16.6660710362922));
#201238=CARTESIAN_POINT('Ctrl Pts',(-20.6904971182236,18.4023580057636,
16.6590602461371));
#201239=CARTESIAN_POINT('Ctrl Pts',(-20.6867761548128,18.393413218159,16.6584650174247));
#201240=CARTESIAN_POINT('Ctrl Pts',(-20.6811908871083,18.3802425289996,
16.6575913355819));
#201241=CARTESIAN_POINT('Ctrl Pts',(-20.6793740071344,18.3759968264975,
16.6573101212883));
#201242=CARTESIAN_POINT('Ctrl Pts',(-20.6761257889718,18.3684745083542,
16.6568126810397));
#201243=CARTESIAN_POINT('Ctrl Pts',(-20.6747000297379,18.365195542979,16.6565961206751));
#201244=CARTESIAN_POINT('Ctrl Pts',(-20.6716271656546,18.3581772389677,
16.6561331897535));
#201245=CARTESIAN_POINT('Ctrl Pts',(-20.6699775452151,18.3544390623605,
16.6558869757115));
#201246=CARTESIAN_POINT('Ctrl Pts',(-20.6654189066792,18.3441892537405,
16.6552127965581));
#201247=CARTESIAN_POINT('Ctrl Pts',(-20.6624877595267,18.337687439939,16.654786165289));
#201248=CARTESIAN_POINT('Ctrl Pts',(-20.6466515873257,18.303028492705,16.6525167802173));
#201249=CARTESIAN_POINT('Ctrl Pts',(-20.6331619195366,18.2751407242402,
16.6507078725077));
#201250=CARTESIAN_POINT('Ctrl Pts',(-20.5446480139625,18.1019550982788,
16.6395212216256));
#201251=CARTESIAN_POINT('Ctrl Pts',(-20.4536052251808,17.9654491021103,
16.6308787033376));
#201252=CARTESIAN_POINT('Ctrl Pts',(-20.2715338455183,17.7510196113438,
16.6154835645376));
#201253=CARTESIAN_POINT('Ctrl Pts',(-20.1879783827937,17.6677908194968,
16.6089133162354));
#201254=CARTESIAN_POINT('Ctrl Pts',(-20.0870076699515,17.5827298209735,
16.6011789972353));
#201255=CARTESIAN_POINT('Ctrl Pts',(-20.0759772281774,17.5736269102728,
16.6003368197567));
#201256=CARTESIAN_POINT('Ctrl Pts',(-20.0582778850036,17.5593194552579,
16.5989893686737));
#201257=CARTESIAN_POINT('Ctrl Pts',(-20.0516684382339,17.5540418163682,
16.5984870422964));
#201258=CARTESIAN_POINT('Ctrl Pts',(-20.0399575017301,17.5448050229905,
16.597598401787));
#201259=CARTESIAN_POINT('Ctrl Pts',(-20.0348691627238,17.5408293147749,
16.5972127547795));
#201260=CARTESIAN_POINT('Ctrl Pts',(-20.0243087484434,17.5326556074793,
16.5964132892473));
#201261=CARTESIAN_POINT('Ctrl Pts',(-20.0188341947642,17.5284609495086,
16.595999344932));
#201262=CARTESIAN_POINT('Ctrl Pts',(-20.0047322471532,17.5177648550862,
16.5949342881041));
#201263=CARTESIAN_POINT('Ctrl Pts',(-19.9960754873648,17.5113026277173,
16.5942816486013));
#201264=CARTESIAN_POINT('Ctrl Pts',(-19.9597641716323,17.4846267628509,
16.5915486534249));
#201265=CARTESIAN_POINT('Ctrl Pts',(-19.9316717847602,17.4650204929477,
16.5894450317506));
#201266=CARTESIAN_POINT('Ctrl Pts',(-19.8572711946517,17.4157353899253,
16.5838980747622));
#201267=CARTESIAN_POINT('Ctrl Pts',(-19.810262510711,17.3871657452674,16.5804164834749));
#201268=CARTESIAN_POINT('Ctrl Pts',(-19.6666535097936,17.3073736265223,
16.5698575039541));
#201269=CARTESIAN_POINT('Ctrl Pts',(-19.5671476058028,17.2617700141565,
16.5626316901323));
#201270=CARTESIAN_POINT('Ctrl Pts',(-19.4286066135071,17.2108301809486,
16.5528808362129));
#201271=CARTESIAN_POINT('Ctrl Pts',(-19.3922848272826,17.1985838306067,
16.5503531180982));
#201272=CARTESIAN_POINT('Ctrl Pts',(-19.3246523566846,17.1778078486303,
16.5457178378031));
#201273=CARTESIAN_POINT('Ctrl Pts',(-19.2934388464731,17.168998812263,16.5436060819469));
#201274=CARTESIAN_POINT('Ctrl Pts',(-19.2559593469489,17.1593453522932,
16.5411116142823));
#201275=CARTESIAN_POINT('Ctrl Pts',(-19.2498774174387,17.1578076454257,
16.5407081151772));
#201276=CARTESIAN_POINT('Ctrl Pts',(-19.2015705670124,17.1458223191853,
16.5375138893784));
#201277=CARTESIAN_POINT('Ctrl Pts',(-19.159036170376,17.1366504776844,16.5347656058128));
#201278=CARTESIAN_POINT('Ctrl Pts',(-19.1088550281401,17.1274383430344,
16.5316212389089));
#201279=CARTESIAN_POINT('Ctrl Pts',(-19.1014565557184,17.1261208298778,
16.5311601309494));
#201280=CARTESIAN_POINT('Ctrl Pts',(-19.0894933795238,17.1240560983347,
16.5304187089213));
#201281=CARTESIAN_POINT('Ctrl Pts',(-19.0849330437054,17.1232844084129,
16.5301370597121));
#201282=CARTESIAN_POINT('Ctrl Pts',(-19.0768421071341,17.1219425380944,
16.5296391383916));
#201283=CARTESIAN_POINT('Ctrl Pts',(-19.0733125568911,17.1213663529253,
16.5294225294626));
#201284=CARTESIAN_POINT('Ctrl Pts',(-19.0657516382568,17.1201517249532,
16.5289598131345));
#201285=CARTESIAN_POINT('Ctrl Pts',(-19.0617198897548,17.1195159973696,
16.5287138605878));
#201286=CARTESIAN_POINT('Ctrl Pts',(-19.0506580944794,17.1178045411081,
16.5280411349471));
#201287=CARTESIAN_POINT('Ctrl Pts',(-19.0436243517688,17.1167525595132,
16.5276156861279));
#201288=CARTESIAN_POINT('Ctrl Pts',(-19.0062028345062,17.111348370723,16.5253638122664));
#201289=CARTESIAN_POINT('Ctrl Pts',(-18.975726688986,17.1076218177237,16.523570617579));
#201290=CARTESIAN_POINT('Ctrl Pts',(-18.8834965209076,17.0983754002523,
16.518237592611));
#201291=CARTESIAN_POINT('Ctrl Pts',(-18.8215679796411,17.0949033867494,
16.5147825375925));
#201292=CARTESIAN_POINT('Ctrl Pts',(-18.612811185808,17.0923815271823,16.5033037353659));
#201293=CARTESIAN_POINT('Ctrl Pts',(-18.4662667659925,17.1058751584313,
16.4954967731419));
#201294=CARTESIAN_POINT('Ctrl Pts',(-18.2488474790931,17.1489809438541,
16.4831218539245));
#201295=CARTESIAN_POINT('Ctrl Pts',(-18.1762313567562,17.1674276533659,
16.478855777376));
#201296=CARTESIAN_POINT('Ctrl Pts',(-18.0922192294708,17.1935811851993,
16.4736930223595));
#201297=CARTESIAN_POINT('Ctrl Pts',(-18.0797254235962,17.1975984010081,
16.4729192958104));
#201298=CARTESIAN_POINT('Ctrl Pts',(-18.0594877861536,17.2043138002028,
16.4716559650957));
#201299=CARTESIAN_POINT('Ctrl Pts',(-18.0517207433681,17.2069413072056,
16.4711686904058));
#201300=CARTESIAN_POINT('Ctrl Pts',(-18.0379186543715,17.2116999420527,
16.4702984058485));
#201301=CARTESIAN_POINT('Ctrl Pts',(-18.031877608758,17.2138134519362,16.4699159839097));
#201302=CARTESIAN_POINT('Ctrl Pts',(-18.0191704131458,17.2183239489796,
16.4691083492976));
#201303=CARTESIAN_POINT('Ctrl Pts',(-18.0125065358845,17.2207270634679,
16.4686829364463));
#201304=CARTESIAN_POINT('Ctrl Pts',(-17.9949161869802,17.2271704136063,
16.4675549638021));
#201305=CARTESIAN_POINT('Ctrl Pts',(-17.9840109017698,17.2312674285262,
16.4668505144229));
#201306=CARTESIAN_POINT('Ctrl Pts',(-17.9335448902501,17.2507038603733,
16.4635661609879));
#201307=CARTESIAN_POINT('Ctrl Pts',(-17.8944194871903,17.267139538666,16.4609496343936));
#201308=CARTESIAN_POINT('Ctrl Pts',(-17.7880576170252,17.3156299758322,
16.4536357557298));
#201309=CARTESIAN_POINT('Ctrl Pts',(-17.72198239082,17.3500720048569,16.4488625503694));
#201310=CARTESIAN_POINT('Ctrl Pts',(-17.5421294548141,17.4562364227782,
16.4352579366508));
#201311=CARTESIAN_POINT('Ctrl Pts',(-17.4331691595399,17.5354142354494,
16.426265373199));
#201312=CARTESIAN_POINT('Ctrl Pts',(-17.3217701230268,17.633819317249,16.4165947511318));
#201313=CARTESIAN_POINT('Ctrl Pts',(-17.3111838170296,17.643362843451,16.4156707861006));
#201314=CARTESIAN_POINT('Ctrl Pts',(-17.2944109768497,17.6587933952721,
16.4141998638855));
#201315=CARTESIAN_POINT('Ctrl Pts',(-17.2881623843253,17.6646121146778,
16.4136502980441));
#201316=CARTESIAN_POINT('Ctrl Pts',(-17.2503901483772,17.7002148992286,
16.4103193771155));
#201317=CARTESIAN_POINT('Ctrl Pts',(-17.2197501394194,17.7309264323014,
16.4075795233403));
#201318=CARTESIAN_POINT('Ctrl Pts',(-17.1849360626935,17.7680355895156,
16.4044436079217));
#201319=CARTESIAN_POINT('Ctrl Pts',(-17.1798281289161,17.7735386367764,
16.4039829081168));
#201320=CARTESIAN_POINT('Ctrl Pts',(-17.1716224247503,17.7824739464397,
16.4032420129867));
#201321=CARTESIAN_POINT('Ctrl Pts',(-17.1685064836133,17.7858893290587,
16.4029604855227));
#201322=CARTESIAN_POINT('Ctrl Pts',(-17.1630002078915,17.7919646088739,
16.4024626989407));
#201323=CARTESIAN_POINT('Ctrl Pts',(-17.1606054017412,17.7946203803622,
16.4022461036791));
#201324=CARTESIAN_POINT('Ctrl Pts',(-17.1554908540555,17.8003212467121,
16.4017833276159));
#201325=CARTESIAN_POINT('Ctrl Pts',(-17.152773195974,17.8033681363064,16.401537302131));
#201326=CARTESIAN_POINT('Ctrl Pts',(-17.1453421272597,17.8117481210668,
16.400864171133));
#201327=CARTESIAN_POINT('Ctrl Pts',(-17.1406467204629,17.8170972102824,
16.4004383925599));
#201328=CARTESIAN_POINT('Ctrl Pts',(-17.1157935924048,17.845700003754,16.398181651692));
#201329=CARTESIAN_POINT('Ctrl Pts',(-17.0961166088964,17.8693687993891,
16.3963840902856));
#201330=CARTESIAN_POINT('Ctrl Pts',(-17.0382313230102,17.9421697107767,
16.3910333186897));
#201331=CARTESIAN_POINT('Ctrl Pts',(-17.0016647670121,17.9925676145352,
16.3875655490246));
#201332=CARTESIAN_POINT('Ctrl Pts',(-16.8863177412652,18.1672583560864,
16.3760574297048));
#201333=CARTESIAN_POINT('Ctrl Pts',(-16.818281524111,18.2981200823489,16.3682331100459));
#201334=CARTESIAN_POINT('Ctrl Pts',(-16.7371336029532,18.5040839523418,
16.3558692723939));
#201335=CARTESIAN_POINT('Ctrl Pts',(-16.7135651951433,18.5745668284206,
16.3516362908328));
#201336=CARTESIAN_POINT('Ctrl Pts',(-16.6902553974999,18.6587604200131,
16.3465102075234));
#201337=CARTESIAN_POINT('Ctrl Pts',(-16.6868778808701,18.6714153710422,
16.3457379844783));
#201338=CARTESIAN_POINT('Ctrl Pts',(-16.681579254526,18.6920345035618,16.3444766272564));
#201339=CARTESIAN_POINT('Ctrl Pts',(-16.6795865296114,18.6999800466228,
16.3439898104134));
#201340=CARTESIAN_POINT('Ctrl Pts',(-16.6761193534797,18.7141527456894,
16.3431200382777));
#201341=CARTESIAN_POINT('Ctrl Pts',(-16.6746269208013,18.7203754299656,
16.342737668335));
#201342=CARTESIAN_POINT('Ctrl Pts',(-16.6715408694223,18.733504892844,16.341929827623));
#201343=CARTESIAN_POINT('Ctrl Pts',(-16.6699536828267,18.7404130884501,
16.3415041550758));
#201344=CARTESIAN_POINT('Ctrl Pts',(-16.6658455440473,18.7587143570004,
16.3403747603357));
#201345=CARTESIAN_POINT('Ctrl Pts',(-16.6633840695393,18.7701204058692,
16.3396691400229));
#201346=CARTESIAN_POINT('Ctrl Pts',(-16.6523679079481,18.8232956412068,
16.3363710424774));
#201347=CARTESIAN_POINT('Ctrl Pts',(-16.6449825124726,18.8652944023139,
16.3337415680137));
#201348=CARTESIAN_POINT('Ctrl Pts',(-16.6281179436273,18.9817086935717,
16.326380479851));
#201349=CARTESIAN_POINT('Ctrl Pts',(-16.6213182247392,19.0564440453024,
16.3215718017951));
#201350=CARTESIAN_POINT('Ctrl Pts',(-16.6120664102933,19.3022537914196,
16.3055433579993));
#201351=CARTESIAN_POINT('Ctrl Pts',(-16.6263613065639,19.4732734475288,
16.2940036296611));
#201352=CARTESIAN_POINT('Ctrl Pts',(-16.6672423124823,19.6704849154768,
16.2812247042703));
#201353=CARTESIAN_POINT('Ctrl Pts',(-16.674056033928,19.7001265730077,16.2793203808293));
#201354=CARTESIAN_POINT('Ctrl Pts',(-16.6833085988988,19.7367450849189,
16.2769968315207));
#201355=CARTESIAN_POINT('Ctrl Pts',(-16.6851479341194,19.7438680255511,
16.276546235937));
#201356=CARTESIAN_POINT('Ctrl Pts',(-16.688090485319,19.7550227265425,16.2758429095609));
#201357=CARTESIAN_POINT('Ctrl Pts',(-16.6891685551354,19.7590609747528,
16.2755887675572));
#201358=CARTESIAN_POINT('Ctrl Pts',(-16.6911880365819,19.766536662922,16.2751192148015));
#201359=CARTESIAN_POINT('Ctrl Pts',(-16.6921261605398,19.7699748883077,
16.2749036228578));
#201360=CARTESIAN_POINT('Ctrl Pts',(-16.6942640504025,19.777733055652,16.274417964383));
#201361=CARTESIAN_POINT('Ctrl Pts',(-16.6954688559691,19.7820515529399,
16.274148194014));
#201362=CARTESIAN_POINT('Ctrl Pts',(-16.6991354261947,19.7950345006919,
16.2733387822597));
#201363=CARTESIAN_POINT('Ctrl Pts',(-16.7016388144918,19.8036872277017,
16.2728015022325));
#201364=CARTESIAN_POINT('Ctrl Pts',(-16.7277644403993,19.891875747321,16.26734524086));
#201365=CARTESIAN_POINT('Ctrl Pts',(-16.7559907964435,19.9699834068524,
16.2626755088247));
#201366=CARTESIAN_POINT('Ctrl Pts',(-16.8485677865108,20.1855942737558,
16.2497330287895));
#201367=CARTESIAN_POINT('Ctrl Pts',(-16.9232019018568,20.3181135927675,
16.2416851553575));
#201368=CARTESIAN_POINT('Ctrl Pts',(-17.0557624904192,20.5036887730365,
16.2289639746873));
#201369=CARTESIAN_POINT('Ctrl Pts',(-17.1034966250975,20.5633987167373,
16.2246145228551));
#201370=CARTESIAN_POINT('Ctrl Pts',(-17.1631304904082,20.6302363970677,
16.2193592460446));
#201371=CARTESIAN_POINT('Ctrl Pts',(-17.1720031448699,20.6399957241842,
16.2185816840114));
#201372=CARTESIAN_POINT('Ctrl Pts',(-17.1865519963965,20.6557010882305,
16.2173133199146));
#201373=CARTESIAN_POINT('Ctrl Pts',(-17.1921727314229,20.6616981867889,
16.216824878432));
#201374=CARTESIAN_POINT('Ctrl Pts',(-17.2022336348675,20.6723082478024,
16.2159532860197));
#201375=CARTESIAN_POINT('Ctrl Pts',(-17.2066600972128,20.6769341091636,
16.2155707295928));
#201376=CARTESIAN_POINT('Ctrl Pts',(-17.2160207792201,20.6866280414095,
16.2147636105943));
#201377=CARTESIAN_POINT('Ctrl Pts',(-17.2209595430058,20.6916915968297,
16.2143388518875));
#201378=CARTESIAN_POINT('Ctrl Pts',(-17.2340654490494,20.7049946228789,
16.2132144611913));
#201379=CARTESIAN_POINT('Ctrl Pts',(-17.2422750200814,20.7131917874288,
16.2125129610422));
#201380=CARTESIAN_POINT('Ctrl Pts',(-17.2804559253733,20.7506933595815,
16.2092629471553));
#201381=CARTESIAN_POINT('Ctrl Pts',(-17.3112243625633,20.779169350315,16.2066787380752));
#201382=CARTESIAN_POINT('Ctrl Pts',(-17.4702251520484,20.9177904566099,
16.1934856211139));
#201383=CARTESIAN_POINT('Ctrl Pts',(-17.6104627465081,21.0131949405217,
16.1822878734906));
#201384=CARTESIAN_POINT('Ctrl Pts',(-17.8533937170849,21.1389940845405,
16.1642470087988));
#201385=CARTESIAN_POINT('Ctrl Pts',(-17.9497204562445,21.1801468752051,
16.1574134825229));
#201386=CARTESIAN_POINT('Ctrl Pts',(-18.0578526454002,21.2171423754431,
16.1503527124055));
#201387=CARTESIAN_POINT('Ctrl Pts',(-18.0670218837612,21.220209465506,16.1497586816396));
#201388=CARTESIAN_POINT('Ctrl Pts',(-18.080597928524,21.2246474430503,16.1488864161077));
#201389=CARTESIAN_POINT('Ctrl Pts',(-18.0849885711777,21.2260668619431,
16.1486054328108));
#201390=CARTESIAN_POINT('Ctrl Pts',(-18.0927892185566,21.2285605357067,
16.1481082477782));
#201391=CARTESIAN_POINT('Ctrl Pts',(-18.0961973347639,21.2296405183625,
16.147891712912));
#201392=CARTESIAN_POINT('Ctrl Pts',(-18.1035086599993,21.2319370065192,
16.1474286666505));
#201393=CARTESIAN_POINT('Ctrl Pts',(-18.1074126508788,21.2331508372785,
16.1471823126587));
#201394=CARTESIAN_POINT('Ctrl Pts',(-18.1181467539414,21.2364542194643,
16.1465073553206));
#201395=CARTESIAN_POINT('Ctrl Pts',(-18.124984035559,21.2385205484021,16.1460800909514));
#201396=CARTESIAN_POINT('Ctrl Pts',(-18.1616683722007,21.24940479267,16.1438012626415));
#201397=CARTESIAN_POINT('Ctrl Pts',(-18.1916983735129,21.257598829291,16.1419838793355));
#201398=CARTESIAN_POINT('Ctrl Pts',(-18.3809297596199,21.3047747632879,
16.1307686751546));
#201399=CARTESIAN_POINT('Ctrl Pts',(-18.5440426464886,21.3258238551038,
16.1221080159552));
#201400=CARTESIAN_POINT('Ctrl Pts',(-18.8251657643572,21.3292813330703,
16.1067187015476));
#201401=CARTESIAN_POINT('Ctrl Pts',(-18.9422677222171,21.3209872657003,
16.1001766564776));
#201402=CARTESIAN_POINT('Ctrl Pts',(-19.0721994938407,21.3008599103215,
16.0924740809648));
#201403=CARTESIAN_POINT('Ctrl Pts',(-19.0863030542917,21.2985286549926,
16.0916322862241));
#201404=CARTESIAN_POINT('Ctrl Pts',(-19.1087102087637,21.2945913144706,
16.0902853331548));
#201405=CARTESIAN_POINT('Ctrl Pts',(-19.1170298087498,21.2930779689371,
16.0897831186065));
#201406=CARTESIAN_POINT('Ctrl Pts',(-19.1316858092682,21.2903212091437,
16.0888946083805));
#201407=CARTESIAN_POINT('Ctrl Pts',(-19.1380260415081,21.2890985660084,
16.0885089792002));
#201408=CARTESIAN_POINT('Ctrl Pts',(-19.1511273017089,21.2865099110984,
16.0877094843103));
#201409=CARTESIAN_POINT('Ctrl Pts',(-19.1578874379376,21.2851398253506,
16.0872954924832));
#201410=CARTESIAN_POINT('Ctrl Pts',(-19.1752210551124,21.2815385185251,
16.0862301737871));
#201411=CARTESIAN_POINT('Ctrl Pts',(-19.1857842702045,21.2792593509,16.0855773184774));
#201412=CARTESIAN_POINT('Ctrl Pts',(-19.2297868470935,21.2694119761867,
16.0828422335204));
#201413=CARTESIAN_POINT('Ctrl Pts',(-19.2630557912861,21.2611132201042,
16.080736693342));
#201414=CARTESIAN_POINT('Ctrl Pts',(-19.3491912086119,21.2373909875361,
16.0751834720756));
#201415=CARTESIAN_POINT('Ctrl Pts',(-19.4016807857419,21.2207069952663,
16.0716974271914));
#201416=CARTESIAN_POINT('Ctrl Pts',(-19.6494098754055,21.1311888175244,
16.0547669633032));
#201417=CARTESIAN_POINT('Ctrl Pts',(-19.8338097655697,21.031853061553,16.0405739686977));
#201418=CARTESIAN_POINT('Ctrl Pts',(-20.00435118889,20.9044926485973,16.0271549253794));
#201419=CARTESIAN_POINT('Ctrl Pts',(-20.0079697057802,20.901772215119,16.0268701185296));
#201420=CARTESIAN_POINT('Ctrl Pts',(-20.0279634473045,20.8866401141797,
16.025296105304));
#201421=CARTESIAN_POINT('Ctrl Pts',(-20.0441667115951,20.8740016402553,
16.0240192156397));
#201422=CARTESIAN_POINT('Ctrl Pts',(-20.0652102920254,20.8570892256756,
16.0223620048336));
#201423=CARTESIAN_POINT('Ctrl Pts',(-20.0702181075084,20.8530267208939,
16.0219677178025));
#201424=CARTESIAN_POINT('Ctrl Pts',(-20.0782511226781,20.8464489889606,
16.0213354907494));
#201425=CARTESIAN_POINT('Ctrl Pts',(-20.081287964225,20.8439481370676,16.0210965377843));
#201426=CARTESIAN_POINT('Ctrl Pts',(-20.0869604319314,20.8392502395933,
16.020650337992));
#201427=CARTESIAN_POINT('Ctrl Pts',(-20.0895976882824,20.837055251444,16.0204429486207));
#201428=CARTESIAN_POINT('Ctrl Pts',(-20.0958336410269,20.831839353648,16.0199526787635));
#201429=CARTESIAN_POINT('Ctrl Pts',(-20.099427661045,20.8288128382458,16.01967020676));
#201430=CARTESIAN_POINT('Ctrl Pts',(-20.1106565996605,20.8192929029103,
16.018787841166));
#201431=CARTESIAN_POINT('Ctrl Pts',(-20.1182556286363,20.8127571034364,
16.0181909641413));
#201432=CARTESIAN_POINT('Ctrl Pts',(-20.1360726278116,20.7972114976654,
16.016791308788));
#201433=CARTESIAN_POINT('Ctrl Pts',(-20.1462507307738,20.788156448322,16.0159915924635));
#201434=CARTESIAN_POINT('Ctrl Pts',(-20.1816416892114,20.7560531975546,
16.0132073665971));
#201435=CARTESIAN_POINT('Ctrl Pts',(-20.2063845877909,20.7324925959874,
16.0112545122457));
#201436=CARTESIAN_POINT('Ctrl Pts',(-20.2842584683261,20.6546600397496,
16.005045449642));
#201437=CARTESIAN_POINT('Ctrl Pts',(-20.3350451785142,20.5981233988142,
16.0008961828023));
#201438=CARTESIAN_POINT('Ctrl Pts',(-20.4906155867975,20.4049823850317,
15.9874090117612));
#201439=CARTESIAN_POINT('Ctrl Pts',(-20.5817953836118,20.2583479078304,
15.978142784349));
#201440=CARTESIAN_POINT('Ctrl Pts',(-20.6640064837358,20.0812319187437,
15.9667988654617));
#201441=CARTESIAN_POINT('Ctrl Pts',(-20.6734389218583,20.0600024883679,
15.9654381553835));
#201442=CARTESIAN_POINT('Ctrl Pts',(-20.6862672065903,20.02980011932,15.9634990949465));
#201443=CARTESIAN_POINT('Ctrl Pts',(-20.6899545521561,20.0209522619473,
15.9629306601334));
#201444=CARTESIAN_POINT('Ctrl Pts',(-20.6958422183918,20.0065499976889,
15.9620046405147));
#201445=CARTESIAN_POINT('Ctrl Pts',(-20.6980793649531,20.0010107187413,
15.9616483063261));
#201446=CARTESIAN_POINT('Ctrl Pts',(-20.7027084833689,19.9894076045086,
15.9609014923674));
#201447=CARTESIAN_POINT('Ctrl Pts',(-20.7050959508037,19.9833420501925,
15.960510865377));
#201448=CARTESIAN_POINT('Ctrl Pts',(-20.7107007408829,19.9689073650376,
15.9595806725925));
#201449=CARTESIAN_POINT('Ctrl Pts',(-20.7138929632435,19.9605286807176,
15.9590402710366));
#201450=CARTESIAN_POINT('Ctrl Pts',(-20.7189003798113,19.9471304031136,
15.9581753084636));
#201451=CARTESIAN_POINT('Ctrl Pts',(-20.7207499860271,19.942123778256,15.9578519123852));
#201452=CARTESIAN_POINT('Ctrl Pts',(-20.7225806064913,19.9371103025619,
15.9575278864865));
#201453=CARTESIAN_POINT('Ctrl Pts',(-20.7225806013824,19.9371103165536,
15.7328936098053));
#201454=CARTESIAN_POINT('Ctrl Pts',(-20.6687684267845,20.0844844057023,
15.743166884953));
#201455=CARTESIAN_POINT('Ctrl Pts',(-20.5987347395985,20.2254367109955,
15.7537162423725));
#201456=CARTESIAN_POINT('Ctrl Pts',(-20.4968362899241,20.3836351557168,
15.7656589472727));
#201457=CARTESIAN_POINT('Ctrl Pts',(-20.4793387436348,20.4095232178004,
15.7676152445733));
#201458=CARTESIAN_POINT('Ctrl Pts',(-20.4571389077526,20.440850577118,15.7699758583636));
#201459=CARTESIAN_POINT('Ctrl Pts',(-20.4529746813286,20.4466642690325,
15.7704136454338));
#201460=CARTESIAN_POINT('Ctrl Pts',(-20.4463824402328,20.4557699015741,
15.7710987177525));
#201461=CARTESIAN_POINT('Ctrl Pts',(-20.4439742522762,20.4590760340178,
15.7713473314855));
#201462=CARTESIAN_POINT('Ctrl Pts',(-20.4394433479387,20.4652586521843,
15.771811979727));
#201463=CARTESIAN_POINT('Ctrl Pts',(-20.4373229518937,20.4681367075116,
15.7720281624065));
#201464=CARTESIAN_POINT('Ctrl Pts',(-20.4324506101249,20.4747150745302,
15.7725220461787));
#201465=CARTESIAN_POINT('Ctrl Pts',(-20.4296938624,20.4784117683572,15.7727994080052));
#201466=CARTESIAN_POINT('Ctrl Pts',(-20.4224404950687,20.4880722295795,
15.7735238561962));
#201467=CARTESIAN_POINT('Ctrl Pts',(-20.417924310188,20.4940213194787,15.7739696100002));
#201468=CARTESIAN_POINT('Ctrl Pts',(-20.3874376245079,20.5337426182823,
15.7769442570205));
#201469=CARTESIAN_POINT('Ctrl Pts',(-20.3604823100834,20.5667506624727,
15.7794084446909));
#201470=CARTESIAN_POINT('Ctrl Pts',(-20.2836442205211,20.6552491803633,
15.7860635771181));
#201471=CARTESIAN_POINT('Ctrl Pts',(-20.2317951831533,20.7089532634295,
15.790158518054));
#201472=CARTESIAN_POINT('Ctrl Pts',(-20.1743796533674,20.7624543133703,
15.7944341890725));
#201473=CARTESIAN_POINT('Ctrl Pts',(-20.1715358442198,20.7650896785448,
15.7946453290362));
#201474=CARTESIAN_POINT('Ctrl Pts',(-20.0884525749971,20.8416599783403,
15.8007958993886));
#201475=CARTESIAN_POINT('Ctrl Pts',(-20.0026247582199,20.9092885662888,
15.8066722015024));
#201476=CARTESIAN_POINT('Ctrl Pts',(-19.8664211878089,21.0005017380355,
15.8157891402054));
#201477=CARTESIAN_POINT('Ctrl Pts',(-19.8197069438152,21.0292227620463,
15.8188809591168));
#201478=CARTESIAN_POINT('Ctrl Pts',(-19.7521462118145,21.0672280859273,
15.823341134852));
#201479=CARTESIAN_POINT('Ctrl Pts',(-19.7321821352076,21.0780395776416,
15.8246576473177));
#201480=CARTESIAN_POINT('Ctrl Pts',(-19.696742059131,21.096501151957,15.8269945800711));
#201481=CARTESIAN_POINT('Ctrl Pts',(-19.6813389625752,21.1042870173958,
15.8280102182647));
#201482=CARTESIAN_POINT('Ctrl Pts',(-19.6584581504781,21.1155035480535,
15.8295195716713));
#201483=CARTESIAN_POINT('Ctrl Pts',(-19.6510526277356,21.1190804782773,
15.830008182365));
#201484=CARTESIAN_POINT('Ctrl Pts',(-19.6381021944432,21.1252428399773,
15.8308628926934));
#201485=CARTESIAN_POINT('Ctrl Pts',(-19.6325665357398,21.1278475703709,
15.8312283175899));
#201486=CARTESIAN_POINT('Ctrl Pts',(-19.6215183369507,21.1329877777601,
15.8319578322705));
#201487=CARTESIAN_POINT('Ctrl Pts',(-19.6160060317938,21.1355236228662,
15.8323219049781));
#201488=CARTESIAN_POINT('Ctrl Pts',(-19.6028189278206,21.1415215769473,
15.8331931371012));
#201489=CARTESIAN_POINT('Ctrl Pts',(-19.5951342713639,21.1449616469509,
15.8337010485587));
#201490=CARTESIAN_POINT('Ctrl Pts',(-19.5674262336606,21.1571673833539,
15.8355332667941));
#201491=CARTESIAN_POINT('Ctrl Pts',(-19.5472884310441,21.1656684226986,
15.8368665538985));
#201492=CARTESIAN_POINT('Ctrl Pts',(-19.3527347733059,21.2442710151523,
15.8497675630087));
#201493=CARTESIAN_POINT('Ctrl Pts',(-19.1698748073467,21.2911462019796,
15.8621583631002));
#201494=CARTESIAN_POINT('Ctrl Pts',(-18.9052259702644,21.3225277001215,
15.8797490960574));
#201495=CARTESIAN_POINT('Ctrl Pts',(-18.8267085652016,21.3274296231783,
15.8849098323942));
#201496=CARTESIAN_POINT('Ctrl Pts',(-18.7124858595279,21.3281901831663,
15.892188560959));
#201497=CARTESIAN_POINT('Ctrl Pts',(-18.6768730135779,21.3275287581502,
15.8944252552227));
#201498=CARTESIAN_POINT('Ctrl Pts',(-18.6338579301177,21.3256432157692,
15.897074039299));
#201499=CARTESIAN_POINT('Ctrl Pts',(-18.6264260007521,21.3252781753177,
15.8975297716938));
#201500=CARTESIAN_POINT('Ctrl Pts',(-18.6148484321837,21.3246483050234,
15.8982365772241));
#201501=CARTESIAN_POINT('Ctrl Pts',(-18.6107014713951,21.324410449243,15.8984891190385));
#201502=CARTESIAN_POINT('Ctrl Pts',(-18.6029952415105,21.3239456861523,
15.8989572114241));
#201503=CARTESIAN_POINT('Ctrl Pts',(-18.5994358801478,21.3237219924297,
15.8991729337287));
#201504=CARTESIAN_POINT('Ctrl Pts',(-18.5913686625607,21.323194525544,15.8996607878753));
#201505=CARTESIAN_POINT('Ctrl Pts',(-18.5868612146184,21.322885316693,15.8999326118657));
#201506=CARTESIAN_POINT('Ctrl Pts',(-18.5752126903372,21.3220487588623,
15.9006332019892));
#201507=CARTESIAN_POINT('Ctrl Pts',(-18.5680731709321,21.3214996002596,
15.9010607746325));
#201508=CARTESIAN_POINT('Ctrl Pts',(-18.5239705186385,21.3178821256638,
15.9036914580934));
#201509=CARTESIAN_POINT('Ctrl Pts',(-18.4870880847228,21.3138788733836,
15.9058456942657));
#201510=CARTESIAN_POINT('Ctrl Pts',(-18.2814941211887,21.2860791065581,
15.9176916625751));
#201511=CARTESIAN_POINT('Ctrl Pts',(-18.1160191661373,21.2429514013927,
15.926655953448));
#201512=CARTESIAN_POINT('Ctrl Pts',(-17.8690123270759,21.1455621848431,
15.9412632235049));
#201513=CARTESIAN_POINT('Ctrl Pts',(-17.782994299292,21.1047580696582,15.9465966981626));
#201514=CARTESIAN_POINT('Ctrl Pts',(-17.6813795596371,21.0478819636713,
15.9533777694065));
#201515=CARTESIAN_POINT('Ctrl Pts',(-17.6629023211226,21.0371694480811,
15.9546309936433));
#201516=CARTESIAN_POINT('Ctrl Pts',(-17.6368704666303,21.0215460114992,
15.9564269250107));
#201517=CARTESIAN_POINT('Ctrl Pts',(-17.6291798633218,21.0168633764833,
15.9569613196871));
#201518=CARTESIAN_POINT('Ctrl Pts',(-17.6159677045651,21.0087028027055,
15.9578861102114));
#201519=CARTESIAN_POINT('Ctrl Pts',(-17.6104318863239,21.005248107969,15.9582756468334));
#201520=CARTESIAN_POINT('Ctrl Pts',(-17.5998655155545,20.9985859600986,
15.95902315031));
#201521=CARTESIAN_POINT('Ctrl Pts',(-17.5948323690298,20.9953827226711,
15.9593809582131));
#201522=CARTESIAN_POINT('Ctrl Pts',(-17.5817849385572,20.9870012653827,
15.9603130885546));
#201523=CARTESIAN_POINT('Ctrl Pts',(-17.5737920692595,20.9817901047953,
15.9608886367991));
#201524=CARTESIAN_POINT('Ctrl Pts',(-17.5466837792203,20.9638538205662,
15.9628562958938));
#201525=CARTESIAN_POINT('Ctrl Pts',(-17.5277408188304,20.9508721352653,
15.9642580285542));
#201526=CARTESIAN_POINT('Ctrl Pts',(-17.3655555694147,20.8358041045491,
15.9764977884836));
#201527=CARTESIAN_POINT('Ctrl Pts',(-17.2353678326145,20.7165585569388,
15.9880431994529));
#201528=CARTESIAN_POINT('Ctrl Pts',(-17.0652545836154,20.5165647747321,
16.0053902667699));
#201529=CARTESIAN_POINT('Ctrl Pts',(-17.013171935578,20.4471081377049,16.0111054114842));
#201530=CARTESIAN_POINT('Ctrl Pts',(-16.9447441029803,20.343111946813,16.019053011665));
#201531=CARTESIAN_POINT('Ctrl Pts',(-16.9248393865284,20.3110238214218,
16.0214275260871));
#201532=CARTESIAN_POINT('Ctrl Pts',(-16.9019865256411,20.2718830748952,
16.0242165390101));
#201533=CARTESIAN_POINT('Ctrl Pts',(-16.8982058398658,20.265327308961,16.0246801364237));
#201534=CARTESIAN_POINT('Ctrl Pts',(-16.8923908775128,20.2551179644544,
16.0253964507646));
#201535=CARTESIAN_POINT('Ctrl Pts',(-16.890332178726,20.2514784712916,16.0256506996772));
#201536=CARTESIAN_POINT('Ctrl Pts',(-16.886538829989,20.2447257498905,16.0261203510784));
#201537=CARTESIAN_POINT('Ctrl Pts',(-16.8848012731718,20.2416142681333,
16.0263359353877));
#201538=CARTESIAN_POINT('Ctrl Pts',(-16.8808966112612,20.2345804369597,
16.0268214520563));
#201539=CARTESIAN_POINT('Ctrl Pts',(-16.8787341040025,20.2306555968949,
16.027091089014));
#201540=CARTESIAN_POINT('Ctrl Pts',(-16.8724048309785,20.2190814940319,
16.0278825614101));
#201541=CARTESIAN_POINT('Ctrl Pts',(-16.8682727352556,20.2114132403275,
16.0284022381136));
#201542=CARTESIAN_POINT('Ctrl Pts',(-16.8392494380522,20.1567471374626,
16.0320752168742));
#201543=CARTESIAN_POINT('Ctrl Pts',(-16.8160874659028,20.1088473493953,
16.0351277602357));
#201544=CARTESIAN_POINT('Ctrl Pts',(-16.7881148402491,20.0449627115505,
16.0390503640187));
#201545=CARTESIAN_POINT('Ctrl Pts',(-16.7816550682472,20.0297259289341,
16.0399751236528));
#201546=CARTESIAN_POINT('Ctrl Pts',(-16.7187558543483,19.8763854384308,
16.049188503332));
#201547=CARTESIAN_POINT('Ctrl Pts',(-16.676885167547,19.7327555678079,16.0570959370483));
#201548=CARTESIAN_POINT('Ctrl Pts',(-16.6395509025466,19.5252737510594,
16.0687600125105));
#201549=CARTESIAN_POINT('Ctrl Pts',(-16.6312927524878,19.4641923995311,
16.0722178001693));
#201550=CARTESIAN_POINT('Ctrl Pts',(-16.6223414882622,19.3658199989051,
16.0778869035785));
#201551=CARTESIAN_POINT('Ctrl Pts',(-16.6199486744876,19.3287185087264,
16.080047418603));
#201552=CARTESIAN_POINT('Ctrl Pts',(-16.6181104691525,19.2804570243006,
16.0828944109975));
#201553=CARTESIAN_POINT('Ctrl Pts',(-16.6177746661088,19.2693362153922,
16.0835529452572));
#201554=CARTESIAN_POINT('Ctrl Pts',(-16.617371142953,19.2512471679603,16.0846283839078));
#201555=CARTESIAN_POINT('Ctrl Pts',(-16.6172501383691,19.2442802421015,
16.0850436143827));
#201556=CARTESIAN_POINT('Ctrl Pts',(-16.6170835927895,19.2308818848883,
16.0858441892655));
#201557=CARTESIAN_POINT('Ctrl Pts',(-16.6170329608621,19.2244505855536,
16.086229369544));
#201558=CARTESIAN_POINT('Ctrl Pts',(-16.6169841377642,19.2097255763105,
16.087113373366));
#201559=CARTESIAN_POINT('Ctrl Pts',(-16.6170053768579,19.2014319466948,
16.0876128005249));
#201560=CARTESIAN_POINT('Ctrl Pts',(-16.6171912595583,19.1794010358939,
16.0889436078002));
#201561=CARTESIAN_POINT('Ctrl Pts',(-16.6174408901145,19.1656650406568,
16.0897776345287));
#201562=CARTESIAN_POINT('Ctrl Pts',(-16.6203596092514,19.0610974959766,
16.096160397941));
#201563=CARTESIAN_POINT('Ctrl Pts',(-16.6287404576868,18.9705318584629,
16.1018878466984));
#201564=CARTESIAN_POINT('Ctrl Pts',(-16.6648429900671,18.7419059894704,
16.1168361282648));
#201565=CARTESIAN_POINT('Ctrl Pts',(-16.7005575127879,18.6055525266388,
16.1262342150391));
#201566=CARTESIAN_POINT('Ctrl Pts',(-16.7683400732216,18.4230969446966,
16.1389735316258));
#201567=CARTESIAN_POINT('Ctrl Pts',(-16.7890967542797,18.373168075765,16.1424735128415));
#201568=CARTESIAN_POINT('Ctrl Pts',(-16.8234970298246,18.2986105420742,
16.1476683327111));
#201569=CARTESIAN_POINT('Ctrl Pts',(-16.8357568570056,18.2733703987011,
16.1494211408575));
#201570=CARTESIAN_POINT('Ctrl Pts',(-16.851657273664,18.2422262384442,16.1515698932825));
#201571=CARTESIAN_POINT('Ctrl Pts',(-16.8548292236553,18.236087728643,16.1519927197007));
#201572=CARTESIAN_POINT('Ctrl Pts',(-16.8599018662612,18.226387649803,16.1526596385724));
#201573=CARTESIAN_POINT('Ctrl Pts',(-16.8617827574412,18.2228158611174,
16.1529049471288));
#201574=CARTESIAN_POINT('Ctrl Pts',(-16.8653533343664,18.2160821686095,
16.1533668788016));
#201575=CARTESIAN_POINT('Ctrl Pts',(-16.8670408141831,18.2129192162611,
16.1535836298079));
#201576=CARTESIAN_POINT('Ctrl Pts',(-16.8709224294182,18.2056879436735,
16.1540786747053));
#201577=CARTESIAN_POINT('Ctrl Pts',(-16.8731218573104,18.2016225168015,
16.1543566284197));
#201578=CARTESIAN_POINT('Ctrl Pts',(-16.879007174615,18.1908287038242,16.1550937284313));
#201579=CARTESIAN_POINT('Ctrl Pts',(-16.8827163919936,18.1841130234875,
16.1555514292739));
#201580=CARTESIAN_POINT('Ctrl Pts',(-16.9092612613792,18.1366638317413,
16.1587799007413));
#201581=CARTESIAN_POINT('Ctrl Pts',(-16.9334045226705,18.0966722639571,
16.1614727934465));
#201582=CARTESIAN_POINT('Ctrl Pts',(-16.9612904215477,18.0537576896911,
16.1643677632592));
#201583=CARTESIAN_POINT('Ctrl Pts',(-16.9637399274954,18.0500140868769,
16.1646203466521));
#201584=CARTESIAN_POINT('Ctrl Pts',(-16.9790345291767,18.0268001500309,
16.1661870601097));
#201585=CARTESIAN_POINT('Ctrl Pts',(-16.9921891435605,18.0075349674985,
16.1674892700612));
#201586=CARTESIAN_POINT('Ctrl Pts',(-17.0319377398353,17.9513398163971,
16.171305524648));
#201587=CARTESIAN_POINT('Ctrl Pts',(-17.0594074724403,17.9150448250689,
16.1737937394058));
#201588=CARTESIAN_POINT('Ctrl Pts',(-17.156793091367,17.7946439776979,16.1822247273343));
#201589=CARTESIAN_POINT('Ctrl Pts',(-17.2320430219157,17.7150820989592,
16.1881127371847));
#201590=CARTESIAN_POINT('Ctrl Pts',(-17.3539495572197,17.6047040510136,
16.1972568865666));
#201591=CARTESIAN_POINT('Ctrl Pts',(-17.3962267197886,17.5693277105988,
16.200364295846));
#201592=CARTESIAN_POINT('Ctrl Pts',(-17.4669834401344,17.5146701412555,
16.2055081454606));
#201593=CARTESIAN_POINT('Ctrl Pts',(-17.4946377629391,17.4943617150345,
16.2075052013834));
#201594=CARTESIAN_POINT('Ctrl Pts',(-17.531637095013,17.4685507826268,16.2101657845621));
#201595=CARTESIAN_POINT('Ctrl Pts',(-17.5405490847524,17.4624346632883,
16.2108057849366));
#201596=CARTESIAN_POINT('Ctrl Pts',(-17.5552247269666,17.4525275264622,
16.2118584844579));
#201597=CARTESIAN_POINT('Ctrl Pts',(-17.560960834115,17.4486959121442,16.2122696423624));
#201598=CARTESIAN_POINT('Ctrl Pts',(-17.5721021357031,17.4413322222077,
16.2130677101101));
#201599=CARTESIAN_POINT('Ctrl Pts',(-17.5775049702283,17.4377967021533,
16.2134544845858));
#201600=CARTESIAN_POINT('Ctrl Pts',(-17.5900196113696,17.4296888666572,
16.2143498682619));
#201601=CARTESIAN_POINT('Ctrl Pts',(-17.5971427682634,17.4251343514277,
16.2148591336148));
#201602=CARTESIAN_POINT('Ctrl Pts',(-17.6163783328129,17.4129969361044,
16.2162334632431));
#201603=CARTESIAN_POINT('Ctrl Pts',(-17.6285403913981,17.405493908408,16.2171014557256));
#201604=CARTESIAN_POINT('Ctrl Pts',(-17.7408542435865,17.3377653763361,
16.2251097572964));
#201605=CARTESIAN_POINT('Ctrl Pts',(-17.8457399219199,17.2858161977551,
16.2325519341344));
#201606=CARTESIAN_POINT('Ctrl Pts',(-18.1056902651641,17.1828456766189,
16.2508154733566));
#201607=CARTESIAN_POINT('Ctrl Pts',(-18.2634243809703,17.1405551807621,
16.2617770107206));
#201608=CARTESIAN_POINT('Ctrl Pts',(-18.4565496705893,17.1120089245101,
16.2741813153607));
#201609=CARTESIAN_POINT('Ctrl Pts',(-18.4887611746939,17.1080020432371,
16.2762152702656));
#201610=CARTESIAN_POINT('Ctrl Pts',(-18.5282532198536,17.1040093449202,
16.2786561058693));
#201611=CARTESIAN_POINT('Ctrl Pts',(-18.5354562169685,17.1033183997965,
16.2790991484562));
#201612=CARTESIAN_POINT('Ctrl Pts',(-18.5467547696273,17.1022930250103,
16.2797905907054));
#201613=CARTESIAN_POINT('Ctrl Pts',(-18.5508479181659,17.1019335718734,
16.2800403592994));
#201614=CARTESIAN_POINT('Ctrl Pts',(-18.5585013303763,17.1012839110047,
16.2805059977598));
#201615=CARTESIAN_POINT('Ctrl Pts',(-18.5620612427187,17.1009908002146,
16.2807220227805));
#201616=CARTESIAN_POINT('Ctrl Pts',(-18.5701900166606,17.1003422140641,
16.2812140320091));
#201617=CARTESIAN_POINT('Ctrl Pts',(-18.5747592924736,17.0999925632661,
16.281489686624));
#201618=CARTESIAN_POINT('Ctrl Pts',(-18.5888100791606,17.0989632468895,
16.2823346438884));
#201619=CARTESIAN_POINT('Ctrl Pts',(-18.5982952117365,17.0983325918007,
16.2829012681832));
#201620=CARTESIAN_POINT('Ctrl Pts',(-18.6836872436832,17.0932324468211,
16.2879710614189));
#201621=CARTESIAN_POINT('Ctrl Pts',(-18.759788118296,17.0927912346997,16.2922670377417));
#201622=CARTESIAN_POINT('Ctrl Pts',(-18.8781794958735,17.0984884048164,
16.2988266480516));
#201623=CARTESIAN_POINT('Ctrl Pts',(-18.9205335974498,17.1018062284293,
16.3011483911178));
#201624=CARTESIAN_POINT('Ctrl Pts',(-19.0714390182891,17.11820890987,16.3094125533286));
#201625=CARTESIAN_POINT('Ctrl Pts',(-19.1790385404864,17.138422028434,16.3152991360514));
#201626=CARTESIAN_POINT('Ctrl Pts',(-19.3377692608823,17.1811761884564,
16.3244399676615));
#201627=CARTESIAN_POINT('Ctrl Pts',(-19.3903645225702,17.1975683533973,
16.3275454753109));
#201628=CARTESIAN_POINT('Ctrl Pts',(-19.4745732064122,17.2274637166386,
16.3326864576675));
#201629=CARTESIAN_POINT('Ctrl Pts',(-19.5066030741639,17.2397189051422,
16.3346826055158));
#201630=CARTESIAN_POINT('Ctrl Pts',(-19.5483165266308,17.256852005256,16.3373421503293));
#201631=CARTESIAN_POINT('Ctrl Pts',(-19.5582814039354,17.261034371719,16.337982043846));
#201632=CARTESIAN_POINT('Ctrl Pts',(-19.574553317376,17.2680108853578,16.3390346123738));
#201633=CARTESIAN_POINT('Ctrl Pts',(-19.5808795699397,17.2707599191705,
16.3394457468954));
#201634=CARTESIAN_POINT('Ctrl Pts',(-19.5931016125269,17.2761420950726,
16.3402438012605));
#201635=CARTESIAN_POINT('Ctrl Pts',(-19.5989990192247,17.278771393387,16.3406305859059));
#201636=CARTESIAN_POINT('Ctrl Pts',(-19.612591397065,17.284906114165,16.3415260397565));
#201637=CARTESIAN_POINT('Ctrl Pts',(-19.6202775403846,17.2884307247288,
16.3420353654378));
#201638=CARTESIAN_POINT('Ctrl Pts',(-19.6408989808854,17.298036972484,16.3434099634373));
#201639=CARTESIAN_POINT('Ctrl Pts',(-19.6537939682846,17.3042036431879,
16.3442781657422));
#201640=CARTESIAN_POINT('Ctrl Pts',(-19.7717736487752,17.3620993811035,
16.3523026798732));
#201641=CARTESIAN_POINT('Ctrl Pts',(-19.8724411974683,17.422326909532,16.3597622791222));
#201642=CARTESIAN_POINT('Ctrl Pts',(-20.1005656385797,17.5858979201879,
16.3780997469604));
#201643=CARTESIAN_POINT('Ctrl Pts',(-20.2220273152436,17.6963273176661,
16.389120010295));
#201644=CARTESIAN_POINT('Ctrl Pts',(-20.3502421957089,17.8433595244109,
16.4015038358265));
#201645=CARTESIAN_POINT('Ctrl Pts',(-20.3703945771774,17.8675371837812,
16.4034747427147));
#201646=CARTESIAN_POINT('Ctrl Pts',(-20.3944666239856,17.8977631741408,
16.4058504738676));
#201647=CARTESIAN_POINT('Ctrl Pts',(-20.3989032624609,17.9033924517667,
16.4062892676042));
#201648=CARTESIAN_POINT('Ctrl Pts',(-20.4058289575597,17.9122722781625,
16.4069755603582));
#201649=CARTESIAN_POINT('Ctrl Pts',(-20.408337272522,17.9155076390406,16.4072243955682));
#201650=CARTESIAN_POINT('Ctrl Pts',(-20.4130180100092,17.9215814110329,
16.4076892321713));
#201651=CARTESIAN_POINT('Ctrl Pts',(-20.41519260431,17.9244180154616,16.4079053830788));
#201652=CARTESIAN_POINT('Ctrl Pts',(-20.4201529585156,17.9309224971171,
16.4083989003309));
#201653=CARTESIAN_POINT('Ctrl Pts',(-20.4229339346652,17.9345939603114,
16.4086759292947));
#201654=CARTESIAN_POINT('Ctrl Pts',(-20.4301819902196,17.9442280542002,
16.4093989368037));
#201655=CARTESIAN_POINT('Ctrl Pts',(-20.4346296589565,17.9502053008563,
16.4098435913896));
#201656=CARTESIAN_POINT('Ctrl Pts',(-20.4640845931016,17.9902294087843,
16.412795916421));
#201657=CARTESIAN_POINT('Ctrl Pts',(-20.4881013628316,18.0249972667431,
16.4152399795657));
#201658=CARTESIAN_POINT('Ctrl Pts',(-20.551518383368,18.1229481083979,16.4218682840979));
#201659=CARTESIAN_POINT('Ctrl Pts',(-20.5886525376176,18.1875277514,16.4259559571741));
#201660=CARTESIAN_POINT('Ctrl Pts',(-20.6728512724097,18.353653330175,16.436104231651));
#201661=CARTESIAN_POINT('Ctrl Pts',(-20.7154130829604,18.4572168760118,
16.4421169227898));
#201662=CARTESIAN_POINT('Ctrl Pts',(-20.7754133478612,18.6440361450615,
16.453020106146));
#201663=CARTESIAN_POINT('Ctrl Pts',(-20.7963949659274,18.7258803855298,
16.4578125155934));
#201664=CARTESIAN_POINT('Ctrl Pts',(-20.815132662147,18.8226990448179,16.4636014619307));
#201665=CARTESIAN_POINT('Ctrl Pts',(-20.8176912851591,18.8366720653435,
16.4644396737766));
#201666=CARTESIAN_POINT('Ctrl Pts',(-20.8214097406657,18.8581998135076,
16.4657356903216));
#201667=CARTESIAN_POINT('Ctrl Pts',(-20.8226696393869,18.8657370101307,
16.4661903114204));
#201668=CARTESIAN_POINT('Ctrl Pts',(-20.8248931359332,18.8794965479966,
16.4670218876966));
#201669=CARTESIAN_POINT('Ctrl Pts',(-20.8258698385557,18.8857167053188,
16.4673984219719));
#201670=CARTESIAN_POINT('Ctrl Pts',(-20.8279419771816,18.8993085853143,
16.4682225715453));
#201671=CARTESIAN_POINT('Ctrl Pts',(-20.829026260834,18.9066818999888,16.468670535182));
#201672=CARTESIAN_POINT('Ctrl Pts',(-20.8318905544563,18.9269007283078,
16.4699014048496));
#201673=CARTESIAN_POINT('Ctrl Pts',(-20.8335914777713,18.9397569551365,
16.4706867993473));
#201674=CARTESIAN_POINT('Ctrl Pts',(-20.8416314806901,19.0051410979391,
16.4746956425342));
#201675=CARTESIAN_POINT('Ctrl Pts',(-20.8461174159483,19.0578739552925,
16.4779769208372));
#201676=CARTESIAN_POINT('Ctrl Pts',(-20.8502336389588,19.1446700912249,
16.483460184015));
#201677=CARTESIAN_POINT('Ctrl Pts',(-20.8510257892714,19.1786565838585,
16.4856277414618));
#201678=CARTESIAN_POINT('Ctrl Pts',(-20.8508977921363,19.3432687474514,
16.496218955091));
#201679=CARTESIAN_POINT('Ctrl Pts',(-20.8387067175164,19.4735944789054,
16.5049104950054));
#201680=CARTESIAN_POINT('Ctrl Pts',(-20.7970384800906,19.695346905119,16.5197604038486));
#201681=CARTESIAN_POINT('Ctrl Pts',(-20.7732180830191,19.787466454308,16.5259401923999));
#201682=CARTESIAN_POINT('Ctrl Pts',(-20.7402342477503,19.8868749495494,
16.5324112593424));
#201683=CARTESIAN_POINT('Ctrl Pts',(-20.7371210656065,19.896046574314,16.5330063461856));
#201684=CARTESIAN_POINT('Ctrl Pts',(-20.7324307951557,19.9095590020489,
16.5338798603169));
#201685=CARTESIAN_POINT('Ctrl Pts',(-20.7309023232884,19.9139163780622,
16.5341610472707));
#201686=CARTESIAN_POINT('Ctrl Pts',(-20.728165063313,19.9216387860185,16.5346584573051));
#201687=CARTESIAN_POINT('Ctrl Pts',(-20.726961996427,19.9250057880776,16.5348750146441));
#201688=CARTESIAN_POINT('Ctrl Pts',(-20.7247001936944,19.9312855986208,
16.5352783186923));
#201689=CARTESIAN_POINT('Ctrl Pts',(-20.7236436008293,19.9341991058504,
16.5354651930116));
#201690=CARTESIAN_POINT('Ctrl Pts',(-20.7225806064499,19.9371103026755,
16.5356516909487));
#201691=CARTESIAN_POINT('Origin',(-18.734,19.211,0.));
#201692=CARTESIAN_POINT('',(-20.722580618353,19.9371102700768,17.5536949396865));
#201693=CARTESIAN_POINT('',(-20.7225806054526,19.9371103054067,17.3329786569753));
#201694=CARTESIAN_POINT('',(-20.7225806064498,19.9371103026755,0.));
#201695=CARTESIAN_POINT('',(-20.8509990201954,19.2127872399449,17.5117108857594));
#201696=CARTESIAN_POINT('Ctrl Pts',(-20.722580618353,19.9371102700768,17.5536949396865));
#201697=CARTESIAN_POINT('Ctrl Pts',(-20.7266413316867,19.9259892927749,
17.5529480158583));
#201698=CARTESIAN_POINT('Ctrl Pts',(-20.7306095645022,19.9148320356873,
17.5522050109842));
#201699=CARTESIAN_POINT('Ctrl Pts',(-20.7395308685426,19.8890654862418,
17.5505046497996));
#201700=CARTESIAN_POINT('Ctrl Pts',(-20.7444177097079,19.8744361555218,
17.549550649084));
#201701=CARTESIAN_POINT('Ctrl Pts',(-20.7509063836573,19.8542811970314,
17.5482531686163));
#201702=CARTESIAN_POINT('Ctrl Pts',(-20.7526460934486,19.8488009172698,
17.5479020745191));
#201703=CARTESIAN_POINT('Ctrl Pts',(-20.7553799364389,19.8400657627298,
17.5473452367977));
#201704=CARTESIAN_POINT('Ctrl Pts',(-20.7563885709251,19.8368155078355,
17.5471386545693));
#201705=CARTESIAN_POINT('Ctrl Pts',(-20.758459556094,19.8300846056304,17.5467121308139));
#201706=CARTESIAN_POINT('Ctrl Pts',(-20.7595207706185,19.8266036477637,
17.5464922617105));
#201707=CARTESIAN_POINT('Ctrl Pts',(-20.7620345457301,19.8182811796242,
17.5459682526278));
#201708=CARTESIAN_POINT('Ctrl Pts',(-20.7634787639705,19.8134371316568,
17.5456645993725));
#201709=CARTESIAN_POINT('Ctrl Pts',(-20.7683204546765,19.7969826202226,
17.5446375424508));
#201710=CARTESIAN_POINT('Ctrl Pts',(-20.7716358259506,19.7853479778766,
17.5439187643947));
#201711=CARTESIAN_POINT('Ctrl Pts',(-20.7896326232094,19.7200738513861,
17.5399243904783));
#201712=CARTESIAN_POINT('Ctrl Pts',(-20.8022969819697,19.6658959757595,
17.536752744696));
#201713=CARTESIAN_POINT('Ctrl Pts',(-20.8381002120249,19.4799544656379,
17.5261607586984));
#201714=CARTESIAN_POINT('Ctrl Pts',(-20.8508862152965,19.3465296112034,
17.519037359307));
#201715=CARTESIAN_POINT('Ctrl Pts',(-20.8509992439645,19.2127891489275,
17.5117113811062));
#201716=CARTESIAN_POINT('Ctrl Pts',(-20.8509992455948,19.212787218789,17.5117112753779));
#201717=CARTESIAN_POINT('Ctrl Pts',(-20.8510695258044,19.1295387930481,
17.5071511275068));
#201718=CARTESIAN_POINT('Ctrl Pts',(-20.8462293912133,19.0463633492458,
17.5025270677366));
#201719=CARTESIAN_POINT('Ctrl Pts',(-20.8325134454039,18.9297566661536,
17.4958024627517));
#201720=CARTESIAN_POINT('Ctrl Pts',(-20.8277010588129,18.895925120176,17.4938229102094));
#201721=CARTESIAN_POINT('Ctrl Pts',(-20.8203844052654,18.8521210862257,
17.4912165343719));
#201722=CARTESIAN_POINT('Ctrl Pts',(-20.8186232314416,18.8420285394258,
17.4906130217416));
#201723=CARTESIAN_POINT('Ctrl Pts',(-20.8155220286154,18.8249882045327,
17.489588800915));
#201724=CARTESIAN_POINT('Ctrl Pts',(-20.8142202866628,18.8180335650957,
17.4891693060336));
#201725=CARTESIAN_POINT('Ctrl Pts',(-20.8115755295169,18.8042852649797,
17.4883370327338));
#201726=CARTESIAN_POINT('Ctrl Pts',(-20.8102339941972,18.7974914074432,
17.4879243060368));
#201727=CARTESIAN_POINT('Ctrl Pts',(-20.8075793288925,18.7843862130888,
17.4871253128691));
#201728=CARTESIAN_POINT('Ctrl Pts',(-20.806270655976,18.7780740440354,17.4867391930152));
#201729=CARTESIAN_POINT('Ctrl Pts',(-20.8031923941714,18.7635603597318,
17.4858483855784));
#201730=CARTESIAN_POINT('Ctrl Pts',(-20.8014028458251,18.7553632305344,
17.4853430629542));
#201731=CARTESIAN_POINT('Ctrl Pts',(-20.7964824081128,18.7334508131591,
17.4839862327915));
#201732=CARTESIAN_POINT('Ctrl Pts',(-20.7932634947401,18.7197559121355,
17.483131911935));
#201733=CARTESIAN_POINT('Ctrl Pts',(-20.7650016192786,18.6046773257395,
17.4758985085358));
#201734=CARTESIAN_POINT('Ctrl Pts',(-20.7326286782233,18.5052574780061,
17.4692808211591));
#201735=CARTESIAN_POINT('Ctrl Pts',(-20.6611667090069,18.3307737651146,
17.4570259400451));
#201736=CARTESIAN_POINT('Ctrl Pts',(-20.6246612391262,18.2548783344609,
17.4514610948834));
#201737=CARTESIAN_POINT('Ctrl Pts',(-20.5387681077716,18.100572081465,17.4397939993481));
#201738=CARTESIAN_POINT('Ctrl Pts',(-20.4885501277334,18.0228104374067,
17.4337049592147));
#201739=CARTESIAN_POINT('Ctrl Pts',(-20.4146638440853,17.9233487510274,
17.4258399888688));
#201740=CARTESIAN_POINT('Ctrl Pts',(-20.3953620683474,17.8985393271178,
17.4238717384569));
#201741=CARTESIAN_POINT('Ctrl Pts',(-20.3709897443403,17.8686122375115,
17.4214987552279));
#201742=CARTESIAN_POINT('Ctrl Pts',(-20.3664373888904,17.8630799346069,
17.4210601439086));
#201743=CARTESIAN_POINT('Ctrl Pts',(-20.3592401808988,17.8544233866523,
17.4203740723007));
#201744=CARTESIAN_POINT('Ctrl Pts',(-20.3566142520256,17.851283579834,17.4201252772176));
#201745=CARTESIAN_POINT('Ctrl Pts',(-20.3516781455532,17.84541617114,17.4196604748008));
#201746=CARTESIAN_POINT('Ctrl Pts',(-20.3493701927867,17.8426868352907,
17.419444318196));
#201747=CARTESIAN_POINT('Ctrl Pts',(-20.3440718016724,17.8364531598767,
17.4189507348051));
#201748=CARTESIAN_POINT('Ctrl Pts',(-20.3410768354129,17.8329527336724,
17.41867364574));
#201749=CARTESIAN_POINT('Ctrl Pts',(-20.3332062439371,17.8238143793443,
17.4179503781609));
#201750=CARTESIAN_POINT('Ctrl Pts',(-20.328312179245,17.8181923192279,17.4175055251567));
#201751=CARTESIAN_POINT('Ctrl Pts',(-20.2954412706125,17.7808321234847,
17.4145491856431));
#201752=CARTESIAN_POINT('Ctrl Pts',(-20.2665460195083,17.7499105996997,
17.4121015032233));
#201753=CARTESIAN_POINT('Ctrl Pts',(-20.1846540736877,17.6673807644727,
17.4054976604523));
#201754=CARTESIAN_POINT('Ctrl Pts',(-20.1298485030154,17.6176494414284,
17.4014360247064));
#201755=CARTESIAN_POINT('Ctrl Pts',(-20.0033179293491,17.5143838268614,
17.3925359590513));
#201756=CARTESIAN_POINT('Ctrl Pts',(-19.9305795752396,17.4623229092268,
17.3877189274544));
#201757=CARTESIAN_POINT('Ctrl Pts',(-19.7945061473346,17.3774074393543,
17.3788987899348));
#201758=CARTESIAN_POINT('Ctrl Pts',(-19.7323923789462,17.3428601679122,
17.374937965075));
#201759=CARTESIAN_POINT('Ctrl Pts',(-19.6443228075205,17.2995248416322,
17.3693227495859));
#201760=CARTESIAN_POINT('Ctrl Pts',(-19.6197553696905,17.2880173618407,
17.3677567025062));
#201761=CARTESIAN_POINT('Ctrl Pts',(-19.5768209842197,17.2689040594172,
17.3650161569712));
#201762=CARTESIAN_POINT('Ctrl Pts',(-19.5585552173372,17.2610788457664,
17.3638491100963));
#201763=CARTESIAN_POINT('Ctrl Pts',(-19.5321199541511,17.2501916033565,
17.3621573736208));
#201764=CARTESIAN_POINT('Ctrl Pts',(-19.5240371149384,17.2469209834848,
17.3616397490928));
#201765=CARTESIAN_POINT('Ctrl Pts',(-19.5098882815928,17.2412973054451,
17.3607329365963));
#201766=CARTESIAN_POINT('Ctrl Pts',(-19.5038311777474,17.2389220890745,
17.3603445013724));
#201767=CARTESIAN_POINT('Ctrl Pts',(-19.4921774263775,17.234414089723,17.3595966801764));
#201768=CARTESIAN_POINT('Ctrl Pts',(-19.4865824809732,17.2322770586158,
17.3592374414597));
#201769=CARTESIAN_POINT('Ctrl Pts',(-19.4719319566534,17.2267523069803,
17.3582961759277));
#201770=CARTESIAN_POINT('Ctrl Pts',(-19.4628621817998,17.223402858979,17.357712875464));
#201771=CARTESIAN_POINT('Ctrl Pts',(-19.4314552563128,17.2120482265024,
17.3556908127909));
#201772=CARTESIAN_POINT('Ctrl Pts',(-19.4090073084605,17.2043567609148,
17.3542416968103));
#201773=CARTESIAN_POINT('Ctrl Pts',(-19.2315960822488,17.1468831061675,
17.3427547134132));
#201774=CARTESIAN_POINT('Ctrl Pts',(-19.07151605238,17.1147546816393,17.3321225323069));
#201775=CARTESIAN_POINT('Ctrl Pts',(-18.7800578764075,17.0905271206785,
17.3127961273034));
#201776=CARTESIAN_POINT('Ctrl Pts',(-18.6500163194528,17.0916887461439,
17.3042053638423));
#201777=CARTESIAN_POINT('Ctrl Pts',(-18.5090085419455,17.1059559518949,
17.2954160528913));
#201778=CARTESIAN_POINT('Ctrl Pts',(-18.4971377171314,17.1072586008024,
17.2946803677359));
#201779=CARTESIAN_POINT('Ctrl Pts',(-18.4802847913946,17.1092524232285,
17.2936425705466));
#201780=CARTESIAN_POINT('Ctrl Pts',(-18.4752934025745,17.1098609800424,
17.2933360330874));
#201781=CARTESIAN_POINT('Ctrl Pts',(-18.4666980282372,17.1109400329748,
17.2928096501668));
#201782=CARTESIAN_POINT('Ctrl Pts',(-18.4630930146798,17.1114020348425,
17.2925893299845));
#201783=CARTESIAN_POINT('Ctrl Pts',(-18.4561076967961,17.1123155316816,
17.2921633184898));
#201784=CARTESIAN_POINT('Ctrl Pts',(-18.4527272938496,17.1127659103674,
17.291957563008));
#201785=CARTESIAN_POINT('Ctrl Pts',(-18.4436144981057,17.1140024467796,
17.2914039477744));
#201786=CARTESIAN_POINT('Ctrl Pts',(-18.4378841668616,17.1148039468894,
17.2910569481935));
#201787=CARTESIAN_POINT('Ctrl Pts',(-18.4166551314657,17.1178620368697,
17.289775364405));
#201788=CARTESIAN_POINT('Ctrl Pts',(-18.4011778915775,17.1202671680025,
17.2888488011517));
#201789=CARTESIAN_POINT('Ctrl Pts',(-18.252272384081,17.1451022749719,17.2799972890781));
#201790=CARTESIAN_POINT('Ctrl Pts',(-18.1212383384864,17.1801065615635,
17.2726831911094));
#201791=CARTESIAN_POINT('Ctrl Pts',(-17.8484332178777,17.2818193034361,
17.2568724230478));
#201792=CARTESIAN_POINT('Ctrl Pts',(-17.7089125452259,17.3521953041116,
17.2483887314886));
#201793=CARTESIAN_POINT('Ctrl Pts',(-17.5605579158077,17.4488492587841,
17.2380771526044));
#201794=CARTESIAN_POINT('Ctrl Pts',(-17.542910159438,17.4607295915006,17.2368287834525));
#201795=CARTESIAN_POINT('Ctrl Pts',(-17.5180639563392,17.4780056680327,
17.2350386133694));
#201796=CARTESIAN_POINT('Ctrl Pts',(-17.5107158709621,17.4831846878929,
17.2345050512705));
#201797=CARTESIAN_POINT('Ctrl Pts',(-17.4980935244035,17.4922019518258,
17.2335812464766));
#201798=CARTESIAN_POINT('Ctrl Pts',(-17.4928035672132,17.4960180873847,
17.2331918580774));
#201799=CARTESIAN_POINT('Ctrl Pts',(-17.4827067162483,17.5033730656228,
17.2324443210061));
#201800=CARTESIAN_POINT('Ctrl Pts',(-17.4778969808966,17.5069079152705,
17.2320863297524));
#201801=CARTESIAN_POINT('Ctrl Pts',(-17.4654245909403,17.5161558223313,
17.2311530223009));
#201802=CARTESIAN_POINT('Ctrl Pts',(-17.4577856266262,17.5219004696122,
17.2305764741588));
#201803=CARTESIAN_POINT('Ctrl Pts',(-17.4318476333021,17.541682738521,17.2286017440046));
#201804=CARTESIAN_POINT('Ctrl Pts',(-17.4137397196967,17.5559671810501,
17.2271938462437));
#201805=CARTESIAN_POINT('Ctrl Pts',(-17.2606301533132,17.6808596672632,
17.2150311543126));
#201806=CARTESIAN_POINT('Ctrl Pts',(-17.139575770845,17.807455753402,17.2035813786229));
#201807=CARTESIAN_POINT('Ctrl Pts',(-16.9831079609131,18.0177877742928,
17.1862602023824));
#201808=CARTESIAN_POINT('Ctrl Pts',(-16.9351878379651,18.0913325993497,
17.1804793097828));
#201809=CARTESIAN_POINT('Ctrl Pts',(-16.8732399865028,18.2007006882016,
17.1724531482782));
#201810=CARTESIAN_POINT('Ctrl Pts',(-16.8554068138177,18.2342602274371,
17.1700629668203));
#201811=CARTESIAN_POINT('Ctrl Pts',(-16.8351093785287,18.2750721788775,
17.1672580674368));
#201812=CARTESIAN_POINT('Ctrl Pts',(-16.8317697243615,18.2818786617992,
17.166793611509));
#201813=CARTESIAN_POINT('Ctrl Pts',(-16.8266436821056,18.2924694422797,
17.1660762598677));
#201814=CARTESIAN_POINT('Ctrl Pts',(-16.8248318664517,18.296241262725,17.1658218251893));
#201815=CARTESIAN_POINT('Ctrl Pts',(-16.8214977704639,18.3032352061702,
17.1653520020817));
#201816=CARTESIAN_POINT('Ctrl Pts',(-16.8199724555475,18.3064557731787,
17.165136430739));
#201817=CARTESIAN_POINT('Ctrl Pts',(-16.816549056206,18.3137314094614,17.1646511591042));
#201818=CARTESIAN_POINT('Ctrl Pts',(-16.814655704842,18.317788646,17.164381752898));
#201819=CARTESIAN_POINT('Ctrl Pts',(-16.8091243790593,18.3297404459087,
17.1635915853232));
#201820=CARTESIAN_POINT('Ctrl Pts',(-16.8055220882627,18.3376515543186,
17.1630729720515));
#201821=CARTESIAN_POINT('Ctrl Pts',(-16.7804016249692,18.3937327552829,
17.1594261287749));
#201822=CARTESIAN_POINT('Ctrl Pts',(-16.7606401043972,18.4426745011667,
17.1563970382605));
#201823=CARTESIAN_POINT('Ctrl Pts',(-16.7373109645124,18.5073123117826,
17.1525305064271));
#201824=CARTESIAN_POINT('Ctrl Pts',(-16.7320651426583,18.5223779613646,
17.1516385895809));
#201825=CARTESIAN_POINT('Ctrl Pts',(-16.7108725009644,18.585531565523,17.147933023092));
#201826=CARTESIAN_POINT('Ctrl Pts',(-16.6964837281179,18.6341261617481,
17.1451614273198));
#201827=CARTESIAN_POINT('Ctrl Pts',(-16.6565747464857,18.7891432622963,
17.1364461509989));
#201828=CARTESIAN_POINT('Ctrl Pts',(-16.6375523632505,18.8970490160094,
17.1305552825568));
#201829=CARTESIAN_POINT('Ctrl Pts',(-16.6216102414295,19.0608561422268,
17.1214044868495));
#201830=CARTESIAN_POINT('Ctrl Pts',(-16.6184148836214,19.1159598080599,
17.1182932675612));
#201831=CARTESIAN_POINT('Ctrl Pts',(-16.61672878575,19.205455191344,17.1131436738121));
#201832=CARTESIAN_POINT('Ctrl Pts',(-16.6169174114437,19.2397968004508,
17.1111447992172));
#201833=CARTESIAN_POINT('Ctrl Pts',(-16.6182634819072,19.2849249316174,
17.1084821365268));
#201834=CARTESIAN_POINT('Ctrl Pts',(-16.6186686401239,19.2957298109645,
17.1078419222804));
#201835=CARTESIAN_POINT('Ctrl Pts',(-16.6194678656833,19.3134228906346,
17.1067889605801));
#201836=CARTESIAN_POINT('Ctrl Pts',(-16.6198128701462,19.3203131913915,
17.1063777558761));
#201837=CARTESIAN_POINT('Ctrl Pts',(-16.6205459420015,19.3336484054593,
17.1055796613158));
#201838=CARTESIAN_POINT('Ctrl Pts',(-16.6209298263292,19.3400934790852,
17.105192907166));
#201839=CARTESIAN_POINT('Ctrl Pts',(-16.6218843586192,19.3549721062545,
17.104297663796));
#201840=CARTESIAN_POINT('Ctrl Pts',(-16.6224760433415,19.3634041573075,
17.1037885190704));
#201841=CARTESIAN_POINT('Ctrl Pts',(-16.6242033358871,19.3860744131268,
17.1024147259844));
#201842=CARTESIAN_POINT('Ctrl Pts',(-16.6254325547246,19.4003048521906,
17.1015471529727));
#201843=CARTESIAN_POINT('Ctrl Pts',(-16.6403646641977,19.5549069822277,
17.0920633076009));
#201844=CARTESIAN_POINT('Ctrl Pts',(-16.6679158734398,19.6935598094669,
17.0829974680668));
#201845=CARTESIAN_POINT('Ctrl Pts',(-16.7372099462143,19.9208242679886,
17.0673666161625));
#201846=CARTESIAN_POINT('Ctrl Pts',(-16.7716755157006,20.0111898685889,
17.0609407118479));
#201847=CARTESIAN_POINT('Ctrl Pts',(-16.832738690007,20.143359639222,17.0514397387777));
#201848=CARTESIAN_POINT('Ctrl Pts',(-16.8548246766492,20.1871095245703,
17.048278174716));
#201849=CARTESIAN_POINT('Ctrl Pts',(-16.8910509596667,20.2530736162929,
17.0435258520863));
#201850=CARTESIAN_POINT('Ctrl Pts',(-16.9041195477913,20.2758550438793,
17.0418874260181));
#201851=CARTESIAN_POINT('Ctrl Pts',(-16.921081490268,20.3041885347935,17.0398589111108));
#201852=CARTESIAN_POINT('Ctrl Pts',(-16.9245814732206,20.3099719256345,
17.039445345445));
#201853=CARTESIAN_POINT('Ctrl Pts',(-16.930198322323,20.3191536604977,17.0387896766877));
#201854=CARTESIAN_POINT('Ctrl Pts',(-16.9322971956717,20.3225628786332,
17.0385464250224));
#201855=CARTESIAN_POINT('Ctrl Pts',(-16.9362980700381,20.32902042937,17.0380860843603));
#201856=CARTESIAN_POINT('Ctrl Pts',(-16.9381981361603,20.3320698352292,
17.0378688803502));
#201857=CARTESIAN_POINT('Ctrl Pts',(-16.9425919068582,20.3390815402062,
17.037369838551));
#201858=CARTESIAN_POINT('Ctrl Pts',(-16.9450909970951,20.3430404135086,
17.0370883604774));
#201859=CARTESIAN_POINT('Ctrl Pts',(-16.951828846634,20.3536359838918,17.0363356854586));
#201860=CARTESIAN_POINT('Ctrl Pts',(-16.9560915842328,20.3602574476933,
17.0358660325559));
#201861=CARTESIAN_POINT('Ctrl Pts',(-16.9884189013182,20.4098622928407,
17.0323517870805));
#201862=CARTESIAN_POINT('Ctrl Pts',(-17.0180040786294,20.4518396696527,
17.0294014473958));
#201863=CARTESIAN_POINT('Ctrl Pts',(-17.0626484294944,20.5105285820624,
17.0252474284108));
#201864=CARTESIAN_POINT('Ctrl Pts',(-17.0764904465676,20.5281380858821,
17.0239970768856));
#201865=CARTESIAN_POINT('Ctrl Pts',(-17.1195404441598,20.5811516675939,
17.0202098749172));
#201866=CARTESIAN_POINT('Ctrl Pts',(-17.1496229850703,20.6158291585129,
17.0177003067727));
#201867=CARTESIAN_POINT('Ctrl Pts',(-17.2551144918941,20.7297312272389,
17.0092479120587));
#201868=CARTESIAN_POINT('Ctrl Pts',(-17.3355231997998,20.8040814927553,
17.0033597070467));
#201869=CARTESIAN_POINT('Ctrl Pts',(-17.4645504801973,20.906058803431,16.9942151039222));
#201870=CARTESIAN_POINT('Ctrl Pts',(-17.5091044536831,20.9385290693859,
16.9911074345531));
#201871=CARTESIAN_POINT('Ctrl Pts',(-17.583366686089,20.9883320114188,16.9859631927978));
#201872=CARTESIAN_POINT('Ctrl Pts',(-17.6123201583285,21.0067450370439,
16.9839660126999));
#201873=CARTESIAN_POINT('Ctrl Pts',(-17.6509662659385,21.0300227504618,
16.981305287538));
#201874=CARTESIAN_POINT('Ctrl Pts',(-17.6602678723747,21.0355287466519,
16.980665272561));
#201875=CARTESIAN_POINT('Ctrl Pts',(-17.6755740106148,21.0444314850177,
16.979612555143));
#201876=CARTESIAN_POINT('Ctrl Pts',(-17.6815537746091,21.047870579597,16.9792013940473));
#201877=CARTESIAN_POINT('Ctrl Pts',(-17.6931630156139,21.0544720129312,
16.9784033244816));
#201878=CARTESIAN_POINT('Ctrl Pts',(-17.6987903681982,21.0576379470049,
16.978016551402));
#201879=CARTESIAN_POINT('Ctrl Pts',(-17.711819513031,21.0648898384521,16.9771211773324));
#201880=CARTESIAN_POINT('Ctrl Pts',(-17.7192314379364,21.0689572770288,
16.9766119202343));
#201881=CARTESIAN_POINT('Ctrl Pts',(-17.7392357645613,21.0797796315547,
16.975237627312));
#201882=CARTESIAN_POINT('Ctrl Pts',(-17.7518723558361,21.0864515377035,
16.9743696635239));
#201883=CARTESIAN_POINT('Ctrl Pts',(-17.868436067835,21.1464940726931,16.9663635436742));
#201884=CARTESIAN_POINT('Ctrl Pts',(-17.9765299840583,21.191295330932,16.9589237105708));
#201885=CARTESIAN_POINT('Ctrl Pts',(-18.2426496289494,21.2766047339658,
16.9406697243583));
#201886=CARTESIAN_POINT('Ctrl Pts',(-18.4027502413841,21.3082414656108,
16.9297156680553));
#201887=CARTESIAN_POINT('Ctrl Pts',(-18.5973698628822,21.3238375975069,
16.9173086143513));
#201888=CARTESIAN_POINT('Ctrl Pts',(-18.6299044169844,21.3256902580934,
16.9152664910865));
#201889=CARTESIAN_POINT('Ctrl Pts',(-18.6697112111448,21.3270360195069,
16.9128172364443));
#201890=CARTESIAN_POINT('Ctrl Pts',(-18.6769530041953,21.3272436362545,
16.9123736544594));
#201891=CARTESIAN_POINT('Ctrl Pts',(-18.6883054688174,21.3275107862288,
16.9116815586666));
#201892=CARTESIAN_POINT('Ctrl Pts',(-18.6924154112572,21.3275955260858,
16.9114316717471));
#201893=CARTESIAN_POINT('Ctrl Pts',(-18.7000967838712,21.3277315203358,
16.9109659307326));
#201894=CARTESIAN_POINT('Ctrl Pts',(-18.703668057698,21.3277857073295,16.9107499207706));
#201895=CARTESIAN_POINT('Ctrl Pts',(-18.7118188566586,21.3278887477691,
16.9102580985994));
#201896=CARTESIAN_POINT('Ctrl Pts',(-18.7163984049109,21.3279317793226,
16.9099826150137));
#201897=CARTESIAN_POINT('Ctrl Pts',(-18.7304690043151,21.3280183307256,
16.9091387027651));
#201898=CARTESIAN_POINT('Ctrl Pts',(-18.739960387906,21.3280128865746,16.9085729428504));
#201899=CARTESIAN_POINT('Ctrl Pts',(-18.8248973036766,21.3273929303706,
16.903538866284));
#201900=CARTESIAN_POINT('Ctrl Pts',(-18.9002684909403,21.3228093449835,
16.8992745218673));
#201901=CARTESIAN_POINT('Ctrl Pts',(-19.0180313935093,21.3093017471572,
16.8927122355578));
#201902=CARTESIAN_POINT('Ctrl Pts',(-19.0606625734108,21.3030888626568,
16.89035771035));
#201903=CARTESIAN_POINT('Ctrl Pts',(-19.2107257497164,21.2765201275709,
16.8820607041474));
#201904=CARTESIAN_POINT('Ctrl Pts',(-19.3167367988922,21.2491505769794,
16.8761738528689));
#201905=CARTESIAN_POINT('Ctrl Pts',(-19.4722619360478,21.1958657558821,
16.8670323969262));
#201906=CARTESIAN_POINT('Ctrl Pts',(-19.5236483769392,21.1759879265342,
16.8639265314401));
#201907=CARTESIAN_POINT('Ctrl Pts',(-19.6056761109337,21.1405195838339,
16.8587850095325));
#201908=CARTESIAN_POINT('Ctrl Pts',(-19.636816585931,21.1261467522292,16.8567886907969));
#201909=CARTESIAN_POINT('Ctrl Pts',(-19.6772926677318,21.1062584893208,
16.8541289505809));
#201910=CARTESIAN_POINT('Ctrl Pts',(-19.6869555537995,21.1014183410733,
16.8534890369579));
#201911=CARTESIAN_POINT('Ctrl Pts',(-19.7027243664439,21.0933681047734,
16.8524364437869));
#201912=CARTESIAN_POINT('Ctrl Pts',(-19.7088524881154,21.0902017466717,
16.8520253048699));
#201913=CARTESIAN_POINT('Ctrl Pts',(-19.7206868970349,21.0840135236379,
16.8512272479995));
#201914=CARTESIAN_POINT('Ctrl Pts',(-19.7263950550936,21.0809953865461,
16.8508404652758));
#201915=CARTESIAN_POINT('Ctrl Pts',(-19.7395461228862,21.0739647048852,
16.8499450246546));
#201916=CARTESIAN_POINT('Ctrl Pts',(-19.7469789411445,21.0699336078668,
16.8494357103421));
#201917=CARTESIAN_POINT('Ctrl Pts',(-19.7669104048741,21.0589689887334,
16.848061162904));
#201918=CARTESIAN_POINT('Ctrl Pts',(-19.7793631444333,21.0519533313886,
16.847193000127));
#201919=CARTESIAN_POINT('Ctrl Pts',(-19.8931592602747,20.9863156852671,
16.8391715748319));
#201920=CARTESIAN_POINT('Ctrl Pts',(-19.9895309153828,20.9195169718493,
16.8317152957038));
#201921=CARTESIAN_POINT('Ctrl Pts',(-20.2060400843744,20.7411966124897,
16.8133923465813));
#201922=CARTESIAN_POINT('Ctrl Pts',(-20.3197428723568,20.6230281197913,
16.802383734368));
#201923=CARTESIAN_POINT('Ctrl Pts',(-20.4378917579976,20.4677594710626,
16.7899959996778));
#201924=CARTESIAN_POINT('Ctrl Pts',(-20.4564984102092,20.4421340167836,
16.78801273413));
#201925=CARTESIAN_POINT('Ctrl Pts',(-20.4786120200789,20.4101953407588,
16.7856242240604));
#201926=CARTESIAN_POINT('Ctrl Pts',(-20.4826697620295,20.404270561386,16.7851845853515));
#201927=CARTESIAN_POINT('Ctrl Pts',(-20.4889950222431,20.3949333829763,
16.7844972683068));
#201928=CARTESIAN_POINT('Ctrl Pts',(-20.4912828720863,20.3915349175494,
16.7842482472938));
#201929=CARTESIAN_POINT('Ctrl Pts',(-20.4955480358932,20.3851593969218,
16.7837832521015));
#201930=CARTESIAN_POINT('Ctrl Pts',(-20.4975276542473,20.3821840099075,
16.7835671272824));
#201931=CARTESIAN_POINT('Ctrl Pts',(-20.5020387383687,20.3753664326526,
16.7830739149219));
#201932=CARTESIAN_POINT('Ctrl Pts',(-20.5045652144511,20.3715210003067,
16.7827971631906));
#201933=CARTESIAN_POINT('Ctrl Pts',(-20.5111412917283,20.3614403959901,
16.7820753549154));
#201934=CARTESIAN_POINT('Ctrl Pts',(-20.5151706592888,20.3551920125831,
16.7816316151908));
#201935=CARTESIAN_POINT('Ctrl Pts',(-20.5417145229974,20.3135501301173,
16.7786977146286));
#201936=CARTESIAN_POINT('Ctrl Pts',(-20.5632073643183,20.2775127907092,
16.7762702620137));
#201937=CARTESIAN_POINT('Ctrl Pts',(-20.5941806202874,20.2218850718296,
16.7726525679296));
#201938=CARTESIAN_POINT('Ctrl Pts',(-20.6044523717743,20.2027502432319,
16.7714306122185));
#201939=CARTESIAN_POINT('Ctrl Pts',(-20.6222715811604,20.1682935721515,
16.7692641207855));
#201940=CARTESIAN_POINT('Ctrl Pts',(-20.6299313569032,20.1530323012153,
16.7683162021039));
#201941=CARTESIAN_POINT('Ctrl Pts',(-20.6692389896475,20.0722941905844,
16.7633540472585));
#201942=CARTESIAN_POINT('Ctrl Pts',(-20.6976644695323,20.0053475411258,
16.7594186685798));
#201943=CARTESIAN_POINT('Ctrl Pts',(-20.7225806782305,19.9371101060915,
16.7554729098499));
#201944=CARTESIAN_POINT('',(-20.8509999221906,19.2115739728967,17.290908287241));
#201945=CARTESIAN_POINT('Ctrl Pts',(-20.7225806064499,19.9371103026755,
16.5356516909487));
#201946=CARTESIAN_POINT('Ctrl Pts',(-20.7222420517169,19.9380374942795,
16.5357110889667));
#201947=CARTESIAN_POINT('Ctrl Pts',(-20.7219028476344,19.9389644515232,
16.5357704488057));
#201948=CARTESIAN_POINT('Ctrl Pts',(-20.7191070447656,19.9465881332496,
16.5362584608096));
#201949=CARTESIAN_POINT('Ctrl Pts',(-20.7166172235478,19.9532727457913,
16.5366851668454));
#201950=CARTESIAN_POINT('Ctrl Pts',(-20.7031297565641,19.9889315139748,
16.5389556645996));
#201951=CARTESIAN_POINT('Ctrl Pts',(-20.6915300434208,20.0176757689274,
16.5407655708978));
#201952=CARTESIAN_POINT('Ctrl Pts',(-20.6147735820571,20.196462055387,16.5519561572183));
#201953=CARTESIAN_POINT('Ctrl Pts',(-20.5330352019228,20.3387984850848,
16.5606012946165));
#201954=CARTESIAN_POINT('Ctrl Pts',(-20.365712353063,20.5649020204647,16.5759958048462));
#201955=CARTESIAN_POINT('Ctrl Pts',(-20.2879589469206,20.6534777757539,
16.5825622185153));
#201956=CARTESIAN_POINT('Ctrl Pts',(-20.1929613282677,20.7450551973625,
16.5902922217907));
#201957=CARTESIAN_POINT('Ctrl Pts',(-20.1825655610694,20.754875417991,16.5911343486701));
#201958=CARTESIAN_POINT('Ctrl Pts',(-20.1658644156388,20.7703347394152,
16.5924817339191));
#201959=CARTESIAN_POINT('Ctrl Pts',(-20.1596232413558,20.7760427805206,
16.5929840455174));
#201960=CARTESIAN_POINT('Ctrl Pts',(-20.1485570613111,20.7860425446627,
16.5938726688127));
#201961=CARTESIAN_POINT('Ctrl Pts',(-20.1437462830484,20.7903499020825,
16.5942583134681));
#201962=CARTESIAN_POINT('Ctrl Pts',(-20.1337566230684,20.7992121910514,
16.5950577828901));
#201963=CARTESIAN_POINT('Ctrl Pts',(-20.1285750439512,20.8037639538443,
16.5954717334905));
#201964=CARTESIAN_POINT('Ctrl Pts',(-20.1152202468021,20.8153803600855,
16.5965368249411));
#201965=CARTESIAN_POINT('Ctrl Pts',(-20.1070151002742,20.8224078433618,
16.5971894929732));
#201966=CARTESIAN_POINT('Ctrl Pts',(-20.0725673194657,20.8514573043545,
16.5999227642694));
#201967=CARTESIAN_POINT('Ctrl Pts',(-20.0458470612861,20.8729024365244,
16.6020266394149));
#201968=CARTESIAN_POINT('Ctrl Pts',(-19.9749015891035,20.9270645174338,
16.6075744238814));
#201969=CARTESIAN_POINT('Ctrl Pts',(-19.9299029338047,20.9587212415474,
16.611056603408));
#201970=CARTESIAN_POINT('Ctrl Pts',(-19.8068132698785,21.038334370842,16.6204783693331));
#201971=CARTESIAN_POINT('Ctrl Pts',(-19.7267584986212,21.0830329964801,
16.6265051250854));
#201972=CARTESIAN_POINT('Ctrl Pts',(-19.5956079726278,21.1454770180192,
16.6361029179627));
#201973=CARTESIAN_POINT('Ctrl Pts',(-19.5462882637157,21.1666987433982,
16.6396529510337));
#201974=CARTESIAN_POINT('Ctrl Pts',(-19.4618372415616,21.1992906688597,
16.6455883741705));
#201975=CARTESIAN_POINT('Ctrl Pts',(-19.4271177968148,21.2116585821317,
16.6479889020655));
#201976=CARTESIAN_POINT('Ctrl Pts',(-19.3471103119782,21.2378262221791,
16.6534068325898));
#201977=CARTESIAN_POINT('Ctrl Pts',(-19.3016440361817,21.2510269091692,
16.6564042779727));
#201978=CARTESIAN_POINT('Ctrl Pts',(-19.2483037318369,21.2645919799044,
16.6597976700758));
#201979=CARTESIAN_POINT('Ctrl Pts',(-19.2408271465266,21.2664499741393,
16.6602705274235));
#201980=CARTESIAN_POINT('Ctrl Pts',(-19.2288395362173,21.2693596102613,
16.6610240447005));
#201981=CARTESIAN_POINT('Ctrl Pts',(-19.2243349937798,21.2704373130965,
16.6613061452149));
#201982=CARTESIAN_POINT('Ctrl Pts',(-19.2163364520529,21.2723232176344,
16.6618051608273));
#201983=CARTESIAN_POINT('Ctrl Pts',(-19.2128438940809,21.2731373345066,
16.6620224127647));
#201984=CARTESIAN_POINT('Ctrl Pts',(-19.2054208874389,21.2748477652032,
16.6624827774711));
#201985=CARTESIAN_POINT('Ctrl Pts',(-19.2014899512415,21.2757417265025,
16.6627257546235));
#201986=CARTESIAN_POINT('Ctrl Pts',(-19.1908386446496,21.2781320360373,
16.6633819839257));
#201987=CARTESIAN_POINT('Ctrl Pts',(-19.184113421763,21.279606852976,16.6637940182909));
#201988=CARTESIAN_POINT('Ctrl Pts',(-19.1502442975397,21.2868612357603,
16.6658580252429));
#201989=CARTESIAN_POINT('Ctrl Pts',(-19.1229944212617,21.292139758116,16.6674829968275));
#201990=CARTESIAN_POINT('Ctrl Pts',(-19.0432544637439,21.3059649611982,
16.6721551623251));
#201991=CARTESIAN_POINT('Ctrl Pts',(-18.9905343821223,21.3130721671704,
16.6751403830227));
#201992=CARTESIAN_POINT('Ctrl Pts',(-18.797470002405,21.331726311849,16.6858718161407));
#201993=CARTESIAN_POINT('Ctrl Pts',(-18.6563386417215,21.3312545783071,
16.6933556709626));
#201994=CARTESIAN_POINT('Ctrl Pts',(-18.4249190351338,21.3073293682037,
16.7062249140832));
#201995=CARTESIAN_POINT('Ctrl Pts',(-18.3342648253121,21.2919460974577,
16.7114159963734));
#201996=CARTESIAN_POINT('Ctrl Pts',(-18.2315114572506,21.2675465471129,
16.7176073324148));
#201997=CARTESIAN_POINT('Ctrl Pts',(-18.218151814816,21.2642362437222,16.7184182619345));
#201998=CARTESIAN_POINT('Ctrl Pts',(-18.1967880141909,21.2587209749307,
16.7197250009955));
#201999=CARTESIAN_POINT('Ctrl Pts',(-18.1887627598864,21.2565987528999,
16.7202181384911));
#202000=CARTESIAN_POINT('Ctrl Pts',(-18.1745411880844,21.2527483235335,
16.7210961367052));
#202001=CARTESIAN_POINT('Ctrl Pts',(-18.1683398432538,21.2510389615254,
16.7214803815956));
#202002=CARTESIAN_POINT('Ctrl Pts',(-18.1554407812215,21.2474200783434,
16.7222825707217));
#202003=CARTESIAN_POINT('Ctrl Pts',(-18.1487445125894,21.2455057182928,
16.7227006686577));
#202004=CARTESIAN_POINT('Ctrl Pts',(-18.1313907261432,21.2404517737632,
16.7237885635952));
#202005=CARTESIAN_POINT('Ctrl Pts',(-18.1207483627601,21.237261301269,16.724460015887));
#202006=CARTESIAN_POINT('Ctrl Pts',(-18.074747959663,21.2230752551771,16.7273812579463));
#202007=CARTESIAN_POINT('Ctrl Pts',(-18.0396584329149,21.2112373863709,
16.7296585095204));
#202008=CARTESIAN_POINT('Ctrl Pts',(-17.9473740482418,21.177383244029,16.7357823574816));
#202009=CARTESIAN_POINT('Ctrl Pts',(-17.8907970727781,21.1537946805069,
16.7396778781684));
#202010=CARTESIAN_POINT('Ctrl Pts',(-17.6945135637467,21.0617684287996,
16.7536785394432));
#202011=CARTESIAN_POINT('Ctrl Pts',(-17.5614180825771,20.98044103373,16.7641153034428));
#202012=CARTESIAN_POINT('Ctrl Pts',(-17.4260648076406,20.8757039401898,
16.7752422062864));
#202013=CARTESIAN_POINT('Ctrl Pts',(-17.4138001253349,20.8659942554115,
16.7762550795443));
#202014=CARTESIAN_POINT('Ctrl Pts',(-17.36384774033,20.8255393496894,16.7803961661011));
#202015=CARTESIAN_POINT('Ctrl Pts',(-17.3271142446875,20.793633187988,16.7834791138499));
#202016=CARTESIAN_POINT('Ctrl Pts',(-17.2858279037991,20.7551977985309,
16.7869573844483));
#202017=CARTESIAN_POINT('Ctrl Pts',(-17.2801751391209,20.7498770384019,
16.7874339089569));
#202018=CARTESIAN_POINT('Ctrl Pts',(-17.2711840645505,20.7413202773861,
16.7881921338877));
#202019=CARTESIAN_POINT('Ctrl Pts',(-17.2678269865608,20.7381042230305,
16.7884753028964));
#202020=CARTESIAN_POINT('Ctrl Pts',(-17.2618974317005,20.7323861788861,
16.7889755280837));
#202021=CARTESIAN_POINT('Ctrl Pts',(-17.2593206896836,20.7298886757621,
16.7891929268846));
#202022=CARTESIAN_POINT('Ctrl Pts',(-17.2538697539085,20.7245784176694,
16.7896528523257));
#202023=CARTESIAN_POINT('Ctrl Pts',(-17.2509972266505,20.7217640274666,
16.7898952471889));
#202024=CARTESIAN_POINT('Ctrl Pts',(-17.2432601359615,20.7141401969508,
16.7905482558267));
#202025=CARTESIAN_POINT('Ctrl Pts',(-17.2384107869143,20.7093152880961,
16.7909576721616));
#202026=CARTESIAN_POINT('Ctrl Pts',(-17.2143864470259,20.6851791761405,
16.7929871694037));
#202027=CARTESIAN_POINT('Ctrl Pts',(-17.1955607235697,20.6655220330636,
16.7945813190472));
#202028=CARTESIAN_POINT('Ctrl Pts',(-17.1421236884195,20.6075263719638,
16.7991369628542));
#202029=CARTESIAN_POINT('Ctrl Pts',(-17.1085281289397,20.5682759539064,
16.8020401077102));
#202030=CARTESIAN_POINT('Ctrl Pts',(-16.9906153898001,20.4198500712191,
16.8125410136528));
#202031=CARTESIAN_POINT('Ctrl Pts',(-16.9155865784353,20.303741249487,16.8198765234653));
#202032=CARTESIAN_POINT('Ctrl Pts',(-16.8441141284517,20.1651204890989,
16.8284838497148));
#202033=CARTESIAN_POINT('Ctrl Pts',(-16.8360514640181,20.1489796652897,
16.8294835060387));
#202034=CARTESIAN_POINT('Ctrl Pts',(-16.8183555773287,20.1123912973631,
16.8317463607716));
#202035=CARTESIAN_POINT('Ctrl Pts',(-16.80884162704,20.091888768662,16.8330121675465));
#202036=CARTESIAN_POINT('Ctrl Pts',(-16.7756490776912,20.0172516041905,
16.8376195413006));
#202037=CARTESIAN_POINT('Ctrl Pts',(-16.7539126431023,19.962287641449,16.8410121895392));
#202038=CARTESIAN_POINT('Ctrl Pts',(-16.7304860229088,19.8949373895622,
16.8452014435171));
#202039=CARTESIAN_POINT('Ctrl Pts',(-16.7265679215877,19.8833503925709,
16.8459232432515));
#202040=CARTESIAN_POINT('Ctrl Pts',(-16.7202764538486,19.8641992929252,
16.8471182860078));
#202041=CARTESIAN_POINT('Ctrl Pts',(-16.717844741408,19.8566545572059,16.8475896023454));
#202042=CARTESIAN_POINT('Ctrl Pts',(-16.7135348003855,19.8430205552864,
16.848442319599));
#202043=CARTESIAN_POINT('Ctrl Pts',(-16.7116415747875,19.8369361019763,
16.8488232222544));
#202044=CARTESIAN_POINT('Ctrl Pts',(-16.7076530215667,19.8239106705224,
16.8496394569432));
#202045=CARTESIAN_POINT('Ctrl Pts',(-16.7055658279232,19.8169673048608,
16.8500750499485));
#202046=CARTESIAN_POINT('Ctrl Pts',(-16.7000054583453,19.7981192287265,
16.8512588771066));
#202047=CARTESIAN_POINT('Ctrl Pts',(-16.696601192232,19.7861946384218,16.8520093477171));
#202048=CARTESIAN_POINT('Ctrl Pts',(-16.6796325708278,19.7247150385587,
16.8558867702653));
#202049=CARTESIAN_POINT('Ctrl Pts',(-16.6677716696659,19.6747115958207,
16.8590684023724));
#202050=CARTESIAN_POINT('Ctrl Pts',(-16.6242413884068,19.4560480100058,
16.8731123178568));
#202051=CARTESIAN_POINT('Ctrl Pts',(-16.6113283116054,19.2843350978315,
16.8845441214865));
#202052=CARTESIAN_POINT('Ctrl Pts',(-16.6234866307426,19.0220139847451,
16.9018091058584));
#202053=CARTESIAN_POINT('Ctrl Pts',(-16.633569184861,18.9313990754729,16.9077194382463));
#202054=CARTESIAN_POINT('Ctrl Pts',(-16.6511444198349,18.8321926861467,
16.9139439449464));
#202055=CARTESIAN_POINT('Ctrl Pts',(-16.6528949752438,18.822690544911,16.91453756761));
#202056=CARTESIAN_POINT('Ctrl Pts',(-16.6555773842658,18.8086696499825,
16.9154093505859));
#202057=CARTESIAN_POINT('Ctrl Pts',(-16.656459024255,18.8041415784687,16.9156902551318));
#202058=CARTESIAN_POINT('Ctrl Pts',(-16.6580501731279,18.7961095363258,
16.916187353207));
#202059=CARTESIAN_POINT('Ctrl Pts',(-16.6587537630014,18.7926044490709,
16.9164038794306));
#202060=CARTESIAN_POINT('Ctrl Pts',(-16.6602811653144,18.7850940063614,
16.9168669652411));
#202061=CARTESIAN_POINT('Ctrl Pts',(-16.6611077021402,18.7810892617399,
16.9171133671211));
#202062=CARTESIAN_POINT('Ctrl Pts',(-16.6634105741372,18.7700924158982,
16.9177885907733));
#202063=CARTESIAN_POINT('Ctrl Pts',(-16.6649107335244,18.7631052814737,
16.9182160718093));
#202064=CARTESIAN_POINT('Ctrl Pts',(-16.6731443930183,18.7256805779571,
16.9204981427327));
#202065=CARTESIAN_POINT('Ctrl Pts',(-16.6805145728341,18.6953852146079,
16.9223184367082));
#202066=CARTESIAN_POINT('Ctrl Pts',(-16.7307909376461,18.5069473644512,
16.933533356784));
#202067=CARTESIAN_POINT('Ctrl Pts',(-16.7912714468313,18.3540549666749,
16.9421917342362));
#202068=CARTESIAN_POINT('Ctrl Pts',(-16.9242256669935,18.1064001312441,
16.957577957569));
#202069=CARTESIAN_POINT('Ctrl Pts',(-16.9881305170594,18.0079378822575,
16.9641193305552));
#202070=CARTESIAN_POINT('Ctrl Pts',(-17.0685967551166,17.9039707846785,
16.9718211495755));
#202071=CARTESIAN_POINT('Ctrl Pts',(-17.077460019757,17.8927554791676,16.972662934909));
#202072=CARTESIAN_POINT('Ctrl Pts',(-17.0917460248004,17.8750500060118,
16.9740098757417));
#202073=CARTESIAN_POINT('Ctrl Pts',(-17.097095346178,17.8685009658746,16.9745120875452));
#202074=CARTESIAN_POINT('Ctrl Pts',(-17.1065983323504,17.8570079373491,
16.9754005945787));
#202075=CARTESIAN_POINT('Ctrl Pts',(-17.1107356726169,17.8520505470732,
16.9757862233266));
#202076=CARTESIAN_POINT('Ctrl Pts',(-17.1193394189939,17.8418368302834,
16.9765857189532));
#202077=CARTESIAN_POINT('Ctrl Pts',(-17.1238089593855,17.836583255291,16.9769997119573));
#202078=CARTESIAN_POINT('Ctrl Pts',(-17.1353465749404,17.8231552663939,
16.9780650371218));
#202079=CARTESIAN_POINT('Ctrl Pts',(-17.1424516467245,17.8150130335644,
16.9787178977584));
#202080=CARTESIAN_POINT('Ctrl Pts',(-17.1723582547554,17.7812659083372,
16.9814530342623));
#202081=CARTESIAN_POINT('Ctrl Pts',(-17.1957167391312,17.7561636151272,
16.9835586217593));
#202082=CARTESIAN_POINT('Ctrl Pts',(-17.2581508549208,17.6922537596297,
16.9891119975448));
#202083=CARTESIAN_POINT('Ctrl Pts',(-17.298147401795,17.6543859377552,16.9925981522907));
#202084=CARTESIAN_POINT('Ctrl Pts',(-17.4218565217009,17.5460891741164,
17.0031659000721));
#202085=CARTESIAN_POINT('Ctrl Pts',(-17.5095936082878,17.4805451213897,
17.010395889878));
#202086=CARTESIAN_POINT('Ctrl Pts',(-17.702130821921,17.3587100584198,17.0254469690628));
#202087=CARTESIAN_POINT('Ctrl Pts',(-17.8074254047905,17.3038560399,17.0332400120437));
#202088=CARTESIAN_POINT('Ctrl Pts',(-17.9255579694875,17.2544210289648,
17.0411497537052));
#202089=CARTESIAN_POINT('Ctrl Pts',(-17.934372513493,17.2508021331462,17.0417350723474));
#202090=CARTESIAN_POINT('Ctrl Pts',(-17.9474663139789,17.2455293690641,
17.0425970289135));
#202091=CARTESIAN_POINT('Ctrl Pts',(-17.9517268543673,17.2438297565147,
17.0428763242981));
#202092=CARTESIAN_POINT('Ctrl Pts',(-17.9593153269607,17.2408311190935,
17.0433716508496));
#202093=CARTESIAN_POINT('Ctrl Pts',(-17.9626410501634,17.2395266592974,
17.0435880057937));
#202094=CARTESIAN_POINT('Ctrl Pts',(-17.9697963453141,17.2367409914192,
17.0440519243042));
#202095=CARTESIAN_POINT('Ctrl Pts',(-17.9736269179161,17.2352625084545,
17.0442993238675));
#202096=CARTESIAN_POINT('Ctrl Pts',(-17.9842075399737,17.2312140433835,
17.0449801014598));
#202097=CARTESIAN_POINT('Ctrl Pts',(-17.990966550506,17.2286674185493,17.0454121018325));
#202098=CARTESIAN_POINT('Ctrl Pts',(-18.0279857950735,17.2149354408564,
17.047763107998));
#202099=CARTESIAN_POINT('Ctrl Pts',(-18.0584874180581,17.2044076673937,
17.049645318332));
#202100=CARTESIAN_POINT('Ctrl Pts',(-18.2443932449099,17.1449614850729,
17.0608552000322));
#202101=CARTESIAN_POINT('Ctrl Pts',(-18.4047918829387,17.1134147502264,
17.0694657658074));
#202102=CARTESIAN_POINT('Ctrl Pts',(-18.6837851614772,17.0913689021639,
17.0847864496237));
#202103=CARTESIAN_POINT('Ctrl Pts',(-18.8008813274884,17.0918305540773,
17.0913128877774));
#202104=CARTESIAN_POINT('Ctrl Pts',(-18.931569432224,17.1031908168632,17.09899789556));
#202105=CARTESIAN_POINT('Ctrl Pts',(-18.9457935912167,17.1045725284568,
17.0998394681574));
#202106=CARTESIAN_POINT('Ctrl Pts',(-18.9684091286237,17.1070007490587,
17.1011861321734));
#202107=CARTESIAN_POINT('Ctrl Pts',(-18.9768102631906,17.107953718895,17.1016882818113));
#202108=CARTESIAN_POINT('Ctrl Pts',(-18.9916166360501,17.1097231595595,
17.1025767164283));
#202109=CARTESIAN_POINT('Ctrl Pts',(-18.9980243057974,17.1105186609104,
17.102962335274));
#202110=CARTESIAN_POINT('Ctrl Pts',(-19.0112697208231,17.1122246225419,
17.1037618472599));
#202111=CARTESIAN_POINT('Ctrl Pts',(-19.0181068482672,17.1131392133591,
17.1041758667074));
#202112=CARTESIAN_POINT('Ctrl Pts',(-19.0356451191562,17.1155725871352,
17.1052413376107));
#202113=CARTESIAN_POINT('Ctrl Pts',(-19.0463392251379,17.1171399229768,
17.1058943183501));
#202114=CARTESIAN_POINT('Ctrl Pts',(-19.0909218854945,17.1240231306882,
17.1086306185752));
#202115=CARTESIAN_POINT('Ctrl Pts',(-19.1246891633661,17.1300801440805,
17.1107372745081));
#202116=CARTESIAN_POINT('Ctrl Pts',(-19.2122748455883,17.1479977764243,
17.1162941400135));
#202117=CARTESIAN_POINT('Ctrl Pts',(-19.2658010346737,17.1611434583797,
17.1197827761873));
#202118=CARTESIAN_POINT('Ctrl Pts',(-19.4264938850115,17.2073261803799,
17.1305297339397));
#202119=CARTESIAN_POINT('Ctrl Pts',(-19.5316004788073,17.2467987994143,
17.1379469158678));
#202120=CARTESIAN_POINT('Ctrl Pts',(-19.7377596912756,17.3435083559375,
17.1529857191004));
#202121=CARTESIAN_POINT('Ctrl Pts',(-19.8382546900748,17.4011142558444,
17.1605795851763));
#202122=CARTESIAN_POINT('Ctrl Pts',(-19.9414396663835,17.472072133917,17.1683151265274));
#202123=CARTESIAN_POINT('Ctrl Pts',(-19.9492920968202,17.477550895263,17.168903325603));
#202124=CARTESIAN_POINT('Ctrl Pts',(-19.9608585874898,17.4857382430863,
17.169768692267));
#202125=CARTESIAN_POINT('Ctrl Pts',(-19.964601304713,17.4884058651775,17.170048547271));
#202126=CARTESIAN_POINT('Ctrl Pts',(-19.971152957884,17.493107807014,17.1705381059388));
#202127=CARTESIAN_POINT('Ctrl Pts',(-19.9739656094503,17.4951368597897,
17.1707481665193));
#202128=CARTESIAN_POINT('Ctrl Pts',(-19.9767861316653,17.4971821476041,
17.1709587007979));
#202129=CARTESIAN_POINT('Ctrl Pts',(-19.976798940029,17.4971914357452,17.1709596568595));
#202130=CARTESIAN_POINT('Ctrl Pts',(-19.9768243308286,17.4972098486273,
17.1709615521142));
#202131=CARTESIAN_POINT('Ctrl Pts',(-19.976836913868,17.4972189737984,17.1709624913524));
#202132=CARTESIAN_POINT('Ctrl Pts',(-19.976861860772,17.4972370656151,17.1709643534645));
#202133=CARTESIAN_POINT('Ctrl Pts',(-19.9768742240742,17.4972460318455,
17.1709652762965));
#202134=CARTESIAN_POINT('Ctrl Pts',(-19.9768987356531,17.4972638087684,
17.1709671059062));
#202135=CARTESIAN_POINT('Ctrl Pts',(-19.9769108839021,17.4972726194336,
17.1709680126819));
#202136=CARTESIAN_POINT('Ctrl Pts',(-19.9769349703243,17.4972900887949,
17.1709698105485));
#202137=CARTESIAN_POINT('Ctrl Pts',(-19.9769469084253,17.4972987474319,
17.1709707016342));
#202138=CARTESIAN_POINT('Ctrl Pts',(-19.9769705784767,17.4973159155634,
17.1709724684141));
#202139=CARTESIAN_POINT('Ctrl Pts',(-19.976982310808,17.4973244253277,17.1709733441368));
#202140=CARTESIAN_POINT('Ctrl Pts',(-19.9770055739011,17.4973412990173,
17.1709750805329));
#202141=CARTESIAN_POINT('Ctrl Pts',(-19.9770171048129,17.4973496630452,
17.1709759412176));
#202142=CARTESIAN_POINT('Ctrl Pts',(-19.9770399705675,17.4973662492331,
17.1709776479483));
#202143=CARTESIAN_POINT('Ctrl Pts',(-19.9770513049473,17.4973744710512,
17.1709784939599));
#202144=CARTESIAN_POINT('Ctrl Pts',(-19.977073780378,17.4973907747896,17.1709801715493));
#202145=CARTESIAN_POINT('Ctrl Pts',(-19.9770849219528,17.497398857084,17.1709810031662));
#202146=CARTESIAN_POINT('Ctrl Pts',(-19.977107016468,17.497414885163,17.1709826523168));
#202147=CARTESIAN_POINT('Ctrl Pts',(-19.9771179693997,17.4974228309356,
17.1709834698499));
#202148=CARTESIAN_POINT('Ctrl Pts',(-19.9771396912811,17.4974385893296,
17.1709850911802));
#202149=CARTESIAN_POINT('Ctrl Pts',(-19.9771504598209,17.4974464016483,
17.1709858949469));
#202150=CARTESIAN_POINT('Ctrl Pts',(-19.9771718164569,17.4974618956853,
17.1709874890087));
#202151=CARTESIAN_POINT('Ctrl Pts',(-19.9771824044771,17.4974695773434,
17.1709882792982));
#202152=CARTESIAN_POINT('Ctrl Pts',(-19.9772034034501,17.4974848124934,
17.1709898466579));
#202153=CARTESIAN_POINT('Ctrl Pts',(-19.9772138145841,17.4974923661119,
17.1709906237416));
#202154=CARTESIAN_POINT('Ctrl Pts',(-19.9772339084215,17.4975069451281,
17.1709921235363));
#202155=CARTESIAN_POINT('Ctrl Pts',(-19.9772435910909,17.4975139704816,
17.1709928462449));
#202156=CARTESIAN_POINT('Ctrl Pts',(-19.97726291965,17.4975279947529,17.1709942889144));
#202157=CARTESIAN_POINT('Ctrl Pts',(-19.9772725657327,17.4975349938098,
17.1709950088896));
#202158=CARTESIAN_POINT('Ctrl Pts',(-19.977291821858,17.4975489660215,17.1709964461475));
#202159=CARTESIAN_POINT('Ctrl Pts',(-19.9773014317922,17.4975559390968,
17.1709971634221));
#202160=CARTESIAN_POINT('Ctrl Pts',(-19.977320616076,17.4975698596732,17.1709985953127));
#202161=CARTESIAN_POINT('Ctrl Pts',(-19.9773301903575,17.497576807124,17.1709993099237));
#202162=CARTESIAN_POINT('Ctrl Pts',(-19.9773493027676,17.4975906760362,
17.1710007364447));
#202163=CARTESIAN_POINT('Ctrl Pts',(-19.9773588413912,17.4975975978559,
17.1710014483916));
#202164=CARTESIAN_POINT('Ctrl Pts',(-19.9806629149965,17.4999952816906,
17.1712480585035));
#202165=CARTESIAN_POINT('Ctrl Pts',(-19.9839505796573,17.5023955639879,
17.171493293435));
#202166=CARTESIAN_POINT('Ctrl Pts',(-19.9907473935226,17.5073879486686,
17.1720000185021));
#202167=CARTESIAN_POINT('Ctrl Pts',(-19.9942554981795,17.5099814484733,
17.1722614116546));
#202168=CARTESIAN_POINT('Ctrl Pts',(-20.0031582711901,17.516605821497,17.1729244618015));
#202169=CARTESIAN_POINT('Ctrl Pts',(-20.0085418140649,17.5206516582818,
17.1733251233222));
#202170=CARTESIAN_POINT('Ctrl Pts',(-20.0240192051829,17.5323991994058,
17.1744764635561));
#202171=CARTESIAN_POINT('Ctrl Pts',(-20.0340633722757,17.5401662434556,
17.1752229672188));
#202172=CARTESIAN_POINT('Ctrl Pts',(-20.0683088146373,17.5671436564281,
17.1777681863004));
#202173=CARTESIAN_POINT('Ctrl Pts',(-20.0921600548039,17.5867939944063,
17.1795409393349));
#202174=CARTESIAN_POINT('Ctrl Pts',(-20.2113467482272,17.6894505634705,
17.188449062742));
#202175=CARTESIAN_POINT('Ctrl Pts',(-20.299546724616,17.7803586925282,17.1952196583335));
#202176=CARTESIAN_POINT('Ctrl Pts',(-20.4097844625949,17.9164690961939,
17.2047555495432));
#202177=CARTESIAN_POINT('Ctrl Pts',(-20.43913807349,17.9553855091922,17.2074206101436));
#202178=CARTESIAN_POINT('Ctrl Pts',(-20.5189778804002,18.0692045004508,
17.2151169900671));
#202179=CARTESIAN_POINT('Ctrl Pts',(-20.5660451944649,18.1463636602338,
17.2202235061175));
#202180=CARTESIAN_POINT('Ctrl Pts',(-20.614423582134,18.2384340743941,17.2263211557695));
#202181=CARTESIAN_POINT('Ctrl Pts',(-20.6206885111512,18.2506439324104,
17.2271297421923));
#202182=CARTESIAN_POINT('Ctrl Pts',(-20.6305464904218,18.2703251773399,
17.2284334242447));
#202183=CARTESIAN_POINT('Ctrl Pts',(-20.6342151974782,18.2777583846572,
17.2289258679561));
#202184=CARTESIAN_POINT('Ctrl Pts',(-20.6406524019749,18.2909962097609,
17.2298030681659));
#202185=CARTESIAN_POINT('Ctrl Pts',(-20.6434382975264,18.2967922869821,
17.2301872126918));
#202186=CARTESIAN_POINT('Ctrl Pts',(-20.6491885396076,18.3088966582987,
17.2309896346162));
#202187=CARTESIAN_POINT('Ctrl Pts',(-20.6521482233075,18.3152070702627,
17.2314080679141));
#202188=CARTESIAN_POINT('Ctrl Pts',(-20.6597551194754,18.3316364746616,
17.2324978029263));
#202189=CARTESIAN_POINT('Ctrl Pts',(-20.6643537093322,18.3417776237763,
17.23317077043));
#202190=CARTESIAN_POINT('Ctrl Pts',(-20.6839918006411,18.3860094952924,
17.2361077301152));
#202191=CARTESIAN_POINT('Ctrl Pts',(-20.6982090530658,18.4204559628926,
17.2383995513923));
#202192=CARTESIAN_POINT('Ctrl Pts',(-20.7335762447422,18.5129993850948,
17.2445727474128));
#202193=CARTESIAN_POINT('Ctrl Pts',(-20.7531018231504,18.5716747977174,
17.2485040294199));
#202194=CARTESIAN_POINT('Ctrl Pts',(-20.8238088869656,18.8199345232613,
17.265181550711));
#202195=CARTESIAN_POINT('Ctrl Pts',(-20.8510531407969,19.015286332678,17.2785154521607));
#202196=CARTESIAN_POINT('Ctrl Pts',(-20.8509999221906,19.2115739728967,
17.290908287241));
#202197=CARTESIAN_POINT('Ctrl Pts',(-20.8509999215533,19.211576318847,17.2909084353551));
#202198=CARTESIAN_POINT('Ctrl Pts',(-20.8509956361944,19.2273177864368,
17.2919022894384));
#202199=CARTESIAN_POINT('Ctrl Pts',(-20.8508157764495,19.2430592819062,
17.2928890187188));
#202200=CARTESIAN_POINT('Ctrl Pts',(-20.8502148553261,19.2696677093326,
17.294543265343));
#202201=CARTESIAN_POINT('Ctrl Pts',(-20.8498856305801,19.2805357712956,
17.295215078138));
#202202=CARTESIAN_POINT('Ctrl Pts',(-20.8492914997326,19.2961682450766,
17.2961753949309));
#202203=CARTESIAN_POINT('Ctrl Pts',(-20.8490942018497,19.3009348492606,
17.2964674073038));
#202204=CARTESIAN_POINT('Ctrl Pts',(-20.8487208813595,19.3092719314371,
17.296976699464));
#202205=CARTESIAN_POINT('Ctrl Pts',(-20.8485519257252,19.3128426846232,
17.2971943609584));
#202206=CARTESIAN_POINT('Ctrl Pts',(-20.8482044716738,19.3198119163801,
17.2976182479406));
#202207=CARTESIAN_POINT('Ctrl Pts',(-20.8480268210971,19.3232104340723,
17.2978245201538));
#202208=CARTESIAN_POINT('Ctrl Pts',(-20.8476550551564,19.3300079760932,
17.2982362092455));
#202209=CARTESIAN_POINT('Ctrl Pts',(-20.8474609356904,19.3334069616119,
17.2984416261313));
#202210=CARTESIAN_POINT('Ctrl Pts',(-20.8469736811295,19.3415917783836,
17.2989352437825));
#202211=CARTESIAN_POINT('Ctrl Pts',(-20.8466724833011,19.3463771363713,
17.299222995435));
#202212=CARTESIAN_POINT('Ctrl Pts',(-20.8455076184958,19.3639326585952,
17.3002756599104));
#202213=CARTESIAN_POINT('Ctrl Pts',(-20.8445443836754,19.3766962389897,
17.3010352044386));
#202214=CARTESIAN_POINT('Ctrl Pts',(-20.8412948234941,19.415109295813,17.303305779114));
#202215=CARTESIAN_POINT('Ctrl Pts',(-20.8386561520336,19.440727409303,17.3047994319179));
#202216=CARTESIAN_POINT('Ctrl Pts',(-20.8160117669933,19.6271347049876,
17.3155582884879));
#202217=CARTESIAN_POINT('Ctrl Pts',(-20.7780853950748,19.7851006901587,
17.3241154224325));
#202218=CARTESIAN_POINT('Ctrl Pts',(-20.7225806054527,19.9371103054064,
17.3329786569753));
#202219=CARTESIAN_POINT('Origin',(-18.734,19.211,0.));
#202220=CARTESIAN_POINT('',(-20.7225806168679,19.9371102741439,18.3568545763217));
#202221=CARTESIAN_POINT('',(-20.7225805905512,19.9371103462167,18.1318063719887));
#202222=CARTESIAN_POINT('',(-20.7225806064498,19.9371103026755,0.));
#202223=CARTESIAN_POINT('Ctrl Pts',(-20.7225806168679,19.9371102741439,
18.3568545763217));
#202224=CARTESIAN_POINT('Ctrl Pts',(-20.7279235886306,19.9224776068176,
18.3558520750571));
#202225=CARTESIAN_POINT('Ctrl Pts',(-20.7331056671166,19.9077842824243,
18.3548454788278));
#202226=CARTESIAN_POINT('Ctrl Pts',(-20.7819939765922,19.7641279866657,
18.3450068771352));
#202227=CARTESIAN_POINT('Ctrl Pts',(-20.8133220094845,19.6312931103634,
18.3359031763939));
#202228=CARTESIAN_POINT('Ctrl Pts',(-20.8417530898284,19.4223144011233,
18.3221216513367));
#202229=CARTESIAN_POINT('Ctrl Pts',(-20.8479010440638,19.3477542444381,
18.3173148433635));
#202230=CARTESIAN_POINT('Ctrl Pts',(-20.8503509135829,19.2641628324461,
18.3121557836362));
#202231=CARTESIAN_POINT('Ctrl Pts',(-20.8505548516267,19.2553062358344,
18.311612076797));
#202232=CARTESIAN_POINT('Ctrl Pts',(-20.8507777608051,19.2419958471638,
18.3107995733725));
#202233=CARTESIAN_POINT('Ctrl Pts',(-20.8508382796755,19.2375429787264,
18.3105285349334));
#202234=CARTESIAN_POINT('Ctrl Pts',(-20.8509183443716,19.229870345947,18.3100628926518));
#202235=CARTESIAN_POINT('Ctrl Pts',(-20.8509445960013,19.2266507069947,
18.3098679164559));
#202236=CARTESIAN_POINT('Ctrl Pts',(-20.8509874023438,19.2193608829985,
18.3094274124076));
#202237=CARTESIAN_POINT('Ctrl Pts',(-20.8509995645905,19.2152907123876,
18.3091821332973));
#202238=CARTESIAN_POINT('Ctrl Pts',(-20.8510007238756,19.2041601518444,
18.3085131479209));
#202239=CARTESIAN_POINT('Ctrl Pts',(-20.8509661391565,19.1970997382133,
18.3080907414477));
#202240=CARTESIAN_POINT('Ctrl Pts',(-20.8505991940029,19.1600402483695,
18.3058831832676));
#202241=CARTESIAN_POINT('Ctrl Pts',(-20.8496644764733,19.1300489297337,
18.3041297304724));
#202242=CARTESIAN_POINT('Ctrl Pts',(-20.8449576379443,19.04033360736,18.2989567920898));
#202243=CARTESIAN_POINT('Ctrl Pts',(-20.8392907053301,18.9807365831336,
18.2956162060616));
#202244=CARTESIAN_POINT('Ctrl Pts',(-20.8082534041835,18.7559400892342,
18.2831217032851));
#202245=CARTESIAN_POINT('Ctrl Pts',(-20.7658882389287,18.5937173192297,
18.2742743496021));
#202246=CARTESIAN_POINT('Ctrl Pts',(-20.6832635060479,18.3830083038489,
18.2615098046473));
#202247=CARTESIAN_POINT('Ctrl Pts',(-20.6593330779176,18.3287924993762,
18.2581084530173));
#202248=CARTESIAN_POINT('Ctrl Pts',(-20.6277538502301,18.264672779265,18.2539094981777));
#202249=CARTESIAN_POINT('Ctrl Pts',(-20.6222501813624,18.2537382295761,
18.2531871161297));
#202250=CARTESIAN_POINT('Ctrl Pts',(-20.6130255038378,18.2357999992725,
18.2519913061925));
#202251=CARTESIAN_POINT('Ctrl Pts',(-20.6093593760602,18.2287683096653,
18.2515198093162));
#202252=CARTESIAN_POINT('Ctrl Pts',(-20.6026761040452,18.2161235119061,
18.2506668971066));
#202253=CARTESIAN_POINT('Ctrl Pts',(-20.5996729454112,18.2105030895702,
18.2502859810478));
#202254=CARTESIAN_POINT('Ctrl Pts',(-20.5931997793556,18.1985190289402,
18.2494698618593));
#202255=CARTESIAN_POINT('Ctrl Pts',(-20.5897223818567,18.1921594944472,
18.2490343985108));
#202256=CARTESIAN_POINT('Ctrl Pts',(-20.5802117614021,18.1749765069678,
18.2478512849531));
#202257=CARTESIAN_POINT('Ctrl Pts',(-20.5741161268356,18.1641880896839,
18.2471014028714));
#202258=CARTESIAN_POINT('Ctrl Pts',(-20.5423238602427,18.1090560473854,
18.243232325567));
#202259=CARTESIAN_POINT('Ctrl Pts',(-20.5151196159157,18.0656058060472,
18.2400587313911));
#202260=CARTESIAN_POINT('Ctrl Pts',(-20.3905640768228,17.8818502138373,
18.2260767525442));
#202261=CARTESIAN_POINT('Ctrl Pts',(-20.2780223785624,17.7526372262008,
18.2147048635678));
#202262=CARTESIAN_POINT('Ctrl Pts',(-20.082846824392,17.5767503536245,18.1974265663112));
#202263=CARTESIAN_POINT('Ctrl Pts',(-20.0105229808749,17.5196535766864,
18.1914504713804));
#202264=CARTESIAN_POINT('Ctrl Pts',(-19.9267413463558,17.4619572449719,
18.1851656487334));
#202265=CARTESIAN_POINT('Ctrl Pts',(-19.9187408031815,17.4565280806922,
18.1845716097907));
#202266=CARTESIAN_POINT('Ctrl Pts',(-19.9068673061104,17.4485889882307,
18.1836993345904));
#202267=CARTESIAN_POINT('Ctrl Pts',(-19.9030230211864,17.4460366947114,
18.1834183497158));
#202268=CARTESIAN_POINT('Ctrl Pts',(-19.8961854772461,17.4415292604913,
18.1829211629406));
#202269=CARTESIAN_POINT('Ctrl Pts',(-19.8931955833309,17.4395691145963,
18.1827046279009));
#202270=CARTESIAN_POINT('Ctrl Pts',(-19.8867759743441,17.4353836937622,
18.1822415824304));
#202271=CARTESIAN_POINT('Ctrl Pts',(-19.8833447842729,17.433160782996,18.1819952293969));
#202272=CARTESIAN_POINT('Ctrl Pts',(-19.873901494864,17.4270816731741,18.1813202773879));
#202273=CARTESIAN_POINT('Ctrl Pts',(-19.8678762220928,17.4232458974844,
18.1808930173543));
#202274=CARTESIAN_POINT('Ctrl Pts',(-19.8354945546945,17.4028608257797,
18.1786142538754));
#202275=CARTESIAN_POINT('Ctrl Pts',(-19.8087935695442,17.3868627953459,
18.176796928762));
#202276=CARTESIAN_POINT('Ctrl Pts',(-19.639330541107,17.2903417119676,18.1655817188541));
#202277=CARTESIAN_POINT('Ctrl Pts',(-19.4879598292091,17.2260293189489,
18.1569210140017));
#202278=CARTESIAN_POINT('Ctrl Pts',(-19.2182121069083,17.1467893281181,
18.1415316377863));
#202279=CARTESIAN_POINT('Ctrl Pts',(-19.1032202690765,17.1231546613371,
18.1349895793114));
#202280=CARTESIAN_POINT('Ctrl Pts',(-18.9726799019284,17.1074493714411,
18.1272869887103));
#202281=CARTESIAN_POINT('Ctrl Pts',(-18.958470743088,17.1058857007117,18.1264451937821));
#202282=CARTESIAN_POINT('Ctrl Pts',(-18.9358327578082,17.1036262685085,
18.1250982404687));
#202283=CARTESIAN_POINT('Ctrl Pts',(-18.9274135620935,17.1028368902909,
18.1245960258657));
#202284=CARTESIAN_POINT('Ctrl Pts',(-18.912557589538,17.1015337450178,18.123707515576));
#202285=CARTESIAN_POINT('Ctrl Pts',(-18.9061227320673,17.1009989437514,
18.1233218863871));
#202286=CARTESIAN_POINT('Ctrl Pts',(-18.892809139967,17.0999537584515,18.1225223915118));
#202287=CARTESIAN_POINT('Ctrl Pts',(-18.8859301638656,17.0994475378411,
18.1221083997082));
#202288=CARTESIAN_POINT('Ctrl Pts',(-18.8682679935417,17.098234541639,18.1210430811407));
#202289=CARTESIAN_POINT('Ctrl Pts',(-18.8574817370218,17.0975767035508,
18.1203902259372));
#202290=CARTESIAN_POINT('Ctrl Pts',(-18.8124546918413,17.095176443615,18.117655142007));
#202291=CARTESIAN_POINT('Ctrl Pts',(-18.7781807231669,17.0941834495625,
18.1155496027715));
#202292=CARTESIAN_POINT('Ctrl Pts',(-18.688839404307,17.0937656779543,18.1099963845837));
#202293=CARTESIAN_POINT('Ctrl Pts',(-18.6337945776069,17.0956563616929,
18.1065103418884));
#202294=CARTESIAN_POINT('Ctrl Pts',(-18.4698250798929,17.1077026203323,
18.0959428093823));
#202295=CARTESIAN_POINT('Ctrl Pts',(-18.3615528642482,17.1241535945483,
18.088712922088));
#202296=CARTESIAN_POINT('Ctrl Pts',(-18.2114893144157,17.1590080248056,
18.0785361845688));
#202297=CARTESIAN_POINT('Ctrl Pts',(-18.1682636355976,17.1705022604532,
18.0755877053219));
#202298=CARTESIAN_POINT('Ctrl Pts',(-18.1012764327963,17.1906074579972,
18.0710174114961));
#202299=CARTESIAN_POINT('Ctrl Pts',(-18.077250090143,17.1982892003561,18.0693780401148));
#202300=CARTESIAN_POINT('Ctrl Pts',(-18.006137231317,17.2224345601641,18.0645356450814));
#202301=CARTESIAN_POINT('Ctrl Pts',(-17.9594855135928,17.2401360028084,
18.061371658143));
#202302=CARTESIAN_POINT('Ctrl Pts',(-17.9062948296633,17.2624994930913,
18.0578132726379));
#202303=CARTESIAN_POINT('Ctrl Pts',(-17.8991073595939,17.2655683364015,
18.0573335036114));
#202304=CARTESIAN_POINT('Ctrl Pts',(-17.8876575865571,17.2705322023204,
18.0565711162539));
#202305=CARTESIAN_POINT('Ctrl Pts',(-17.8833843460532,17.2724015978434,
18.056287004365));
#202306=CARTESIAN_POINT('Ctrl Pts',(-17.875832536487,17.275735032019,18.0557857086616));
#202307=CARTESIAN_POINT('Ctrl Pts',(-17.8725514708351,17.2771933074717,
18.055568177123));
#202308=CARTESIAN_POINT('Ctrl Pts',(-17.865611165972,17.2802991074329,18.0551086247204));
#202309=CARTESIAN_POINT('Ctrl Pts',(-17.8619529037576,17.2819486875214,
18.0548667322983));
#202310=CARTESIAN_POINT('Ctrl Pts',(-17.8521061472497,17.2864225124618,
18.054216501074));
#202311=CARTESIAN_POINT('Ctrl Pts',(-17.8459264774879,17.2892662269344,
18.0538093422824));
#202312=CARTESIAN_POINT('Ctrl Pts',(-17.8155064714923,17.3034427516473,
18.0518090780955));
#202313=CARTESIAN_POINT('Ctrl Pts',(-17.7914676120732,17.3152052151806,
18.0502410158005));
#202314=CARTESIAN_POINT('Ctrl Pts',(-17.7228425003853,17.3504123358398,
18.0457829537353));
#202315=CARTESIAN_POINT('Ctrl Pts',(-17.678859712758,17.3749973867461,18.0429483593201));
#202316=CARTESIAN_POINT('Ctrl Pts',(-17.5228519653038,17.4696609479272,
18.0328288287506));
#202317=CARTESIAN_POINT('Ctrl Pts',(-17.4165711005165,17.5486147279255,
18.0257912722745));
#202318=CARTESIAN_POINT('Ctrl Pts',(-17.2410480228008,17.7064769250663,
18.0128047330271));
#202319=CARTESIAN_POINT('Ctrl Pts',(-17.1689908609921,17.7815813626763,
18.0069646491463));
#202320=CARTESIAN_POINT('Ctrl Pts',(-17.0937851868561,17.8725000941801,
18.0000501723039));
#202321=CARTESIAN_POINT('Ctrl Pts',(-17.0849331101857,17.8834213733836,
17.9992221269926));
#202322=CARTESIAN_POINT('Ctrl Pts',(-17.0709745037462,17.9009978831344,
17.9978930751351));
#202323=CARTESIAN_POINT('Ctrl Pts',(-17.0657975265354,17.9075968191615,
17.9973948898039));
#202324=CARTESIAN_POINT('Ctrl Pts',(-17.0567114623928,17.9193213588089,
17.9965110615274));
#202325=CARTESIAN_POINT('Ctrl Pts',(-17.0527862941115,17.9244344073417,
17.9961260625336));
#202326=CARTESIAN_POINT('Ctrl Pts',(-17.0446920345478,17.9350785402328,
17.9953254495193));
#202327=CARTESIAN_POINT('Ctrl Pts',(-17.0405266188825,17.9406123114154,
17.9949096973999));
#202328=CARTESIAN_POINT('Ctrl Pts',(-17.0298540954973,17.9549365658835,
17.9938346880525));
#202329=CARTESIAN_POINT('Ctrl Pts',(-17.0233878775954,17.9637571311048,
17.9931738483764));
#202330=CARTESIAN_POINT('Ctrl Pts',(-16.9962601444118,18.0013698608516,
17.9903603332824));
#202331=CARTESIAN_POINT('Ctrl Pts',(-16.9762559466372,18.0306269726025,
17.9881826429289));
#202332=CARTESIAN_POINT('Ctrl Pts',(-16.9256702920182,18.1087502383496,
17.9823920771855));
#202333=CARTESIAN_POINT('Ctrl Pts',(-16.8963354105636,18.1583847826659,
17.9787366240366));
#202334=CARTESIAN_POINT('Ctrl Pts',(-16.7931942183012,18.3503815039853,
17.9646995012915));
#202335=CARTESIAN_POINT('Ctrl Pts',(-16.7336208999361,18.4997564510137,
17.9539364305487));
#202336=CARTESIAN_POINT('Ctrl Pts',(-16.6877207719693,18.6681976139541,
17.9425813488462));
#202337=CARTESIAN_POINT('Ctrl Pts',(-16.68410418427,18.6820195959151,17.9416554963001));
#202338=CARTESIAN_POINT('Ctrl Pts',(-16.6785657088547,18.7040969632575,
17.9401870890761));
#202339=CARTESIAN_POINT('Ctrl Pts',(-16.6765530321099,18.712328974593,17.9396418592465));
#202340=CARTESIAN_POINT('Ctrl Pts',(-16.6646682505495,18.762235764839,17.9363511025041));
#202341=CARTESIAN_POINT('Ctrl Pts',(-16.6560124564913,18.804193448197,17.9336463329712));
#202342=CARTESIAN_POINT('Ctrl Pts',(-16.6473466573013,18.8537566855506,
17.930545618189));
#202343=CARTESIAN_POINT('Ctrl Pts',(-16.6460973255535,18.8611323333694,
17.9300866318769));
#202344=CARTESIAN_POINT('Ctrl Pts',(-16.6441405110127,18.8730686266629,
17.9293479491722));
#202345=CARTESIAN_POINT('Ctrl Pts',(-16.6434088124107,18.877625159766,17.9290669332108));
#202346=CARTESIAN_POINT('Ctrl Pts',(-16.6421367095041,18.8857158845745,
17.9285697121013));
#202347=CARTESIAN_POINT('Ctrl Pts',(-16.6415903529058,18.8892490850111,
17.928353173642));
#202348=CARTESIAN_POINT('Ctrl Pts',(-16.6404384571288,18.8968252435236,
17.9278901437483));
#202349=CARTESIAN_POINT('Ctrl Pts',(-16.6398356785746,18.9008685650967,
17.9276438095914));
#202350=CARTESIAN_POINT('Ctrl Pts',(-16.638212126157,18.9119796294738,17.9269689625562));
#202351=CARTESIAN_POINT('Ctrl Pts',(-16.6372153844792,18.9190509058753,
17.9265417879267));
#202352=CARTESIAN_POINT('Ctrl Pts',(-16.6320693322199,18.9569453925563,
17.9242643010476));
#202353=CARTESIAN_POINT('Ctrl Pts',(-16.6285636239004,18.9878539208088,
17.9224481218038));
#202354=CARTESIAN_POINT('Ctrl Pts',(-16.6108607051316,19.1820694907886,
17.9112327987635));
#202355=CARTESIAN_POINT('Ctrl Pts',(-16.6149886575892,19.3465018782596,
17.9025711946963));
#202356=CARTESIAN_POINT('Ctrl Pts',(-16.6545441347814,19.6248738248299,
17.8871806013251));
#202357=CARTESIAN_POINT('Ctrl Pts',(-16.6806410937662,19.7393371488572,
17.880638279104));
#202358=CARTESIAN_POINT('Ctrl Pts',(-16.7203942459428,19.8646705680541,
17.8729353916303));
#202359=CARTESIAN_POINT('Ctrl Pts',(-16.7248539255653,19.878252112002,17.8720935930106));
#202360=CARTESIAN_POINT('Ctrl Pts',(-16.7321700699384,19.8997941911237,
17.8707466348939));
#202361=CARTESIAN_POINT('Ctrl Pts',(-16.7349373303762,19.9077847202459,
17.8702444192122));
#202362=CARTESIAN_POINT('Ctrl Pts',(-16.7399019451138,19.9218471292961,
17.8693559076657));
#202363=CARTESIAN_POINT('Ctrl Pts',(-16.7420793578828,19.9279259709419,
17.8689702783047));
#202364=CARTESIAN_POINT('Ctrl Pts',(-16.7466401843047,19.9404775800184,
17.8681707837129));
#202365=CARTESIAN_POINT('Ctrl Pts',(-16.7490274876515,19.9469488435071,
17.8677567923678));
#202366=CARTESIAN_POINT('Ctrl Pts',(-16.755235989049,19.9635282482156,17.8666914763274));
#202367=CARTESIAN_POINT('Ctrl Pts',(-16.7591030005804,19.9736189155141,
17.8660386232066));
#202368=CARTESIAN_POINT('Ctrl Pts',(-16.7755605404946,20.0155988587882,
17.863303559453));
#202369=CARTESIAN_POINT('Ctrl Pts',(-16.7888469702367,20.0472080572438,
17.8611980387414));
#202370=CARTESIAN_POINT('Ctrl Pts',(-16.8254562142462,20.128704309467,17.8556448810496));
#202371=CARTESIAN_POINT('Ctrl Pts',(-16.8499670865737,20.1780262374202,
17.8521588813683));
#202372=CARTESIAN_POINT('Ctrl Pts',(-16.9288198107064,20.3222932200393,
17.8415914314985));
#202373=CARTESIAN_POINT('Ctrl Pts',(-16.988621974948,20.4140379127527,17.834361583553));
#202374=CARTESIAN_POINT('Ctrl Pts',(-17.0824452229109,20.5361605065567,
17.8241885267367));
#202375=CARTESIAN_POINT('Ctrl Pts',(-17.110768268272,20.5707067589978,17.8212436790553));
#202376=CARTESIAN_POINT('Ctrl Pts',(-17.1568585388308,20.6234295589014,
17.8166674393319));
#202377=CARTESIAN_POINT('Ctrl Pts',(-17.1738960661287,20.6422261299244,
17.8150186759653));
#202378=CARTESIAN_POINT('Ctrl Pts',(-17.2253673726505,20.6970000573184,
17.8101725035341));
#202379=CARTESIAN_POINT('Ctrl Pts',(-17.2607397999422,20.7320765333519,
17.8070138580573));
#202380=CARTESIAN_POINT('Ctrl Pts',(-17.3030568212839,20.7711767980069,
17.8034607457834));
#202381=CARTESIAN_POINT('Ctrl Pts',(-17.3088236473285,20.7764463867677,
17.8029811862584));
#202382=CARTESIAN_POINT('Ctrl Pts',(-17.3180794188717,20.7848105519321,
17.8022190675972));
#202383=CARTESIAN_POINT('Ctrl Pts',(-17.3215495863083,20.7879256720775,
17.801935016521));
#202384=CARTESIAN_POINT('Ctrl Pts',(-17.3277097403663,20.7934189067434,
17.8014337899495));
#202385=CARTESIAN_POINT('Ctrl Pts',(-17.3303955184644,20.7958016755775,
17.8012162670592));
#202386=CARTESIAN_POINT('Ctrl Pts',(-17.3360964234948,20.8008335443592,
17.8007566910019));
#202387=CARTESIAN_POINT('Ctrl Pts',(-17.3391130195072,20.803480901061,17.8005147664904));
#202388=CARTESIAN_POINT('Ctrl Pts',(-17.3472644947487,20.8105936811273,
17.7998643579212));
#202389=CARTESIAN_POINT('Ctrl Pts',(-17.3524134562302,20.8150429954258,
17.7994570549838));
#202390=CARTESIAN_POINT('Ctrl Pts',(-17.3779365132596,20.836883876991,17.7974549385015));
#202391=CARTESIAN_POINT('Ctrl Pts',(-17.3986189788513,20.8539133395081,
17.795885223844));
#202392=CARTESIAN_POINT('Ctrl Pts',(-17.4591673799483,20.9018683658375,
17.7914210089148));
#202393=CARTESIAN_POINT('Ctrl Pts',(-17.4998242932351,20.9317687362996,
17.7885820971808));
#202394=CARTESIAN_POINT('Ctrl Pts',(-17.653842795072,21.0367687972392,17.7782457286038));
#202395=CARTESIAN_POINT('Ctrl Pts',(-17.7732895619697,21.1023511818719,
17.7710112720879));
#202396=CARTESIAN_POINT('Ctrl Pts',(-17.9902203303781,21.1955682718228,
17.7580012076775));
#202397=CARTESIAN_POINT('Ctrl Pts',(-18.0849153183013,21.2285244231646,
17.7523642927888));
#202398=CARTESIAN_POINT('Ctrl Pts',(-18.1950693905495,21.2583001903951,
17.7456767073605));
#202399=CARTESIAN_POINT('Ctrl Pts',(-18.2085947232566,21.2618129004394,
17.7448535528168));
#202400=CARTESIAN_POINT('Ctrl Pts',(-18.2302682573637,21.2672133321497,
17.7435308735146));
#202401=CARTESIAN_POINT('Ctrl Pts',(-18.2383947298294,21.2691871511032,
17.7430341269616));
#202402=CARTESIAN_POINT('Ctrl Pts',(-18.2528015878765,21.2725961265103,
17.7421519645916));
#202403=CARTESIAN_POINT('Ctrl Pts',(-18.2590772636499,21.2740508703748,
17.7417671846968));
#202404=CARTESIAN_POINT('Ctrl Pts',(-18.2721242579922,21.2770125653109,
17.7409661429812));
#202405=CARTESIAN_POINT('Ctrl Pts',(-18.2788965307704,21.2785149217335,
17.740549738684));
#202406=CARTESIAN_POINT('Ctrl Pts',(-18.2964119598141,21.2823103050414,
17.7394711440535));
#202407=CARTESIAN_POINT('Ctrl Pts',(-18.3071656985573,21.2845530243213,
17.7388073511231));
#202408=CARTESIAN_POINT('Ctrl Pts',(-18.3531107373858,21.2937624261987,
17.7359642653186));
#202409=CARTESIAN_POINT('Ctrl Pts',(-18.3884569324463,21.2999173501348,
17.7337592980743));
#202410=CARTESIAN_POINT('Ctrl Pts',(-18.4819311258842,21.3137569704982,
17.7278780969134));
#202411=CARTESIAN_POINT('Ctrl Pts',(-18.5402484715471,21.3199298147708,
17.7241576093364));
#202412=CARTESIAN_POINT('Ctrl Pts',(-18.7473246243964,21.3331871926574,
17.7107831679876));
#202413=CARTESIAN_POINT('Ctrl Pts',(-18.8964911736824,21.3269977588632,
17.7008169090588));
#202414=CARTESIAN_POINT('Ctrl Pts',(-19.0680941647076,21.3016160512741,
17.6894824109724));
#202415=CARTESIAN_POINT('Ctrl Pts',(-19.0923699971672,21.2975918133585,
17.6878831494053));
#202416=CARTESIAN_POINT('Ctrl Pts',(-19.1336879945986,21.2900000956134,
17.6851737561915));
#202417=CARTESIAN_POINT('Ctrl Pts',(-19.1507662212408,21.2866439575585,
17.6840575710416));
#202418=CARTESIAN_POINT('Ctrl Pts',(-19.2014517908399,21.2760326371987,
17.68075953865));
#202419=CARTESIAN_POINT('Ctrl Pts',(-19.234927723046,21.2681686119622,17.6786005102154));
#202420=CARTESIAN_POINT('Ctrl Pts',(-19.2749606341334,21.2577289552398,
17.6760537072737));
#202421=CARTESIAN_POINT('Ctrl Pts',(-19.281713263303,21.2559322747254,17.6756253352694));
#202422=CARTESIAN_POINT('Ctrl Pts',(-19.2927662000449,21.2529327292171,
17.6749262962257));
#202423=CARTESIAN_POINT('Ctrl Pts',(-19.2970717556372,21.2517496504495,
17.6746545255179));
#202424=CARTESIAN_POINT('Ctrl Pts',(-19.3048060212234,21.2495980917104,
17.6741673305775));
#202425=CARTESIAN_POINT('Ctrl Pts',(-19.3082360407309,21.2486345755521,
17.6739516244455));
#202426=CARTESIAN_POINT('Ctrl Pts',(-19.3156983919501,21.2465180100373,
17.6734831149007));
#202427=CARTESIAN_POINT('Ctrl Pts',(-19.3197297216952,21.2453616399762,
17.6732305075531));
#202428=CARTESIAN_POINT('Ctrl Pts',(-19.3310810019851,21.2420690341085,
17.6725205431446));
#202429=CARTESIAN_POINT('Ctrl Pts',(-19.3383929711427,21.2399051936171,
17.672064765109));
#202430=CARTESIAN_POINT('Ctrl Pts',(-19.3828137042124,21.2264982581414,
17.6693044194649));
#202431=CARTESIAN_POINT('Ctrl Pts',(-19.4196220666681,21.2142761319886,
17.667053425374));
#202432=CARTESIAN_POINT('Ctrl Pts',(-19.6072900349678,21.1461820192928,
17.6556662031394));
#202433=CARTESIAN_POINT('Ctrl Pts',(-19.7517706429219,21.0742546919518,
17.6471669127988));
#202434=CARTESIAN_POINT('Ctrl Pts',(-19.9805519550366,20.9257338806469,
17.6322084729279));
#202435=CARTESIAN_POINT('Ctrl Pts',(-20.0693962758234,20.8574859732337,
17.6259478962023));
#202436=CARTESIAN_POINT('Ctrl Pts',(-20.1629762519826,20.7730236270999,
17.618562114518));
#202437=CARTESIAN_POINT('Ctrl Pts',(-20.1734290681947,20.7633964968133,
17.617725214094));
#202438=CARTESIAN_POINT('Ctrl Pts',(-20.1899281862006,20.7478907606142,
17.616384630862));
#202439=CARTESIAN_POINT('Ctrl Pts',(-20.1960377677347,20.7420798986383,
17.6158838479257));
#202440=CARTESIAN_POINT('Ctrl Pts',(-20.206761648039,20.7317576303522,17.6149970039737));
#202441=CARTESIAN_POINT('Ctrl Pts',(-20.2113903636002,20.7272613080624,
17.6146116014342));
#202442=CARTESIAN_POINT('Ctrl Pts',(-20.2209311219444,20.717908276504,17.6138117228439));
#202443=CARTESIAN_POINT('Ctrl Pts',(-20.2258400906605,20.71304855359,17.6133971164644));
#202444=CARTESIAN_POINT('Ctrl Pts',(-20.2379841116499,20.7009080999245,
17.6123637774134));
#202445=CARTESIAN_POINT('Ctrl Pts',(-20.2451901055315,20.6935986690433,
17.611743772359));
#202446=CARTESIAN_POINT('Ctrl Pts',(-20.2743289188332,20.6636084412211,
17.6092083273068));
#202447=CARTESIAN_POINT('Ctrl Pts',(-20.2958056583352,20.6404920002535,
17.6072732809639));
#202448=CARTESIAN_POINT('Ctrl Pts',(-20.3496120081945,20.5799172378429,
17.6022484230892));
#202449=CARTESIAN_POINT('Ctrl Pts',(-20.3811581764752,20.5417914567174,
17.5991283981105));
#202450=CARTESIAN_POINT('Ctrl Pts',(-20.456884626703,20.4434490420288,17.5911881263281));
#202451=CARTESIAN_POINT('Ctrl Pts',(-20.4992672687428,20.3819364192391,
17.5863149739154));
#202452=CARTESIAN_POINT('Ctrl Pts',(-20.6123298743042,20.1977075209771,
17.5720784258114));
#202453=CARTESIAN_POINT('Ctrl Pts',(-20.674057921606,20.0699982049781,17.5626201593295));
#202454=CARTESIAN_POINT('Ctrl Pts',(-20.722580618353,19.9371102700768,17.5536949396865));
#202455=CARTESIAN_POINT('Ctrl Pts',(-20.7225806054527,19.9371103054064,
17.3329786569753));
#202456=CARTESIAN_POINT('Ctrl Pts',(-20.7107372615498,19.9695453828509,
17.3348698511496));
#202457=CARTESIAN_POINT('Ctrl Pts',(-20.69809355522,20.0017093644426,17.3367731947366));
#202458=CARTESIAN_POINT('Ctrl Pts',(-20.6631258654366,20.084632120709,17.3417759629018));
#202459=CARTESIAN_POINT('Ctrl Pts',(-20.6395993912192,20.1348235723141,
17.3448999022645));
#202460=CARTESIAN_POINT('Ctrl Pts',(-20.5983005827594,20.2146228301491,
17.3500686680486));
#202461=CARTESIAN_POINT('Ctrl Pts',(-20.5817252546882,20.2448213735337,
17.3520736077853));
#202462=CARTESIAN_POINT('Ctrl Pts',(-20.5589828763181,20.2839602388475,
17.3547432045851));
#202463=CARTESIAN_POINT('Ctrl Pts',(-20.55347284462,20.2932775679583,17.3553841308147));
#202464=CARTESIAN_POINT('Ctrl Pts',(-20.5443331076743,20.3084655674537,
17.3564379653732));
#202465=CARTESIAN_POINT('Ctrl Pts',(-20.5407456763262,20.314361541758,17.3568493259298));
#202466=CARTESIAN_POINT('Ctrl Pts',(-20.5337470645155,20.3257381650232,
17.357647510178));
#202467=CARTESIAN_POINT('Ctrl Pts',(-20.5303395160898,20.3312209667267,
17.3580341970362));
#202468=CARTESIAN_POINT('Ctrl Pts',(-20.5224157843031,20.3438412605666,
17.3589289750136));
#202469=CARTESIAN_POINT('Ctrl Pts',(-20.5178818789106,20.350967446049,17.3594377194915));
#202470=CARTESIAN_POINT('Ctrl Pts',(-20.5055785197891,20.3700521632243,
17.3608097327707));
#202471=CARTESIAN_POINT('Ctrl Pts',(-20.4977307779454,20.381959476737,17.3616759144424));
#202472=CARTESIAN_POINT('Ctrl Pts',(-20.4097690748589,20.5125324609073,
17.3712886761429));
#202473=CARTESIAN_POINT('Ctrl Pts',(-20.3179499613997,20.6228347390983,
17.3804995450441));
#202474=CARTESIAN_POINT('Ctrl Pts',(-20.1284438847175,20.8085445979911,
17.3979634441502));
#202475=CARTESIAN_POINT('Ctrl Pts',(-20.0339203875375,20.8863599849291,
17.4061169907457));
#202476=CARTESIAN_POINT('Ctrl Pts',(-19.9081786424971,20.972793436586,17.4159185159027));
#202477=CARTESIAN_POINT('Ctrl Pts',(-19.882778923142,20.9894596629663,17.4178489467286));
#202478=CARTESIAN_POINT('Ctrl Pts',(-19.846394270088,21.0122288441255,17.4205360087966));
#202479=CARTESIAN_POINT('Ctrl Pts',(-19.8357012363898,21.0187889155282,
17.4213163850369));
#202480=CARTESIAN_POINT('Ctrl Pts',(-19.8192281999252,21.0286945109135,
17.4225036333364));
#202481=CARTESIAN_POINT('Ctrl Pts',(-19.8134898179126,21.0321082660285,
17.4229144617344));
#202482=CARTESIAN_POINT('Ctrl Pts',(-19.8039959216146,21.0376955284253,
17.4235895119217));
#202483=CARTESIAN_POINT('Ctrl Pts',(-19.8002497525258,21.0398847125606,
17.4238546919686));
#202484=CARTESIAN_POINT('Ctrl Pts',(-19.7929983829729,21.0440924104025,
17.4243656669975));
#202485=CARTESIAN_POINT('Ctrl Pts',(-19.7894940794257,21.0461124241158,
17.4246115563074));
#202486=CARTESIAN_POINT('Ctrl Pts',(-19.7829733771193,21.049846347518,17.4250671303521));
#202487=CARTESIAN_POINT('Ctrl Pts',(-19.7799585842192,21.0515628693513,
17.4252769791314));
#202488=CARTESIAN_POINT('Ctrl Pts',(-19.7730363508562,21.0554816558671,
17.4257570326747));
#202489=CARTESIAN_POINT('Ctrl Pts',(-19.7691261314201,21.0576789136537,
17.4260269140089));
#202490=CARTESIAN_POINT('Ctrl Pts',(-19.7575850076347,21.0641160076553,
17.4268197693601));
#202491=CARTESIAN_POINT('Ctrl Pts',(-19.7499347208584,21.0683211500908,
17.4273405733387));
#202492=CARTESIAN_POINT('Ctrl Pts',(-19.6951764371157,21.0979806341236,
17.4310360739689));
#202493=CARTESIAN_POINT('Ctrl Pts',(-19.6471394695405,21.1216892463029,
17.434108625441));
#202494=CARTESIAN_POINT('Ctrl Pts',(-19.4916634117191,21.1912192252019,
17.4436851942316));
#202495=CARTESIAN_POINT('Ctrl Pts',(-19.3813085562977,21.2299891372507,
17.4499509611491));
#202496=CARTESIAN_POINT('Ctrl Pts',(-19.1761931552175,21.283490717544,17.4614898217016));
#202497=CARTESIAN_POINT('Ctrl Pts',(-19.0825624455541,21.3012762190636,
17.4667180555095));
#202498=CARTESIAN_POINT('Ctrl Pts',(-18.9385360012558,21.3186864959933,
17.4749610431713));
#202499=CARTESIAN_POINT('Ctrl Pts',(-18.8888203583134,21.3229203160779,
17.477840919349));
#202500=CARTESIAN_POINT('Ctrl Pts',(-18.8267333282971,21.3260036588071,
17.4814992759886));
#202501=CARTESIAN_POINT('Ctrl Pts',(-18.8144575320636,21.3265062096081,
17.4822255760903));
#202502=CARTESIAN_POINT('Ctrl Pts',(-18.7949570560709,21.3271345507961,
17.4833843065467));
#202503=CARTESIAN_POINT('Ctrl Pts',(-18.7877347897942,21.3273302601763,
17.4838145419713));
#202504=CARTESIAN_POINT('Ctrl Pts',(-18.7741378589279,21.3276290648453,
17.484626615893));
#202505=CARTESIAN_POINT('Ctrl Pts',(-18.7677634412721,21.3277403417811,
17.4850081932904));
#202506=CARTESIAN_POINT('Ctrl Pts',(-18.7534248828736,21.3279258623002,
17.48586850014));
#202507=CARTESIAN_POINT('Ctrl Pts',(-18.7454606624291,21.3279839590941,
17.4863477305348));
#202508=CARTESIAN_POINT('Ctrl Pts',(-18.7251431478532,21.3280175150718,
17.4875738974931));
#202509=CARTESIAN_POINT('Ctrl Pts',(-18.7127901773076,21.3279297901023,
17.4883228012243));
#202510=CARTESIAN_POINT('Ctrl Pts',(-18.6394447694136,21.3267668882894,
17.4927901495022));
#202511=CARTESIAN_POINT('Ctrl Pts',(-18.5785264392339,21.323164056277,17.4965870761019));
#202512=CARTESIAN_POINT('Ctrl Pts',(-18.3707966944676,21.3018433151371,
17.5098383270292));
#202513=CARTESIAN_POINT('Ctrl Pts',(-18.2257395968538,21.2713892263614,
17.5196499713553));
#202514=CARTESIAN_POINT('Ctrl Pts',(-18.0159111296659,21.2038157892865,
17.5341823189913));
#202515=CARTESIAN_POINT('Ctrl Pts',(-17.947949759154,21.1780009850968,17.5389378098836));
#202516=CARTESIAN_POINT('Ctrl Pts',(-17.8503835164574,21.13507447377,17.5457198782743));
#202517=CARTESIAN_POINT('Ctrl Pts',(-17.8196518391715,21.1206618586582,
17.5478489603545));
#202518=CARTESIAN_POINT('Ctrl Pts',(-17.7827140675482,21.1022424156838,
17.5503876257111));
#202519=CARTESIAN_POINT('Ctrl Pts',(-17.7761670036374,21.0989350504891,
17.5508367994235));
#202520=CARTESIAN_POINT('Ctrl Pts',(-17.7659600340271,21.0937120560369,
17.5515356676651));
#202521=CARTESIAN_POINT('Ctrl Pts',(-17.7622883941272,21.0918196663564,
17.5517867789505));
#202522=CARTESIAN_POINT('Ctrl Pts',(-17.7554545829876,21.0882721180536,
17.5522535926805));
#202523=CARTESIAN_POINT('Ctrl Pts',(-17.7522910915845,21.086619726321,17.5524694583381));
#202524=CARTESIAN_POINT('Ctrl Pts',(-17.7451036055166,21.0828423086251,
17.5529593974633));
#202525=CARTESIAN_POINT('Ctrl Pts',(-17.7410822833731,21.0807123084254,
17.5532331521132));
#202526=CARTESIAN_POINT('Ctrl Pts',(-17.7288253931758,21.0741694250837,
17.5540665408118));
#202527=CARTESIAN_POINT('Ctrl Pts',(-17.7206120161803,21.0697149050539,
17.5546236018812));
#202528=CARTESIAN_POINT('Ctrl Pts',(-17.6513704198039,21.0315663617996,
17.5593102676685));
#202529=CARTESIAN_POINT('Ctrl Pts',(-17.5920046723172,20.9949275328306,
17.5632659062163));
#202530=CARTESIAN_POINT('Ctrl Pts',(-17.4067875931376,20.8675737749099,
17.5757546912446));
#202531=CARTESIAN_POINT('Ctrl Pts',(-17.2890612848439,20.7659550599222,
17.5839596662159));
#202532=CARTESIAN_POINT('Ctrl Pts',(-17.130037604616,20.5948915937186,17.5969243318276));
#202533=CARTESIAN_POINT('Ctrl Pts',(-17.079833929813,20.5344742189831,17.6013673154118));
#202534=CARTESIAN_POINT('Ctrl Pts',(-17.0216305412835,20.4559301973032,
17.6070725164429));
#202535=CARTESIAN_POINT('Ctrl Pts',(-17.0103694539777,20.440291691923,17.6082049787826));
#202536=CARTESIAN_POINT('Ctrl Pts',(-16.9943717466052,20.4174232963172,
17.6098570282562));
#202537=CARTESIAN_POINT('Ctrl Pts',(-16.9894632311524,20.4103144244406,
17.6103700374884));
#202538=CARTESIAN_POINT('Ctrl Pts',(-16.9809590426679,20.3978353580696,
17.6112697253927));
#202539=CARTESIAN_POINT('Ctrl Pts',(-16.9773441712078,20.3924783379263,
17.6116556697315));
#202540=CARTESIAN_POINT('Ctrl Pts',(-16.9703908196474,20.3820714346777,
17.6124049401289));
#202541=CARTESIAN_POINT('Ctrl Pts',(-16.9670493560623,20.3770236133315,
17.612768148682));
#202542=CARTESIAN_POINT('Ctrl Pts',(-16.9591417351451,20.3649658265094,
17.6136352578056));
#202543=CARTESIAN_POINT('Ctrl Pts',(-16.9545954158748,20.3579430290676,
17.614139894276));
#202544=CARTESIAN_POINT('Ctrl Pts',(-16.9384994771111,20.3327532279346,
17.6159486811806));
#202545=CARTESIAN_POINT('Ctrl Pts',(-16.9271857870728,20.3144377093108,
17.6172615160218));
#202546=CARTESIAN_POINT('Ctrl Pts',(-16.8182812837237,20.1319675156603,
17.6303220639662));
#202547=CARTESIAN_POINT('Ctrl Pts',(-16.7430660574381,19.9555208824072,
17.6429233810988));
#202548=CARTESIAN_POINT('Ctrl Pts',(-16.6722305095885,19.6974930882674,
17.6605786701504));
#202549=CARTESIAN_POINT('Ctrl Pts',(-16.6559617673459,19.6224944254427,
17.6656084794748));
#202550=CARTESIAN_POINT('Ctrl Pts',(-16.6382338312498,19.5121375158887,
17.6727274943662));
#202551=CARTESIAN_POINT('Ctrl Pts',(-16.6335311845082,19.4773657733027,
17.6749300831848));
#202552=CARTESIAN_POINT('Ctrl Pts',(-16.6288846328592,19.4351275686235,
17.6775440286927));
#202553=CARTESIAN_POINT('Ctrl Pts',(-16.6281132376696,19.4277598301391,
17.6779977238622));
#202554=CARTESIAN_POINT('Ctrl Pts',(-16.6269703931374,19.4162618562939,
17.6787020646977));
#202555=CARTESIAN_POINT('Ctrl Pts',(-16.6265723866486,19.4121344053361,
17.6789541628302));
#202556=CARTESIAN_POINT('Ctrl Pts',(-16.625854545772,19.4044540481614,17.6794218558287));
#202557=CARTESIAN_POINT('Ctrl Pts',(-16.6255315674642,19.4009015381619,
17.6796376197926));
#202558=CARTESIAN_POINT('Ctrl Pts',(-16.6248189947903,19.3928378102745,
17.6801261078331));
#202559=CARTESIAN_POINT('Ctrl Pts',(-16.6244348941075,19.3883261595433,
17.6803985207111));
#202560=CARTESIAN_POINT('Ctrl Pts',(-16.6234780888912,19.376644205732,17.6811016369797));
#202561=CARTESIAN_POINT('Ctrl Pts',(-16.6229274429083,19.3694720864936,
17.681531132493));
#202562=CARTESIAN_POINT('Ctrl Pts',(-16.6197242451253,19.3247664981104,
17.6841954659425));
#202563=CARTESIAN_POINT('Ctrl Pts',(-16.618036014944,19.2871681597603,17.686379984521));
#202564=CARTESIAN_POINT('Ctrl Pts',(-16.6171148458618,19.2365798023398,
17.6892673807175));
#202565=CARTESIAN_POINT('Ctrl Pts',(-16.6169978857392,19.2236151706559,
17.6900027761428));
#202566=CARTESIAN_POINT('Ctrl Pts',(-16.6170042896852,19.1848747290861,
17.692188689228));
#202567=CARTESIAN_POINT('Ctrl Pts',(-16.6174792879254,19.1591008864693,
17.6936276784161));
#202568=CARTESIAN_POINT('Ctrl Pts',(-16.6200590283671,19.0888235659277,
17.6975244091758));
#202569=CARTESIAN_POINT('Ctrl Pts',(-16.623098011573,19.0443670984207,17.6999600550654));
#202570=CARTESIAN_POINT('Ctrl Pts',(-16.6384332104871,18.8912442291542,
17.7083383509827));
#202571=CARTESIAN_POINT('Ctrl Pts',(-16.657741016693,18.7834585732879,17.7142258926028));
#202572=CARTESIAN_POINT('Ctrl Pts',(-16.7043530048111,18.6044115055277,
17.7245135041554));
#202573=CARTESIAN_POINT('Ctrl Pts',(-16.7273314285105,18.5322540763416,
17.7288036395353));
#202574=CARTESIAN_POINT('Ctrl Pts',(-16.760811013953,18.4438160500737,17.7343245780101));
#202575=CARTESIAN_POINT('Ctrl Pts',(-16.7677364774085,18.42623652406,17.7354352202146));
#202576=CARTESIAN_POINT('Ctrl Pts',(-16.7781438865704,18.4008214316912,
17.7370611386422));
#202577=CARTESIAN_POINT('Ctrl Pts',(-16.7814397140792,18.392910288821,17.7375701289746));
#202578=CARTESIAN_POINT('Ctrl Pts',(-16.7873007030189,18.3790790468757,
17.7384651578349));
#202579=CARTESIAN_POINT('Ctrl Pts',(-16.7898450758653,18.3731502195176,
17.7388504851312));
#202580=CARTESIAN_POINT('Ctrl Pts',(-16.794837010872,18.3616633272829,17.7396003275869));
#202581=CARTESIAN_POINT('Ctrl Pts',(-16.7972814688259,18.3561039760079,
17.7399647335836));
#202582=CARTESIAN_POINT('Ctrl Pts',(-16.8031802346635,18.342843753052,17.740837550642));
#202583=CARTESIAN_POINT('Ctrl Pts',(-16.8066567211035,18.3351529143772,
17.7413467199704));
#202584=CARTESIAN_POINT('Ctrl Pts',(-16.8193553198058,18.3075022473958,
17.7431880817465));
#202585=CARTESIAN_POINT('Ctrl Pts',(-16.828842015343,18.2876661293805,17.7445293717071));
#202586=CARTESIAN_POINT('Ctrl Pts',(-16.921854595549,18.1007209015869,17.7573689595346));
#202587=CARTESIAN_POINT('Ctrl Pts',(-17.0268335037852,17.9452413153183,
17.7696787408762));
#202588=CARTESIAN_POINT('Ctrl Pts',(-17.2034837459381,17.7462457880477,
17.787244444502));
#202589=CARTESIAN_POINT('Ctrl Pts',(-17.259457919604,17.6899108344471,17.7924557967283));
#202590=CARTESIAN_POINT('Ctrl Pts',(-17.3450960810183,17.6129019148492,
17.7997960844044));
#202591=CARTESIAN_POINT('Ctrl Pts',(-17.3723311964465,17.5896332902146,
17.8020457991995));
#202592=CARTESIAN_POINT('Ctrl Pts',(-17.4059330237369,17.5623694606464,
17.8047078690292));
#202593=CARTESIAN_POINT('Ctrl Pts',(-17.4117455114608,17.5577040131707,
17.8051643693612));
#202594=CARTESIAN_POINT('Ctrl Pts',(-17.4208377280944,17.5504846813245,
17.8058721037866));
#202595=CARTESIAN_POINT('Ctrl Pts',(-17.4241004777766,17.5479096481919,
17.8061248126904));
#202596=CARTESIAN_POINT('Ctrl Pts',(-17.430176662357,17.5431431651432,17.806593056121));
#202597=CARTESIAN_POINT('Ctrl Pts',(-17.4329880236853,17.5409492357654,
17.8068087633725));
#202598=CARTESIAN_POINT('Ctrl Pts',(-17.4393708521949,17.5359941049726,
17.8072963816911));
#202599=CARTESIAN_POINT('Ctrl Pts',(-17.4429456064722,17.5332372239965,
17.8075679861549));
#202600=CARTESIAN_POINT('Ctrl Pts',(-17.4535664186062,17.5251004083867,
17.8083706246931));
#202601=CARTESIAN_POINT('Ctrl Pts',(-17.4606375820238,17.5197531971771,
17.8088994079338));
#202602=CARTESIAN_POINT('Ctrl Pts',(-17.5135329503136,17.4802735547926,
17.8128151609077));
#202603=CARTESIAN_POINT('Ctrl Pts',(-17.5606929769423,17.4479612299922,
17.8160856481336));
#202604=CARTESIAN_POINT('Ctrl Pts',(-17.7373522143991,17.3371537717986,
17.8277772353816));
#202605=CARTESIAN_POINT('Ctrl Pts',(-17.8738610968989,17.2706976737131,
17.8357925855879));
#202606=CARTESIAN_POINT('Ctrl Pts',(-18.1035158456062,17.1879395951192,
17.8492379777048));
#202607=CARTESIAN_POINT('Ctrl Pts',(-18.1926940813409,17.1622763248223,
17.8544437674218));
#202608=CARTESIAN_POINT('Ctrl Pts',(-18.3038463519949,17.1380550581362,
17.8610702493794));
#202609=CARTESIAN_POINT('Ctrl Pts',(-18.3244972738103,17.1338769023156,
17.8623067836611));
#202610=CARTESIAN_POINT('Ctrl Pts',(-18.3540092729156,17.1283631522901,
17.8640829019583));
#202611=CARTESIAN_POINT('Ctrl Pts',(-18.3628222045709,17.1267744285859,
17.8646144252363));
#202612=CARTESIAN_POINT('Ctrl Pts',(-18.3780651986401,17.124126289835,17.8655358187572));
#202613=CARTESIAN_POINT('Ctrl Pts',(-18.3844906078812,17.123040553949,17.865924846753));
#202614=CARTESIAN_POINT('Ctrl Pts',(-18.3968182773979,17.1210159801144,
17.8666724770175));
#202615=CARTESIAN_POINT('Ctrl Pts',(-18.4027197092853,17.1200724342341,
17.8670309256468));
#202616=CARTESIAN_POINT('Ctrl Pts',(-18.4181096284813,17.1176786181755,
17.867967160809));
#202617=CARTESIAN_POINT('Ctrl Pts',(-18.4276040451626,17.1162678814382,
17.8685461945864));
#202618=CARTESIAN_POINT('Ctrl Pts',(-18.4601866623367,17.1116528193219,
17.8705384378405));
#202619=CARTESIAN_POINT('Ctrl Pts',(-18.483317371144,17.1087653603039,17.8719615972887));
#202620=CARTESIAN_POINT('Ctrl Pts',(-18.6762834447713,17.0879068901408,
17.8839119107713));
#202621=CARTESIAN_POINT('Ctrl Pts',(-18.8476432299002,17.0901701865104,
17.8951009097751));
#202622=CARTESIAN_POINT('Ctrl Pts',(-19.1063740477653,17.1250493423621,
17.9123529957993));
#202623=CARTESIAN_POINT('Ctrl Pts',(-19.1950575677666,17.1428412794891,
17.9183161543863));
#202624=CARTESIAN_POINT('Ctrl Pts',(-19.3196739190989,17.1762593939394,
17.926559300344));
#202625=CARTESIAN_POINT('Ctrl Pts',(-19.3567321142378,17.1872933950379,
17.9289921969329));
#202626=CARTESIAN_POINT('Ctrl Pts',(-19.4007094570309,17.2017101891573,
17.9318403551817));
#202627=CARTESIAN_POINT('Ctrl Pts',(-19.4079362977276,17.2041225959948,
17.9323071167012));
#202628=CARTESIAN_POINT('Ctrl Pts',(-19.419119572097,17.2079229299966,17.9330272534485));
#202629=CARTESIAN_POINT('Ctrl Pts',(-19.423085085747,17.2092836560222,17.933282186451));
#202630=CARTESIAN_POINT('Ctrl Pts',(-19.4304131490909,17.211822564126,17.9337524721009));
#202631=CARTESIAN_POINT('Ctrl Pts',(-19.43377673889,17.2129974448585,17.9339680105886));
#202632=CARTESIAN_POINT('Ctrl Pts',(-19.4413507316474,17.2156644654282,
17.9344526336642));
#202633=CARTESIAN_POINT('Ctrl Pts',(-19.4455593750435,17.2171614384018,
17.9347214276589));
#202634=CARTESIAN_POINT('Ctrl Pts',(-19.4578987888647,17.2215944927505,
17.9355081380936));
#202635=CARTESIAN_POINT('Ctrl Pts',(-19.4660164632558,17.2245671085841,
17.9360239344966));
#202636=CARTESIAN_POINT('Ctrl Pts',(-19.5224620839178,17.2456299683968,
17.9395997359455));
#202637=CARTESIAN_POINT('Ctrl Pts',(-19.570136866398,17.2654337864405,17.9425649448127));
#202638=CARTESIAN_POINT('Ctrl Pts',(-19.6369258537576,17.2960868296322,
17.9467038075734));
#202639=CARTESIAN_POINT('Ctrl Pts',(-19.6566654900655,17.3055194866697,
17.9479250922272));
#202640=CARTESIAN_POINT('Ctrl Pts',(-19.7995548873995,17.3765408966788,
17.9567753038505));
#202641=CARTESIAN_POINT('Ctrl Pts',(-19.916583287637,17.4497087583583,17.9640986673369));
#202642=CARTESIAN_POINT('Ctrl Pts',(-20.0975674204316,17.5890858973673,
17.9766928902694));
#202643=CARTESIAN_POINT('Ctrl Pts',(-20.1658131855151,17.6490045663342,
17.9817933921475));
#202644=CARTESIAN_POINT('Ctrl Pts',(-20.2447378821601,17.7278297923862,
17.9882924957569));
#202645=CARTESIAN_POINT('Ctrl Pts',(-20.2592564965341,17.74276453268,17.9895151166081));
#202646=CARTESIAN_POINT('Ctrl Pts',(-20.2796703579813,17.7643930734421,
17.9912747006375));
#202647=CARTESIAN_POINT('Ctrl Pts',(-20.2857476201939,17.7709139695741,
17.9918038099723));
#202648=CARTESIAN_POINT('Ctrl Pts',(-20.2961911316462,17.7822627122393,
17.9927223534401));
#202649=CARTESIAN_POINT('Ctrl Pts',(-20.3005766617647,17.7870727088133,
17.9931109595467));
#202650=CARTESIAN_POINT('Ctrl Pts',(-20.3089521410906,17.7963443603903,
17.993858720674));
#202651=CARTESIAN_POINT('Ctrl Pts',(-20.3129454934828,17.800802867372,17.9942177265764));
#202652=CARTESIAN_POINT('Ctrl Pts',(-20.3233262651086,17.8124921857426,
17.9951575132199));
#202653=CARTESIAN_POINT('Ctrl Pts',(-20.3296832024114,17.8197497722463,
17.9957395598317));
#202654=CARTESIAN_POINT('Ctrl Pts',(-20.3514219108505,17.8449134054578,
17.997752883754));
#202655=CARTESIAN_POINT('Ctrl Pts',(-20.366553229559,17.8630326030041,17.9991943958255));
#202656=CARTESIAN_POINT('Ctrl Pts',(-20.4850678414537,18.0098725749781,
18.0108162033018));
#202657=CARTESIAN_POINT('Ctrl Pts',(-20.5733548934424,18.1500100955293,
18.0216100250107));
#202658=CARTESIAN_POINT('Ctrl Pts',(-20.6994383638687,18.4141136283923,
18.0409499476056));
#202659=CARTESIAN_POINT('Ctrl Pts',(-20.7438992365239,18.534030521824,18.0493910847454));
#202660=CARTESIAN_POINT('Ctrl Pts',(-20.7804090212664,18.6687441839928,
18.0580465963771));
#202661=CARTESIAN_POINT('Ctrl Pts',(-20.7834316336782,18.6802823290836,
18.0587813705075));
#202662=CARTESIAN_POINT('Ctrl Pts',(-20.787589128825,18.6967180262668,18.0598181150712));
#202663=CARTESIAN_POINT('Ctrl Pts',(-20.7888042685242,18.701594780371,18.0601244989699));
#202664=CARTESIAN_POINT('Ctrl Pts',(-20.7908681038565,18.7100051802587,
18.060650701977));
#202665=CARTESIAN_POINT('Ctrl Pts',(-20.7917250850009,18.7135367537126,
18.0608709949494));
#202666=CARTESIAN_POINT('Ctrl Pts',(-20.7933688049623,18.7203873630446,
18.0612970197116));
#202667=CARTESIAN_POINT('Ctrl Pts',(-20.794156616175,18.7237060932013,18.0615028153574));
#202668=CARTESIAN_POINT('Ctrl Pts',(-20.7962599601198,18.7326629064712,
18.0620566780443));
#202669=CARTESIAN_POINT('Ctrl Pts',(-20.7975604026104,18.7383045539363,
18.0624038835368));
#202670=CARTESIAN_POINT('Ctrl Pts',(-20.802298076856,18.7592499787697,18.063687031871));
#202671=CARTESIAN_POINT('Ctrl Pts',(-20.8055884394109,18.7745869082983,
18.0646149284832));
#202672=CARTESIAN_POINT('Ctrl Pts',(-20.8354454531704,18.9217095450431,
18.0734168415235));
#202673=CARTESIAN_POINT('Ctrl Pts',(-20.8495760153237,19.0557259553302,
18.0806879720517));
#202674=CARTESIAN_POINT('Ctrl Pts',(-20.8509595374546,19.1964793462705,
18.0883318990536));
#202675=CARTESIAN_POINT('Ctrl Pts',(-20.8509933270319,19.2027667816616,
18.0886733340331));
#202676=CARTESIAN_POINT('Ctrl Pts',(-20.8511331455446,19.3548927652846,
18.0969355644505));
#202677=CARTESIAN_POINT('Ctrl Pts',(-20.8361978951726,19.5003359712167,
18.1048962803306));
#202678=CARTESIAN_POINT('Ctrl Pts',(-20.8015323056837,19.6666057069565,
18.1147555389692));
#202679=CARTESIAN_POINT('Ctrl Pts',(-20.7962279558318,19.690042987735,18.1161623214917));
#202680=CARTESIAN_POINT('Ctrl Pts',(-20.7882195563418,19.7228256285329,
18.1181560508981));
#202681=CARTESIAN_POINT('Ctrl Pts',(-20.7858481762291,19.7322509152032,
18.1187323030259));
#202682=CARTESIAN_POINT('Ctrl Pts',(-20.7819083815182,19.7474664419076,
18.1196676110311));
#202683=CARTESIAN_POINT('Ctrl Pts',(-20.7803800924553,19.7532669992248,
18.1200253656573));
#202684=CARTESIAN_POINT('Ctrl Pts',(-20.7771446742239,19.7653384144605,
18.1207723986571));
#202685=CARTESIAN_POINT('Ctrl Pts',(-20.7754332818565,19.7716080554388,
18.1211618120893));
#202686=CARTESIAN_POINT('Ctrl Pts',(-20.7713216373953,19.7864024486274,
18.1220841100033));
#202687=CARTESIAN_POINT('Ctrl Pts',(-20.7688967216706,19.7949201662001,
18.1226177924416));
#202688=CARTESIAN_POINT('Ctrl Pts',(-20.7606830621833,19.8230987014574,
18.1243923673513));
#202689=CARTESIAN_POINT('Ctrl Pts',(-20.7546623942917,19.8426901905225,
18.1256408005816));
#202690=CARTESIAN_POINT('Ctrl Pts',(-20.7402319533099,19.8873285460168,
18.1285198080292));
#202691=CARTESIAN_POINT('Ctrl Pts',(-20.7316376301585,19.9123060540526,
18.1301559494639));
#202692=CARTESIAN_POINT('Ctrl Pts',(-20.7225805905512,19.9371103462167,
18.1318063719887));
#202693=CARTESIAN_POINT('Origin',(-18.734,19.211,0.));
#202694=CARTESIAN_POINT('',(-20.7202231500468,19.93627084876,19.1554367712949));
#202695=CARTESIAN_POINT('',(-20.7225805923249,19.9371103413593,18.9348455557956));
#202696=CARTESIAN_POINT('',(-20.7225806064498,19.9371103026755,0.));
#202697=CARTESIAN_POINT('',(-20.8499620916056,19.2091158126,19.1109437209775));
#202698=CARTESIAN_POINT('Ctrl Pts',(-20.8499620916056,19.2091158126,19.1109437209775));
#202699=CARTESIAN_POINT('Ctrl Pts',(-20.8478499414866,19.4559462748795,
19.12577473775));
#202700=CARTESIAN_POINT('Ctrl Pts',(-20.8034780786863,19.7034419500621,
19.1406057545224));
#202701=CARTESIAN_POINT('Ctrl Pts',(-20.7202231500468,19.93627084876,19.1554367712949));
#202702=CARTESIAN_POINT('Ctrl Pts',(-20.8509991255302,19.2090758107338,
19.1115402065938));
#202703=CARTESIAN_POINT('Ctrl Pts',(-20.8509516894146,19.1568864461007,
19.108121049185));
#202704=CARTESIAN_POINT('Ctrl Pts',(-20.8489743712533,19.1047170798901,
19.1046744518397));
#202705=CARTESIAN_POINT('Ctrl Pts',(-20.8355939732812,18.9263061605855,
19.0928511306297));
#202706=CARTESIAN_POINT('Ctrl Pts',(-20.8147881617888,18.8010303123376,
19.0844726261103));
#202707=CARTESIAN_POINT('Ctrl Pts',(-20.7798982971389,18.6668205583257,
19.0758731777046));
#202708=CARTESIAN_POINT('Ctrl Pts',(-20.7768015033896,18.6553084131162,
19.0751387839972));
#202709=CARTESIAN_POINT('Ctrl Pts',(-20.7722613418263,18.6389816869146,
19.0741024790361));
#202710=CARTESIAN_POINT('Ctrl Pts',(-20.7708978864628,18.6341453827811,
19.0737961593069));
#202711=CARTESIAN_POINT('Ctrl Pts',(-20.7685187432036,18.6258199522268,
19.0732700314745));
#202712=CARTESIAN_POINT('Ctrl Pts',(-20.7675112714562,18.6223285174239,
19.0730497498653));
#202713=CARTESIAN_POINT('Ctrl Pts',(-20.7655406248523,18.6155645913163,
19.0726237195193));
#202714=CARTESIAN_POINT('Ctrl Pts',(-20.764578530616,18.6122918342616,19.0724179070573));
#202715=CARTESIAN_POINT('Ctrl Pts',(-20.7619618414276,18.6034695030517,
19.0718639407828));
#202716=CARTESIAN_POINT('Ctrl Pts',(-20.760292365231,18.5979243216301,19.0715166490958));
#202717=CARTESIAN_POINT('Ctrl Pts',(-20.7540140035938,18.5773764977283,
19.0702328458126));
#202718=CARTESIAN_POINT('Ctrl Pts',(-20.7492609525142,18.5624179749817,
19.069304391038));
#202719=CARTESIAN_POINT('Ctrl Pts',(-20.6977077257283,18.4062134970419,
19.0596600658168));
#202720=CARTESIAN_POINT('Ctrl Pts',(-20.6362994852711,18.2702031321059,
19.0516823747842));
#202721=CARTESIAN_POINT('Ctrl Pts',(-20.5205652768002,18.0724387348816,
19.0392298958366));
#202722=CARTESIAN_POINT('Ctrl Pts',(-20.4760980019424,18.0054997670339,
19.0348482182288));
#202723=CARTESIAN_POINT('Ctrl Pts',(-20.3988169588823,17.9024011865837,
19.0276435918523));
#202724=CARTESIAN_POINT('Ctrl Pts',(-20.3683694435708,17.8645667791617,
19.0248921510687));
#202725=CARTESIAN_POINT('Ctrl Pts',(-20.3163399544824,17.8042820051318,
19.0202985329374));
#202726=CARTESIAN_POINT('Ctrl Pts',(-20.2955152301747,17.7812009626752,
19.0184859975746));
#202727=CARTESIAN_POINT('Ctrl Pts',(-20.26717632535,17.7511493625238,19.0160488582923));
#202728=CARTESIAN_POINT('Ctrl Pts',(-20.2601082998709,17.7437621256712,
19.0154433564929));
#202729=CARTESIAN_POINT('Ctrl Pts',(-20.2481822913166,17.7314769101663,
19.0144254279768));
#202730=CARTESIAN_POINT('Ctrl Pts',(-20.2433533296475,17.7265509071584,
19.0140142692992));
#202731=CARTESIAN_POINT('Ctrl Pts',(-20.2339579094634,17.7170599206848,
19.013216201102));
#202732=CARTESIAN_POINT('Ctrl Pts',(-20.2293944668913,17.7124920495025,
19.0128294269554));
#202733=CARTESIAN_POINT('Ctrl Pts',(-20.2188074257031,17.7019912553693,
19.0119340455725));
#202734=CARTESIAN_POINT('Ctrl Pts',(-20.2127690695207,17.6960734279891,
19.0114247821942));
#202735=CARTESIAN_POINT('Ctrl Pts',(-20.1964298236759,17.6802510929699,
19.0100504613606));
#202736=CARTESIAN_POINT('Ctrl Pts',(-20.1860639670904,17.670414583572,19.0091824757563));
#202737=CARTESIAN_POINT('Ctrl Pts',(-20.0900233636271,17.5811088655016,
19.0011746983341));
#202738=CARTESIAN_POINT('Ctrl Pts',(-19.9980197569223,17.5087688997371,
18.9937330845983));
#202739=CARTESIAN_POINT('Ctrl Pts',(-19.7647250564385,17.3547186341645,
18.9754718456826));
#202740=CARTESIAN_POINT('Ctrl Pts',(-19.619033802088,17.2810026174587,18.96451211118));
#202741=CARTESIAN_POINT('Ctrl Pts',(-19.4358588681189,17.2134669361007,
18.952107146499));
#202742=CARTESIAN_POINT('Ctrl Pts',(-19.4051238166674,17.2029319476545,
18.95007122557));
#202743=CARTESIAN_POINT('Ctrl Pts',(-19.3672574607857,17.1909192152583,
18.9476283632737));
#202744=CARTESIAN_POINT('Ctrl Pts',(-19.3603470229541,17.1887658892093,
18.9471851906261));
#202745=CARTESIAN_POINT('Ctrl Pts',(-19.3494960884831,17.1854456434043,
18.9464935907858));
#202746=CARTESIAN_POINT('Ctrl Pts',(-19.3455630824792,17.1842547068579,
18.9462437936542));
#202747=CARTESIAN_POINT('Ctrl Pts',(-19.3382049520362,17.1820499920733,
18.9457781304773));
#202748=CARTESIAN_POINT('Ctrl Pts',(-19.3347807673545,17.1810334415223,
18.945562109106));
#202749=CARTESIAN_POINT('Ctrl Pts',(-19.3269582586138,17.1787326708496,
18.9450701450696));
#202750=CARTESIAN_POINT('Ctrl Pts',(-19.3225583364721,17.1774540627109,
18.9447945317634));
#202751=CARTESIAN_POINT('Ctrl Pts',(-19.3090209435828,17.1735677418406,
18.9439498269588));
#202752=CARTESIAN_POINT('Ctrl Pts',(-19.2998698941502,17.1710072150481,
18.9433834114928));
#202753=CARTESIAN_POINT('Ctrl Pts',(-19.2174761923205,17.1485499798146,
18.9383221687416));
#202754=CARTESIAN_POINT('Ctrl Pts',(-19.1432216932006,17.1325415507712,
18.9340337611397));
#202755=CARTESIAN_POINT('Ctrl Pts',(-18.9181952179629,17.0965600397241,
18.9214210653693));
#202756=CARTESIAN_POINT('Ctrl Pts',(-18.7659829277571,17.0887926840675,
18.9133657723101));
#202757=CARTESIAN_POINT('Ctrl Pts',(-18.559227941065,17.1005070466343,18.901850981901));
#202758=CARTESIAN_POINT('Ctrl Pts',(-18.5043552591716,17.1057711700339,
18.8987436322711));
#202759=CARTESIAN_POINT('Ctrl Pts',(-18.4157574817194,17.1177757841177,
18.893599872603));
#202760=CARTESIAN_POINT('Ctrl Pts',(-18.3818804108329,17.12320750151,18.8916028451718));
#202761=CARTESIAN_POINT('Ctrl Pts',(-18.3375239044313,17.1314297235214,
18.8889422945815));
#202762=CARTESIAN_POINT('Ctrl Pts',(-18.3269115927588,17.1334810828053,
18.8883022975686));
#202763=CARTESIAN_POINT('Ctrl Pts',(-18.309553058374,17.1369745956055,18.8872496021747));
#202764=CARTESIAN_POINT('Ctrl Pts',(-18.3027972696982,17.1383686319131,
18.8868384450124));
#202765=CARTESIAN_POINT('Ctrl Pts',(-18.2897313051546,17.1411314008716,
18.8860403777034));
#202766=CARTESIAN_POINT('Ctrl Pts',(-18.2834203337178,17.1424960348654,
18.8856536029188));
#202767=CARTESIAN_POINT('Ctrl Pts',(-18.2688601920183,17.1457141982544,
18.8847582170681));
#202768=CARTESIAN_POINT('Ctrl Pts',(-18.2606157268999,17.1475883080191,
18.8842489498393));
#202769=CARTESIAN_POINT('Ctrl Pts',(-18.2384672506628,17.1527627672891,
18.8828746118452));
#202770=CARTESIAN_POINT('Ctrl Pts',(-18.2245852508197,17.1561545534074,
18.8820066128172));
#202771=CARTESIAN_POINT('Ctrl Pts',(-18.0974921218371,17.1885742154504,
18.8739978114357));
#202772=CARTESIAN_POINT('Ctrl Pts',(-17.9868506330444,17.2267852069755,
18.8665550976252));
#202773=CARTESIAN_POINT('Ctrl Pts',(-17.7309819747738,17.3395978556687,
18.8482893605931));
#202774=CARTESIAN_POINT('Ctrl Pts',(-17.5900993418143,17.422234360456,18.8373260994925));
#202775=CARTESIAN_POINT('Ctrl Pts',(-17.4341820375042,17.5397090069427,
18.8249224243594));
#202776=CARTESIAN_POINT('Ctrl Pts',(-17.4087356316912,17.5598140807818,
18.8228903476481));
#202777=CARTESIAN_POINT('Ctrl Pts',(-17.3781881188452,17.5851108672491,
18.8204514483935));
#202778=CARTESIAN_POINT('Ctrl Pts',(-17.3726402090257,17.589753303141,18.8200085301963));
#202779=CARTESIAN_POINT('Ctrl Pts',(-17.3639788635493,17.5970768405167,
18.8193172386712));
#202780=CARTESIAN_POINT('Ctrl Pts',(-17.3608493116709,17.5997386720824,
18.8190674973748));
#202781=CARTESIAN_POINT('Ctrl Pts',(-17.355013283545,17.6047318419703,18.8186018825525));
#202782=CARTESIAN_POINT('Ctrl Pts',(-17.3523049887731,17.6070608939741,
18.8183858540368));
#202783=CARTESIAN_POINT('Ctrl Pts',(-17.3461351185857,17.6123940207103,
18.8178938015523));
#202784=CARTESIAN_POINT('Ctrl Pts',(-17.3426774022816,17.615402483059,18.8176181074007));
#202785=CARTESIAN_POINT('Ctrl Pts',(-17.3320758871606,17.6246872294373,
18.8167729084355));
#202786=CARTESIAN_POINT('Ctrl Pts',(-17.3249644703827,17.631000535406,18.816206084201));
#202787=CARTESIAN_POINT('Ctrl Pts',(-17.2286610701478,17.7176631811832,
18.8085279725265));
#202788=CARTESIAN_POINT('Ctrl Pts',(-17.1464047277001,17.8054218983844,
18.8019382913532));
#202789=CARTESIAN_POINT('Ctrl Pts',(-17.0046327502323,17.9851064714334,
18.7894810467888));
#202790=CARTESIAN_POINT('Ctrl Pts',(-16.9439268368985,18.0755867921844,
18.7836199419601));
#202791=CARTESIAN_POINT('Ctrl Pts',(-16.8536586056344,18.235497260102,18.7734039861693));
#202792=CARTESIAN_POINT('Ctrl Pts',(-16.8203558046817,18.3025653263309,
18.7691597391762));
#202793=CARTESIAN_POINT('Ctrl Pts',(-16.7832259174287,18.3884903257147,
18.7636941062077));
#202794=CARTESIAN_POINT('Ctrl Pts',(-16.7760064074826,18.4058275069566,
18.7625900826683));
#202795=CARTESIAN_POINT('Ctrl Pts',(-16.7658374710658,18.4311933896602,
18.7609720988818));
#202796=CARTESIAN_POINT('Ctrl Pts',(-16.7627044009515,18.4391478459372,
18.7604643372393));
#202797=CARTESIAN_POINT('Ctrl Pts',(-16.7572928130651,18.4531350513834,
18.7595707284595));
#202798=CARTESIAN_POINT('Ctrl Pts',(-16.7549935041877,18.4591596769698,
18.7591855855115));
#202799=CARTESIAN_POINT('Ctrl Pts',(-16.7505801062103,18.4708841429516,
18.758435550657));
#202800=CARTESIAN_POINT('Ctrl Pts',(-16.7484629705489,18.4765827749738,
18.7580707653219));
#202801=CARTESIAN_POINT('Ctrl Pts',(-16.7434571483718,18.4902366642788,
18.7571961476977));
#202802=CARTESIAN_POINT('Ctrl Pts',(-16.7405915820036,18.4982002342207,
18.7566855500572));
#202803=CARTESIAN_POINT('Ctrl Pts',(-16.7304040956047,18.5270537659047,
18.7548336947767));
#202804=CARTESIAN_POINT('Ctrl Pts',(-16.7233623787762,18.5480405012563,
18.7534832039145));
#202805=CARTESIAN_POINT('Ctrl Pts',(-16.6604503530236,18.745769212172,18.7407222535653));
#202806=CARTESIAN_POINT('Ctrl Pts',(-16.6277020998735,18.928990290587,18.728514762743));
#202807=CARTESIAN_POINT('Ctrl Pts',(-16.6155433094807,19.1943019699739,
18.7109795572108));
#202808=CARTESIAN_POINT('Ctrl Pts',(-16.6164340970995,19.2746705786126,
18.7057030263833));
#202809=CARTESIAN_POINT('Ctrl Pts',(-16.6243396653045,19.3907872072471,
18.6982836184296));
#202810=CARTESIAN_POINT('Ctrl Pts',(-16.6277094524878,19.4267096579234,
18.6960172700313));
#202811=CARTESIAN_POINT('Ctrl Pts',(-16.6328832983173,19.4699466914154,
18.693338239438));
#202812=CARTESIAN_POINT('Ctrl Pts',(-16.6338099568734,19.477357972771,18.6928807658437));
#202813=CARTESIAN_POINT('Ctrl Pts',(-16.635313775009,19.4888892466954,18.6921718543056));
#202814=CARTESIAN_POINT('Ctrl Pts',(-16.6358638777318,19.493012619428,18.6919189337654));
#202815=CARTESIAN_POINT('Ctrl Pts',(-16.6369080897043,19.5006674552641,
18.6914504985302));
#202816=CARTESIAN_POINT('Ctrl Pts',(-16.6373989625544,19.5041992580581,
18.6912348098564));
#202817=CARTESIAN_POINT('Ctrl Pts',(-16.6385308602937,19.5121949886956,
18.6907474880104));
#202818=CARTESIAN_POINT('Ctrl Pts',(-16.6391772248875,19.5166581070596,
18.69047615987));
#202819=CARTESIAN_POINT('Ctrl Pts',(-16.6408827680919,19.5281752408796,
18.6897776948434));
#202820=CARTESIAN_POINT('Ctrl Pts',(-16.6419633554103,19.535226095327,18.6893517394058));
#202821=CARTESIAN_POINT('Ctrl Pts',(-16.6488138792592,19.5784652562542,
18.6867489664919));
#202822=CARTESIAN_POINT('Ctrl Pts',(-16.6554873799883,19.6145065355942,
18.6846198421916));
#202823=CARTESIAN_POINT('Ctrl Pts',(-16.6985016282384,19.8172531114208,
18.6727801149832));
#202824=CARTESIAN_POINT('Ctrl Pts',(-16.7539571675207,19.979270088939,18.6638037167283));
#202825=CARTESIAN_POINT('Ctrl Pts',(-16.8697799711943,20.2187004902832,
18.649172630837));
#202826=CARTESIAN_POINT('Ctrl Pts',(-16.9170369077137,20.3016047160456,
18.643827422453));
#202827=CARTESIAN_POINT('Ctrl Pts',(-16.9815335280367,20.398858380119,18.6370321384681));
#202828=CARTESIAN_POINT('Ctrl Pts',(-16.9936210628571,20.4164988064763,
18.635777390431));
#202829=CARTESIAN_POINT('Ctrl Pts',(-17.0111774721167,20.4413059336624,
18.6339796512418));
#202830=CARTESIAN_POINT('Ctrl Pts',(-17.0164283373035,20.4486258451847,
18.633444995718));
#202831=CARTESIAN_POINT('Ctrl Pts',(-17.0255634541739,20.4611904494717,
18.6325198962453));
#202832=CARTESIAN_POINT('Ctrl Pts',(-17.029425561523,20.4664511433283,18.6321303130682));
#202833=CARTESIAN_POINT('Ctrl Pts',(-17.0368641792246,20.4764859099862,
18.6313828196084));
#202834=CARTESIAN_POINT('Ctrl Pts',(-17.0404366688373,20.4812628959164,
18.6310250687564));
#202835=CARTESIAN_POINT('Ctrl Pts',(-17.0497729168165,20.493637547185,18.6300933050721));
#202836=CARTESIAN_POINT('Ctrl Pts',(-17.0555678617548,20.5012114159425,
18.629518068344));
#202837=CARTESIAN_POINT('Ctrl Pts',(-17.0754716082051,20.5268641547522,
18.6275526135447));
#202838=CARTESIAN_POINT('Ctrl Pts',(-17.0898225243021,20.544752324703,18.6261528028665));
#202839=CARTESIAN_POINT('Ctrl Pts',(-17.2170159590825,20.6981237804615,
18.6138892561262));
#202840=CARTESIAN_POINT('Ctrl Pts',(-17.3460659156701,20.819226643004,18.6023142772999));
#202841=CARTESIAN_POINT('Ctrl Pts',(-17.5584852768959,20.9737604683381,
18.5849591995691));
#202842=CARTESIAN_POINT('Ctrl Pts',(-17.631430743594,21.0202822526329,18.5792643130506));
#202843=CARTESIAN_POINT('Ctrl Pts',(-17.7399657190424,21.080493057856,18.5713409505952));
#202844=CARTESIAN_POINT('Ctrl Pts',(-17.7733956414394,21.0978884749886,
18.5689712915508));
#202845=CARTESIAN_POINT('Ctrl Pts',(-17.8140744686911,21.1176943174974,
18.5661872042153));
#202846=CARTESIAN_POINT('Ctrl Pts',(-17.8208924054788,21.1209687767929,
18.5657238742943));
#202847=CARTESIAN_POINT('Ctrl Pts',(-17.8315058502969,21.1259962886751,
18.5650078831804));
#202848=CARTESIAN_POINT('Ctrl Pts',(-17.8352891693654,21.1277747179794,
18.5647536921738));
#202849=CARTESIAN_POINT('Ctrl Pts',(-17.8423075547456,21.1310485109308,
18.5642840942205));
#202850=CARTESIAN_POINT('Ctrl Pts',(-17.8455411008406,21.1325468992593,
18.5640685057935));
#202851=CARTESIAN_POINT('Ctrl Pts',(-17.8528501348538,21.1359114281825,
18.5635829123951));
#202852=CARTESIAN_POINT('Ctrl Pts',(-17.8569277632702,21.1377727898229,
18.5633132032368));
#202853=CARTESIAN_POINT('Ctrl Pts',(-17.8689518254206,21.1432154709269,
18.5625213223534));
#202854=CARTESIAN_POINT('Ctrl Pts',(-17.8769146113193,21.1467607323357,
18.5620013126987));
#202855=CARTESIAN_POINT('Ctrl Pts',(-17.9337070100982,21.1716272020756,
18.5583221566122));
#202856=CARTESIAN_POINT('Ctrl Pts',(-17.9833086758754,21.1911493497732,
18.5552641461112));
#202857=CARTESIAN_POINT('Ctrl Pts',(-18.0356440139679,21.2094975895958,
18.5521451003604));
#202858=CARTESIAN_POINT('Ctrl Pts',(-18.0376907282989,21.2102116188758,
18.5520232905384));
#202859=CARTESIAN_POINT('Ctrl Pts',(-18.1790205433749,21.2592734416253,
18.5436234960636));
#202860=CARTESIAN_POINT('Ctrl Pts',(-18.322979181674,21.2929446935847,18.5358056356231));
#202861=CARTESIAN_POINT('Ctrl Pts',(-18.5662414571187,21.3236044769383,
18.522332945513));
#202862=CARTESIAN_POINT('Ctrl Pts',(-18.6639257798467,21.3290951254383,
18.5168602791409));
#202863=CARTESIAN_POINT('Ctrl Pts',(-18.783299637179,21.3275368086815,18.5099105333103));
#202864=CARTESIAN_POINT('Ctrl Pts',(-18.8049598843882,21.3269213502096,
18.5086393390396));
#202865=CARTESIAN_POINT('Ctrl Pts',(-18.8356539658716,21.3255773782255,
18.5068220999333));
#202866=CARTESIAN_POINT('Ctrl Pts',(-18.8446988915386,21.3251231678433,
18.5062846428918));
#202867=CARTESIAN_POINT('Ctrl Pts',(-18.8602650000054,21.3242413149596,
18.505356221637));
#202868=CARTESIAN_POINT('Ctrl Pts',(-18.8667876775168,21.323841484045,18.5049661348351));
#202869=CARTESIAN_POINT('Ctrl Pts',(-18.8792508224765,21.3230195702709,
18.5042187334738));
#202870=CARTESIAN_POINT('Ctrl Pts',(-18.8851915736479,21.3226026078713,
18.5038615834564));
#202871=CARTESIAN_POINT('Ctrl Pts',(-18.9005868951636,21.3214567577393,
18.5029336937404));
#202872=CARTESIAN_POINT('Ctrl Pts',(-18.9100383920755,21.3206894083886,
18.5023617502846));
#202873=CARTESIAN_POINT('Ctrl Pts',(-18.9420029207091,21.3178779737555,
18.5004195299524));
#202874=CARTESIAN_POINT('Ctrl Pts',(-18.9644876566442,21.3155368586171,
18.4990399655902));
#202875=CARTESIAN_POINT('Ctrl Pts',(-19.1659636333705,21.2912917226362,
18.4865540242466));
#202876=CARTESIAN_POINT('Ctrl Pts',(-19.3414790078144,21.2469641746786,
18.4746991957193));
#202877=CARTESIAN_POINT('Ctrl Pts',(-19.5870772016413,21.1503168477156,
18.4572661070518));
#202878=CARTESIAN_POINT('Ctrl Pts',(-19.6630607017603,21.1150847106651,
18.4517594970013));
#202879=CARTESIAN_POINT('Ctrl Pts',(-19.7693186806952,21.0579354803178,
18.444062116749));
#202880=CARTESIAN_POINT('Ctrl Pts',(-19.8014123158424,21.0395750659402,
18.4417382248148));
#202881=CARTESIAN_POINT('Ctrl Pts',(-19.8394398199671,21.0164773291489,
18.4390006181416));
#202882=CARTESIAN_POINT('Ctrl Pts',(-19.8458481296641,21.0125380434795,
18.438539843267));
#202883=CARTESIAN_POINT('Ctrl Pts',(-19.8557774389215,21.0063611833208,
18.4378269401707));
#202884=CARTESIAN_POINT('Ctrl Pts',(-19.8593129767356,21.0041472628124,
18.4375733028131));
#202885=CARTESIAN_POINT('Ctrl Pts',(-19.8658575976277,21.0000221031603,
18.4371042138961));
#202886=CARTESIAN_POINT('Ctrl Pts',(-19.8688683701277,20.9981137316007,
18.4368885841197));
#202887=CARTESIAN_POINT('Ctrl Pts',(-19.8756640900429,20.9937821802581,
18.4364022481211));
#202888=CARTESIAN_POINT('Ctrl Pts',(-19.8794461398497,20.9913545540983,
18.436131841685));
#202889=CARTESIAN_POINT('Ctrl Pts',(-19.8905864055577,20.9841536348853,
18.4353360109431));
#202890=CARTESIAN_POINT('Ctrl Pts',(-19.8979228248307,20.9793465696196,
18.4348127810934));
#202891=CARTESIAN_POINT('Ctrl Pts',(-19.9507592810769,20.9442550936977,
18.4310491635101));
#202892=CARTESIAN_POINT('Ctrl Pts',(-19.9951053824365,20.9122614940637,
18.4279152610807));
#202893=CARTESIAN_POINT('Ctrl Pts',(-20.1707479744334,20.7748967603769,
18.4153889348266));
#202894=CARTESIAN_POINT('Ctrl Pts',(-20.2904962805355,20.6557645756205,
18.4065304697253));
#202895=CARTESIAN_POINT('Ctrl Pts',(-20.4314204825302,20.4774620379215,
18.3939311570114));
#202896=CARTESIAN_POINT('Ctrl Pts',(-20.4660158367833,20.429721775069,18.3906172273238));
#202897=CARTESIAN_POINT('Ctrl Pts',(-20.5184688932347,20.3505861641391,
18.3851630618666));
#202898=CARTESIAN_POINT('Ctrl Pts',(-20.5375946958178,20.3200679886129,
18.3830687427483));
#202899=CARTESIAN_POINT('Ctrl Pts',(-20.5615339482237,20.2796110957751,
18.3802971236516));
#202900=CARTESIAN_POINT('Ctrl Pts',(-20.5670618584833,20.2701006665981,
18.3796459307387));
#202901=CARTESIAN_POINT('Ctrl Pts',(-20.5759561099417,20.2545204149895,
18.3785795032806));
#202902=CARTESIAN_POINT('Ctrl Pts',(-20.5793672076699,20.2484762814373,
18.3781658896052));
#202903=CARTESIAN_POINT('Ctrl Pts',(-20.5858865449141,20.2367907730763,
18.3773663502096));
#202904=CARTESIAN_POINT('Ctrl Pts',(-20.5889988843644,20.231151764664,18.3769805773689));
#202905=CARTESIAN_POINT('Ctrl Pts',(-20.5960893284217,20.2181653992436,
18.3760922473868));
#202906=CARTESIAN_POINT('Ctrl Pts',(-20.6000497474464,20.2108085543667,
18.3755890666401));
#202907=CARTESIAN_POINT('Ctrl Pts',(-20.6105050996627,20.1911082361159,
18.3742417105235));
#202908=CARTESIAN_POINT('Ctrl Pts',(-20.6169216854225,20.1787238529215,
18.3733947830993));
#202909=CARTESIAN_POINT('Ctrl Pts',(-20.6608289641559,20.0918901009572,
18.3674560923311));
#202910=CARTESIAN_POINT('Ctrl Pts',(-20.6940057709894,20.0153675122898,
18.3622160718341));
#202911=CARTESIAN_POINT('Ctrl Pts',(-20.7225806168679,19.9371102741439,
18.3568545763217));
#202912=CARTESIAN_POINT('',(-20.8509999550631,19.2114361911346,18.8870728602009));
#202913=CARTESIAN_POINT('Ctrl Pts',(-20.7225805905512,19.9371103462167,
18.1318063719887));
#202914=CARTESIAN_POINT('Ctrl Pts',(-20.7014550076874,19.9949664617037,
18.1356559894487));
#202915=CARTESIAN_POINT('Ctrl Pts',(-20.6778120315239,20.0518801287616,
18.1395843992343));
#202916=CARTESIAN_POINT('Ctrl Pts',(-20.5968950914491,20.224934280491,18.1519521847457));
#202917=CARTESIAN_POINT('Ctrl Pts',(-20.5314380472283,20.3369012678676,
18.1605861116263));
#202918=CARTESIAN_POINT('Ctrl Pts',(-20.4404259146217,20.4642090398079,
18.1708509745924));
#202919=CARTESIAN_POINT('Ctrl Pts',(-20.4242556921629,20.485934535488,18.1726189867731));
#202920=CARTESIAN_POINT('Ctrl Pts',(-20.3724969077827,20.5527588064822,
18.1780958165893));
#202921=CARTESIAN_POINT('Ctrl Pts',(-20.3354836828427,20.5967272765699,
18.1817564171383));
#202922=CARTESIAN_POINT('Ctrl Pts',(-20.2907363266949,20.6456915335486,
18.1858494298112));
#202923=CARTESIAN_POINT('Ctrl Pts',(-20.2847071114606,20.6522061782003,
18.1863943426289));
#202924=CARTESIAN_POINT('Ctrl Pts',(-20.2755483185451,20.6619783533334,
18.1872119820656));
#202925=CARTESIAN_POINT('Ctrl Pts',(-20.2724490850876,20.66526401101,18.1874869371576));
#202926=CARTESIAN_POINT('Ctrl Pts',(-20.2668839605058,20.6711261870312,
18.1879775404821));
#202927=CARTESIAN_POINT('Ctrl Pts',(-20.2644220611377,20.6737064072546,
18.1881934883807));
#202928=CARTESIAN_POINT('Ctrl Pts',(-20.2590779310063,20.6792791171241,
18.1886599050395));
#202929=CARTESIAN_POINT('Ctrl Pts',(-20.2561934168391,20.6822693376259,
18.1889101918702));
#202930=CARTESIAN_POINT('Ctrl Pts',(-20.2481154104312,20.6905941854478,
18.1896071070354));
#202931=CARTESIAN_POINT('Ctrl Pts',(-20.2429024933695,20.695909996921,18.1900522479129));
#202932=CARTESIAN_POINT('Ctrl Pts',(-20.2125438421952,20.7265429247764,
18.1926189565747));
#202933=CARTESIAN_POINT('Ctrl Pts',(-20.1867876621509,20.7512501739136,
18.1946953023093));
#202934=CARTESIAN_POINT('Ctrl Pts',(-20.10214195486,20.8284351276772,18.2012502157399));
#202935=CARTESIAN_POINT('Ctrl Pts',(-20.0409377282773,20.8782805742249,
18.205591708788));
#202936=CARTESIAN_POINT('Ctrl Pts',(-19.903360404184,20.978082920464,18.2148611437696));
#202937=CARTESIAN_POINT('Ctrl Pts',(-19.8262564389236,21.0267537140959,
18.2197680932191));
#202938=CARTESIAN_POINT('Ctrl Pts',(-19.6529377496387,21.1211131645764,
18.2306138081417));
#202939=CARTESIAN_POINT('Ctrl Pts',(-19.5559369742601,21.164815304497,18.2365764534918));
#202940=CARTESIAN_POINT('Ctrl Pts',(-19.4428143753893,21.205860931257,18.2436280282627));
#202941=CARTESIAN_POINT('Ctrl Pts',(-19.4295076127225,21.210539221949,18.2444588019421));
#202942=CARTESIAN_POINT('Ctrl Pts',(-19.408202400471,21.2177911451676,18.2457914076723));
#202943=CARTESIAN_POINT('Ctrl Pts',(-19.4002335180901,21.2204507889951,
18.246290394381));
#202944=CARTESIAN_POINT('Ctrl Pts',(-19.3861205857683,21.2250678539145,
18.247175151934));
#202945=CARTESIAN_POINT('Ctrl Pts',(-19.3799829936524,21.2270447785321,
18.2475602743498));
#202946=CARTESIAN_POINT('Ctrl Pts',(-19.3672397023328,21.231085238857,18.2483606554466));
#202947=CARTESIAN_POINT('Ctrl Pts',(-19.3606327325623,21.2331444828624,
18.2487760498115));
#202948=CARTESIAN_POINT('Ctrl Pts',(-19.3435839202667,21.238366636684,18.2498490913408));
#202949=CARTESIAN_POINT('Ctrl Pts',(-19.333127606431,21.2414812581307,18.2505083099329));
#202950=CARTESIAN_POINT('Ctrl Pts',(-19.2888347032104,21.2543028617376,
18.2533057235464));
#202951=CARTESIAN_POINT('Ctrl Pts',(-19.2547844205216,21.263245474215,18.2554685783143));
#202952=CARTESIAN_POINT('Ctrl Pts',(-19.1649549720866,21.2844578494643,
18.2612100587309));
#202953=CARTESIAN_POINT('Ctrl Pts',(-19.1088774663373,21.2953261788324,
18.2648303699799));
#202954=CARTESIAN_POINT('Ctrl Pts',(-18.9020410036757,21.3267959593207,
18.2782996189891));
#202955=CARTESIAN_POINT('Ctrl Pts',(-18.7496251547766,21.3333994417114,
18.2884871436087));
#202956=CARTESIAN_POINT('Ctrl Pts',(-18.5753870926614,21.3221696184504,
18.299891168646));
#202957=CARTESIAN_POINT('Ctrl Pts',(-18.5529584413561,21.3203646475768,
18.301353571541));
#202958=CARTESIAN_POINT('Ctrl Pts',(-18.4794374827478,21.3132666418875,
18.3061210164816));
#202959=CARTESIAN_POINT('Ctrl Pts',(-18.428504485824,21.3064714354772,18.3093821980804));
#202960=CARTESIAN_POINT('Ctrl Pts',(-18.3701013410559,21.2965044462548,
18.3130364374369));
#202961=CARTESIAN_POINT('Ctrl Pts',(-18.3623450304538,21.2951361801352,
18.3135199892109));
#202962=CARTESIAN_POINT('Ctrl Pts',(-18.3499902583087,21.2928855489414,
18.3142872263364));
#202963=CARTESIAN_POINT('Ctrl Pts',(-18.3453868620607,21.2920311748256,
18.3145724345939));
#202964=CARTESIAN_POINT('Ctrl Pts',(-18.3372558422888,21.2904941651123,
18.3150749786665));
#202965=CARTESIAN_POINT('Ctrl Pts',(-18.3337270742182,21.2898178118939,
18.3152926681362));
#202966=CARTESIAN_POINT('Ctrl Pts',(-18.3262701896523,21.2883688714348,
18.3157518034549));
#202967=CARTESIAN_POINT('Ctrl Pts',(-18.3223425449182,21.2875941265784,
18.3159931246794));
#202968=CARTESIAN_POINT('Ctrl Pts',(-18.3117895442108,21.2854813847912,
18.3166401999731));
#202969=CARTESIAN_POINT('Ctrl Pts',(-18.3051682946728,21.2841227788403,
18.3170447937068));
#202970=CARTESIAN_POINT('Ctrl Pts',(-18.2728640481678,21.2773329209507,
18.3190124156881));
#202971=CARTESIAN_POINT('Ctrl Pts',(-18.2472758454926,21.2714557375733,
18.3205513730988));
#202972=CARTESIAN_POINT('Ctrl Pts',(-18.1742917918238,21.2532569176944,
18.3249016689608));
#202973=CARTESIAN_POINT('Ctrl Pts',(-18.1272033909768,21.2397644274806,
18.3276607572441));
#202974=CARTESIAN_POINT('Ctrl Pts',(-17.9887178939118,21.1948294535513,
18.3357444543911));
#202975=CARTESIAN_POINT('Ctrl Pts',(-17.8989593561815,21.1587508293806,
18.3409474140977));
#202976=CARTESIAN_POINT('Ctrl Pts',(-17.6850124696732,21.0552363196111,
18.3538802746827));
#202977=CARTESIAN_POINT('Ctrl Pts',(-17.5645233672985,20.9812822697259,
18.3616599362714));
#202978=CARTESIAN_POINT('Ctrl Pts',(-17.4409209454358,20.8872576057647,
18.3707580344716));
#202979=CARTESIAN_POINT('Ctrl Pts',(-17.4296412792304,20.8784955217034,
18.371599137892));
#202980=CARTESIAN_POINT('Ctrl Pts',(-17.4118288561947,20.864367446892,18.3729451913875));
#202981=CARTESIAN_POINT('Ctrl Pts',(-17.4052379645834,20.8590752100642,
18.3734472039031));
#202982=CARTESIAN_POINT('Ctrl Pts',(-17.3936689194967,20.8496711936877,
18.3743354788066));
#202983=CARTESIAN_POINT('Ctrl Pts',(-17.3886775236237,20.8455758225045,
18.3747210758297));
#202984=CARTESIAN_POINT('Ctrl Pts',(-17.3783915517784,20.8370572964553,
18.3755206239967));
#202985=CARTESIAN_POINT('Ctrl Pts',(-17.373099712929,20.8326309700862,18.3759347018494));
#202986=CARTESIAN_POINT('Ctrl Pts',(-17.3595698259514,20.8212011088449,
18.3770004946254));
#202987=CARTESIAN_POINT('Ctrl Pts',(-17.351363702253,20.8141602463947,18.3776537406161));
#202988=CARTESIAN_POINT('Ctrl Pts',(-17.3173217825595,20.7844964588721,
18.3803926126732));
#202989=CARTESIAN_POINT('Ctrl Pts',(-17.2919856265056,20.7613104874583,
18.3825016300847));
#202990=CARTESIAN_POINT('Ctrl Pts',(-17.2274341787727,20.699285469669,18.3880662112844));
#202991=CARTESIAN_POINT('Ctrl Pts',(-17.1891558159554,20.6595129739667,
18.3915603348426));
#202992=CARTESIAN_POINT('Ctrl Pts',(-17.079712317872,20.5365198516453,18.4021433884306));
#202993=CARTESIAN_POINT('Ctrl Pts',(-17.0134042554094,20.4492315744595,
18.4093806639699));
#202994=CARTESIAN_POINT('Ctrl Pts',(-16.9252676750691,20.3123725070272,
18.4201335400683));
#202995=CARTESIAN_POINT('Ctrl Pts',(-16.8980924733817,20.2664515219804,
18.423649098732));
#202996=CARTESIAN_POINT('Ctrl Pts',(-16.8666535691045,20.2084298603262,
18.427943873464));
#202997=CARTESIAN_POINT('Ctrl Pts',(-16.8607268113086,20.1972538157768,
18.4287645453795));
#202998=CARTESIAN_POINT('Ctrl Pts',(-16.8303567746165,20.1387237151428,
18.4330260693232));
#202999=CARTESIAN_POINT('Ctrl Pts',(-16.8076055108233,20.0905078891366,
18.4364135828855));
#203000=CARTESIAN_POINT('Ctrl Pts',(-16.7832770591629,20.0334627575651,
18.4402391919341));
#203001=CARTESIAN_POINT('Ctrl Pts',(-16.7799070889915,20.0254236493611,
18.4407741885624));
#203002=CARTESIAN_POINT('Ctrl Pts',(-16.7748794475646,20.0132192675484,
18.4415798921587));
#203003=CARTESIAN_POINT('Ctrl Pts',(-16.7731852414488,20.0090692800151,
18.4418527339967));
#203004=CARTESIAN_POINT('Ctrl Pts',(-16.7701676973725,20.0016101367109,
18.4423410696028));
#203005=CARTESIAN_POINT('Ctrl Pts',(-16.7688395290751,19.9983030072413,
18.4425568512549));
#203006=CARTESIAN_POINT('Ctrl Pts',(-16.7659715776412,19.991109353844,18.4430246303433));
#203007=CARTESIAN_POINT('Ctrl Pts',(-16.7644349577649,19.987221630893,18.44327643657));
#203008=CARTESIAN_POINT('Ctrl Pts',(-16.7601507300588,19.9762876956346,
18.4439818872953));
#203009=CARTESIAN_POINT('Ctrl Pts',(-16.7574293183007,19.969231192774,18.4444339847251));
#203010=CARTESIAN_POINT('Ctrl Pts',(-16.7413800264958,19.9269424347717,
18.4471252075736));
#203011=CARTESIAN_POINT('Ctrl Pts',(-16.728955722396,19.8913717868833,18.4493138265337));
#203012=CARTESIAN_POINT('Ctrl Pts',(-16.6911827020441,19.7731849057294,
18.4563989895548));
#203013=CARTESIAN_POINT('Ctrl Pts',(-16.669939913382,19.6893437057548,18.4611316698816));
#203014=CARTESIAN_POINT('Ctrl Pts',(-16.6211081375412,19.4311652019751,
18.4754304050701));
#203015=CARTESIAN_POINT('Ctrl Pts',(-16.6101154567431,19.2545031734588,
18.4849065781047));
#203016=CARTESIAN_POINT('Ctrl Pts',(-16.6225836427218,19.055643226487,18.4964854424401));
#203017=CARTESIAN_POINT('Ctrl Pts',(-16.624390123769,19.032784202349,18.4978288338834));
#203018=CARTESIAN_POINT('Ctrl Pts',(-16.6274730760298,19.0004667381701,
18.4997473952577));
#203019=CARTESIAN_POINT('Ctrl Pts',(-16.6284427813954,18.9909801590596,
18.5003129355149));
#203020=CARTESIAN_POINT('Ctrl Pts',(-16.6301231906189,18.9755707061212,
18.5012355224035));
#203021=CARTESIAN_POINT('Ctrl Pts',(-16.6307949002812,18.9696436475599,
18.5015913369993));
#203022=CARTESIAN_POINT('Ctrl Pts',(-16.632253958639,18.9572379663657,18.5023381074554));
#203023=CARTESIAN_POINT('Ctrl Pts',(-16.6330462329962,18.9507599963057,
18.5027292151583));
#203024=CARTESIAN_POINT('Ctrl Pts',(-16.63500344822,18.9353487050685,18.5036624825223));
#203025=CARTESIAN_POINT('Ctrl Pts',(-16.6361954772838,18.926419007431,18.5042054927138));
#203026=CARTESIAN_POINT('Ctrl Pts',(-16.6404094781528,18.8963174553767,
18.5060437008792));
#203027=CARTESIAN_POINT('Ctrl Pts',(-16.6436951880649,18.8751843994187,
18.5073472017004));
#203028=CARTESIAN_POINT('Ctrl Pts',(-16.6633755087638,18.7601170653344,
18.5145178641753));
#203029=CARTESIAN_POINT('Ctrl Pts',(-16.6857800060727,18.6673348307803,
18.5205745432654));
#203030=CARTESIAN_POINT('Ctrl Pts',(-16.7654990620338,18.4136301285492,
18.5378562431451));
#203031=CARTESIAN_POINT('Ctrl Pts',(-16.8361232310038,18.2576609675694,
18.5493674729598));
#203032=CARTESIAN_POINT('Ctrl Pts',(-16.9437230669628,18.0805396478754,
18.5625930779529));
#203033=CARTESIAN_POINT('Ctrl Pts',(-16.9635622741014,18.0497150493651,
18.5648981586729));
#203034=CARTESIAN_POINT('Ctrl Pts',(-16.9882081863394,18.0135231417081,
18.5675945047978));
#203035=CARTESIAN_POINT('Ctrl Pts',(-16.9922530497112,18.0076474135751,
18.5680319258315));
#203036=CARTESIAN_POINT('Ctrl Pts',(-16.9989034819625,17.9980905184959,
18.5687427051508));
#203037=CARTESIAN_POINT('Ctrl Pts',(-17.0014912130962,17.9943970896796,
18.5690172292113));
#203038=CARTESIAN_POINT('Ctrl Pts',(-17.0061461442436,17.9877981491884,
18.5695073681991));
#203039=CARTESIAN_POINT('Ctrl Pts',(-17.0082088932235,17.9848895763197,
18.5697232803919));
#203040=CARTESIAN_POINT('Ctrl Pts',(-17.0126939869186,17.978599126359,18.570189966734));
#203041=CARTESIAN_POINT('Ctrl Pts',(-17.0151189457656,17.9752191836336,
18.5704405570921));
#203042=CARTESIAN_POINT('Ctrl Pts',(-17.021925507103,17.965790896765,18.5711391748603));
#203043=CARTESIAN_POINT('Ctrl Pts',(-17.0263292270764,17.9597584905057,
18.5715857030078));
#203044=CARTESIAN_POINT('Ctrl Pts',(-17.0521852350735,17.924730579548,18.5741766312995));
#203045=CARTESIAN_POINT('Ctrl Pts',(-17.0743451903466,17.8962619317625,
18.5762748056793));
#203046=CARTESIAN_POINT('Ctrl Pts',(-17.1481437640279,17.806295273004,18.5829305490586));
#203047=CARTESIAN_POINT('Ctrl Pts',(-17.2025586858378,17.7471609077914,
18.587346139373));
#203048=CARTESIAN_POINT('Ctrl Pts',(-17.3932703468835,17.5622152803035,
18.6018276925815));
#203049=CARTESIAN_POINT('Ctrl Pts',(-17.5426891605687,17.451221746326,18.6117428572409));
#203050=CARTESIAN_POINT('Ctrl Pts',(-17.7239879405533,17.3503403016593,
18.6238093829938));
#203051=CARTESIAN_POINT('Ctrl Pts',(-17.7434955031188,17.3398827774709,
18.6251068105974));
#203052=CARTESIAN_POINT('Ctrl Pts',(-17.7706835638669,17.3258522427365,
18.6269153199065));
#203053=CARTESIAN_POINT('Ctrl Pts',(-17.7782273326181,17.3220163505299,
18.6274171446793));
#203054=CARTESIAN_POINT('Ctrl Pts',(-17.7912290431025,17.3155029996447,
18.6282821712426));
#203055=CARTESIAN_POINT('Ctrl Pts',(-17.796675928187,17.3128036090174,18.628644600817));
#203056=CARTESIAN_POINT('Ctrl Pts',(-17.8079245431053,17.3072891941951,
18.6293931859976));
#203057=CARTESIAN_POINT('Ctrl Pts',(-17.8137276540915,17.3044771462345,
18.6297794405168));
#203058=CARTESIAN_POINT('Ctrl Pts',(-17.8272543474449,17.2979985838706,
18.6306799647255));
#203059=CARTESIAN_POINT('Ctrl Pts',(-17.8349874330673,17.294352276059,18.6311949286769));
#203060=CARTESIAN_POINT('Ctrl Pts',(-17.8597787799449,17.2828456948266,
18.6328464176771));
#203061=CARTESIAN_POINT('Ctrl Pts',(-17.8769192795361,17.2751657175578,
18.6339891180636));
#203062=CARTESIAN_POINT('Ctrl Pts',(-17.9628696376711,17.2380200536409,
18.6397249928209));
#203063=CARTESIAN_POINT('Ctrl Pts',(-18.0330990949681,17.2119933227832,
18.644433032704));
#203064=CARTESIAN_POINT('Ctrl Pts',(-18.2084873225002,17.1573750587722,
18.6562343147341));
#203065=CARTESIAN_POINT('Ctrl Pts',(-18.3147562448931,17.1330755144151,
18.6634279804527));
#203066=CARTESIAN_POINT('Ctrl Pts',(-18.5410782417617,17.0993978681545,
18.6785444460428));
#203067=CARTESIAN_POINT('Ctrl Pts',(-18.6610446929986,17.0918571167076,
18.6864394334074));
#203068=CARTESIAN_POINT('Ctrl Pts',(-18.7905255665961,17.0947333931917,
18.6944387466851));
#203069=CARTESIAN_POINT('Ctrl Pts',(-18.8000345575661,17.0950087581136,
18.6950230991984));
#203070=CARTESIAN_POINT('Ctrl Pts',(-18.8141225778557,17.0955117856868,
18.6958839116011));
#203071=CARTESIAN_POINT('Ctrl Pts',(-18.818703091444,17.0956902355463,18.6961630189385));
#203072=CARTESIAN_POINT('Ctrl Pts',(-18.8268519529105,17.0960342142993,
18.6966581391539));
#203073=CARTESIAN_POINT('Ctrl Pts',(-18.8304204901521,17.0961938978762,
18.6968744747662));
#203074=CARTESIAN_POINT('Ctrl Pts',(-18.8380920598155,17.096556641007,18.6973384937323));
#203075=CARTESIAN_POINT('Ctrl Pts',(-18.8421948983607,17.0967626103168,
18.6975860123356));
#203076=CARTESIAN_POINT('Ctrl Pts',(-18.8535187886543,17.0973641377088,
18.6982674533202));
#203077=CARTESIAN_POINT('Ctrl Pts',(-18.8607385313378,17.0977847607705,
18.6986999936056));
#203078=CARTESIAN_POINT('Ctrl Pts',(-18.9002851624277,17.100292153106,18.7010594048153));
#203079=CARTESIAN_POINT('Ctrl Pts',(-18.9325649386611,17.1030838265953,
18.7029491691305));
#203080=CARTESIAN_POINT('Ctrl Pts',(-19.1266009342844,17.1243620946157,
18.7141585654862));
#203081=CARTESIAN_POINT('Ctrl Pts',(-19.2858615262963,17.1607185577273,
18.7227633917145));
#203082=CARTESIAN_POINT('Ctrl Pts',(-19.549573589651,17.2539143043239,18.7380750868553));
#203083=CARTESIAN_POINT('Ctrl Pts',(-19.6563256189776,17.3019020740949,
18.7445985568056));
#203084=CARTESIAN_POINT('Ctrl Pts',(-19.7721868663751,17.365979864426,18.7523548877149));
#203085=CARTESIAN_POINT('Ctrl Pts',(-19.7857238043305,17.3736627173271,
18.7532718945608));
#203086=CARTESIAN_POINT('Ctrl Pts',(-19.8061730604815,17.385568678129,18.7546741709939));
#203087=CARTESIAN_POINT('Ctrl Pts',(-19.8131480780999,17.3896834417822,
18.7551555215593));
#203088=CARTESIAN_POINT('Ctrl Pts',(-19.8254397220556,17.3970300326623,
18.7560092619945));
#203089=CARTESIAN_POINT('Ctrl Pts',(-19.8307660606806,17.400245484295,18.7563810508131));
#203090=CARTESIAN_POINT('Ctrl Pts',(-19.8420027225034,17.4070966996114,
18.7571693257224));
#203091=CARTESIAN_POINT('Ctrl Pts',(-19.8479094886132,17.4107381302653,
18.7575860172026));
#203092=CARTESIAN_POINT('Ctrl Pts',(-19.8599606508176,17.4182495036909,
18.7584409698363));
#203093=CARTESIAN_POINT('Ctrl Pts',(-19.866103246299,17.4221221487008,18.758879327386));
#203094=CARTESIAN_POINT('Ctrl Pts',(-19.8812447569507,17.4317774489148,
18.759966334535));
#203095=CARTESIAN_POINT('Ctrl Pts',(-19.8902199257273,17.4375968040521,
18.7606163438544));
#203096=CARTESIAN_POINT('Ctrl Pts',(-19.996728812433,17.5078076929853,18.7683988411112));
#203097=CARTESIAN_POINT('Ctrl Pts',(-20.0887969077889,17.5800905647174,
18.7758355776126));
#203098=CARTESIAN_POINT('Ctrl Pts',(-20.310417376706,17.7858558121241,18.7955807218107));
#203099=CARTESIAN_POINT('Ctrl Pts',(-20.4292197414015,17.9294541777997,
18.808144404582));
#203100=CARTESIAN_POINT('Ctrl Pts',(-20.535338539805,18.0987630240731,18.8205838211335));
#203101=CARTESIAN_POINT('Ctrl Pts',(-20.542776691332,18.1109006719478,18.8214632787622));
#203102=CARTESIAN_POINT('Ctrl Pts',(-20.5529510031847,18.1278854172129,
18.8226759152318));
#203103=CARTESIAN_POINT('Ctrl Pts',(-20.5557911451072,18.1326693565273,
18.8230154997651));
#203104=CARTESIAN_POINT('Ctrl Pts',(-20.5603198777447,18.1403665233724,
18.8235586561472));
#203105=CARTESIAN_POINT('Ctrl Pts',(-20.5620204116266,18.1432726414643,
18.8237629951947));
#203106=CARTESIAN_POINT('Ctrl Pts',(-20.5655581675288,18.1493516959139,
18.8241888840266));
#203107=CARTESIAN_POINT('Ctrl Pts',(-20.567394086377,18.1525253584206,18.8244103446589));
#203108=CARTESIAN_POINT('Ctrl Pts',(-20.5718154178768,18.1602143122068,
18.8249447950763));
#203109=CARTESIAN_POINT('Ctrl Pts',(-20.574392468853,18.1647344344013,18.8252572462968));
#203110=CARTESIAN_POINT('Ctrl Pts',(-20.5833492816421,18.1805800851206,
18.8263466679732));
#203111=CARTESIAN_POINT('Ctrl Pts',(-20.5896415238493,18.1919550940256,
18.8271182177777));
#203112=CARTESIAN_POINT('Ctrl Pts',(-20.6261717186448,18.2594542348069,
18.8316391787254));
#203113=CARTESIAN_POINT('Ctrl Pts',(-20.6539696182429,18.3168683694867,
18.8352523704476));
#203114=CARTESIAN_POINT('Ctrl Pts',(-20.7670746929877,18.5801751691126,
18.8511806925627));
#203115=CARTESIAN_POINT('Ctrl Pts',(-20.8221439376655,18.7974839958582,
18.8627824789036));
#203116=CARTESIAN_POINT('Ctrl Pts',(-20.8447697705718,19.0464467519669,
18.877249995478));
#203117=CARTESIAN_POINT('Ctrl Pts',(-20.8467072345963,19.0735415067363,
18.8788370064226));
#203118=CARTESIAN_POINT('Ctrl Pts',(-20.8486554028962,19.1108703059235,
18.8810435528669));
#203119=CARTESIAN_POINT('Ctrl Pts',(-20.8491140969093,19.1210790339432,
18.8816490613351));
#203120=CARTESIAN_POINT('Ctrl Pts',(-20.8497282755774,19.1373794130681,
18.8826193142311));
#203121=CARTESIAN_POINT('Ctrl Pts',(-20.8499314061028,19.1434691894635,
18.882982561869));
#203122=CARTESIAN_POINT('Ctrl Pts',(-20.8502862993201,19.1556923162535,
18.8837132236441));
#203123=CARTESIAN_POINT('Ctrl Pts',(-20.8504376956191,19.1618256173907,
18.8840806456684));
#203124=CARTESIAN_POINT('Ctrl Pts',(-20.8507174560923,19.1755831175595,
18.8849066150619));
#203125=CARTESIAN_POINT('Ctrl Pts',(-20.8508312920298,19.18320749748,18.8853656133632));
#203126=CARTESIAN_POINT('Ctrl Pts',(-20.8509693631967,19.1977001098008,
18.8862405120949));
#203127=CARTESIAN_POINT('Ctrl Pts',(-20.8510013701644,19.2045681711671,
18.8866561616126));
#203128=CARTESIAN_POINT('Ctrl Pts',(-20.8509999550631,19.2114361911346,
18.8870728602009));
#203129=CARTESIAN_POINT('Ctrl Pts',(-20.8509999552301,19.2114353802296,
18.8870728110014));
#203130=CARTESIAN_POINT('Ctrl Pts',(-20.8509977625579,19.2220970650987,
18.8877196798475));
#203131=CARTESIAN_POINT('Ctrl Pts',(-20.850915028038,19.2327584644317,18.8883690662257));
#203132=CARTESIAN_POINT('Ctrl Pts',(-20.850420668131,19.2650373055968,18.8903430083297));
#203133=CARTESIAN_POINT('Ctrl Pts',(-20.8497584121093,19.286648942304,18.8916752809909));
#203134=CARTESIAN_POINT('Ctrl Pts',(-20.8411876622882,19.4730331322725,
18.903259385164));
#203135=CARTESIAN_POINT('Ctrl Pts',(-20.8143762766218,19.6363439341123,
18.9141120151009));
#203136=CARTESIAN_POINT('Ctrl Pts',(-20.7551361081569,19.8428126233419,
18.9283024366599));
#203137=CARTESIAN_POINT('Ctrl Pts',(-20.739687226211,19.8902608224799,18.9315919516632));
#203138=CARTESIAN_POINT('Ctrl Pts',(-20.7225805923249,19.9371103413593,
18.9348455557956));
#203139=CARTESIAN_POINT('Origin',(-18.734,19.211,0.));
#203140=CARTESIAN_POINT('',(-20.7225806070201,19.9371103011137,19.9537492499338));
#203141=CARTESIAN_POINT('',(-20.7225805741668,19.9371103910883,19.7345261348292));
#203142=CARTESIAN_POINT('',(-20.7225806064498,19.9371103026755,0.));
#203143=CARTESIAN_POINT('',(-20.8479141177977,19.2118284581339,19.910995664247));
#203144=CARTESIAN_POINT('Ctrl Pts',(-20.7225806070201,19.9371103011137,
19.9537492499338));
#203145=CARTESIAN_POINT('Ctrl Pts',(-20.7405653140382,19.8878560217788,
19.9507625358576));
#203146=CARTESIAN_POINT('Ctrl Pts',(-20.7567162132681,19.8379441465122,
19.9478475669179));
#203147=CARTESIAN_POINT('Ctrl Pts',(-20.8240164289173,19.6001371512545,
19.9342646615474));
#203148=CARTESIAN_POINT('Ctrl Pts',(-20.8509329967896,19.4064030179224,
19.9239833448394));
#203149=CARTESIAN_POINT('Ctrl Pts',(-20.8509998750784,19.2117272674118,
19.9127739856851));
#203150=CARTESIAN_POINT('Ctrl Pts',(-20.7202231500468,19.93627084876,19.1554367712949));
#203151=CARTESIAN_POINT('Ctrl Pts',(-20.632847054901,20.1806249108887,19.1710019318661));
#203152=CARTESIAN_POINT('Ctrl Pts',(-20.1480309705507,21.030328314946,19.2289590279977));
#203153=CARTESIAN_POINT('Ctrl Pts',(-18.3741968251021,21.6882711019052,
19.3293080596899));
#203154=CARTESIAN_POINT('Ctrl Pts',(-16.4562524007973,20.2493623486039,
19.4564838663713));
#203155=CARTESIAN_POINT('Ctrl Pts',(-16.6280000239015,17.8578205442181,
19.5836596730528));
#203156=CARTESIAN_POINT('Ctrl Pts',(-18.7318719156385,16.7077369880417,
19.7108354797341));
#203157=CARTESIAN_POINT('Ctrl Pts',(-20.5383022142055,17.6912382698633,
19.8199301623757));
#203158=CARTESIAN_POINT('Ctrl Pts',(-20.8463944722286,18.8061996577397,
19.8866329094569));
#203159=CARTESIAN_POINT('Ctrl Pts',(-20.8478239854299,19.2118314138296,
19.9109437209775));
#203160=CARTESIAN_POINT('Ctrl Pts',(-20.7225805923249,19.9371103413593,
18.9348455557956));
#203161=CARTESIAN_POINT('Ctrl Pts',(-20.710360467218,19.9705772984304,18.9371697681339));
#203162=CARTESIAN_POINT('Ctrl Pts',(-20.6972943982248,20.0037387601119,
18.9394755308538));
#203163=CARTESIAN_POINT('Ctrl Pts',(-20.6687906446562,20.0710444200022,
18.9441406592123));
#203164=CARTESIAN_POINT('Ctrl Pts',(-20.6532742864404,20.1051352555742,
18.9464955566324));
#203165=CARTESIAN_POINT('Ctrl Pts',(-20.6335516713709,20.1455851764302,
18.9492646624661));
#203166=CARTESIAN_POINT('Ctrl Pts',(-20.6302064116756,20.152353946439,18.9497271749787));
#203167=CARTESIAN_POINT('Ctrl Pts',(-20.6249540245575,20.162839970243,18.9504421783014));
#203168=CARTESIAN_POINT('Ctrl Pts',(-20.6230720245406,20.1665696409664,
18.9506961922967));
#203169=CARTESIAN_POINT('Ctrl Pts',(-20.6195639348222,20.17347096097,18.95116562712));
#203170=CARTESIAN_POINT('Ctrl Pts',(-20.6179408903305,20.1766440467623,
18.9513812283854));
#203171=CARTESIAN_POINT('Ctrl Pts',(-20.6142568256493,20.1838018268405,
18.9518670574669));
#203172=CARTESIAN_POINT('Ctrl Pts',(-20.6121911544154,20.1877840667376,
18.9521369882068));
#203173=CARTESIAN_POINT('Ctrl Pts',(-20.6060667987521,20.1994994558908,
18.9529301232858));
#203174=CARTESIAN_POINT('Ctrl Pts',(-20.6019728447992,20.2072141990175,
18.9534511552968));
#203175=CARTESIAN_POINT('Ctrl Pts',(-20.5723566895963,20.2621990772766,
18.95715723626));
#203176=CARTESIAN_POINT('Ctrl Pts',(-20.5450888442467,20.3085122120635,
18.9602394581677));
#203177=CARTESIAN_POINT('Ctrl Pts',(-20.4252331004243,20.4954252059314,
18.9727226983674));
#203178=CARTESIAN_POINT('Ctrl Pts',(-20.3178045746723,20.6257750065153,
18.9815807144511));
#203179=CARTESIAN_POINT('Ctrl Pts',(-20.1529709502013,20.7831835048041,
18.9942099302935));
#203180=CARTESIAN_POINT('Ctrl Pts',(-20.1081622153545,20.8224952531611,
18.9975588869045));
#203181=CARTESIAN_POINT('Ctrl Pts',(-20.0334871111794,20.8826278599759,
19.0030654766779));
#203182=CARTESIAN_POINT('Ctrl Pts',(-20.0046373039412,20.9046608470138,
19.0051760294489));
#203183=CARTESIAN_POINT('Ctrl Pts',(-19.9686169170661,20.9307316196453,
19.0077975438664));
#203184=CARTESIAN_POINT('Ctrl Pts',(-19.9619696259046,20.9354843781678,
19.0082807642692));
#203185=CARTESIAN_POINT('Ctrl Pts',(-19.9490943378091,20.9445779124438,
19.0092157415624));
#203186=CARTESIAN_POINT('Ctrl Pts',(-19.942870173226,20.9489239138337,19.0096672896238));
#203187=CARTESIAN_POINT('Ctrl Pts',(-19.9365819733175,20.9532645034312,
19.0101230790902));
#203188=CARTESIAN_POINT('Ctrl Pts',(-19.9365411161683,20.9532927039936,
19.0101260405339));
#203189=CARTESIAN_POINT('Ctrl Pts',(-19.9364577119075,20.9533502672387,
19.0101320858799));
#203190=CARTESIAN_POINT('Ctrl Pts',(-19.9364151647884,20.9533796297475,
19.0101351697812));
#203191=CARTESIAN_POINT('Ctrl Pts',(-19.936328266968,20.9534395947502,19.0101414682732));
#203192=CARTESIAN_POINT('Ctrl Pts',(-19.9362839159617,20.9534701972554,
19.0101446828844));
#203193=CARTESIAN_POINT('Ctrl Pts',(-19.936193284958,20.9535327281756,19.0101512518811));
#203194=CARTESIAN_POINT('Ctrl Pts',(-19.9361470049187,20.9535646563977,
19.0101546062679));
#203195=CARTESIAN_POINT('Ctrl Pts',(-19.9360523782072,20.9536299330311,
19.0101614647866));
#203196=CARTESIAN_POINT('Ctrl Pts',(-19.9360040315621,20.9536632811757,
19.0101649689146));
#203197=CARTESIAN_POINT('Ctrl Pts',(-19.9359051206447,20.9537315010468,
19.0101721378536));
#203198=CARTESIAN_POINT('Ctrl Pts',(-19.935854556117,20.9537663726712,19.0101758026809));
#203199=CARTESIAN_POINT('Ctrl Pts',(-19.935751041673,20.9538377543462,19.0101833051708));
#203200=CARTESIAN_POINT('Ctrl Pts',(-19.9356980917437,20.9538742640926,
19.0101871428318));
#203201=CARTESIAN_POINT('Ctrl Pts',(-19.9355896214927,20.9539490486151,
19.01019500439));
#203202=CARTESIAN_POINT('Ctrl Pts',(-19.9355341008688,20.9539873232462,
19.0101990283062));
#203203=CARTESIAN_POINT('Ctrl Pts',(-19.9354202827788,20.9540657787762,
19.0102072773288));
#203204=CARTESIAN_POINT('Ctrl Pts',(-19.9353619851864,20.9541059593616,
19.0102115024412));
#203205=CARTESIAN_POINT('Ctrl Pts',(-19.9352423834067,20.9541883839248,
19.0102201704975));
#203206=CARTESIAN_POINT('Ctrl Pts',(-19.9351810789387,20.9542306276401,
19.0102246134582));
#203207=CARTESIAN_POINT('Ctrl Pts',(-19.9350552059521,20.954317354472,19.0102337358588));
#203208=CARTESIAN_POINT('Ctrl Pts',(-19.9349906371787,20.9543618372435,
19.0102384153131));
#203209=CARTESIAN_POINT('Ctrl Pts',(-19.9348579461057,20.9544532400145,
19.0102480316671));
#203210=CARTESIAN_POINT('Ctrl Pts',(-19.9347898236244,20.9545001595418,
19.0102529685753));
#203211=CARTESIAN_POINT('Ctrl Pts',(-19.9346496988297,20.9545966587324,
19.0102631234702));
#203212=CARTESIAN_POINT('Ctrl Pts',(-19.934577696169,20.9546462379462,19.0102683414766));
#203213=CARTESIAN_POINT('Ctrl Pts',(-19.9344294410399,20.9547483091474,
19.0102790853632));
#203214=CARTESIAN_POINT('Ctrl Pts',(-19.9343531881439,20.9548008006314,
19.0102846112681));
#203215=CARTESIAN_POINT('Ctrl Pts',(-19.9341960107911,20.9549089842453,
19.0102960014956));
#203216=CARTESIAN_POINT('Ctrl Pts',(-19.93411508598,20.9549646756897,19.0103018658366));
#203217=CARTESIAN_POINT('Ctrl Pts',(-19.9339480823981,20.9550795883405,
19.0103139678715));
#203218=CARTESIAN_POINT('Ctrl Pts',(-19.9338620030314,20.9551388088677,
19.0103202055999));
#203219=CARTESIAN_POINT('Ctrl Pts',(-19.9336841343563,20.9552611588247,
19.0103330946722));
#203220=CARTESIAN_POINT('Ctrl Pts',(-19.9335923444732,20.9553242873652,
19.0103397460475));
#203221=CARTESIAN_POINT('Ctrl Pts',(-19.9334024105831,20.9554548924156,
19.0103535090615));
#203222=CARTESIAN_POINT('Ctrl Pts',(-19.9333042659174,20.9555223678525,
19.0103606207358));
#203223=CARTESIAN_POINT('Ctrl Pts',(-19.928070984362,20.9591196507895,19.0107398251101));
#203224=CARTESIAN_POINT('Ctrl Pts',(-19.9229203365489,20.9626267471199,
19.0111127765554));
#203225=CARTESIAN_POINT('Ctrl Pts',(-19.9111823831209,20.9705435415101,
19.0119621437524));
#203226=CARTESIAN_POINT('Ctrl Pts',(-19.9045856707945,20.9749390642151,
19.0124390877911));
#203227=CARTESIAN_POINT('Ctrl Pts',(-19.8856079655805,20.9874309534452,
19.0138101307927));
#203228=CARTESIAN_POINT('Ctrl Pts',(-19.8731667749699,20.9954346107718,
19.0147076757062));
#203229=CARTESIAN_POINT('Ctrl Pts',(-19.7870665135087,21.0495571748562,
19.0209116588197));
#203230=CARTESIAN_POINT('Ctrl Pts',(-19.7107213885186,21.0912269970739,
19.0263802955044));
#203231=CARTESIAN_POINT('Ctrl Pts',(-19.5002142292279,21.1898370772005,
19.041362164052));
#203232=CARTESIAN_POINT('Ctrl Pts',(-19.3623745568207,21.2378250907786,
19.0510971074492));
#203233=CARTESIAN_POINT('Ctrl Pts',(-19.1686221922198,21.2835970023539,
19.064123768228));
#203234=CARTESIAN_POINT('Ctrl Pts',(-19.1160714135176,21.2939251062326,
19.0675892319824));
#203235=CARTESIAN_POINT('Ctrl Pts',(-19.0356443044213,21.3065850847056,
19.0727392354969));
#203236=CARTESIAN_POINT('Ctrl Pts',(-19.0080217517752,21.3103757136771,
19.0744806576681));
#203237=CARTESIAN_POINT('Ctrl Pts',(-18.9734827023116,21.3144221109289,
19.076617480215));
#203238=CARTESIAN_POINT('Ctrl Pts',(-18.9666305192715,21.3151909575839,
19.0770394140795));
#203239=CARTESIAN_POINT('Ctrl Pts',(-18.9557640864944,21.3163564921782,
19.0777052490511));
#203240=CARTESIAN_POINT('Ctrl Pts',(-18.9517523188098,21.3167752010832,
19.0779503596852));
#203241=CARTESIAN_POINT('Ctrl Pts',(-18.9441719577815,21.3175444703217,
19.0784121347089));
#203242=CARTESIAN_POINT('Ctrl Pts',(-18.9406037151162,21.3178974256834,
19.0786289257584));
#203243=CARTESIAN_POINT('Ctrl Pts',(-18.9324281491159,21.3186851485056,
19.0791243394291));
#203244=CARTESIAN_POINT('Ctrl Pts',(-18.9278202899357,21.3191138754187,
19.0794026200616));
#203245=CARTESIAN_POINT('Ctrl Pts',(-18.9155512871331,21.3202148477527,
19.0801411602876));
#203246=CARTESIAN_POINT('Ctrl Pts',(-18.9078877422194,21.3208604695593,
19.0805999654418));
#203247=CARTESIAN_POINT('Ctrl Pts',(-18.8532924827852,21.3251604063639,
19.0838517383281));
#203248=CARTESIAN_POINT('Ctrl Pts',(-18.806250099316,21.3272905208898,19.0865655601787));
#203249=CARTESIAN_POINT('Ctrl Pts',(-18.723838485101,21.3282705044033,19.0912259481555));
#203250=CARTESIAN_POINT('Ctrl Pts',(-18.6884984494264,21.3278059531367,
19.0931942599116));
#203251=CARTESIAN_POINT('Ctrl Pts',(-18.5088934341252,21.3209446859869,
19.1031148531432));
#203252=CARTESIAN_POINT('Ctrl Pts',(-18.3655446402525,21.3006846503446,
19.1107882244793));
#203253=CARTESIAN_POINT('Ctrl Pts',(-18.1498061241505,21.2472874048348,
19.1231297656917));
#203254=CARTESIAN_POINT('Ctrl Pts',(-18.0753373027004,21.224432506524,19.1275372810849));
#203255=CARTESIAN_POINT('Ctrl Pts',(-17.9842993655213,21.1909004968648,
19.1331997171494));
#203256=CARTESIAN_POINT('Ctrl Pts',(-17.9663892477625,21.1840257768368,
19.1343271466788));
#203257=CARTESIAN_POINT('Ctrl Pts',(-17.9405677842116,21.1737095243329,
19.1359731727588));
#203258=CARTESIAN_POINT('Ctrl Pts',(-17.9325798270281,21.1704614211452,
19.1364852593386));
#203259=CARTESIAN_POINT('Ctrl Pts',(-17.9186427371285,21.1646947731278,
19.1373838757599));
#203260=CARTESIAN_POINT('Ctrl Pts',(-17.9126848365619,21.1621976151952,
19.1377696765811));
#203261=CARTESIAN_POINT('Ctrl Pts',(-17.9011622136924,21.1573059679266,
19.1385190707323));
#203262=CARTESIAN_POINT('Ctrl Pts',(-17.8955961505203,21.154914782875,19.1388825484548));
#203263=CARTESIAN_POINT('Ctrl Pts',(-17.8823527276467,21.1491579380113,
19.1397509439929));
#203264=CARTESIAN_POINT('Ctrl Pts',(-17.8746849880861,21.1457705229098,
19.1402566027372));
#203265=CARTESIAN_POINT('Ctrl Pts',(-17.8473048028855,21.1334797724892,
19.1420726525973));
#203266=CARTESIAN_POINT('Ctrl Pts',(-17.8277094675391,21.1243202200647,
19.1433918191923));
#203267=CARTESIAN_POINT('Ctrl Pts',(-17.6373490279054,21.0317586070133,
19.1564028942634));
#203268=CARTESIAN_POINT('Ctrl Pts',(-17.4784384557029,20.9260337740172,
19.1689388675631));
#203269=CARTESIAN_POINT('Ctrl Pts',(-17.2777781476593,20.749531281651,19.1865741499127));
#203270=CARTESIAN_POINT('Ctrl Pts',(-17.2225886338018,20.6953510003441,
19.1916444691733));
#203271=CARTESIAN_POINT('Ctrl Pts',(-17.1467200222394,20.6122399955117,
19.1988129755024));
#203272=CARTESIAN_POINT('Ctrl Pts',(-17.1236097314221,20.5856180460662,
19.2010261829913));
#203273=CARTESIAN_POINT('Ctrl Pts',(-17.0964520410258,20.5527081317394,
19.2036509814267));
#203274=CARTESIAN_POINT('Ctrl Pts',(-17.0917605665561,20.5469617044302,
19.2041053149122));
#203275=CARTESIAN_POINT('Ctrl Pts',(-17.0844924704814,20.5379631202775,
19.2048104280743));
#203276=CARTESIAN_POINT('Ctrl Pts',(-17.0818950929783,20.5347279136561,
19.205062665289));
#203277=CARTESIAN_POINT('Ctrl Pts',(-17.0770823192423,20.52869705257,19.2055304832227));
#203278=CARTESIAN_POINT('Ctrl Pts',(-17.0748644996438,20.5259034621915,
19.2057462338662));
#203279=CARTESIAN_POINT('Ctrl Pts',(-17.0698492653394,20.5195533256198,
19.2062345220013));
#203280=CARTESIAN_POINT('Ctrl Pts',(-17.0670561928381,20.5159934169565,
19.2065067493486));
#203281=CARTESIAN_POINT('Ctrl Pts',(-17.0587944816236,20.5053936555235,
19.2073129382117));
#203282=CARTESIAN_POINT('Ctrl Pts',(-17.0533587918804,20.498328085664,19.2078446192109));
#203283=CARTESIAN_POINT('Ctrl Pts',(-17.0125863679976,20.4446317077314,
19.2118440752282));
#203284=CARTESIAN_POINT('Ctrl Pts',(-16.9791483487723,20.3965838531807,
19.2151896658664));
#203285=CARTESIAN_POINT('Ctrl Pts',(-16.9338102353811,20.325306755169,19.2199207081904));
#203286=CARTESIAN_POINT('Ctrl Pts',(-16.9202828959771,20.3031506611426,
19.2213605209325));
#203287=CARTESIAN_POINT('Ctrl Pts',(-16.8894949372539,20.2505734796657,
19.2247185505662));
#203288=CARTESIAN_POINT('Ctrl Pts',(-16.8725738817601,20.2199622610429,
19.226628795461));
#203289=CARTESIAN_POINT('Ctrl Pts',(-16.8059466662384,20.0920430349865,
19.2344809016797));
#203290=CARTESIAN_POINT('Ctrl Pts',(-16.7630527418978,19.9913797145756,
19.2403645402569));
#203291=CARTESIAN_POINT('Ctrl Pts',(-16.7105361226236,19.8357463335977,
19.2494985279907));
#203292=CARTESIAN_POINT('Ctrl Pts',(-16.6949896865018,19.7829705794275,
19.2526001135353));
#203293=CARTESIAN_POINT('Ctrl Pts',(-16.6731233521427,19.6964380022404,
19.2577351816077));
#203294=CARTESIAN_POINT('Ctrl Pts',(-16.6655381810007,19.663026679826,19.2597294558342));
#203295=CARTESIAN_POINT('Ctrl Pts',(-16.6566319193872,19.6188572875588,
19.2623868581051));
#203296=CARTESIAN_POINT('Ctrl Pts',(-16.6545776757776,19.6082511804153,
19.2630265310129));
#203297=CARTESIAN_POINT('Ctrl Pts',(-16.6513451368779,19.5908490340386,
19.2640788291151));
#203298=CARTESIAN_POINT('Ctrl Pts',(-16.6501187007899,19.5840620546476,
19.2644899153744));
#203299=CARTESIAN_POINT('Ctrl Pts',(-16.6478082567528,19.5709093047483,
19.2652879421731));
#203300=CARTESIAN_POINT('Ctrl Pts',(-16.6467201653675,19.5645443221721,
19.2656747478645));
#203301=CARTESIAN_POINT('Ctrl Pts',(-16.644274193639,19.5498312099219,19.2665703468044));
#203302=CARTESIAN_POINT('Ctrl Pts',(-16.6429371943768,19.5414797638049,
19.2670797971981));
#203303=CARTESIAN_POINT('Ctrl Pts',(-16.6394743233533,19.5189865216858,
19.2684549500153));
#203304=CARTESIAN_POINT('Ctrl Pts',(-16.6374416711351,19.5048310153593,
19.2693235861058));
#203305=CARTESIAN_POINT('Ctrl Pts',(-16.6200053137569,19.3739944049202,
19.2773832049));
#203306=CARTESIAN_POINT('Ctrl Pts',(-16.614215954678,19.2562586098793,19.2848805640885));
#203307=CARTESIAN_POINT('Ctrl Pts',(-16.623825124451,18.9751838202362,19.3032565838769));
#203308=CARTESIAN_POINT('Ctrl Pts',(-16.6483428164416,18.8129023375953,
19.3142741634878));
#203309=CARTESIAN_POINT('Ctrl Pts',(-16.699437533551,18.6251631820092,19.3266195441605));
#203310=CARTESIAN_POINT('Ctrl Pts',(-16.7082309720774,18.595443920189,19.3285596068383));
#203311=CARTESIAN_POINT('Ctrl Pts',(-16.7198477210385,18.559133085433,19.3309034076885));
#203312=CARTESIAN_POINT('Ctrl Pts',(-16.7220555274467,18.552350381573,19.3313400661016));
#203313=CARTESIAN_POINT('Ctrl Pts',(-16.7255819785141,18.5416998075673,
19.3320237699227));
#203314=CARTESIAN_POINT('Ctrl Pts',(-16.7268775887796,18.5378244481199,
19.3322721351946));
#203315=CARTESIAN_POINT('Ctrl Pts',(-16.7293279256252,18.5305650960337,
19.3327365730172));
#203316=CARTESIAN_POINT('Ctrl Pts',(-16.7304799912676,18.5271803167993,
19.3329527922301));
#203317=CARTESIAN_POINT('Ctrl Pts',(-16.733139611945,18.5194307476886,19.3334470912534));
#203318=CARTESIAN_POINT('Ctrl Pts',(-16.7346528737838,18.5150679680834,
19.3337248296645));
#203319=CARTESIAN_POINT('Ctrl Pts',(-16.7393843956434,18.5015696620112,
19.3345825786688));
#203320=CARTESIAN_POINT('Ctrl Pts',(-16.7426511368823,18.4924510962974,
19.3351597918934));
#203321=CARTESIAN_POINT('Ctrl Pts',(-16.782233407973,18.3843072369727,19.3419824613633));
#203322=CARTESIAN_POINT('Ctrl Pts',(-16.825843217814,18.288092902431,19.347826747512));
#203323=CARTESIAN_POINT('Ctrl Pts',(-16.8828238724875,18.1838619972237,
19.3543153306785));
#203324=CARTESIAN_POINT('Ctrl Pts',(-16.8893067805204,18.1722640078486,
19.3550395624094));
#203325=CARTESIAN_POINT('Ctrl Pts',(-16.9500458701202,18.0659633657181,
19.3617043523912));
#203326=CARTESIAN_POINT('Ctrl Pts',(-17.0114401382486,17.9755293015901,
19.367582333004));
#203327=CARTESIAN_POINT('Ctrl Pts',(-17.1265553838227,17.8313289783191,
19.3778440205913));
#203328=CARTESIAN_POINT('Ctrl Pts',(-17.1766884818254,17.7749813951203,
19.3821175480254));
#203329=CARTESIAN_POINT('Ctrl Pts',(-17.2429809863635,17.7080340220333,
19.3876184696232));
#203330=CARTESIAN_POINT('Ctrl Pts',(-17.2564243099218,17.6948158172497,
19.3887267200522));
#203331=CARTESIAN_POINT('Ctrl Pts',(-17.2762273314517,17.6758579329323,
19.3903497715966));
#203332=CARTESIAN_POINT('Ctrl Pts',(-17.282448394039,17.6699742860051,19.3908583184327));
#203333=CARTESIAN_POINT('Ctrl Pts',(-17.2934182847214,17.6597247402399,
19.3917528344675));
#203334=CARTESIAN_POINT('Ctrl Pts',(-17.2981517212091,17.655342477018,19.3921380949773));
#203335=CARTESIAN_POINT('Ctrl Pts',(-17.3073819409107,17.6468750617717,
19.3928880058906));
#203336=CARTESIAN_POINT('Ctrl Pts',(-17.3118764307328,17.6427874948064,
19.3932525480644));
#203337=CARTESIAN_POINT('Ctrl Pts',(-17.3226630549573,17.6330619769255,
19.3941260119258));
#203338=CARTESIAN_POINT('Ctrl Pts',(-17.3289714303737,17.6274422674233,
19.3946356944235));
#203339=CARTESIAN_POINT('Ctrl Pts',(-17.3518580106305,17.6072985618245,
19.3964808122856));
#203340=CARTESIAN_POINT('Ctrl Pts',(-17.3686287026021,17.5929963089691,
19.3978253935882));
#203341=CARTESIAN_POINT('Ctrl Pts',(-17.5292457002971,17.4602956773197,
19.4106372794999));
#203342=CARTESIAN_POINT('Ctrl Pts',(-17.6878828996533,17.3611325344479,
19.4229109461565));
#203343=CARTESIAN_POINT('Ctrl Pts',(-17.9299281455313,17.2510237596132,
19.4404658321746));
#203344=CARTESIAN_POINT('Ctrl Pts',(-18.0042692086399,17.2221477973117,
19.4457001127579));
#203345=CARTESIAN_POINT('Ctrl Pts',(-18.1142142211104,17.1864398711878,
19.4530682522978));
#203346=CARTESIAN_POINT('Ctrl Pts',(-18.1486417971045,17.1762188678025,
19.455323835402));
#203347=CARTESIAN_POINT('Ctrl Pts',(-18.1905168607368,17.1649377553637,
19.4579918904362));
#203348=CARTESIAN_POINT('Ctrl Pts',(-18.1977290814757,17.1630356113103,
19.4584487351114));
#203349=CARTESIAN_POINT('Ctrl Pts',(-18.2089770486817,17.1601325770354,
19.4591568860153));
#203350=CARTESIAN_POINT('Ctrl Pts',(-18.2130058626501,17.1591054131555,
19.4594096698069));
#203351=CARTESIAN_POINT('Ctrl Pts',(-18.2204957745019,17.1572193089659,
19.4598779810289));
#203352=CARTESIAN_POINT('Ctrl Pts',(-18.2239559835913,17.1563572529343,
19.4600936816281));
#203353=CARTESIAN_POINT('Ctrl Pts',(-18.2317999597048,17.1544240876331,
19.4605811946995));
#203354=CARTESIAN_POINT('Ctrl Pts',(-18.2361849719355,17.1533582521489,
19.4608527011257));
#203355=CARTESIAN_POINT('Ctrl Pts',(-18.2475195531728,17.1506415856584,
19.4615519300798));
#203356=CARTESIAN_POINT('Ctrl Pts',(-18.2544741939716,17.149011875563,19.4619784668367));
#203357=CARTESIAN_POINT('Ctrl Pts',(-18.2973128436093,17.1392017725516,
19.4645912322538));
#203358=CARTESIAN_POINT('Ctrl Pts',(-18.3333992389099,17.1319225686439,
19.4667293464963));
#203359=CARTESIAN_POINT('Ctrl Pts',(-18.5372545400412,17.0963071907067,
19.4785490410011));
#203360=CARTESIAN_POINT('Ctrl Pts',(-18.7077828051435,17.0873335752921,
19.4875021820234));
#203361=CARTESIAN_POINT('Ctrl Pts',(-18.9729221913493,17.1053549287741,
19.5021193022167));
#203362=CARTESIAN_POINT('Ctrl Pts',(-19.0677256280792,17.1182866662317,
19.5074779677641));
#203363=CARTESIAN_POINT('Ctrl Pts',(-19.1822978235601,17.1418995625317,
19.5142895534746));
#203364=CARTESIAN_POINT('Ctrl Pts',(-19.2032036328508,17.1465399106918,
19.5155460470912));
#203365=CARTESIAN_POINT('Ctrl Pts',(-19.2328036959159,17.1535829013516,
19.5173458569852));
#203366=CARTESIAN_POINT('Ctrl Pts',(-19.2415589656451,17.1557252890582,
19.5178808110472));
#203367=CARTESIAN_POINT('Ctrl Pts',(-19.2566302080594,17.1595153500928,
19.5188062641754));
#203368=CARTESIAN_POINT('Ctrl Pts',(-19.2629527797747,17.1611364536929,
19.5191959006996));
#203369=CARTESIAN_POINT('Ctrl Pts',(-19.2750379683482,17.1642947240077,
19.5199433829838));
#203370=CARTESIAN_POINT('Ctrl Pts',(-19.2808017926091,17.1658270565946,
19.5203010687652));
#203371=CARTESIAN_POINT('Ctrl Pts',(-19.295759345937,17.1698713241267,19.5212324140364));
#203372=CARTESIAN_POINT('Ctrl Pts',(-19.3049426485793,17.1724210043251,
19.5218072952429));
#203373=CARTESIAN_POINT('Ctrl Pts',(-19.3361289682145,17.1813069240238,
19.5237702343509));
#203374=CARTESIAN_POINT('Ctrl Pts',(-19.3580456744929,17.1879379128245,
19.5251678515803));
#203375=CARTESIAN_POINT('Ctrl Pts',(-19.548203047858,17.2488547856926,19.537457156646));
#203376=CARTESIAN_POINT('Ctrl Pts',(-19.7091077895023,17.3236523101553,
19.5490643047287));
#203377=CARTESIAN_POINT('Ctrl Pts',(-19.9317637694991,17.4632969362629,
19.5664282131301));
#203378=CARTESIAN_POINT('Ctrl Pts',(-20.0018593303351,17.5134609994542,
19.5721011973772));
#203379=CARTESIAN_POINT('Ctrl Pts',(-20.097888861105,17.5914601044017,19.579998338313));
#203380=CARTESIAN_POINT('Ctrl Pts',(-20.1264353098609,17.6159368006453,
19.5823627329963));
#203381=CARTESIAN_POINT('Ctrl Pts',(-20.159921597287,17.6462336497171,19.5851414786787));
#203382=CARTESIAN_POINT('Ctrl Pts',(-20.1654994975822,17.6513348676824,
19.585604517822));
#203383=CARTESIAN_POINT('Ctrl Pts',(-20.1741190256151,17.6593029743435,
19.5863201575645));
#203384=CARTESIAN_POINT('Ctrl Pts',(-20.1771796217529,17.6621491203399,
19.5865742856182));
#203385=CARTESIAN_POINT('Ctrl Pts',(-20.1828344831225,17.6674390707224,
19.587043825551));
#203386=CARTESIAN_POINT('Ctrl Pts',(-20.1854309831364,17.6698803409972,
19.5872594185393));
#203387=CARTESIAN_POINT('Ctrl Pts',(-20.191280159151,17.6754077231099,19.5877450956895));
#203388=CARTESIAN_POINT('Ctrl Pts',(-20.1945291941452,17.6784976094637,
19.5880148835894));
#203389=CARTESIAN_POINT('Ctrl Pts',(-20.2040697214724,17.6876287084534,
19.5888072098692));
#203390=CARTESIAN_POINT('Ctrl Pts',(-20.2103338113511,17.6936985924732,
19.5893275825398));
#203391=CARTESIAN_POINT('Ctrl Pts',(-20.2546653754833,17.7371902075102,
19.5930129526955));
#203392=CARTESIAN_POINT('Ctrl Pts',(-20.2913463584163,17.7760045888628,
19.5960764366407));
#203393=CARTESIAN_POINT('Ctrl Pts',(-20.3355351790522,17.8264563437825,
19.5998480552725));
#203394=CARTESIAN_POINT('Ctrl Pts',(-20.3444469243096,17.83683233148,19.6006131013246));
#203395=CARTESIAN_POINT('Ctrl Pts',(-20.3868878945445,17.8872265294452,
19.6042819091224));
#203396=CARTESIAN_POINT('Ctrl Pts',(-20.41903072729,17.928390774779,19.6071384787977));
#203397=CARTESIAN_POINT('Ctrl Pts',(-20.5137301712,18.0593821262715,19.6159391053306));
#203398=CARTESIAN_POINT('Ctrl Pts',(-20.5708676845734,18.1528981882664,
19.6218309622777));
#203399=CARTESIAN_POINT('Ctrl Pts',(-20.6549212173413,18.3179719316179,
19.6321302759991));
#203400=CARTESIAN_POINT('Ctrl Pts',(-20.6856664510528,18.3873290901251,
19.6364279098019));
#203401=CARTESIAN_POINT('Ctrl Pts',(-20.7193494083111,18.4758575524414,
19.6419578861143));
#203402=CARTESIAN_POINT('Ctrl Pts',(-20.7258375509708,18.493622953052,19.6430696069066));
#203403=CARTESIAN_POINT('Ctrl Pts',(-20.7349196687835,18.5195645463489,
19.6446968180629));
#203404=CARTESIAN_POINT('Ctrl Pts',(-20.7377034727636,18.527673652325,19.6452060082569));
#203405=CARTESIAN_POINT('Ctrl Pts',(-20.7424958165883,18.541914664089,19.6461012683676));
#203406=CARTESIAN_POINT('Ctrl Pts',(-20.7445257362882,18.5480392965761,
19.6464866259066));
#203407=CARTESIAN_POINT('Ctrl Pts',(-20.7484115459096,18.5599454756364,
19.6472364380232));
#203408=CARTESIAN_POINT('Ctrl Pts',(-20.7502706246648,18.5657259210947,
19.6476007830185));
#203409=CARTESIAN_POINT('Ctrl Pts',(-20.7546531727144,18.5795564733271,
19.6484733100267));
#203410=CARTESIAN_POINT('Ctrl Pts',(-20.7571534260446,18.5876137768294,
19.6489822491658));
#203411=CARTESIAN_POINT('Ctrl Pts',(-20.7659891994505,18.6167010109599,
19.6508219303307));
#203412=CARTESIAN_POINT('Ctrl Pts',(-20.772045345411,18.6378137230619,19.6521617482522));
#203413=CARTESIAN_POINT('Ctrl Pts',(-20.8265422866381,18.8395937663336,
19.6650135735315));
#203414=CARTESIAN_POINT('Ctrl Pts',(-20.8511563470631,19.0258066908902,
19.6773393374397));
#203415=CARTESIAN_POINT('Ctrl Pts',(-20.850946310095,19.2757905616587,19.6938413459655));
#203416=CARTESIAN_POINT('Ctrl Pts',(-20.8480800912412,19.3387716790032,
19.6979838416257));
#203417=CARTESIAN_POINT('Ctrl Pts',(-20.8379188606408,19.4512138802063,
19.7052635903443));
#203418=CARTESIAN_POINT('Ctrl Pts',(-20.8316744049217,19.5007244175735,
19.7084279455097));
#203419=CARTESIAN_POINT('Ctrl Pts',(-20.8224344769448,19.5576864775276,
19.7119866950838));
#203420=CARTESIAN_POINT('Ctrl Pts',(-20.8211403746751,19.5653940446792,
19.7124664790857));
#203421=CARTESIAN_POINT('Ctrl Pts',(-20.8190058160902,19.5776899264423,
19.7132288856703));
#203422=CARTESIAN_POINT('Ctrl Pts',(-20.8181928415456,19.5822828510634,
19.7135130019263));
#203423=CARTESIAN_POINT('Ctrl Pts',(-20.8167271896715,19.5904065697911,
19.7140143026017));
#203424=CARTESIAN_POINT('Ctrl Pts',(-20.8160807012237,19.5939384364748,
19.7142318347685));
#203425=CARTESIAN_POINT('Ctrl Pts',(-20.8146926430744,19.6014141754152,
19.7146913854627));
#203426=CARTESIAN_POINT('Ctrl Pts',(-20.8139488460453,19.6053575810862,
19.7149332755635));
#203427=CARTESIAN_POINT('Ctrl Pts',(-20.8119140362788,19.6159796643295,
19.7155834940726));
#203428=CARTESIAN_POINT('Ctrl Pts',(-20.8106020269407,19.6226543395387,
19.7159906425494));
#203429=CARTESIAN_POINT('Ctrl Pts',(-20.8039707292014,19.6555515583572,
19.7179907747884));
#203430=CARTESIAN_POINT('Ctrl Pts',(-20.7981865499891,19.6816792383203,
19.7195587194152));
#203431=CARTESIAN_POINT('Ctrl Pts',(-20.7800922296375,19.7566481994357,
19.7240163436332));
#203432=CARTESIAN_POINT('Ctrl Pts',(-20.7665321440998,19.8051709596792,
19.7268506308771));
#203433=CARTESIAN_POINT('Ctrl Pts',(-20.7422796869634,19.8813557567109,
19.7312843855716));
#203434=CARTESIAN_POINT('Ctrl Pts',(-20.7327195890317,19.9093429217765,
19.7329095481473));
#203435=CARTESIAN_POINT('Ctrl Pts',(-20.7225805741668,19.9371103910883,
19.7345261348292));
#203436=CARTESIAN_POINT('Origin',(-18.734,19.211,0.));
#203437=CARTESIAN_POINT('',(-20.7225806115196,19.937110288791,20.7554137119617));
#203438=CARTESIAN_POINT('',(-20.7225806064498,19.9371103026755,20.5336910513061));
#203439=CARTESIAN_POINT('',(-20.7225806064498,19.9371103026755,0.));
#203440=CARTESIAN_POINT('Ctrl Pts',(-20.7225806115197,19.937110288791,20.7554137119617));
#203441=CARTESIAN_POINT('Ctrl Pts',(-20.7319594608855,19.9114246618344,
20.7536067965805));
#203442=CARTESIAN_POINT('Ctrl Pts',(-20.7408447670006,19.8855460679731,
20.7517981735461));
#203443=CARTESIAN_POINT('Ctrl Pts',(-20.7725200156157,19.7871126712942,
20.744976017502));
#203444=CARTESIAN_POINT('Ctrl Pts',(-20.791895809394,19.7135296827932,20.7399903788199));
#203445=CARTESIAN_POINT('Ctrl Pts',(-20.8143280456744,19.6048809225687,
20.7329254081469));
#203446=CARTESIAN_POINT('Ctrl Pts',(-20.8205389580097,19.5705308933176,
20.730734451597));
#203447=CARTESIAN_POINT('Ctrl Pts',(-20.8270336482829,19.528732356022,20.7281324246831));
#203448=CARTESIAN_POINT('Ctrl Pts',(-20.8281309514486,19.5214178873819,
20.7276794520147));
#203449=CARTESIAN_POINT('Ctrl Pts',(-20.8297832003997,19.5099965687853,
20.7269759956358));
#203450=CARTESIAN_POINT('Ctrl Pts',(-20.8303644473521,19.5058936686014,
20.72672406501));
#203451=CARTESIAN_POINT('Ctrl Pts',(-20.831423622601,19.4982557598256,20.7262565460339));
#203452=CARTESIAN_POINT('Ctrl Pts',(-20.8319046586589,19.4947212851344,
20.7260407894414));
#203453=CARTESIAN_POINT('Ctrl Pts',(-20.8329764095951,19.4866946847737,
20.7255521419681));
#203454=CARTESIAN_POINT('Ctrl Pts',(-20.8335616373001,19.4822018792406,
20.7252795633578));
#203455=CARTESIAN_POINT('Ctrl Pts',(-20.8352591881885,19.4688348537539,
20.7244712782587));
#203456=CARTESIAN_POINT('Ctrl Pts',(-20.8363297205133,19.4599552979474,
20.7239378705038));
#203457=CARTESIAN_POINT('Ctrl Pts',(-20.84407733881,19.3920752179413,20.7198853164858));
#203458=CARTESIAN_POINT('Ctrl Pts',(-20.8483264321573,19.332818346711,20.7164920697119));
#203459=CARTESIAN_POINT('Ctrl Pts',(-20.8506770362225,19.2531771322551,
20.7120328020572));
#203460=CARTESIAN_POINT('Ctrl Pts',(-20.8509840406739,19.2328904078398,
20.7109057277409));
#203461=CARTESIAN_POINT('Ctrl Pts',(-20.8511051845657,19.0728052824201,
20.7020608117506));
#203462=CARTESIAN_POINT('Ctrl Pts',(-20.8373639114502,18.9333413712754,
20.6946257510641));
#203463=CARTESIAN_POINT('Ctrl Pts',(-20.7922497953957,18.7075304791036,
20.6818795084201));
#203464=CARTESIAN_POINT('Ctrl Pts',(-20.7688588121515,18.6200511751906,
20.6767638173073));
#203465=CARTESIAN_POINT('Ctrl Pts',(-20.7355595959724,18.5213358782081,
20.670656054497));
#203466=CARTESIAN_POINT('Ctrl Pts',(-20.731045868669,18.5083726433531,20.6698472828421));
#203467=CARTESIAN_POINT('Ctrl Pts',(-20.7236045524634,18.4876526117024,
20.6685433909434));
#203468=CARTESIAN_POINT('Ctrl Pts',(-20.7207568610039,18.4798673912279,
20.6680509247335));
#203469=CARTESIAN_POINT('Ctrl Pts',(-20.7156191778919,18.4660733041462,
20.6671737389019));
#203470=CARTESIAN_POINT('Ctrl Pts',(-20.7133473834866,18.4600577369328,
20.6667896316463));
#203471=CARTESIAN_POINT('Ctrl Pts',(-20.7085566166868,18.4475448755953,
20.6659873429947));
#203472=CARTESIAN_POINT('Ctrl Pts',(-20.7060329030993,18.4410494907019,
20.665569005995));
#203473=CARTESIAN_POINT('Ctrl Pts',(-20.6993949387511,18.4242118304519,
20.6644796438639));
#203474=CARTESIAN_POINT('Ctrl Pts',(-20.6952311498232,18.4138894314087,
20.6638069544908));
#203475=CARTESIAN_POINT('Ctrl Pts',(-20.6767885690955,18.3691880460115,
20.6608723820402));
#203476=CARTESIAN_POINT('Ctrl Pts',(-20.6616864794048,18.3351579187671,
20.6585827206034));
#203477=CARTESIAN_POINT('Ctrl Pts',(-20.6191743051355,18.2457963052023,
20.6524167207909));
#203478=CARTESIAN_POINT('Ctrl Pts',(-20.5902290418303,18.1912387775485,
20.6484906099546));
#203479=CARTESIAN_POINT('Ctrl Pts',(-20.4847193340871,18.0117847032291,
20.6350415632723));
#203480=CARTESIAN_POINT('Ctrl Pts',(-20.3975967056339,17.8935872679175,
20.6252363275487));
#203481=CARTESIAN_POINT('Ctrl Pts',(-20.2858389487258,17.7709076254773,
20.6144037567855));
#203482=CARTESIAN_POINT('Ctrl Pts',(-20.2724917961671,17.7566571257403,
20.6131348661711));
#203483=CARTESIAN_POINT('Ctrl Pts',(-20.2223172484832,17.7045505680223,
20.6084614050712));
#203484=CARTESIAN_POINT('Ctrl Pts',(-20.1842711531,17.6678886251204,20.605105231731));
#203485=CARTESIAN_POINT('Ctrl Pts',(-20.1384093794248,17.6268917773531,
20.601310736214));
#203486=CARTESIAN_POINT('Ctrl Pts',(-20.1318927161191,17.6211382053026,
20.6007772142511));
#203487=CARTESIAN_POINT('Ctrl Pts',(-20.1219663903597,17.6124824547285,
20.5999733084864));
#203488=CARTESIAN_POINT('Ctrl Pts',(-20.1185827491749,17.6095507641988,
20.5997008031928));
#203489=CARTESIAN_POINT('Ctrl Pts',(-20.1124893426092,17.6043049979951,
20.5992128389033));
#203490=CARTESIAN_POINT('Ctrl Pts',(-20.1097830253459,17.6019870215254,
20.5989970938741));
#203491=CARTESIAN_POINT('Ctrl Pts',(-20.1038860824252,17.5969620114554,
20.5985291224611));
#203492=CARTESIAN_POINT('Ctrl Pts',(-20.1006932904125,17.5942576092882,
20.5982770887486));
#203493=CARTESIAN_POINT('Ctrl Pts',(-20.0916937737522,17.5866804261981,
20.5975703739912));
#203494=CARTESIAN_POINT('Ctrl Pts',(-20.0858687975873,17.5818292848294,
20.5971172488461));
#203495=CARTESIAN_POINT('Ctrl Pts',(-20.0507099894218,17.5528668276233,
20.5944070919613));
#203496=CARTESIAN_POINT('Ctrl Pts',(-20.0207558647556,17.5295153697371,
20.5922013954487));
#203497=CARTESIAN_POINT('Ctrl Pts',(-19.9196794697699,17.4550027540113,
20.5850329924155));
#203498=CARTESIAN_POINT('Ctrl Pts',(-19.8460072153081,17.4074466970137,
20.5802385721238));
#203499=CARTESIAN_POINT('Ctrl Pts',(-19.6172789241837,17.2791600141768,
20.5659713132993));
#203500=CARTESIAN_POINT('Ctrl Pts',(-19.4549969360529,17.2129148995996,
20.5565784041035));
#203501=CARTESIAN_POINT('Ctrl Pts',(-19.264170974169,17.1613318975066,20.5450925279135));
#203502=CARTESIAN_POINT('Ctrl Pts',(-19.2418174041197,17.1556795834021,
20.5437418189163));
#203503=CARTESIAN_POINT('Ctrl Pts',(-19.2100739715762,17.1482024059493,
20.5418145788387));
#203504=CARTESIAN_POINT('Ctrl Pts',(-19.2007567289617,17.146074216382,20.5412477970871));
#203505=CARTESIAN_POINT('Ctrl Pts',(-19.1855973918144,17.1427194517776,
20.5403237225324));
#203506=CARTESIAN_POINT('Ctrl Pts',(-19.1797638916359,17.1414543536712,
20.5399676695837));
#203507=CARTESIAN_POINT('Ctrl Pts',(-19.1675441579272,17.1388583499105,
20.5392208366072));
#203508=CARTESIAN_POINT('Ctrl Pts',(-19.1611569757308,17.1375322593504,
20.5388299066604));
#203509=CARTESIAN_POINT('Ctrl Pts',(-19.1459516440064,17.1344486061607,
20.5378978712834));
#203510=CARTESIAN_POINT('Ctrl Pts',(-19.137128278846,17.132717671934,20.5373559214713));
#203511=CARTESIAN_POINT('Ctrl Pts',(-19.1073848159145,17.1270792492144,
20.5355251447754));
#203512=CARTESIAN_POINT('Ctrl Pts',(-19.0864174187928,17.1234311203348,
20.5342281069482));
#203513=CARTESIAN_POINT('Ctrl Pts',(-18.9080248086676,17.0951566177093,
20.5231347158308));
#203514=CARTESIAN_POINT('Ctrl Pts',(-18.7483666254294,17.0880649382601,
20.5127652433662));
#203515=CARTESIAN_POINT('Ctrl Pts',(-18.458107873658,17.1079294302074,20.4935470591489));
#203516=CARTESIAN_POINT('Ctrl Pts',(-18.3278725959667,17.1291525195447,
20.4848055002219));
#203517=CARTESIAN_POINT('Ctrl Pts',(-18.1852097317475,17.1663078288577,
20.4756083763572));
#203518=CARTESIAN_POINT('Ctrl Pts',(-18.1700194199341,17.170445474349,20.4746342979864));
#203519=CARTESIAN_POINT('Ctrl Pts',(-18.1492987920717,17.1763385734168,
20.4733140610667));
#203520=CARTESIAN_POINT('Ctrl Pts',(-18.1437278747749,17.1779477519309,
20.4729599469653));
#203521=CARTESIAN_POINT('Ctrl Pts',(-18.1348886176375,17.1805403969771,
20.4723995005999));
#203522=CARTESIAN_POINT('Ctrl Pts',(-18.1316159712683,17.1815088986902,
20.4721923107605));
#203523=CARTESIAN_POINT('Ctrl Pts',(-18.1248643808252,17.183524723435,20.4717655314615));
#203524=CARTESIAN_POINT('Ctrl Pts',(-18.1213857891828,17.1845730882947,
20.4715460102469));
#203525=CARTESIAN_POINT('Ctrl Pts',(-18.1131073251393,17.1870912853772,
20.4710244270176));
#203526=CARTESIAN_POINT('Ctrl Pts',(-18.1083099118622,17.1885692561649,
20.470722839672));
#203527=CARTESIAN_POINT('Ctrl Pts',(-18.0921655793462,17.1936058909986,
20.4697100607117));
#203528=CARTESIAN_POINT('Ctrl Pts',(-18.0808431626198,17.1972431688565,
20.4690033218647));
#203529=CARTESIAN_POINT('Ctrl Pts',(-17.9457644037088,17.2418957899126,
20.4606076528749));
#203530=CARTESIAN_POINT('Ctrl Pts',(-17.8260028073034,17.2941698765269,
20.4535153747759));
#203531=CARTESIAN_POINT('Ctrl Pts',(-17.5697669395943,17.4354558547063,
20.4376192524189));
#203532=CARTESIAN_POINT('Ctrl Pts',(-17.4372220491727,17.529823152826,20.428839909868));
#203533=CARTESIAN_POINT('Ctrl Pts',(-17.2991276785097,17.6542747879464,
20.4180455186159));
#203534=CARTESIAN_POINT('Ctrl Pts',(-17.2817710489797,17.6704536774819,
20.4166561462275));
#203535=CARTESIAN_POINT('Ctrl Pts',(-17.2577300776008,17.6936307002352,
20.4146830950954));
#203536=CARTESIAN_POINT('Ctrl Pts',(-17.2508157880993,17.7003885130496,
20.4141098133899));
#203537=CARTESIAN_POINT('Ctrl Pts',(-17.2396937293743,17.7114088425107,
20.4131780377926));
#203538=CARTESIAN_POINT('Ctrl Pts',(-17.2354572831054,17.7156423188553,
20.4128208258322));
#203539=CARTESIAN_POINT('Ctrl Pts',(-17.2266562504412,17.7245121421823,
20.4120738932573));
#203540=CARTESIAN_POINT('Ctrl Pts',(-17.2220949648797,17.7291516629275,
20.4116840330172));
#203541=CARTESIAN_POINT('Ctrl Pts',(-17.2113470127608,17.7401852466036,
20.4107588038574));
#203542=CARTESIAN_POINT('Ctrl Pts',(-17.2051791613167,17.7465973921808,
20.4102226229608));
#203543=CARTESIAN_POINT('Ctrl Pts',(-17.1847745268702,17.7680796195697,
20.4084311588112));
#203544=CARTESIAN_POINT('Ctrl Pts',(-17.1707190562697,17.7833195617206,
20.4071681362666));
#203545=CARTESIAN_POINT('Ctrl Pts',(-17.0968871011185,17.8657711017735,
20.400374317518));
#203546=CARTESIAN_POINT('Ctrl Pts',(-17.0412232627048,17.9365264810432,
20.3946755832227));
#203547=CARTESIAN_POINT('Ctrl Pts',(-16.9134444272628,18.1221449757554,
20.380071654885));
#203548=CARTESIAN_POINT('Ctrl Pts',(-16.8475388060186,18.2407998440682,
20.3710207776676));
#203549=CARTESIAN_POINT('Ctrl Pts',(-16.7632408397996,18.4341472259182,
20.3572277647944));
#203550=CARTESIAN_POINT('Ctrl Pts',(-16.73678177814,18.5049449098675,20.3523662003512));
#203551=CARTESIAN_POINT('Ctrl Pts',(-16.7113184618252,18.5860692024997,
20.3471147443877));
#203552=CARTESIAN_POINT('Ctrl Pts',(-16.7085366015627,18.5951451990588,
20.3465316486341));
#203553=CARTESIAN_POINT('Ctrl Pts',(-16.7045031605297,18.6086275618938,
20.3456723275603));
#203554=CARTESIAN_POINT('Ctrl Pts',(-16.7032047245632,18.6130196275928,
20.3453934677242));
#203555=CARTESIAN_POINT('Ctrl Pts',(-16.7009190838297,18.6208443044117,
20.3448986220294));
#203556=CARTESIAN_POINT('Ctrl Pts',(-16.6999263046087,18.6242752271264,
20.3446823147866));
#203557=CARTESIAN_POINT('Ctrl Pts',(-16.6978096390765,18.6316601082382,
20.3442181733061));
#203558=CARTESIAN_POINT('Ctrl Pts',(-16.6966885873758,18.6356148205278,
20.3439705047833));
#203559=CARTESIAN_POINT('Ctrl Pts',(-16.6936238539204,18.6465474765274,
20.3432882160112));
#203560=CARTESIAN_POINT('Ctrl Pts',(-16.6917044350856,18.6535322451253,
20.3428549835999));
#203561=CARTESIAN_POINT('Ctrl Pts',(-16.6813527832255,18.6919730489355,
20.3404846691113));
#203562=CARTESIAN_POINT('Ctrl Pts',(-16.6736109104277,18.723612438899,20.3385851003717));
#203563=CARTESIAN_POINT('Ctrl Pts',(-16.6315987518309,18.9142613278309,
20.3273764793654));
#203564=CARTESIAN_POINT('Ctrl Pts',(-16.6150144513749,19.0766239483737,
20.3187792468002));
#203565=CARTESIAN_POINT('Ctrl Pts',(-16.6187508688498,19.3561207785592,
20.3034768593061));
#203566=CARTESIAN_POINT('Ctrl Pts',(-16.6299799881108,19.4725978897949,
20.2969546135077));
#203567=CARTESIAN_POINT('Ctrl Pts',(-16.6532984651167,19.6016076314741,
20.2892743280244));
#203568=CARTESIAN_POINT('Ctrl Pts',(-16.6559824261698,19.615643234189,20.2884328251108));
#203569=CARTESIAN_POINT('Ctrl Pts',(-16.6604801817901,19.6379379861606,
20.2870862559164));
#203570=CARTESIAN_POINT('Ctrl Pts',(-16.6622017498402,19.6462154501024,
20.2865841308636));
#203571=CARTESIAN_POINT('Ctrl Pts',(-16.6653254325329,19.6607957573312,
20.285695729946));
#203572=CARTESIAN_POINT('Ctrl Pts',(-16.6667068937379,19.667102949754,20.2853101201121));
#203573=CARTESIAN_POINT('Ctrl Pts',(-16.6696238752663,19.6801351604111,
20.2845106172281));
#203574=CARTESIAN_POINT('Ctrl Pts',(-16.6711634531293,19.6868591832116,
20.2840965978255));
#203575=CARTESIAN_POINT('Ctrl Pts',(-16.6751997194969,19.7040996174062,
20.2830311069467));
#203576=CARTESIAN_POINT('Ctrl Pts',(-16.677744112739,19.7146045541937,20.2823781060042));
#203577=CARTESIAN_POINT('Ctrl Pts',(-16.6886997911577,19.7583691662894,
20.2796415520354));
#203578=CARTESIAN_POINT('Ctrl Pts',(-16.6978380967502,19.7914398641706,
20.2775346565797));
#203579=CARTESIAN_POINT('Ctrl Pts',(-16.7237398566325,19.8770181068045,
20.2719769928336));
#203580=CARTESIAN_POINT('Ctrl Pts',(-16.7417565160111,19.9291163151129,
20.2684877832575));
#203581=CARTESIAN_POINT('Ctrl Pts',(-16.8015457833695,20.0823653990312,
20.25791417993));
#203582=CARTESIAN_POINT('Ctrl Pts',(-16.8491453204952,20.1810393442023,
20.2506814069109));
#203583=CARTESIAN_POINT('Ctrl Pts',(-16.9285020628891,20.317440726491,20.2402571474394));
#203584=CARTESIAN_POINT('Ctrl Pts',(-16.95428280989,20.3584497122096,20.2370647154989));
#203585=CARTESIAN_POINT('Ctrl Pts',(-16.9913672209158,20.4131783104903,
20.2327518680978));
#203586=CARTESIAN_POINT('Ctrl Pts',(-17.0014698655874,20.4276926690173,
20.2316028871623));
#203587=CARTESIAN_POINT('Ctrl Pts',(-17.0427745989141,20.4854768865867,
20.2270123268101));
#203588=CARTESIAN_POINT('Ctrl Pts',(-17.0754280444275,20.5276908507773,
20.2236211945346));
#203589=CARTESIAN_POINT('Ctrl Pts',(-17.1152364292531,20.575320174496,20.2197919623708));
#203590=CARTESIAN_POINT('Ctrl Pts',(-17.1208698812611,20.5819763902199,
20.2192567625324));
#203591=CARTESIAN_POINT('Ctrl Pts',(-17.1294617005198,20.5920017898809,
20.2184508166554));
#203592=CARTESIAN_POINT('Ctrl Pts',(-17.1323898274872,20.595396602969,20.2181779338012));
#203593=CARTESIAN_POINT('Ctrl Pts',(-17.137665022377,20.6014734231494,20.2176895557199));
#203594=CARTESIAN_POINT('Ctrl Pts',(-17.1400080879951,20.6041588158979,
20.2174737723777));
#203595=CARTESIAN_POINT('Ctrl Pts',(-17.1451139090325,20.609980864961,20.2170060241877));
#203596=CARTESIAN_POINT('Ctrl Pts',(-17.1478791669049,20.6131152499392,
20.216754250361));
#203597=CARTESIAN_POINT('Ctrl Pts',(-17.1556721850333,20.6218959802807,
20.2160489851467));
#203598=CARTESIAN_POINT('Ctrl Pts',(-17.1607209933318,20.6275236777955,
20.2155970395043));
#203599=CARTESIAN_POINT('Ctrl Pts',(-17.1910740434903,20.6609944899808,
20.2129086417882));
#203600=CARTESIAN_POINT('Ctrl Pts',(-17.2170884181499,20.6881879279899,
20.2107225725016));
#203601=CARTESIAN_POINT('Ctrl Pts',(-17.3050599681396,20.7753702031143,
20.2036497927681));
#203602=CARTESIAN_POINT('Ctrl Pts',(-17.3699603895679,20.8322717350403,
20.1989262911385));
#203603=CARTESIAN_POINT('Ctrl Pts',(-17.5778023360435,20.9931566253885,
20.1846226480845));
#203604=CARTESIAN_POINT('Ctrl Pts',(-17.730408020612,21.0833439234493,20.1751339207402));
#203605=CARTESIAN_POINT('Ctrl Pts',(-17.9134551616087,21.1626454603613,
20.1635410827757));
#203606=CARTESIAN_POINT('Ctrl Pts',(-17.9346222919178,21.1714104300638,
20.1621988566356));
#203607=CARTESIAN_POINT('Ctrl Pts',(-17.9647924607332,21.1833335506415,
20.1602816708539));
#203608=CARTESIAN_POINT('Ctrl Pts',(-17.9736814654442,21.1867772128821,
20.1597163216907));
#203609=CARTESIAN_POINT('Ctrl Pts',(-17.9881694342987,21.1922777044502,
20.1587939589089));
#203610=CARTESIAN_POINT('Ctrl Pts',(-17.9937544296414,21.1943711375659,
20.1584381760813));
#203611=CARTESIAN_POINT('Ctrl Pts',(-18.0054694057876,21.198705907113,20.1576914007266));
#203612=CARTESIAN_POINT('Ctrl Pts',(-18.0116010459482,21.2009425493163,
20.1573002560392));
#203613=CARTESIAN_POINT('Ctrl Pts',(-18.026223355109,21.2061998486978,20.1563667679629));
#203614=CARTESIAN_POINT('Ctrl Pts',(-18.0347231103111,21.2091946959489,
20.1558235730168));
#203615=CARTESIAN_POINT('Ctrl Pts',(-18.063474169852,21.2191190806929,20.1539841059794));
#203616=CARTESIAN_POINT('Ctrl Pts',(-18.0838108543454,21.2257955611465,
20.1526795157118));
#203617=CARTESIAN_POINT('Ctrl Pts',(-18.1954218305781,21.2605713934878,
20.1454985875525));
#203618=CARTESIAN_POINT('Ctrl Pts',(-18.2884045165872,21.2827745397511,
20.1394321265378));
#203619=CARTESIAN_POINT('Ctrl Pts',(-18.5505653488837,21.3269081264424,
20.1221547077014));
#203620=CARTESIAN_POINT('Ctrl Pts',(-18.7213619391097,21.3348061779101,
20.1106597896389));
#203621=CARTESIAN_POINT('Ctrl Pts',(-18.9278509626435,21.3194253804058,
20.097445229846));
#203622=CARTESIAN_POINT('Ctrl Pts',(-18.9643736387357,21.3157479995503,
20.0951369196735));
#203623=CARTESIAN_POINT('Ctrl Pts',(-19.0078641269271,21.3102232772998,
20.0924372735665));
#203624=CARTESIAN_POINT('Ctrl Pts',(-19.0149391402448,21.3092881429308,
20.091999656085));
#203625=CARTESIAN_POINT('Ctrl Pts',(-19.0264781434135,21.3077035751006,
20.0912886202263));
#203626=CARTESIAN_POINT('Ctrl Pts',(-19.0309449585705,21.3070756280881,
20.0910140347365));
#203627=CARTESIAN_POINT('Ctrl Pts',(-19.0389393201024,21.3059257090552,
20.0905238279934));
#203628=CARTESIAN_POINT('Ctrl Pts',(-19.0424675729542,21.3054090986354,
20.09030790914));
#203629=CARTESIAN_POINT('Ctrl Pts',(-19.0501083029149,21.3042706082124,
20.0898412565913));
#203630=CARTESIAN_POINT('Ctrl Pts',(-19.0542202447514,21.3036455251458,
20.0895907064297));
#203631=CARTESIAN_POINT('Ctrl Pts',(-19.0657076913509,21.3018645916607,
20.0888923157202));
#203632=CARTESIAN_POINT('Ctrl Pts',(-19.0730790475414,21.3006818266059,
20.0884459728507));
#203633=CARTESIAN_POINT('Ctrl Pts',(-19.1159749303773,21.2935660447723,
20.085858307056));
#203634=CARTESIAN_POINT('Ctrl Pts',(-19.1513519635593,21.2867658502693,
20.0837630738567));
#203635=CARTESIAN_POINT('Ctrl Pts',(-19.2647854184227,21.2619439916857,
20.0771209800265));
#203636=CARTESIAN_POINT('Ctrl Pts',(-19.3420019693395,21.2403940049983,
20.0727154284637));
#203637=CARTESIAN_POINT('Ctrl Pts',(-19.5935258045246,21.1545469261092,
20.0582269968559));
#203638=CARTESIAN_POINT('Ctrl Pts',(-19.76056264221,21.0717316821763,20.0482971339798));
#203639=CARTESIAN_POINT('Ctrl Pts',(-19.9329971413593,20.9558733814055,
20.0362146834589));
#203640=CARTESIAN_POINT('Ctrl Pts',(-19.9511436682172,20.9432639807019,
20.0349193587355));
#203641=CARTESIAN_POINT('Ctrl Pts',(-19.9759578324821,20.9254390536575,
20.0331133193342));
#203642=CARTESIAN_POINT('Ctrl Pts',(-19.9827969500325,20.9204638635564,
20.0326118280876));
#203643=CARTESIAN_POINT('Ctrl Pts',(-19.9944992178101,20.9118432200179,
20.0317472244393));
#203644=CARTESIAN_POINT('Ctrl Pts',(-19.9993768526169,20.9082175337466,
20.0313848825236));
#203645=CARTESIAN_POINT('Ctrl Pts',(-20.0092323688007,20.9008255440933,
20.0306487201526));
#203646=CARTESIAN_POINT('Ctrl Pts',(-20.0142093374333,20.8970581291763,
20.0302748583196));
#203647=CARTESIAN_POINT('Ctrl Pts',(-20.0257370299678,20.8882515464841,
20.0294039696079));
#203648=CARTESIAN_POINT('Ctrl Pts',(-20.0322750185584,20.8831959448388,
20.0289062961787));
#203649=CARTESIAN_POINT('Ctrl Pts',(-20.0459563402021,20.872488048422,20.027856890871));
#203650=CARTESIAN_POINT('Ctrl Pts',(-20.0530931163535,20.866827684261,20.0273048427003));
#203651=CARTESIAN_POINT('Ctrl Pts',(-20.071994794807,20.8516365152644,20.0258302504324));
#203652=CARTESIAN_POINT('Ctrl Pts',(-20.0836941922862,20.8420253875333,
20.0249044937169));
#203653=CARTESIAN_POINT('Ctrl Pts',(-20.1190566220114,20.8123339060278,
20.0220657955205));
#203654=CARTESIAN_POINT('Ctrl Pts',(-20.1423812652576,20.7918586841645,
20.0201370322303));
#203655=CARTESIAN_POINT('Ctrl Pts',(-20.2893760931676,20.6569855062784,
20.0076101401539));
#203656=CARTESIAN_POINT('Ctrl Pts',(-20.3994520606363,20.5286955146946,
19.9964221181894));
#203657=CARTESIAN_POINT('Ctrl Pts',(-20.5482381121422,20.3064614442645,
19.9788043017855));
#203658=CARTESIAN_POINT('Ctrl Pts',(-20.597495842582,20.220397644303,19.9723516834433));
#203659=CARTESIAN_POINT('Ctrl Pts',(-20.6447646744775,20.1224611048589,
19.9656327945442));
#203660=CARTESIAN_POINT('Ctrl Pts',(-20.648918711576,20.1137011261553,19.9650371214703));
#203661=CARTESIAN_POINT('Ctrl Pts',(-20.6549630916588,20.1007253169797,
19.9641629148744));
#203662=CARTESIAN_POINT('Ctrl Pts',(-20.6568999796039,20.0965314836658,
19.9638816154837));
#203663=CARTESIAN_POINT('Ctrl Pts',(-20.6603117270737,20.0890802442637,
19.9633840817029));
#203664=CARTESIAN_POINT('Ctrl Pts',(-20.6617920753913,20.085825411134,19.9631675124284));
#203665=CARTESIAN_POINT('Ctrl Pts',(-20.6649460109109,20.0788439897306,
19.9627046254899));
#203666=CARTESIAN_POINT('Ctrl Pts',(-20.6666170558024,20.0751163138345,
19.9624584640114));
#203667=CARTESIAN_POINT('Ctrl Pts',(-20.6711741838904,20.0648711771758,
19.9617845754104));
#203668=CARTESIAN_POINT('Ctrl Pts',(-20.6740381883078,20.0583438718376,
19.9613581802235));
#203669=CARTESIAN_POINT('Ctrl Pts',(-20.6891489403583,20.0234269582299,
19.9590922948952));
#203670=CARTESIAN_POINT('Ctrl Pts',(-20.7008063068103,19.9947844856062,
19.9572865274356));
#203671=CARTESIAN_POINT('Ctrl Pts',(-20.7154851133572,19.956325874309,19.9549187250179));
#203672=CARTESIAN_POINT('Ctrl Pts',(-20.7190678396831,19.9467306315134,
19.9543326139909));
#203673=CARTESIAN_POINT('Ctrl Pts',(-20.7225806070201,19.9371103011137,
19.9537492499338));
#203674=CARTESIAN_POINT('',(-20.8509996091577,19.2097135994841,20.489056279057));
#203675=CARTESIAN_POINT('Ctrl Pts',(-20.7225805741668,19.9371103910883,
19.7345261348292));
#203676=CARTESIAN_POINT('Ctrl Pts',(-20.6874528645367,20.0333137808797,
19.7401269736001));
#203677=CARTESIAN_POINT('Ctrl Pts',(-20.6453763458548,20.1268797428984,
19.7456315769633));
#203678=CARTESIAN_POINT('Ctrl Pts',(-20.5472451465103,20.3085633188397,
19.7569907920168));
#203679=CARTESIAN_POINT('Ctrl Pts',(-20.4911568811255,20.3962842901653,
19.7628329049756));
#203680=CARTESIAN_POINT('Ctrl Pts',(-20.4204318604439,20.4907789784509,
19.7697496500948));
#203681=CARTESIAN_POINT('Ctrl Pts',(-20.4118958786208,20.5019500609643,
19.7705777418217));
#203682=CARTESIAN_POINT('Ctrl Pts',(-20.398090742683,20.5196486737819,19.771906854087));
#203683=CARTESIAN_POINT('Ctrl Pts',(-20.3928928706097,20.5262314594874,
19.7724050529998));
#203684=CARTESIAN_POINT('Ctrl Pts',(-20.3836314069099,20.5378182891011,
19.7732888969456));
#203685=CARTESIAN_POINT('Ctrl Pts',(-20.3795837994358,20.5428350155228,
19.7736738979507));
#203686=CARTESIAN_POINT('Ctrl Pts',(-20.3711396544079,20.55320368208,19.7744745067719));
#203687=CARTESIAN_POINT('Ctrl Pts',(-20.3667396426101,20.5585526816788,
19.7748902526454));
#203688=CARTESIAN_POINT('Ctrl Pts',(-20.3553245519944,20.5722917767487,
19.7759652279275));
#203689=CARTESIAN_POINT('Ctrl Pts',(-20.3482706301432,20.5806491996022,
19.776626039594));
#203690=CARTESIAN_POINT('Ctrl Pts',(-20.3180882549007,20.6158519458345,
19.7794392765532));
#203691=CARTESIAN_POINT('Ctrl Pts',(-20.2943535689076,20.6421677367845,
19.7816167106324));
#203692=CARTESIAN_POINT('Ctrl Pts',(-20.2303134738308,20.7096846878417,
19.7874064274032));
#203693=CARTESIAN_POINT('Ctrl Pts',(-20.1889686577498,20.7498551199264,
19.7910612723479));
#203694=CARTESIAN_POINT('Ctrl Pts',(-20.0462318602119,20.8776378722556,
19.8034000038617));
#203695=CARTESIAN_POINT('Ctrl Pts',(-19.9381729570585,20.9573094284539,
19.8123264104771));
#203696=CARTESIAN_POINT('Ctrl Pts',(-19.7463729164797,21.0724091967956,
19.8270272051316));
#203697=CARTESIAN_POINT('Ctrl Pts',(-19.6665527321374,21.1136540115788,
19.8328477324719));
#203698=CARTESIAN_POINT('Ctrl Pts',(-19.57550799869,21.1535875640848,19.8389897336681));
#203699=CARTESIAN_POINT('Ctrl Pts',(-19.5666425092047,21.1574040217694,
19.8395827352411));
#203700=CARTESIAN_POINT('Ctrl Pts',(-19.5535033405703,21.1629540304545,
19.8404537836909));
#203701=CARTESIAN_POINT('Ctrl Pts',(-19.5492497457969,21.1647344023998,
19.8407345682682));
#203702=CARTESIAN_POINT('Ctrl Pts',(-19.5416882441973,21.167870327662,19.8412315338358));
#203703=CARTESIAN_POINT('Ctrl Pts',(-19.5383826911072,21.1692314127856,
19.8414480468562));
#203704=CARTESIAN_POINT('Ctrl Pts',(-19.531287447963,21.1721319323638,19.8419111928304));
#203705=CARTESIAN_POINT('Ctrl Pts',(-19.5274967500655,21.1736687542994,
19.8421576676146));
#203706=CARTESIAN_POINT('Ctrl Pts',(-19.5170660107303,21.1778624179042,
19.8428332971481));
#203707=CARTESIAN_POINT('Ctrl Pts',(-19.5104168523787,21.180496641985,19.8432611084763));
#203708=CARTESIAN_POINT('Ctrl Pts',(-19.4746420261715,21.1944603701148,
19.845548135564));
#203709=CARTESIAN_POINT('Ctrl Pts',(-19.4452798777489,21.2051782317934,
19.847372878789));
#203710=CARTESIAN_POINT('Ctrl Pts',(-19.260629078845,21.2679822568139,19.8585873624618));
#203711=CARTESIAN_POINT('Ctrl Pts',(-19.0999557890122,21.3025551348048,
19.8672422485546));
#203712=CARTESIAN_POINT('Ctrl Pts',(-18.8202504278169,21.3294853923018,
19.8826237568739));
#203713=CARTESIAN_POINT('Ctrl Pts',(-18.7028972239463,21.3310110417204,
19.8891641172679));
#203714=CARTESIAN_POINT('Ctrl Pts',(-18.5717696863479,21.321823217635,19.8968647966411));
#203715=CARTESIAN_POINT('Ctrl Pts',(-18.5575209697598,21.3206797073814,
19.8977065677578));
#203716=CARTESIAN_POINT('Ctrl Pts',(-18.5348635439064,21.3186302275625,
19.8990534900374));
#203717=CARTESIAN_POINT('Ctrl Pts',(-18.526446641612,21.3178180046074,19.8995556976312));
#203718=CARTESIAN_POINT('Ctrl Pts',(-18.5116115659835,21.3162966721673,
19.9004441996928));
#203719=CARTESIAN_POINT('Ctrl Pts',(-18.505191311686,21.3156085802708,19.9008298277014));
#203720=CARTESIAN_POINT('Ctrl Pts',(-18.49191942482,21.3141247163812,19.901629324225));
#203721=CARTESIAN_POINT('Ctrl Pts',(-18.4850683402041,21.3133248094747,
19.9020433188774));
#203722=CARTESIAN_POINT('Ctrl Pts',(-18.467493998862,21.3111857851513,19.9031086533977));
#203723=CARTESIAN_POINT('Ctrl Pts',(-18.4567769623727,21.3097980277819,
19.9037615217948));
#203724=CARTESIAN_POINT('Ctrl Pts',(-18.4121028993987,21.3036650105896,
19.9064967342604));
#203725=CARTESIAN_POINT('Ctrl Pts',(-18.3782546071803,21.2981774216519,
19.9086023915845));
#203726=CARTESIAN_POINT('Ctrl Pts',(-18.2904310922278,21.2817408669927,
19.9141559958322));
#203727=CARTESIAN_POINT('Ctrl Pts',(-18.2367260743028,21.2695040533783,
19.917642313157));
#203728=CARTESIAN_POINT('Ctrl Pts',(-18.0779619707337,21.2267537357433,
19.9282103742442));
#203729=CARTESIAN_POINT('Ctrl Pts',(-17.9747307738845,21.1901805866374,
19.9354405137537));
#203730=CARTESIAN_POINT('Ctrl Pts',(-17.8336070264534,21.1275105133743,
19.9456407028877));
#203731=CARTESIAN_POINT('Ctrl Pts',(-17.7930121217363,21.1079085505382,
19.9486123189255));
#203732=CARTESIAN_POINT('Ctrl Pts',(-17.7315240442198,21.0757579661745,
19.9531457788603));
#203733=CARTESIAN_POINT('Ctrl Pts',(-17.7101701880462,21.0641197732191,
19.9547263472012));
#203734=CARTESIAN_POINT('Ctrl Pts',(-17.6764762065792,21.0449957732786,
19.9572253256428));
#203735=CARTESIAN_POINT('Ctrl Pts',(-17.664004201647,21.0377474042532,19.9581514497857));
#203736=CARTESIAN_POINT('Ctrl Pts',(-17.6196457580066,21.0113573810365,
19.961446908818));
#203737=CARTESIAN_POINT('Ctrl Pts',(-17.5881887951268,20.9915024986112,
19.9637868957674));
#203738=CARTESIAN_POINT('Ctrl Pts',(-17.5513117985625,20.9668442349921,
19.9665188397064));
#203739=CARTESIAN_POINT('Ctrl Pts',(-17.5453745339745,20.9628304325025,
19.9669583295065));
#203740=CARTESIAN_POINT('Ctrl Pts',(-17.5357261091608,20.9562361191214,
19.9676717902986));
#203741=CARTESIAN_POINT('Ctrl Pts',(-17.5320026849954,20.9536737745633,
19.9679469414648));
#203742=CARTESIAN_POINT('Ctrl Pts',(-17.5253558873047,20.9490682176025,
19.968437756491));
#203743=CARTESIAN_POINT('Ctrl Pts',(-17.5224294544831,20.9470295314428,
19.9686537211069));
#203744=CARTESIAN_POINT('Ctrl Pts',(-17.5161070028874,20.9426012502507,
19.9691200171473));
#203745=CARTESIAN_POINT('Ctrl Pts',(-17.5127128690109,20.940209063892,19.9693701674822));
#203746=CARTESIAN_POINT('Ctrl Pts',(-17.5032615164751,20.9335060399016,
19.9700663160942));
#203747=CARTESIAN_POINT('Ctrl Pts',(-17.497219866501,20.9291732093798,19.970510832222));
#203748=CARTESIAN_POINT('Ctrl Pts',(-17.4624537730576,20.9039619549484,
19.9730667204714));
#203749=CARTESIAN_POINT('Ctrl Pts',(-17.4342336170357,20.8823939310384,
19.9751333153187));
#203750=CARTESIAN_POINT('Ctrl Pts',(-17.3456225008949,20.8110680574318,
19.9816435231452));
#203751=CARTESIAN_POINT('Ctrl Pts',(-17.2874386481221,20.7586666397095,
19.9859522075909));
#203752=CARTESIAN_POINT('Ctrl Pts',(-17.0994165507255,20.569440708076,20.0005035983331));
#203753=CARTESIAN_POINT('Ctrl Pts',(-16.9850164731049,20.4185906179988,
20.0105710568498));
#203754=CARTESIAN_POINT('Ctrl Pts',(-16.8813488187142,20.2356209234951,
20.0228057707912));
#203755=CARTESIAN_POINT('Ctrl Pts',(-16.8708941611175,20.2164854635343,
20.0240842277369));
#203756=CARTESIAN_POINT('Ctrl Pts',(-16.8568190163854,20.1897498653763,
20.0258704203196));
#203757=CARTESIAN_POINT('Ctrl Pts',(-16.8529452524452,20.1822840870812,
20.0263691989217));
#203758=CARTESIAN_POINT('Ctrl Pts',(-16.8463547618638,20.1693951397965,
20.0272303673294));
#203759=CARTESIAN_POINT('Ctrl Pts',(-16.8436166441755,20.1639829777535,
20.027592000695));
#203760=CARTESIAN_POINT('Ctrl Pts',(-16.8380122020275,20.1527860420176,
20.0283402463647));
#203761=CARTESIAN_POINT('Ctrl Pts',(-16.8351490080665,20.1469997799148,
20.0287269633922));
#203762=CARTESIAN_POINT('Ctrl Pts',(-16.8285349301214,20.1334780611912,
20.0296308165883));
#203763=CARTESIAN_POINT('Ctrl Pts',(-16.8248046292708,20.1257327144509,
20.0301486628408));
#203764=CARTESIAN_POINT('Ctrl Pts',(-16.812964708747,20.1007611566909,20.031818719909));
#203765=CARTESIAN_POINT('Ctrl Pts',(-16.805040443855,20.0834485656936,20.0329773029342));
#203766=CARTESIAN_POINT('Ctrl Pts',(-16.7663465140776,19.9958067320823,
20.0388477162392));
#203767=CARTESIAN_POINT('Ctrl Pts',(-16.7391880485159,19.9239550022546,
20.0436805596129));
#203768=CARTESIAN_POINT('Ctrl Pts',(-16.6822908531277,19.7444926184962,
20.0557898003521));
#203769=CARTESIAN_POINT('Ctrl Pts',(-16.6570431131656,19.6357014647624,
20.0631697140928));
#203770=CARTESIAN_POINT('Ctrl Pts',(-16.6293970110739,19.4516347686704,
20.0754613631624));
#203771=CARTESIAN_POINT('Ctrl Pts',(-16.6222218536133,19.3772923795296,
20.0803704675103));
#203772=CARTESIAN_POINT('Ctrl Pts',(-16.6171535358165,19.2604232395742,
20.0878711166196));
#203773=CARTESIAN_POINT('Ctrl Pts',(-16.6165883462097,19.2180748651562,
20.0905441807989));
#203774=CARTESIAN_POINT('Ctrl Pts',(-16.6174179332694,19.1682807342008,
20.0936130481782));
#203775=CARTESIAN_POINT('Ctrl Pts',(-16.6175815007662,19.1608270915809,
20.0940704648653));
#203776=CARTESIAN_POINT('Ctrl Pts',(-16.6179098542651,19.1487688032113,
20.0948071204086));
#203777=CARTESIAN_POINT('Ctrl Pts',(-16.6180503012006,19.1441636340961,
20.0950876673628));
#203778=CARTESIAN_POINT('Ctrl Pts',(-16.6183264053844,19.1359865522908,
20.0955843708287));
#203779=CARTESIAN_POINT('Ctrl Pts',(-16.6184560758463,19.1324144928156,
20.0958008580551));
#203780=CARTESIAN_POINT('Ctrl Pts',(-16.6187536301728,19.1247529952551,
20.0962641244538));
#203781=CARTESIAN_POINT('Ctrl Pts',(-16.6189243255965,19.1206637221614,
20.0965107445366));
#203782=CARTESIAN_POINT('Ctrl Pts',(-16.6194263708169,19.1094191238481,
20.0971871832219));
#203783=CARTESIAN_POINT('Ctrl Pts',(-16.619782181935,19.102264868829,20.0976156530432));
#203784=CARTESIAN_POINT('Ctrl Pts',(-16.6218936123549,19.0637517105565,
20.0999126006471));
#203785=CARTESIAN_POINT('Ctrl Pts',(-16.6243107150034,19.0324312192418,
20.1017462509021));
#203786=CARTESIAN_POINT('Ctrl Pts',(-16.6436439148964,18.8383327301782,
20.1129599034163));
#203787=CARTESIAN_POINT('Ctrl Pts',(-16.6786921959594,18.6779038018545,
20.1216078327003));
#203788=CARTESIAN_POINT('Ctrl Pts',(-16.7699426851546,18.4123204300067,
20.1369798811944));
#203789=CARTESIAN_POINT('Ctrl Pts',(-16.8171287102505,18.3049043318235,
20.1435181531083));
#203790=CARTESIAN_POINT('Ctrl Pts',(-16.8797636682858,18.1893831726543,
20.1512164811181));
#203791=CARTESIAN_POINT('Ctrl Pts',(-16.8867037059908,18.1768869969954,
20.1520582216722));
#203792=CARTESIAN_POINT('Ctrl Pts',(-16.8979497820688,18.1571119135259,
20.1534051037197));
#203793=CARTESIAN_POINT('Ctrl Pts',(-16.9021738860903,18.1497867382985,
20.1539073019108));
#203794=CARTESIAN_POINT('Ctrl Pts',(-16.9097007604109,18.13691295632,20.1547957924554));
#203795=CARTESIAN_POINT('Ctrl Pts',(-16.9129852621242,18.1313537542417,
20.1551814183988));
#203796=CARTESIAN_POINT('Ctrl Pts',(-16.9198309274037,18.1198871945549,
20.1559809156624));
#203797=CARTESIAN_POINT('Ctrl Pts',(-16.9233956286274,18.1139820481023,
20.1563949131447));
#203798=CARTESIAN_POINT('Ctrl Pts',(-16.9326191540797,18.098870136136,20.157460265513));
#203799=CARTESIAN_POINT('Ctrl Pts',(-16.9383196809577,18.0896891728121,
20.1581131490353));
#203800=CARTESIAN_POINT('Ctrl Pts',(-16.9624000762208,18.0515611465621,
20.1608485144656));
#203801=CARTESIAN_POINT('Ctrl Pts',(-16.9814107292305,18.0230204644939,
20.1629543129613));
#203802=CARTESIAN_POINT('Ctrl Pts',(-17.0327382898508,17.9498773812034,
20.1685083796784));
#203803=CARTESIAN_POINT('Ctrl Pts',(-17.0661158288889,17.9060543159262,
20.1719950263878));
#203804=CARTESIAN_POINT('Ctrl Pts',(-17.1707700623992,17.7792311363261,
20.1825637171255));
#203805=CARTESIAN_POINT('Ctrl Pts',(-17.246805960605,17.7004039787809,20.1897941551204));
#203806=CARTESIAN_POINT('Ctrl Pts',(-17.4171986714331,17.5491443517543,
20.2048450423653));
#203807=CARTESIAN_POINT('Ctrl Pts',(-17.5122733757762,17.4780486079682,
20.2126374394778));
#203808=CARTESIAN_POINT('Ctrl Pts',(-17.6208857716582,17.4102344980526,
20.2205462053651));
#203809=CARTESIAN_POINT('Ctrl Pts',(-17.6289972541556,17.4052456928466,
20.2211311706908));
#203810=CARTESIAN_POINT('Ctrl Pts',(-17.6410646136959,17.3979356681566,
20.2219927084499));
#203811=CARTESIAN_POINT('Ctrl Pts',(-17.6449946851759,17.3955723767559,
20.2222719346882));
#203812=CARTESIAN_POINT('Ctrl Pts',(-17.6519998027772,17.3913908841978,
20.2227671848337));
#203813=CARTESIAN_POINT('Ctrl Pts',(-17.6550717964235,17.3895676808383,
20.2229835321382));
#203814=CARTESIAN_POINT('Ctrl Pts',(-17.6616852885319,17.3856652295397,
20.2234474857179));
#203815=CARTESIAN_POINT('Ctrl Pts',(-17.6652282160521,17.3835885139964,
20.2236949277196));
#203816=CARTESIAN_POINT('Ctrl Pts',(-17.6750217721551,17.3778861661999,
20.2243759439892));
#203817=CARTESIAN_POINT('Ctrl Pts',(-17.6812850229684,17.3742821677578,
20.2248081389945));
#203818=CARTESIAN_POINT('Ctrl Pts',(-17.7156527973087,17.3547398194418,
20.2271621837761));
#203819=CARTESIAN_POINT('Ctrl Pts',(-17.7441025606535,17.3394134538812,
20.229047125599));
#203820=CARTESIAN_POINT('Ctrl Pts',(-17.9180134275817,17.250800467562,20.2402567665192));
#203821=CARTESIAN_POINT('Ctrl Pts',(-18.0711964126083,17.1938436787367,
20.2488651981567));
#203822=CARTESIAN_POINT('Ctrl Pts',(-18.3429424056517,17.1271504400649,
20.2641830549628));
#203823=CARTESIAN_POINT('Ctrl Pts',(-18.4585725957482,17.1087418074613,
20.2707089322401));
#203824=CARTESIAN_POINT('Ctrl Pts',(-18.5893728266064,17.0988976800505,
20.2783933096479));
#203825=CARTESIAN_POINT('Ctrl Pts',(-18.6036336292863,17.0979695166197,
20.279234874441));
#203826=CARTESIAN_POINT('Ctrl Pts',(-18.6263447455836,17.0967221485764,
20.280581528103));
#203827=CARTESIAN_POINT('Ctrl Pts',(-18.6347896167472,17.0963090572107,
20.2810836752558));
#203828=CARTESIAN_POINT('Ctrl Pts',(-18.64968757838,17.0956697405005,20.2819721067216));
#203829=CARTESIAN_POINT('Ctrl Pts',(-18.6561396898981,17.0954224283003,
20.282357724913));
#203830=CARTESIAN_POINT('Ctrl Pts',(-18.6694869113169,17.0949719650697,
20.2831572367602));
#203831=CARTESIAN_POINT('Ctrl Pts',(-18.6763820769847,17.0947729903392,
20.2835712567292));
#203832=CARTESIAN_POINT('Ctrl Pts',(-18.6940833346544,17.0943487577032,
20.2846367315312));
#203833=CARTESIAN_POINT('Ctrl Pts',(-18.70489030412,17.0941725529676,20.2852897156728));
#203834=CARTESIAN_POINT('Ctrl Pts',(-18.7500000923134,17.0937825527587,
20.2880260518357));
#203835=CARTESIAN_POINT('Ctrl Pts',(-18.7843026335893,17.0943197807308,
20.290132741089));
#203836=CARTESIAN_POINT('Ctrl Pts',(-18.8736326308795,17.0978914215381,
20.2956897176309));
#203837=CARTESIAN_POINT('Ctrl Pts',(-18.9285787366785,17.1022412583556,
20.2991784334485));
#203838=CARTESIAN_POINT('Ctrl Pts',(-19.0871592007349,17.1210458663305,
20.309442931949));
#203839=CARTESIAN_POINT('Ctrl Pts',(-19.1899664820562,17.1410431983778,
20.3163493047314));
#203840=CARTESIAN_POINT('Ctrl Pts',(-19.4098671599444,17.2009983945365,
20.3314098294747));
#203841=CARTESIAN_POINT('Ctrl Pts',(-19.5258188950069,17.243785553549,20.339539024291));
#203842=CARTESIAN_POINT('Ctrl Pts',(-19.6459307954948,17.3004607260458,
20.3477410089447));
#203843=CARTESIAN_POINT('Ctrl Pts',(-19.6544402859681,17.3045457570014,
20.3483207756051));
#203844=CARTESIAN_POINT('Ctrl Pts',(-19.6670283912397,17.3106926825183,
20.3491761548535));
#203845=CARTESIAN_POINT('Ctrl Pts',(-19.6711279760125,17.3127110237867,
20.3494543675911));
#203846=CARTESIAN_POINT('Ctrl Pts',(-19.6784194657484,17.3163302073944,
20.3499485095131));
#203847=CARTESIAN_POINT('Ctrl Pts',(-19.6816138794697,17.3179258634747,
20.3501647564579));
#203848=CARTESIAN_POINT('Ctrl Pts',(-19.688409416523,17.3213418440018,20.3506242685243));
#203849=CARTESIAN_POINT('Ctrl Pts',(-19.6920093650211,17.3231643773795,
20.3508673923215));
#203850=CARTESIAN_POINT('Ctrl Pts',(-19.7018355054494,17.328174368415,20.3515302328636));
#203851=CARTESIAN_POINT('Ctrl Pts',(-19.7080512103204,17.331382441201,20.3519486756186));
#203852=CARTESIAN_POINT('Ctrl Pts',(-19.7219082459135,17.3386215838536,
20.3528798861944));
#203853=CARTESIAN_POINT('Ctrl Pts',(-19.72954107462,17.3426687633563,20.3533916941851));
#203854=CARTESIAN_POINT('Ctrl Pts',(-19.7529959856932,17.3552898877915,
20.3549616005021));
#203855=CARTESIAN_POINT('Ctrl Pts',(-19.7687340848304,17.3640191508954,
20.3560110062428));
#203856=CARTESIAN_POINT('Ctrl Pts',(-19.8288875693707,17.3983940185225,
20.3600139473651));
#203857=CARTESIAN_POINT('Ctrl Pts',(-19.8724793884733,17.4254511703355,
20.3628978631502));
#203858=CARTESIAN_POINT('Ctrl Pts',(-20.0283843359217,17.5302538040623,
20.373307393401));
#203859=CARTESIAN_POINT('Ctrl Pts',(-20.1340846186065,17.6172296022106,
20.3805736985629));
#203860=CARTESIAN_POINT('Ctrl Pts',(-20.3002739040948,17.7833585882957,
20.3935317161442));
#203861=CARTESIAN_POINT('Ctrl Pts',(-20.3649301418683,17.8576939485678,
20.3990753213143));
#203862=CARTESIAN_POINT('Ctrl Pts',(-20.4325720095384,17.9473796252565,
20.405659270609));
#203863=CARTESIAN_POINT('Ctrl Pts',(-20.4408556706767,17.958591508861,20.4064804514039));
#203864=CARTESIAN_POINT('Ctrl Pts',(-20.4539248241869,17.9766510340835,
20.4078005605493));
#203865=CARTESIAN_POINT('Ctrl Pts',(-20.4587816472569,17.9834467275316,
20.4082967280098));
#203866=CARTESIAN_POINT('Ctrl Pts',(-20.4673119315461,17.9955329171899,
20.4091782237183));
#203867=CARTESIAN_POINT('Ctrl Pts',(-20.4710017251783,18.0008117969722,
20.4095629192933));
#203868=CARTESIAN_POINT('Ctrl Pts',(-20.4786180326546,18.0118148171145,
20.4103641471899));
#203869=CARTESIAN_POINT('Ctrl Pts',(-20.4825405921835,18.017541589155,20.410780823781));
#203870=CARTESIAN_POINT('Ctrl Pts',(-20.4926091153895,18.0323973991309,
20.411860903163));
#203871=CARTESIAN_POINT('Ctrl Pts',(-20.4987121274749,18.0415551695413,
20.4125259168787));
#203872=CARTESIAN_POINT('Ctrl Pts',(-20.5245037155325,18.0809179587915,
20.415381281402));
#203873=CARTESIAN_POINT('Ctrl Pts',(-20.5434893668762,18.1115742610356,
20.4175975827553));
#203874=CARTESIAN_POINT('Ctrl Pts',(-20.5914726758973,18.1936655763423,
20.4235165806251));
#203875=CARTESIAN_POINT('Ctrl Pts',(-20.6191159820387,18.2458519230385,
20.4272642400987));
#203876=CARTESIAN_POINT('Ctrl Pts',(-20.7103286358132,18.4369579849455,
20.4409173756229));
#203877=CARTESIAN_POINT('Ctrl Pts',(-20.761004583689,18.5815065457925,20.4511535737685));
#203878=CARTESIAN_POINT('Ctrl Pts',(-20.8019773254567,18.7572088796499,
20.4629187575841));
#203879=CARTESIAN_POINT('Ctrl Pts',(-20.8077392299131,18.7843123994527,
20.464713888162));
#203880=CARTESIAN_POINT('Ctrl Pts',(-20.8211288701866,18.8539949184674,
20.4692668936239));
#203881=CARTESIAN_POINT('Ctrl Pts',(-20.8279872952478,18.8967113660204,
20.4719990528603));
#203882=CARTESIAN_POINT('Ctrl Pts',(-20.834494318318,18.9470513297185,20.4751272534771));
#203883=CARTESIAN_POINT('Ctrl Pts',(-20.8354165132923,18.9544967381812,
20.4755875809307));
#203884=CARTESIAN_POINT('Ctrl Pts',(-20.8368427998261,18.9665362684793,
20.4763279959977));
#203885=CARTESIAN_POINT('Ctrl Pts',(-20.8373714516943,18.9711273380694,
20.4766094130056));
#203886=CARTESIAN_POINT('Ctrl Pts',(-20.8382824844706,18.9792738422144,
20.4771070767456));
#203887=CARTESIAN_POINT('Ctrl Pts',(-20.8386708949005,18.9828285480352,
20.47732365902));
#203888=CARTESIAN_POINT('Ctrl Pts',(-20.8394063458069,18.9897210366878,
20.4777424893418));
#203889=CARTESIAN_POINT('Ctrl Pts',(-20.8397544550189,18.993058640691,20.4779447988319));
#203890=CARTESIAN_POINT('Ctrl Pts',(-20.8405037123441,19.0004117879156,
20.4783894290261));
#203891=CARTESIAN_POINT('Ctrl Pts',(-20.8409013186364,19.0044276898395,
20.478631552258));
#203892=CARTESIAN_POINT('Ctrl Pts',(-20.8418560175519,19.0143599179749,
20.4792286755137));
#203893=CARTESIAN_POINT('Ctrl Pts',(-20.8423996911825,19.0202775401958,
20.4795829495));
#203894=CARTESIAN_POINT('Ctrl Pts',(-20.8445839025751,19.0452031904335,
20.4810692025915));
#203895=CARTESIAN_POINT('Ctrl Pts',(-20.8459924232064,19.064231299655,20.4821891524991));
#203896=CARTESIAN_POINT('Ctrl Pts',(-20.849686309312,19.125345466913,20.485746622392));
#203897=CARTESIAN_POINT('Ctrl Pts',(-20.8509723412172,19.1674831001617,
20.48813942538));
#203898=CARTESIAN_POINT('Ctrl Pts',(-20.8509995586411,19.2096329911406,
20.4904972704014));
#203899=CARTESIAN_POINT('Ctrl Pts',(-20.7225806064498,19.9371103026755,
20.5336910513061));
#203900=CARTESIAN_POINT('Ctrl Pts',(-20.7472974864126,19.8694187853333,
20.5293719591642));
#203901=CARTESIAN_POINT('Ctrl Pts',(-20.7685453196057,19.800487370849,20.5250528670223));
#203902=CARTESIAN_POINT('Ctrl Pts',(-20.7862158025195,19.7307107848498,
20.5207337748803));
#203903=CARTESIAN_POINT('Ctrl Pts',(-20.8038940120027,19.660903688443,20.5164127941785));
#203904=CARTESIAN_POINT('Ctrl Pts',(-20.8179916608039,19.5902511717225,
20.5120918134767));
#203905=CARTESIAN_POINT('Ctrl Pts',(-20.8284516779761,19.5191577008985,
20.5077708327749));
#203906=CARTESIAN_POINT('Ctrl Pts',(-20.8389271851641,19.4479589492739,
20.5034434532251));
#203907=CARTESIAN_POINT('Ctrl Pts',(-20.8457542653409,19.3763184341297,
20.4991160736754));
#203908=CARTESIAN_POINT('Ctrl Pts',(-20.8489278371988,19.3046442387004,
20.4947886941257));
#203909=CARTESIAN_POINT('Ctrl Pts',(-20.8503291649484,19.2729956599096,
20.4928778891028));
#203910=CARTESIAN_POINT('Ctrl Pts',(-20.8510188273247,19.2413404929336,
20.4909670840799));
#203911=CARTESIAN_POINT('Ctrl Pts',(-20.8509996091577,19.2097135994841,
20.489056279057));
#203912=CARTESIAN_POINT('Origin',(-18.734,19.211,0.));
#203913=CARTESIAN_POINT('',(-20.7225806064499,19.9371103026755,21.5555703710623));
#203914=CARTESIAN_POINT('',(-20.7225806064498,19.9371103026755,21.3335535417785));
#203915=CARTESIAN_POINT('',(-20.7225806064498,19.9371103026755,0.));
#203916=CARTESIAN_POINT('',(-20.8509993841528,19.2093852254739,21.5109437210328));
#203917=CARTESIAN_POINT('Ctrl Pts',(-20.8509993841528,19.2093852254739,
21.5109437210328));
#203918=CARTESIAN_POINT('Ctrl Pts',(-20.8510540319531,19.2810295063139,
21.515267181414));
#203919=CARTESIAN_POINT('Ctrl Pts',(-20.8474675450903,19.3528083048161,
21.5195906417951));
#203920=CARTESIAN_POINT('Ctrl Pts',(-20.8402254623162,19.4243150296886,
21.5239141021763));
#203921=CARTESIAN_POINT('Ctrl Pts',(-20.8329909780013,19.4957467290533,
21.5282330263434));
#203922=CARTESIAN_POINT('Ctrl Pts',(-20.8221085494476,19.5669064297487,
21.5325519505105));
#203923=CARTESIAN_POINT('Ctrl Pts',(-20.8076157375584,19.6373880544179,
21.5368708746776));
#203924=CARTESIAN_POINT('Ctrl Pts',(-20.7931333528068,19.7078189697004,
21.54118669151));
#203925=CARTESIAN_POINT('Ctrl Pts',(-20.7750458366717,19.7775722915727,
21.5455025083425));
#203926=CARTESIAN_POINT('Ctrl Pts',(-20.7534422764442,19.8462494723413,
21.5498183251749));
#203927=CARTESIAN_POINT('Ctrl Pts',(-20.74384465954,19.8767600578253,21.551735673804));
#203928=CARTESIAN_POINT('Ctrl Pts',(-20.7335537650588,19.9070583803701,
21.5536530224332));
#203929=CARTESIAN_POINT('Ctrl Pts',(-20.7225806064499,19.9371103026755,
21.5555703710623));
#203930=CARTESIAN_POINT('Ctrl Pts',(-20.8509994310935,19.209447985236,21.5099894778226));
#203931=CARTESIAN_POINT('Ctrl Pts',(-20.8509485247462,19.1400100451657,
21.5054226012226));
#203932=CARTESIAN_POINT('Ctrl Pts',(-20.8474812625977,19.070609682484,21.5009009210634));
#203933=CARTESIAN_POINT('Ctrl Pts',(-20.8382974076878,18.9782625879113,
21.4950376552809));
#203934=CARTESIAN_POINT('Ctrl Pts',(-20.8356021208678,18.955064636439,21.4935779570289));
#203935=CARTESIAN_POINT('Ctrl Pts',(-20.8317146611693,18.9258336681481,
21.4917592268508));
#203936=CARTESIAN_POINT('Ctrl Pts',(-20.8308794579723,18.9197558115299,
21.4913821951208));
#203937=CARTESIAN_POINT('Ctrl Pts',(-20.8294395976148,18.9096051687547,
21.4907544964862));
#203938=CARTESIAN_POINT('Ctrl Pts',(-20.8288494645369,18.9055304055484,
21.490503054755));
#203939=CARTESIAN_POINT('Ctrl Pts',(-20.8277537217301,18.8981170278529,
21.4900466025938));
#203940=CARTESIAN_POINT('Ctrl Pts',(-20.8272520064267,18.8947778637144,
21.4898413773219));
#203941=CARTESIAN_POINT('Ctrl Pts',(-20.8262053651731,18.8879235964327,
21.4894208972805));
#203942=CARTESIAN_POINT('Ctrl Pts',(-20.8256595713239,18.8844086792437,
21.4892056988165));
#203943=CARTESIAN_POINT('Ctrl Pts',(-20.8244066210198,18.8764716559245,
21.4887207236645));
#203944=CARTESIAN_POINT('Ctrl Pts',(-20.8236942930991,18.872050421987,21.4884512443155));
#203945=CARTESIAN_POINT('Ctrl Pts',(-20.8214988526174,18.8586939146337,
21.487639087692));
#203946=CARTESIAN_POINT('Ctrl Pts',(-20.8199723987706,18.8497657329395,
21.4870988243196));
#203947=CARTESIAN_POINT('Ctrl Pts',(-20.8078162681548,18.7813126038274,
21.4829748366242));
#203948=CARTESIAN_POINT('Ctrl Pts',(-20.7946969717277,18.7222520052379,
21.4795225738979));
#203949=CARTESIAN_POINT('Ctrl Pts',(-20.7741789047046,18.6455652344342,
21.4750848284973));
#203950=CARTESIAN_POINT('Ctrl Pts',(-20.769047825688,18.6273675720153,21.4740351573819));
#203951=CARTESIAN_POINT('Ctrl Pts',(-20.7520373438111,18.5699929222378,
21.4707297776502));
#203952=CARTESIAN_POINT('Ctrl Pts',(-20.7392648735595,18.5310899039518,
21.4684945105134));
#203953=CARTESIAN_POINT('Ctrl Pts',(-20.7134212063805,18.4594543385383,
21.4643518162005));
#203954=CARTESIAN_POINT('Ctrl Pts',(-20.7006455075783,18.426631045212,21.4624429242906));
#203955=CARTESIAN_POINT('Ctrl Pts',(-20.6589745566515,18.3269984218837,
21.456579322497));
#203956=CARTESIAN_POINT('Ctrl Pts',(-20.6274493266644,18.2613501573964,
21.4526165474976));
#203957=CARTESIAN_POINT('Ctrl Pts',(-20.5661683690656,18.1489747119488,
21.4455035834002));
#203958=CARTESIAN_POINT('Ctrl Pts',(-20.5378440241279,18.1015475542015,
21.4423912149869));
#203959=CARTESIAN_POINT('Ctrl Pts',(-20.4889707173757,18.0265407422782,
21.437242441228));
#203960=CARTESIAN_POINT('Ctrl Pts',(-20.46954686055,17.9982581275559,21.4352459080517));
#203961=CARTESIAN_POINT('Ctrl Pts',(-20.4431388058229,17.9617404747413,
21.4325885652031));
#203962=CARTESIAN_POINT('Ctrl Pts',(-20.4367661202885,17.9530682243842,
21.4319514493151));
#203963=CARTESIAN_POINT('Ctrl Pts',(-20.4262258339138,17.9389513638011,
21.4309042074722));
#203964=CARTESIAN_POINT('Ctrl Pts',(-20.4220973657203,17.9334776761409,
21.4304956227199));
#203965=CARTESIAN_POINT('Ctrl Pts',(-20.4140585606519,17.9229265147463,
21.4297030757405));
#203966=CARTESIAN_POINT('Ctrl Pts',(-20.410151609093,17.9178465471731,21.4293192505649));
#203967=CARTESIAN_POINT('Ctrl Pts',(-20.401083684171,17.9061662213702,21.4284314840878));
#203968=CARTESIAN_POINT('Ctrl Pts',(-20.3959064983369,17.8995786384633,
21.4279268969342));
#203969=CARTESIAN_POINT('Ctrl Pts',(-20.3818932538587,17.8819640741492,
21.4265670672812));
#203970=CARTESIAN_POINT('Ctrl Pts',(-20.3729857877455,17.8709946863608,
21.4257089485314));
#203971=CARTESIAN_POINT('Ctrl Pts',(-20.2682893331065,17.7446685562268,
21.4156928918964));
#203972=CARTESIAN_POINT('Ctrl Pts',(-20.1606339789355,17.6397358276293,
21.4060184879308));
#203973=CARTESIAN_POINT('Ctrl Pts',(-19.9681106254966,17.4882998852229,
21.3898622740542));
#203974=CARTESIAN_POINT('Ctrl Pts',(-19.8895235800659,17.4346299533531,
21.3835371506906));
#203975=CARTESIAN_POINT('Ctrl Pts',(-19.7687994158836,17.3635949698684,
21.3744153798713));
#203976=CARTESIAN_POINT('Ctrl Pts',(-19.7292832156593,17.3420090901545,
21.3715175443189));
#203977=CARTESIAN_POINT('Ctrl Pts',(-19.6670844694445,17.3105655023594,
21.3671223254294));
#203978=CARTESIAN_POINT('Ctrl Pts',(-19.6448684014709,17.2998179609983,
21.3655841816557));
#203979=CARTESIAN_POINT('Ctrl Pts',(-19.6165123943238,17.2867069007583,
21.3636654869528));
#203980=CARTESIAN_POINT('Ctrl Pts',(-19.6105435276297,17.2839806683043,
21.3632640753004));
#203981=CARTESIAN_POINT('Ctrl Pts',(-19.6014998841082,17.2799007700546,
21.3626597155254));
#203982=CARTESIAN_POINT('Ctrl Pts',(-19.5984344687366,17.2785266277516,
21.3624555260014));
#203983=CARTESIAN_POINT('Ctrl Pts',(-19.5921228733737,17.2757153343784,
21.3620364884064));
#203984=CARTESIAN_POINT('Ctrl Pts',(-19.588876396879,17.2742790730183,21.3618217028377));
#203985=CARTESIAN_POINT('Ctrl Pts',(-19.581585452878,17.2710754188185,21.3613410032991));
#203986=CARTESIAN_POINT('Ctrl Pts',(-19.5775390665966,17.2693125059526,
21.3610753655008));
#203987=CARTESIAN_POINT('Ctrl Pts',(-19.5672278349354,17.2648584674879,
21.3604012884986));
#203988=CARTESIAN_POINT('Ctrl Pts',(-19.5609553935305,17.2621849062964,
21.3599938957968));
#203989=CARTESIAN_POINT('Ctrl Pts',(-19.5252603478117,17.2471736430602,
21.3576899717216));
#203990=CARTESIAN_POINT('Ctrl Pts',(-19.4955730149619,17.2354712891341,
21.3558294172624));
#203991=CARTESIAN_POINT('Ctrl Pts',(-19.2794566073922,17.1558775630741,
21.3426052583473));
#203992=CARTESIAN_POINT('Ctrl Pts',(-19.0845512124342,17.1138151352113,
21.3322947409037));
#203993=CARTESIAN_POINT('Ctrl Pts',(-18.8308756325093,17.0954793164923,
21.3181606736389));
#203994=CARTESIAN_POINT('Ctrl Pts',(-18.7749971763512,17.0936594007002,
21.3150108109257));
#203995=CARTESIAN_POINT('Ctrl Pts',(-18.6844317030418,17.0942962020247,
21.3098016555587));
#203996=CARTESIAN_POINT('Ctrl Pts',(-18.6497613107883,17.0953923745127,
21.3077829610819));
#203997=CARTESIAN_POINT('Ctrl Pts',(-18.6042833866856,17.0979498994386,
21.3050967049045));
#203998=CARTESIAN_POINT('Ctrl Pts',(-18.593436913348,17.0986436997351,21.3044531783053));
#203999=CARTESIAN_POINT('Ctrl Pts',(-18.5756915912462,17.0999160676557,
21.3033954832749));
#204000=CARTESIAN_POINT('Ctrl Pts',(-18.5687893026128,17.1004450148345,
21.3029828742043));
#204001=CARTESIAN_POINT('Ctrl Pts',(-18.5554410671539,17.1015338186446,
21.3021825566981));
#204002=CARTESIAN_POINT('Ctrl Pts',(-18.5489948411741,17.1020893919963,
21.3017949870326));
#204003=CARTESIAN_POINT('Ctrl Pts',(-18.5341273125988,17.1034394533369,
21.3008985760075));
#204004=CARTESIAN_POINT('Ctrl Pts',(-18.5257080644039,17.1042548765098,
21.3003890824661));
#204005=CARTESIAN_POINT('Ctrl Pts',(-18.5031016628748,17.1065811933053,
21.2990159238409));
#204006=CARTESIAN_POINT('Ctrl Pts',(-18.4889247100316,17.1081850669386,
21.2981493541523));
#204007=CARTESIAN_POINT('Ctrl Pts',(-18.3611864329124,17.1239457148605,
21.2902910156079));
#204008=CARTESIAN_POINT('Ctrl Pts',(-18.2489491712357,17.1471434355782,
21.2830112441605));
#204009=CARTESIAN_POINT('Ctrl Pts',(-17.9820760906419,17.2252792964654,
21.2648705845793));
#204010=CARTESIAN_POINT('Ctrl Pts',(-17.8308695830361,17.2893258808947,
21.2538531237831));
#204011=CARTESIAN_POINT('Ctrl Pts',(-17.6600546573147,17.3863344394032,
21.2413709737737));
#204012=CARTESIAN_POINT('Ctrl Pts',(-17.6319353162539,17.4031790152025,
21.2393169273819));
#204013=CARTESIAN_POINT('Ctrl Pts',(-17.5980619654777,17.4245547172719,
21.2368539684987));
#204014=CARTESIAN_POINT('Ctrl Pts',(-17.5919271522271,17.4284704545616,
21.2364083701365));
#204015=CARTESIAN_POINT('Ctrl Pts',(-17.5823438714907,17.4346570692357,
21.2357131842111));
#204016=CARTESIAN_POINT('Ctrl Pts',(-17.5788817137874,17.4369064873755,
21.2354622172765));
#204017=CARTESIAN_POINT('Ctrl Pts',(-17.5724291994517,17.4411256832554,
21.2349948599569));
#204018=CARTESIAN_POINT('Ctrl Pts',(-17.5694372856936,17.4430929021827,
21.2347783105817));
#204019=CARTESIAN_POINT('Ctrl Pts',(-17.5626240950573,17.4475974570067,
21.2342855277546));
#204020=CARTESIAN_POINT('Ctrl Pts',(-17.5588060739463,17.4501396204159,
21.2340096221169));
#204021=CARTESIAN_POINT('Ctrl Pts',(-17.547098897815,17.4579896792205,21.2331642649505));
#204022=CARTESIAN_POINT('Ctrl Pts',(-17.5392370913703,17.4633384163671,
21.2325974878786));
#204023=CARTESIAN_POINT('Ctrl Pts',(-17.4690435160698,17.5117892757753,
21.2275427144372));
#204024=CARTESIAN_POINT('Ctrl Pts',(-17.4090248231839,17.5581614228085,
21.2232601553324));
#204025=CARTESIAN_POINT('Ctrl Pts',(-17.2444327716054,17.7000708042158,
21.2112299033746));
#204026=CARTESIAN_POINT('Ctrl Pts',(-17.1467844093052,17.802999092525,21.2037070623203));
#204027=CARTESIAN_POINT('Ctrl Pts',(-17.0222853102931,17.9637855823246,
21.1924562586107));
#204028=CARTESIAN_POINT('Ctrl Pts',(-16.9865976089396,18.014298279497,21.1889869012016));
#204029=CARTESIAN_POINT('Ctrl Pts',(-16.9330234364155,18.0976442436342,
21.1833006497682));
#204030=CARTESIAN_POINT('Ctrl Pts',(-16.913706115801,18.1295160434126,21.1811349016532));
#204031=CARTESIAN_POINT('Ctrl Pts',(-16.8897206261323,18.1715546343917,
21.1782817610181));
#204032=CARTESIAN_POINT('Ctrl Pts',(-16.8842770147697,18.1812728770676,
21.1776224368546));
#204033=CARTESIAN_POINT('Ctrl Pts',(-16.8755507543703,18.197143981157,21.1765458845813));
#204034=CARTESIAN_POINT('Ctrl Pts',(-16.8722213227779,18.2032709784969,
21.1761303343307));
#204035=CARTESIAN_POINT('Ctrl Pts',(-16.8658780886553,18.2150828726806,
21.1753292636372));
#204036=CARTESIAN_POINT('Ctrl Pts',(-16.8628598094832,18.2207652873432,
21.1749439080694));
#204037=CARTESIAN_POINT('Ctrl Pts',(-16.8560100733578,18.233804199237,21.1740596714827));
#204038=CARTESIAN_POINT('Ctrl Pts',(-16.8521958700176,18.2411695968248,
21.1735601876388));
#204039=CARTESIAN_POINT('Ctrl Pts',(-16.8421815755563,18.2607891535973,
21.1722296015074));
#204040=CARTESIAN_POINT('Ctrl Pts',(-16.8360573534164,18.2730814001101,
21.171395856851));
#204041=CARTESIAN_POINT('Ctrl Pts',(-16.7905178052886,18.3667588896692,
21.1650403450218));
#204042=CARTESIAN_POINT('Ctrl Pts',(-16.756238845878,18.4505243796976,21.1593417238349));
#204043=CARTESIAN_POINT('Ctrl Pts',(-16.6828169397694,18.6688559318926,
21.1444680071484));
#204044=CARTESIAN_POINT('Ctrl Pts',(-16.6514754114365,18.8055884718426,
21.1351165692679));
#204045=CARTESIAN_POINT('Ctrl Pts',(-16.6269181785219,18.9990359132272,
21.1223457036317));
#204046=CARTESIAN_POINT('Ctrl Pts',(-16.6221164443191,19.0539291383938,
21.118776421195));
#204047=CARTESIAN_POINT('Ctrl Pts',(-16.618091467603,19.1373295991591,21.1134917535915));
#204048=CARTESIAN_POINT('Ctrl Pts',(-16.6172932400701,19.1657349844734,
21.1117161606127));
#204049=CARTESIAN_POINT('Ctrl Pts',(-16.6170118442327,19.2010865739133,
21.1095435945588));
#204050=CARTESIAN_POINT('Ctrl Pts',(-16.6169907239664,19.2080241064856,
21.1091190261783));
#204051=CARTESIAN_POINT('Ctrl Pts',(-16.6170112722203,19.219004310664,21.1084500090418));
#204052=CARTESIAN_POINT('Ctrl Pts',(-16.6170304170123,19.2230469030434,
21.1082043308985));
#204053=CARTESIAN_POINT('Ctrl Pts',(-16.6170883600609,19.2306706474873,
21.1077422458833));
#204054=CARTESIAN_POINT('Ctrl Pts',(-16.6171246650422,19.2342517121927,
21.1075257080974));
#204055=CARTESIAN_POINT('Ctrl Pts',(-16.6172284509331,19.2424393599015,
21.107031779873));
#204056=CARTESIAN_POINT('Ctrl Pts',(-16.6173018816797,19.2470458195799,
21.1067547253964));
#204057=CARTESIAN_POINT('Ctrl Pts',(-16.6175368076541,19.2592775902263,
21.1060211791791));
#204058=CARTESIAN_POINT('Ctrl Pts',(-16.6177244757066,19.2669024106611,
21.1055661136631));
#204059=CARTESIAN_POINT('Ctrl Pts',(-16.6193295724009,19.3203679187707,
21.1023895689404));
#204060=CARTESIAN_POINT('Ctrl Pts',(-16.6221952109507,19.3661565922118,
21.0997432654898));
#204061=CARTESIAN_POINT('Ctrl Pts',(-16.6301239875518,19.4493632914149,
21.095011849846));
#204062=CARTESIAN_POINT('Ctrl Pts',(-16.6347043021177,19.4868063418828,
21.0929114942282));
#204063=CARTESIAN_POINT('Ctrl Pts',(-16.6596407163324,19.6535530483251,
21.0836113186086));
#204064=CARTESIAN_POINT('Ctrl Pts',(-16.6909611652801,19.7809240601643,
21.0766339409727));
#204065=CARTESIAN_POINT('Ctrl Pts',(-16.7627858596949,19.9880502685771,
21.0645332885749));
#204066=CARTESIAN_POINT('Ctrl Pts',(-16.7969196931691,20.0696091230245,
21.0595612073858));
#204067=CARTESIAN_POINT('Ctrl Pts',(-16.8451366468308,20.1671932288146,
21.0532176403441));
#204068=CARTESIAN_POINT('Ctrl Pts',(-16.8544955238402,20.1854604343622,
21.0520126238853));
#204069=CARTESIAN_POINT('Ctrl Pts',(-16.8682706978211,20.2114107181779,
21.0502742766851));
#204070=CARTESIAN_POINT('Ctrl Pts',(-16.8724721084835,20.2192069924006,
21.049748550832));
#204071=CARTESIAN_POINT('Ctrl Pts',(-16.8798389788427,20.2326741573723,
21.0488342821788));
#204072=CARTESIAN_POINT('Ctrl Pts',(-16.8829818648119,20.2383573078415,
21.0484465497055));
#204073=CARTESIAN_POINT('Ctrl Pts',(-16.8890741224098,20.2492549761701,
21.0476993358038));
#204074=CARTESIAN_POINT('Ctrl Pts',(-16.8920195799181,20.2544716192744,
21.0473399979043));
#204075=CARTESIAN_POINT('Ctrl Pts',(-16.8997915044371,20.2681008756961,
21.0463968010359));
#204076=CARTESIAN_POINT('Ctrl Pts',(-16.9046536700514,20.2764928750558,
21.0458116546712));
#204077=CARTESIAN_POINT('Ctrl Pts',(-16.9217170000874,20.3054827383888,
21.0437748245424));
#204078=CARTESIAN_POINT('Ctrl Pts',(-16.9342094177044,20.3259062392807,
21.0423125676579));
#204079=CARTESIAN_POINT('Ctrl Pts',(-17.0303110731261,20.4771945641552,
21.0312703117044));
#204080=CARTESIAN_POINT('Ctrl Pts',(-17.1277324331254,20.5986932536174,
21.0211541474364));
#204081=CARTESIAN_POINT('Ctrl Pts',(-17.2901177526393,20.7609737751704,
21.0059872620563));
#204082=CARTESIAN_POINT('Ctrl Pts',(-17.3454296123493,20.8107148113477,
21.0010640328941));
#204083=CARTESIAN_POINT('Ctrl Pts',(-17.4390019262775,20.8863455978038,
20.9932277997709));
#204084=CARTESIAN_POINT('Ctrl Pts',(-17.4756938277581,20.9140763357967,
20.9902669931262));
#204085=CARTESIAN_POINT('Ctrl Pts',(-17.5269183518952,20.9502303746368,
20.9863123308879));
#204086=CARTESIAN_POINT('Ctrl Pts',(-17.5406889084463,20.9597072587755,
20.9852661645677));
#204087=CARTESIAN_POINT('Ctrl Pts',(-17.5644673557033,20.9756598597418,
20.9834904517178));
#204088=CARTESIAN_POINT('Ctrl Pts',(-17.5744201527961,20.9822158591289,
20.9827562590566));
#204089=CARTESIAN_POINT('Ctrl Pts',(-17.5886443071773,20.9914141506185,
20.9817203841181));
#204090=CARTESIAN_POINT('Ctrl Pts',(-17.592870309317,20.9941256941223,20.9814142901151));
#204091=CARTESIAN_POINT('Ctrl Pts',(-17.6001689555432,20.9987721742109,
20.9808885589087));
#204092=CARTESIAN_POINT('Ctrl Pts',(-17.6032369892324,21.00071427846,20.9806684486337));
#204093=CARTESIAN_POINT('Ctrl Pts',(-17.6091968772973,21.0044655197048,
20.9802425986785));
#204094=CARTESIAN_POINT('Ctrl Pts',(-17.6120881041877,21.0062755592464,
20.9800367960242));
#204095=CARTESIAN_POINT('Ctrl Pts',(-17.6198977606497,21.011138525541,20.9794829645837));
#204096=CARTESIAN_POINT('Ctrl Pts',(-17.6248244002329,21.0141783055303,
20.9791357969227));
#204097=CARTESIAN_POINT('Ctrl Pts',(-17.6431400771674,21.025375771212,20.9778530778109));
#204098=CARTESIAN_POINT('Ctrl Pts',(-17.6566075193382,21.0334050827068,
20.9769255641445));
#204099=CARTESIAN_POINT('Ctrl Pts',(-17.7862406194556,21.1087531812253,
20.9681341967482));
#204100=CARTESIAN_POINT('Ctrl Pts',(-17.9084898030845,21.1650362866008,
20.9608716366963));
#204101=CARTESIAN_POINT('Ctrl Pts',(-18.1869543705648,21.2624029526393,
20.9448518903304));
#204102=CARTESIAN_POINT('Ctrl Pts',(-18.3441712705311,21.2979926668626,
20.9361045578553));
#204103=CARTESIAN_POINT('Ctrl Pts',(-18.5224425239592,21.3174853802441,
20.9256316224447));
#204104=CARTESIAN_POINT('Ctrl Pts',(-18.5410182405574,21.3192683013261,
20.9245344989187));
#204105=CARTESIAN_POINT('Ctrl Pts',(-18.5681149671023,21.3215079731011,
20.922924673644));
#204106=CARTESIAN_POINT('Ctrl Pts',(-18.5766193347084,21.3221591772313,
20.9224180773337));
#204107=CARTESIAN_POINT('Ctrl Pts',(-18.5915588554365,21.323212368742,20.9215256888576));
#204108=CARTESIAN_POINT('Ctrl Pts',(-18.5979923812902,21.323636385317,20.9211405933602));
#204109=CARTESIAN_POINT('Ctrl Pts',(-18.6105049471416,21.3244036632546,
20.9203900295935));
#204110=CARTESIAN_POINT('Ctrl Pts',(-18.6165837343203,21.3247501014283,
20.920024665026));
#204111=CARTESIAN_POINT('Ctrl Pts',(-18.6311455225416,21.3255169883941,
20.9191476478695));
#204112=CARTESIAN_POINT('Ctrl Pts',(-18.6396296753501,21.3259126167004,
20.918635221551));
#204113=CARTESIAN_POINT('Ctrl Pts',(-18.6704140468053,21.3271625302186,
20.9167705223329));
#204114=CARTESIAN_POINT('Ctrl Pts',(-18.6927244282053,21.3277152135136,
20.9154088546442));
#204115=CARTESIAN_POINT('Ctrl Pts',(-18.8983629617634,21.3295571239853,
20.9027594275979));
#204116=CARTESIAN_POINT('Ctrl Pts',(-19.0810913454143,21.3073779395509,
20.8906948008643));
#204117=CARTESIAN_POINT('Ctrl Pts',(-19.3376246637083,21.2417570241417,
20.8732107339467));
#204118=CARTESIAN_POINT('Ctrl Pts',(-19.4153876737813,21.217003345286,20.8678506049209));
#204119=CARTESIAN_POINT('Ctrl Pts',(-19.5255260965356,21.1747975052296,
20.8603296642829));
#204120=CARTESIAN_POINT('Ctrl Pts',(-19.5591797901394,21.1608956088291,
20.8580420257412));
#204121=CARTESIAN_POINT('Ctrl Pts',(-19.5993086988834,21.1430936790258,
20.8553410773665));
#204122=CARTESIAN_POINT('Ctrl Pts',(-19.6061409439404,21.1400192603111,
20.8548821771412));
#204123=CARTESIAN_POINT('Ctrl Pts',(-19.6167472360498,21.1351787018984,
20.8541714431051));
#204124=CARTESIAN_POINT('Ctrl Pts',(-19.6205325546415,21.1334376166326,
20.853918116734));
#204125=CARTESIAN_POINT('Ctrl Pts',(-19.6275486861944,21.1301853653737,
20.8534492210959));
#204126=CARTESIAN_POINT('Ctrl Pts',(-19.6307807916059,21.1286772234568,
20.8532334758975));
#204127=CARTESIAN_POINT('Ctrl Pts',(-19.6380869386121,21.1252455705182,
20.852746362086));
#204128=CARTESIAN_POINT('Ctrl Pts',(-19.6421586496785,21.1233172238658,
20.8524752965508));
#204129=CARTESIAN_POINT('Ctrl Pts',(-19.6544483063059,21.1174487858528,
20.851658265905));
#204130=CARTESIAN_POINT('Ctrl Pts',(-19.6626471178375,21.1134685529421,
20.8511147275499));
#204131=CARTESIAN_POINT('Ctrl Pts',(-19.7255937342003,21.0824063123546,
20.8469515638468));
#204132=CARTESIAN_POINT('Ctrl Pts',(-19.7791774679564,21.053016625207,20.8434651113395));
#204133=CARTESIAN_POINT('Ctrl Pts',(-19.970858594242,20.9368208952867,20.830935854194));
#204134=CARTESIAN_POINT('Ctrl Pts',(-20.1000689129344,20.8364655914837,
20.822334830644));
#204135=CARTESIAN_POINT('Ctrl Pts',(-20.273107884421,20.6667223149079,20.8088862894272));
#204136=CARTESIAN_POINT('Ctrl Pts',(-20.326559848166,20.6080439164103,20.8043989788281));
#204137=CARTESIAN_POINT('Ctrl Pts',(-20.3888156628394,20.5314732708347,
20.7986403352534));
#204138=CARTESIAN_POINT('Ctrl Pts',(-20.4008334149378,20.516270419079,20.7975016064567));
#204139=CARTESIAN_POINT('Ctrl Pts',(-20.4179162143748,20.4940394201979,
20.7958420496877));
#204140=CARTESIAN_POINT('Ctrl Pts',(-20.4231497182485,20.4871415269321,
20.7953278842124));
#204141=CARTESIAN_POINT('Ctrl Pts',(-20.4322172523282,20.4750367765264,
20.7944268409866));
#204142=CARTESIAN_POINT('Ctrl Pts',(-20.4360700412672,20.4698440656832,
20.794040704147));
#204143=CARTESIAN_POINT('Ctrl Pts',(-20.44348071136,20.4597598975513,20.7932915529837));
#204144=CARTESIAN_POINT('Ctrl Pts',(-20.4470415409671,20.4548706773554,
20.7929286584954));
#204145=CARTESIAN_POINT('Ctrl Pts',(-20.4554657132141,20.4431990307194,
20.7920630847887));
#204146=CARTESIAN_POINT('Ctrl Pts',(-20.4603099695392,20.436403010861,20.7915596757553));
#204147=CARTESIAN_POINT('Ctrl Pts',(-20.47743454376,20.4120758252375,20.7897596208191));
#204148=CARTESIAN_POINT('Ctrl Pts',(-20.4894886989085,20.3943877308616,
20.7884543995981));
#204149=CARTESIAN_POINT('Ctrl Pts',(-20.5919348107623,20.239049248216,20.7770190655048));
#204150=CARTESIAN_POINT('Ctrl Pts',(-20.666182344048,20.0915668540658,20.7662793195637));
#204151=CARTESIAN_POINT('Ctrl Pts',(-20.7225806115197,19.937110288791,20.7554137119617));
#204152=CARTESIAN_POINT('',(-20.8509997094729,19.2098909049546,21.2890562789773));
#204153=CARTESIAN_POINT('Ctrl Pts',(-20.8509997094729,19.2098909049547,
21.2890562789773));
#204154=CARTESIAN_POINT('Ctrl Pts',(-20.8509573536458,19.1290436646228,
21.2842160160334));
#204155=CARTESIAN_POINT('Ctrl Pts',(-20.8462795755055,19.0483584782395,
21.2793757530895));
#204156=CARTESIAN_POINT('Ctrl Pts',(-20.837046582522,18.9683395958493,21.2745354901457));
#204157=CARTESIAN_POINT('Ctrl Pts',(-20.8277795400084,18.8880256189704,
21.2696773772284));
#204158=CARTESIAN_POINT('Ctrl Pts',(-20.8139237586678,18.8083831470337,
21.2648192643112));
#204159=CARTESIAN_POINT('Ctrl Pts',(-20.795610244073,18.7299052052522,21.259961151394));
#204160=CARTESIAN_POINT('Ctrl Pts',(-20.7772066847249,18.6510413994209,
21.2550791518778));
#204161=CARTESIAN_POINT('Ctrl Pts',(-20.7543015879878,18.5733538729021,
21.2501971523617));
#204162=CARTESIAN_POINT('Ctrl Pts',(-20.7270761473527,18.4973218716721,
21.2453151528455));
#204163=CARTESIAN_POINT('Ctrl Pts',(-20.7141466883093,18.4612140025996,
21.2429966738302));
#204164=CARTESIAN_POINT('Ctrl Pts',(-20.7002435345946,18.4254791783653,
21.2406781948149));
#204165=CARTESIAN_POINT('Ctrl Pts',(-20.6853897306834,18.3901668141557,
21.2383597157996));
#204166=CARTESIAN_POINT('Ctrl Pts',(-20.6572744298791,18.3233275218235,
21.2339712954789));
#204167=CARTESIAN_POINT('Ctrl Pts',(-20.6256662319327,18.2578040404403,
21.2295828751582));
#204168=CARTESIAN_POINT('Ctrl Pts',(-20.5907099296459,18.1939861175213,
21.2251944548374));
#204169=CARTESIAN_POINT('Ctrl Pts',(-20.555805493452,18.1302628838601,21.2208125457951));
#204170=CARTESIAN_POINT('Ctrl Pts',(-20.5175630443477,18.0682406045754,
21.2164306367528));
#204171=CARTESIAN_POINT('Ctrl Pts',(-20.4761752802482,18.0082887741057,
21.2120487277105));
#204172=CARTESIAN_POINT('Ctrl Pts',(-20.4348361356984,17.9484073709969,
21.207671966239));
#204173=CARTESIAN_POINT('Ctrl Pts',(-20.3903592887853,17.8905919800195,
21.2032952047674));
#204174=CARTESIAN_POINT('Ctrl Pts',(-20.3429823042688,17.8351857158214,
21.1989184432959));
#204175=CARTESIAN_POINT('Ctrl Pts',(-20.2956353568299,17.779814579276,21.1945444566975));
#204176=CARTESIAN_POINT('Ctrl Pts',(-20.2453922326902,17.7268499046386,
21.1901704700991));
#204177=CARTESIAN_POINT('Ctrl Pts',(-20.1925317242827,17.6766029818652,
21.1857964835008));
#204178=CARTESIAN_POINT('Ctrl Pts',(-20.1396872964519,17.6263713445954,
21.181423827503));
#204179=CARTESIAN_POINT('Ctrl Pts',(-20.084227414496,17.5788561499108,21.1770511715053));
#204180=CARTESIAN_POINT('Ctrl Pts',(-20.0264676125179,17.5343317350793,
21.1726785155076));
#204181=CARTESIAN_POINT('Ctrl Pts',(-19.9687063332045,17.4898061814369,
21.1683057476695));
#204182=CARTESIAN_POINT('Ctrl Pts',(-19.9086454002984,17.4482718524075,
21.1639329798313));
#204183=CARTESIAN_POINT('Ctrl Pts',(-19.8466319557782,17.409961651996,21.1595602119932));
#204184=CARTESIAN_POINT('Ctrl Pts',(-19.7845541750513,17.3716117064453,
21.1551829076018));
#204185=CARTESIAN_POINT('Ctrl Pts',(-19.7205202495877,17.3364928218529,
21.1508056032104));
#204186=CARTESIAN_POINT('Ctrl Pts',(-19.6549040128954,17.3047930859864,
21.1464282988189));
#204187=CARTESIAN_POINT('Ctrl Pts',(-19.5892519496617,17.2730760420274,
21.1420486044142));
#204188=CARTESIAN_POINT('Ctrl Pts',(-19.5220162999603,17.2447820509217,
21.1376689100095));
#204189=CARTESIAN_POINT('Ctrl Pts',(-19.4535905649465,17.220050874874,21.1332892156048));
#204190=CARTESIAN_POINT('Ctrl Pts',(-19.3850436009877,17.1952758829377,
21.1289017617551));
#204191=CARTESIAN_POINT('Ctrl Pts',(-19.3153028030891,17.1740764516624,
21.1245143079053));
#204192=CARTESIAN_POINT('Ctrl Pts',(-19.2447759299221,17.1565421762878,
21.1201268540555));
#204193=CARTESIAN_POINT('Ctrl Pts',(-19.196857633423,17.1446288081125,21.1171458724097));
#204194=CARTESIAN_POINT('Ctrl Pts',(-19.1485767107386,17.13440631873,21.1141648907639));
#204195=CARTESIAN_POINT('Ctrl Pts',(-19.1000625458484,17.1258891606135,
21.111183909118));
#204196=CARTESIAN_POINT('Ctrl Pts',(-19.0286448054896,17.1133510454397,
21.1067956036885));
#204197=CARTESIAN_POINT('Ctrl Pts',(-18.9564428209882,17.1044619390322,
21.102407298259));
#204198=CARTESIAN_POINT('Ctrl Pts',(-18.8838626628663,17.0993110592991,
21.0980189928294));
#204199=CARTESIAN_POINT('Ctrl Pts',(-18.8113901833097,17.0941678213148,
21.0936371978078));
#204200=CARTESIAN_POINT('Ctrl Pts',(-18.7385411210672,17.0927518343552,
21.0892554027861));
#204201=CARTESIAN_POINT('Ctrl Pts',(-18.6657304479849,17.0951010732392,
21.0848736077645));
#204202=CARTESIAN_POINT('Ctrl Pts',(-18.593005279013,17.09744755333,21.0804969584374));
#204203=CARTESIAN_POINT('Ctrl Pts',(-18.5203188893578,17.1035504601723,
21.0761203091104));
#204204=CARTESIAN_POINT('Ctrl Pts',(-18.4480883559106,17.1133957637881,
21.0717436597833));
#204205=CARTESIAN_POINT('Ctrl Pts',(-18.3759035978361,17.123234828042,21.0673697841136));
#204206=CARTESIAN_POINT('Ctrl Pts',(-18.3041745995243,17.1368115183043,
21.0629959084439));
#204207=CARTESIAN_POINT('Ctrl Pts',(-18.2333139941715,17.1540599124993,
21.0586220327743));
#204208=CARTESIAN_POINT('Ctrl Pts',(-18.1624749233001,17.171303064921,21.0542494863219));
#204209=CARTESIAN_POINT('Ctrl Pts',(-18.0925041898433,17.192215591997,21.0498769398696));
#204210=CARTESIAN_POINT('Ctrl Pts',(-18.0238032429013,17.2166806759683,
21.0455043934172));
#204211=CARTESIAN_POINT('Ctrl Pts',(-17.955100514348,17.2411463943888,21.0411317335723));
#204212=CARTESIAN_POINT('Ctrl Pts',(-17.8876680914168,17.269164688916,21.0367590737273));
#204213=CARTESIAN_POINT('Ctrl Pts',(-17.8218896924817,17.3005697377504,
21.0323864138824));
#204214=CARTESIAN_POINT('Ctrl Pts',(-17.7560430020855,17.3320073914629,
21.0280092143203));
#204215=CARTESIAN_POINT('Ctrl Pts',(-17.691854200438,17.3668386114322,21.0236320147581));
#204216=CARTESIAN_POINT('Ctrl Pts',(-17.6296837695453,17.404850874608,21.019254815196));
#204217=CARTESIAN_POINT('Ctrl Pts',(-17.567479369866,17.4428839069893,21.0148752240121));
#204218=CARTESIAN_POINT('Ctrl Pts',(-17.5072959348518,17.4841011703041,
21.0104956328281));
#204219=CARTESIAN_POINT('Ctrl Pts',(-17.4494639567956,17.5282474472731,
21.0061160416442));
#204220=CARTESIAN_POINT('Ctrl Pts',(-17.3915294664699,17.5724719774023,
21.0017286872495));
#204221=CARTESIAN_POINT('Ctrl Pts',(-17.3359551248471,17.6196355768842,
20.9973413328549));
#204222=CARTESIAN_POINT('Ctrl Pts',(-17.2830369579979,17.6694438866055,
20.9929539784602));
#204223=CARTESIAN_POINT('Ctrl Pts',(-17.2470700010395,17.703297163062,20.9899720197857));
#204224=CARTESIAN_POINT('Ctrl Pts',(-17.2123293114184,17.738371385165,20.9869900611112));
#204225=CARTESIAN_POINT('Ctrl Pts',(-17.1788971521192,17.7745654792115,
20.9840081024367));
#204226=CARTESIAN_POINT('Ctrl Pts',(-17.1297000971194,17.8278268560652,
20.9796200046294));
#204227=CARTESIAN_POINT('Ctrl Pts',(-17.0831463841702,17.8837226314485,
20.975231906822));
#204228=CARTESIAN_POINT('Ctrl Pts',(-17.0395308345184,17.941959714102,20.9708438090147));
#204229=CARTESIAN_POINT('Ctrl Pts',(-16.9959800368753,18.000110337497,20.9664622258139));
#204230=CARTESIAN_POINT('Ctrl Pts',(-16.9553590301246,18.0605949850623,
20.9620806426132));
#204231=CARTESIAN_POINT('Ctrl Pts',(-16.9179243707118,18.1230853394197,
20.9576990594124));
#204232=CARTESIAN_POINT('Ctrl Pts',(-16.8805337191531,18.1855022306699,
20.9533226271621));
#204233=CARTESIAN_POINT('Ctrl Pts',(-16.8463222204768,18.2499197329738,
20.9489461949117));
#204234=CARTESIAN_POINT('Ctrl Pts',(-16.8155038458629,18.3159796055054,
20.9445697626614));
#204235=CARTESIAN_POINT('Ctrl Pts',(-16.7847050250506,18.3819975640277,
20.9401961071924));
#204236=CARTESIAN_POINT('Ctrl Pts',(-16.7572952601506,18.4496553891047,
20.9358224517234));
#204237=CARTESIAN_POINT('Ctrl Pts',(-16.7334424864511,18.5185704837437,
20.9314487962544));
#204238=CARTESIAN_POINT('Ctrl Pts',(-16.709596977258,18.5874645898738,20.9270764728086));
#204239=CARTESIAN_POINT('Ctrl Pts',(-16.68930646627,18.6576147497773,20.9227041493628));
#204240=CARTESIAN_POINT('Ctrl Pts',(-16.6726900413674,18.7286202176274,
20.918331825917));
#204241=CARTESIAN_POINT('Ctrl Pts',(-16.6560731949978,18.7996274864939,
20.9139593915695));
#204242=CARTESIAN_POINT('Ctrl Pts',(-16.6431307277095,18.8714896362078,
20.9095869572221));
#204243=CARTESIAN_POINT('Ctrl Pts',(-16.6339309262445,18.9437943012289,
20.9052145228746));
#204244=CARTESIAN_POINT('Ctrl Pts',(-16.6247215778304,19.0161739992776,
20.9008375511022));
#204245=CARTESIAN_POINT('Ctrl Pts',(-16.6192627107137,19.0889966499121,
20.8964605793299));
#204246=CARTESIAN_POINT('Ctrl Pts',(-16.617570766158,19.1618441444085,20.8920836075575));
#204247=CARTESIAN_POINT('Ctrl Pts',(-16.6158778977392,19.23473141628,20.8877042457998));
#204248=CARTESIAN_POINT('Ctrl Pts',(-16.6179560333427,19.307643076478,20.883324884042));
#204249=CARTESIAN_POINT('Ctrl Pts',(-16.6237694821509,19.3801631210935,
20.8789455222842));
#204250=CARTESIAN_POINT('Ctrl Pts',(-16.6295932362114,19.4528117188942,
20.874558397419));
#204251=CARTESIAN_POINT('Ctrl Pts',(-16.6391654627898,19.5250668361741,
20.8701712725537));
#204252=CARTESIAN_POINT('Ctrl Pts',(-16.6523989027095,19.5965202611523,
20.8657841476884));
#204253=CARTESIAN_POINT('Ctrl Pts',(-16.6613997706558,19.645120084512,20.862800197044));
#204254=CARTESIAN_POINT('Ctrl Pts',(-16.6720933116133,19.6933492436894,
20.8598162463996));
#204255=CARTESIAN_POINT('Ctrl Pts',(-16.684438979983,19.741083602111,20.8568322957552));
#204256=CARTESIAN_POINT('Ctrl Pts',(-16.702594716654,19.8112825104007,20.852444050379));
#204257=CARTESIAN_POINT('Ctrl Pts',(-16.7243966034831,19.8806845781119,
20.8480558050029));
#204258=CARTESIAN_POINT('Ctrl Pts',(-16.749757746659,19.9488832428347,20.8436675596267));
#204259=CARTESIAN_POINT('Ctrl Pts',(-16.7750812520095,20.0169806956596,
20.8392858267335));
#204260=CARTESIAN_POINT('Ctrl Pts',(-16.8039533610691,20.0838778424496,
20.8349040938403));
#204261=CARTESIAN_POINT('Ctrl Pts',(-16.8362368493152,20.1491812319072,
20.8305223609472));
#204262=CARTESIAN_POINT('Ctrl Pts',(-16.868482404701,20.2144078903644,20.8261457765578));
#204263=CARTESIAN_POINT('Ctrl Pts',(-16.9041311639573,20.2780440812599,
20.8217691921684));
#204264=CARTESIAN_POINT('Ctrl Pts',(-16.9429976922085,20.3397159667008,
20.817392607779));
#204265=CARTESIAN_POINT('Ctrl Pts',(-16.9818395737555,20.4013487437166,
20.8130187987438));
#204266=CARTESIAN_POINT('Ctrl Pts',(-17.0238949191149,20.4610192797036,
20.8086449897085));
#204267=CARTESIAN_POINT('Ctrl Pts',(-17.0689328967322,20.5183792646418,
20.8042711806733));
#204268=CARTESIAN_POINT('Ctrl Pts',(-17.1139571706356,20.5757217966466,
20.7998987024578));
#204269=CARTESIAN_POINT('Ctrl Pts',(-17.1619619773634,20.6307547941729,
20.7955262242422));
#204270=CARTESIAN_POINT('Ctrl Pts',(-17.212674786275,20.6831611984034,20.7911537460267));
#204271=CARTESIAN_POINT('Ctrl Pts',(-17.2633888928252,20.7355689436083,
20.7867811559282));
#204272=CARTESIAN_POINT('Ctrl Pts',(-17.3168108022569,20.7853496168292,
20.7824085658297));
#204273=CARTESIAN_POINT('Ctrl Pts',(-17.3726307171725,20.8322225867455,
20.7780359757313));
#204274=CARTESIAN_POINT('Ctrl Pts',(-17.4285085618265,20.8791442012878,
20.7736588477721));
#204275=CARTESIAN_POINT('Ctrl Pts',(-17.4867890105141,20.9231517768141,
20.7692817198129));
#204276=CARTESIAN_POINT('Ctrl Pts',(-17.5471293748475,20.9640051680329,
20.7649045918536));
#204277=CARTESIAN_POINT('Ctrl Pts',(-17.6075026927368,21.0048808704282,
20.7605250734228));
#204278=CARTESIAN_POINT('Ctrl Pts',(-17.6699377529298,21.0425987092605,
20.7561455549919));
#204279=CARTESIAN_POINT('Ctrl Pts',(-17.7340654194772,21.0769635137576,
20.751766036561));
#204280=CARTESIAN_POINT('Ctrl Pts',(-17.7983067443387,21.1113892255971,
20.7473787559784));
#204281=CARTESIAN_POINT('Ctrl Pts',(-17.8642462295391,21.1424498297606,
20.7429914753957));
#204282=CARTESIAN_POINT('Ctrl Pts',(-17.931493378709,21.1699977342468,20.738604194813));
#204283=CARTESIAN_POINT('Ctrl Pts',(-17.9772094505245,21.18872539773,20.7356216262333));
#204284=CARTESIAN_POINT('Ctrl Pts',(-18.023529468233,21.2058306584364,20.7326390576535));
#204285=CARTESIAN_POINT('Ctrl Pts',(-18.0703272881618,21.2212804609212,
20.7296564890738));
#204286=CARTESIAN_POINT('Ctrl Pts',(-18.1391803751011,21.2440115752187,
20.7252682706902));
#204287=CARTESIAN_POINT('Ctrl Pts',(-18.2093370327966,21.2632455876901,
20.7208800523066));
#204288=CARTESIAN_POINT('Ctrl Pts',(-18.2804083778876,21.278835496443,20.716491833923));
#204289=CARTESIAN_POINT('Ctrl Pts',(-18.3513742461451,21.2944022682451,
20.7121101280851));
#204290=CARTESIAN_POINT('Ctrl Pts',(-18.423251639725,21.3063355698589,20.7077284222471));
#204291=CARTESIAN_POINT('Ctrl Pts',(-18.4956354561782,21.3145378162155,
20.7033467164092));
#204292=CARTESIAN_POINT('Ctrl Pts',(-18.5679342223251,21.3227304250094,
20.6989701590346));
#204293=CARTESIAN_POINT('Ctrl Pts',(-18.6407377523612,21.3272006332577,
20.6945936016599));
#204294=CARTESIAN_POINT('Ctrl Pts',(-18.7136313399141,21.3279020094672,
20.6902170442853));
#204295=CARTESIAN_POINT('Ctrl Pts',(-18.7864787033138,21.3286029409117,
20.6858432622256));
#204296=CARTESIAN_POINT('Ctrl Pts',(-18.8594155297534,21.325539777633,20.6814694801658));
#204297=CARTESIAN_POINT('Ctrl Pts',(-18.9320240051558,21.3187180773011,
20.6770956981061));
#204298=CARTESIAN_POINT('Ctrl Pts',(-19.0046103891442,21.3118984524984,
20.6727232467868));
#204299=CARTESIAN_POINT('Ctrl Pts',(-19.0768681404601,21.3013226060357,
20.6683507954674));
#204300=CARTESIAN_POINT('Ctrl Pts',(-19.1483831512649,21.2870480736119,
20.663978344148));
#204301=CARTESIAN_POINT('Ctrl Pts',(-19.2198999939593,21.2727731755395,
20.6596057808264));
#204302=CARTESIAN_POINT('Ctrl Pts',(-19.2906735857164,21.2547994997832,
20.6552332175047));
#204303=CARTESIAN_POINT('Ctrl Pts',(-19.3603002766085,21.2332356350139,
20.650860654183));
#204304=CARTESIAN_POINT('Ctrl Pts',(-19.4299992322408,21.2116493893579,
20.6464835526282));
#204305=CARTESIAN_POINT('Ctrl Pts',(-19.4985484486157,21.1864656580614,
20.6421064510734));
#204306=CARTESIAN_POINT('Ctrl Pts',(-19.5655605148557,21.1578426002461,
20.6377293495187));
#204307=CARTESIAN_POINT('Ctrl Pts',(-19.6326091810389,21.1292039093911,
20.6333498573247));
#204308=CARTESIAN_POINT('Ctrl Pts',(-19.6981185920468,21.0971223643352,
20.6289703651308));
#204309=CARTESIAN_POINT('Ctrl Pts',(-19.761724838013,21.0618027062146,20.6245908729369));
#204310=CARTESIAN_POINT('Ctrl Pts',(-19.8254438270173,21.0264204434629,
20.6202036180265));
#204311=CARTESIAN_POINT('Ctrl Pts',(-19.8872525050491,20.9877888617786,
20.6158163631161));
#204312=CARTESIAN_POINT('Ctrl Pts',(-19.9468154065796,20.9461564164545,
20.6114291082057));
#204313=CARTESIAN_POINT('Ctrl Pts',(-19.9873110556401,20.9178513330544,
20.6084462996012));
#204314=CARTESIAN_POINT('Ctrl Pts',(-20.0267692618289,20.8881600264952,
20.6054634909968));
#204315=CARTESIAN_POINT('Ctrl Pts',(-20.065093928451,20.8571706939564,20.6024806823923));
#204316=CARTESIAN_POINT('Ctrl Pts',(-20.1207334286554,20.8121805837716,
20.59815026038));
#204317=CARTESIAN_POINT('Ctrl Pts',(-20.1742116960449,20.7642672661332,
20.5938198383676));
#204318=CARTESIAN_POINT('Ctrl Pts',(-20.2251992661504,20.7136688752458,
20.5894894163552));
#204319=CARTESIAN_POINT('Ctrl Pts',(-20.2761150699366,20.6631417028979,
20.5851650895235));
#204320=CARTESIAN_POINT('Ctrl Pts',(-20.3245467786866,20.6099372970267,
20.5808407626917));
#204321=CARTESIAN_POINT('Ctrl Pts',(-20.3701971565707,20.5543346064291,
20.57651643586));
#204322=CARTESIAN_POINT('Ctrl Pts',(-20.4157961637033,20.4987944860036,
20.5721969752293));
#204323=CARTESIAN_POINT('Ctrl Pts',(-20.4586197391826,20.4408618191658,
20.5678775145986));
#204324=CARTESIAN_POINT('Ctrl Pts',(-20.498408153215,20.3808516439567,20.563558053968));
#204325=CARTESIAN_POINT('Ctrl Pts',(-20.5381709780786,20.3208800631614,
20.5592413713171));
#204326=CARTESIAN_POINT('Ctrl Pts',(-20.5749022411959,20.2588340376598,
20.5549246886661));
#204327=CARTESIAN_POINT('Ctrl Pts',(-20.6083841486135,20.1950594816507,
20.5506080060152));
#204328=CARTESIAN_POINT('Ctrl Pts',(-20.6418605361497,20.1312954396179,
20.5462920350196));
#204329=CARTESIAN_POINT('Ctrl Pts',(-20.6720883966209,20.0658038696194,
20.5419760640239));
#204330=CARTESIAN_POINT('Ctrl Pts',(-20.6988955814925,19.9989558070293,
20.5376600930283));
#204331=CARTESIAN_POINT('Ctrl Pts',(-20.7071130320822,19.978464261424,20.5363370791209));
#204332=CARTESIAN_POINT('Ctrl Pts',(-20.7150093912817,19.9578454053111,
20.5350140652135));
#204333=CARTESIAN_POINT('Ctrl Pts',(-20.7225806064498,19.9371103026755,
20.5336910513061));
#204334=CARTESIAN_POINT('Ctrl Pts',(-20.7225806064498,19.9371103026755,
21.3335535417785));
#204335=CARTESIAN_POINT('Ctrl Pts',(-20.7478890194195,19.8677987682902,
21.3291191901433));
#204336=CARTESIAN_POINT('Ctrl Pts',(-20.7695971958024,19.7970870004519,
21.324684838508));
#204337=CARTESIAN_POINT('Ctrl Pts',(-20.7875591110991,19.725377271292,21.3202504868728));
#204338=CARTESIAN_POINT('Ctrl Pts',(-20.8055066416424,19.6537249706835,
21.3158196864766));
#204339=CARTESIAN_POINT('Ctrl Pts',(-20.8197137585767,19.5810767457616,
21.3113888860803));
#204340=CARTESIAN_POINT('Ctrl Pts',(-20.8300842035801,19.5078501499109,
21.3069580856841));
#204341=CARTESIAN_POINT('Ctrl Pts',(-20.8404495509225,19.4346595490787,
21.3025294632772));
#204342=CARTESIAN_POINT('Ctrl Pts',(-20.8469819090597,19.360891601732,21.2981008408703));
#204343=CARTESIAN_POINT('Ctrl Pts',(-20.8496363437061,19.2869727661079,
21.2936722184634));
#204344=CARTESIAN_POINT('Ctrl Pts',(-20.8505585800474,19.2612909748395,
21.2921335719831));
#204345=CARTESIAN_POINT('Ctrl Pts',(-20.8510131737418,19.2355910222583,
21.2905949255028));
#204346=CARTESIAN_POINT('Ctrl Pts',(-20.8509997094733,19.2098909057104,
21.2890562790225));
#204347=CARTESIAN_POINT('Origin',(-18.734,19.211,0.));
#204348=CARTESIAN_POINT('',(-20.3539402646795,17.8481050888384,21.9999997807644));
#204349=CARTESIAN_POINT('Ctrl Pts',(-20.3539402646795,17.8481050888384,
21.9999997807644));
#204350=CARTESIAN_POINT('Ctrl Pts',(-20.3072934957001,17.7926606237751,
21.9956147707751));
#204351=CARTESIAN_POINT('Ctrl Pts',(-20.2577053013778,17.7395048193498,
21.9912297607858));
#204352=CARTESIAN_POINT('Ctrl Pts',(-20.2054290597327,17.6889666487971,
21.9868447507965));
#204353=CARTESIAN_POINT('Ctrl Pts',(-20.1532304392223,17.6385035186453,
21.982466251785));
#204354=CARTESIAN_POINT('Ctrl Pts',(-20.0983520388586,17.5906506399773,
21.9780877527736));
#204355=CARTESIAN_POINT('Ctrl Pts',(-20.0410869968869,17.545703455066,21.9737092537621));
#204356=CARTESIAN_POINT('Ctrl Pts',(-19.9838893502852,17.5008091686081,
21.969335907817));
#204357=CARTESIAN_POINT('Ctrl Pts',(-19.9243110199867,17.4588140795273,
21.9649625618719));
#204358=CARTESIAN_POINT('Ctrl Pts',(-19.8626801771137,17.4199751375844,
21.9605892159267));
#204359=CARTESIAN_POINT('Ctrl Pts',(-19.8010883319371,17.381160771474,21.9562186372717));
#204360=CARTESIAN_POINT('Ctrl Pts',(-19.7374469588082,17.3454988470316,
21.9518480586166));
#204361=CARTESIAN_POINT('Ctrl Pts',(-19.6721141643387,17.3132036951593,
21.9474774799615));
#204362=CARTESIAN_POINT('Ctrl Pts',(-19.6068010732891,17.2809182830347,
21.9431082194094));
#204363=CARTESIAN_POINT('Ctrl Pts',(-19.539798006527,17.2519978415642,21.9387389588572));
#204364=CARTESIAN_POINT('Ctrl Pts',(-19.4714871908732,17.2266105111904,
21.934369698305));
#204365=CARTESIAN_POINT('Ctrl Pts',(-19.4031743543433,17.2012224297694,
21.9300003084946));
#204366=CARTESIAN_POINT('Ctrl Pts',(-19.33355414576,17.1793678332055,21.9256309186843));
#204367=CARTESIAN_POINT('Ctrl Pts',(-19.2630266691229,17.1611659132123,
21.9212615288739));
#204368=CARTESIAN_POINT('Ctrl Pts',(-19.1924273973489,17.142945464138,21.9168876911383));
#204369=CARTESIAN_POINT('Ctrl Pts',(-19.1209194825959,17.1283852352836,
21.9125138534028));
#204370=CARTESIAN_POINT('Ctrl Pts',(-19.0489151638194,17.1175536931661,
21.9081400156672));
#204371=CARTESIAN_POINT('Ctrl Pts',(-18.9768710224476,17.1067161605729,
21.9037637589438));
#204372=CARTESIAN_POINT('Ctrl Pts',(-18.9043304115686,17.0996114670891,
21.8993875022204));
#204373=CARTESIAN_POINT('Ctrl Pts',(-18.8317099769259,17.096256100515,21.895011245497));
#204374=CARTESIAN_POINT('Ctrl Pts',(-18.7589654023404,17.0928949981583,
21.8906275078454));
#204375=CARTESIAN_POINT('Ctrl Pts',(-18.6861412147951,17.0932960158796,
21.8862437701938));
#204376=CARTESIAN_POINT('Ctrl Pts',(-18.6136526546588,17.0974235248117,
21.8818600325422));
#204377=CARTESIAN_POINT('Ctrl Pts',(-18.5716446773508,17.099815465019,21.8793196047637));
#204378=CARTESIAN_POINT('Ctrl Pts',(-18.5297493105789,17.1034579173405,
21.8767791769852));
#204379=CARTESIAN_POINT('Ctrl Pts',(-18.4880458594114,17.1083360799388,
21.8742387492067));
#204380=CARTESIAN_POINT('Ctrl Pts',(-18.4158852200683,17.116776900112,21.8698429764932));
#204381=CARTESIAN_POINT('Ctrl Pts',(-18.3440242584073,17.1289525208195,
21.8654472037797));
#204382=CARTESIAN_POINT('Ctrl Pts',(-18.272878821027,17.1448305349506,21.8610514310662));
#204383=CARTESIAN_POINT('Ctrl Pts',(-18.2018362105903,17.160685600489,21.8566620115904));
#204384=CARTESIAN_POINT('Ctrl Pts',(-18.1315075364803,17.1802323315536,
21.8522725921145));
#204385=CARTESIAN_POINT('Ctrl Pts',(-18.0623022824371,17.2033866965422,
21.8478831726387));
#204386=CARTESIAN_POINT('Ctrl Pts',(-17.9931750463637,17.2265149586492,
21.8434987015386));
#204387=CARTESIAN_POINT('Ctrl Pts',(-17.9251691678202,17.2532426232453,
21.8391142304384));
#204388=CARTESIAN_POINT('Ctrl Pts',(-17.8586810826102,17.2834352688276,
21.8347297593383));
#204389=CARTESIAN_POINT('Ctrl Pts',(-17.7922332814893,17.3136096211591,
21.8303479447205));
#204390=CARTESIAN_POINT('Ctrl Pts',(-17.7273018852858,17.3472445902797,
21.8259661301027));
#204391=CARTESIAN_POINT('Ctrl Pts',(-17.6642640529712,17.384157367578,21.8215843154849));
#204392=CARTESIAN_POINT('Ctrl Pts',(-17.601243827434,17.4210598349556,21.8172037247295));
#204393=CARTESIAN_POINT('Ctrl Pts',(-17.5401165299889,17.4612380500253,
21.8128231339742));
#204394=CARTESIAN_POINT('Ctrl Pts',(-17.4812339028314,17.5044637109674,
21.8084425432188));
#204395=CARTESIAN_POINT('Ctrl Pts',(-17.4223484927206,17.547691414872,21.8040617454248));
#204396=CARTESIAN_POINT('Ctrl Pts',(-17.365708349646,17.5939665647424,21.7996809476307));
#204397=CARTESIAN_POINT('Ctrl Pts',(-17.3116341001189,17.6430190540522,
21.7953001498367));
#204398=CARTESIAN_POINT('Ctrl Pts',(-17.2575027316979,17.692123357746,21.7909147245846));
#204399=CARTESIAN_POINT('Ctrl Pts',(-17.2059430246541,17.7440105345835,
21.7865292993325));
#204400=CARTESIAN_POINT('Ctrl Pts',(-17.1572399043858,17.798372447926,21.7821438740803));
#204401=CARTESIAN_POINT('Ctrl Pts',(-17.1085095392263,17.852764771731,21.7777559955884));
#204402=CARTESIAN_POINT('Ctrl Pts',(-17.0626392444271,17.9096342143152,
21.7733681170964));
#204403=CARTESIAN_POINT('Ctrl Pts',(-17.0198729444951,17.9686403750982,
21.7689802386045));
#204404=CARTESIAN_POINT('Ctrl Pts',(-16.9770309082245,18.0277510319582,
21.7645845894648));
#204405=CARTESIAN_POINT('Ctrl Pts',(-16.9373041057529,18.0890055601327,
21.7601889403251));
#204406=CARTESIAN_POINT('Ctrl Pts',(-16.9008922045882,18.1520359730375,
21.7557932911855));
#204407=CARTESIAN_POINT('Ctrl Pts',(-16.8767858983712,18.1937649238989,
21.7528831749654));
#204408=CARTESIAN_POINT('Ctrl Pts',(-16.8541315758308,18.2362717295104,
21.7499730587453));
#204409=CARTESIAN_POINT('Ctrl Pts',(-16.8329755513189,18.2794448242231,
21.7470629425252));
#204410=CARTESIAN_POINT('Ctrl Pts',(-16.8011149074337,18.3444628334097,
21.7426803527574));
#204411=CARTESIAN_POINT('Ctrl Pts',(-16.772529978103,18.4112473176336,21.7382977629896));
#204412=CARTESIAN_POINT('Ctrl Pts',(-16.7474198249775,18.4794344129146,
21.7339151732219));
#204413=CARTESIAN_POINT('Ctrl Pts',(-16.7223474511024,18.5475189179272,
21.7295391772393));
#204414=CARTESIAN_POINT('Ctrl Pts',(-16.7007396419766,18.6170013950868,
21.7251631812567));
#204415=CARTESIAN_POINT('Ctrl Pts',(-16.6827487806458,18.6874950476855,
21.7207871852741));
#204416=CARTESIAN_POINT('Ctrl Pts',(-16.6647794728902,18.7579042468375,
21.7164164318621));
#204417=CARTESIAN_POINT('Ctrl Pts',(-16.650418624554,18.8293217487381,21.71204567845));
#204418=CARTESIAN_POINT('Ctrl Pts',(-16.6397692918518,18.9013441570891,
21.7076749250379));
#204419=CARTESIAN_POINT('Ctrl Pts',(-16.6291268554032,18.973319925447,21.7033070020215));
#204420=CARTESIAN_POINT('Ctrl Pts',(-16.6221912368165,19.0458993457387,
21.698939079005));
#204421=CARTESIAN_POINT('Ctrl Pts',(-16.6190144349639,19.1186687502037,
21.6945711559885));
#204422=CARTESIAN_POINT('Ctrl Pts',(-16.6158386349475,19.19141520611,21.6902046104402));
#204423=CARTESIAN_POINT('Ctrl Pts',(-16.6164193196609,19.2643510442235,
21.6858380648919));
#204424=CARTESIAN_POINT('Ctrl Pts',(-16.6207564965869,19.3370590944058,
21.6814715193436));
#204425=CARTESIAN_POINT('Ctrl Pts',(-16.6250937465921,19.4097683696811,
21.6771049002213));
#204426=CARTESIAN_POINT('Ctrl Pts',(-16.6331875836567,19.4822493665785,
21.6727382810989));
#204427=CARTESIAN_POINT('Ctrl Pts',(-16.6449860089037,19.5540882466713,
21.6683716619766));
#204428=CARTESIAN_POINT('Ctrl Pts',(-16.6567966463011,19.6260014847561,
21.6640005231147));
#204429=CARTESIAN_POINT('Ctrl Pts',(-16.6723194491993,19.6972708005986,
21.6596293842528));
#204430=CARTESIAN_POINT('Ctrl Pts',(-16.6914510872628,19.7674916343271,
21.6552582453909));
#204431=CARTESIAN_POINT('Ctrl Pts',(-16.7105931022024,19.8377505553794,
21.6508847356516));
#204432=CARTESIAN_POINT('Ctrl Pts',(-16.7333476979536,19.9069594022358,
21.6465112259124));
#204433=CARTESIAN_POINT('Ctrl Pts',(-16.7595621821267,19.9747305174941,
21.6421377161732));
#204434=CARTESIAN_POINT('Ctrl Pts',(-16.7858234022015,20.0426224569562,
21.6377564092208));
#204435=CARTESIAN_POINT('Ctrl Pts',(-16.8155566307479,20.1090711042367,
21.6333751022684));
#204436=CARTESIAN_POINT('Ctrl Pts',(-16.8485619796008,20.1737110008893,
21.6289937953161));
#204437=CARTESIAN_POINT('Ctrl Pts',(-16.8714294691446,20.2184962315317,
21.6259582421587));
#204438=CARTESIAN_POINT('Ctrl Pts',(-16.8958666987907,20.2624137158362,
21.6229226890013));
#204439=CARTESIAN_POINT('Ctrl Pts',(-16.9217951496002,20.3053503004923,
21.6198871358439));
#204440=CARTESIAN_POINT('Ctrl Pts',(-16.9592870711159,20.3674355779312,
21.6154977983717));
#204441=CARTESIAN_POINT('Ctrl Pts',(-17.0000461372983,20.4277127259959,
21.6111084608995));
#204442=CARTESIAN_POINT('Ctrl Pts',(-17.0438725612033,20.4858169439674,
21.6067191234274));
#204443=CARTESIAN_POINT('Ctrl Pts',(-17.0876339985392,20.5438350040133,
21.6023362945397));
#204444=CARTESIAN_POINT('Ctrl Pts',(-17.1344534764691,20.5996861485813,
21.597953465652));
#204445=CARTESIAN_POINT('Ctrl Pts',(-17.1840867418393,20.6530325558661,
21.5935706367643));
#204446=CARTESIAN_POINT('Ctrl Pts',(-17.2336617074652,20.7063163019118,
21.5891929559925));
#204447=CARTESIAN_POINT('Ctrl Pts',(-17.2860435680415,20.7571008040507,
21.5848152752207));
#204448=CARTESIAN_POINT('Ctrl Pts',(-17.3409474964239,20.8050808393179,
21.580437594449));
#204449=CARTESIAN_POINT('Ctrl Pts',(-17.3958166125325,20.853030452461,21.5760626893806));
#204450=CARTESIAN_POINT('Ctrl Pts',(-17.4532042613681,20.8981788105171,
21.5716877843123));
#204451=CARTESIAN_POINT('Ctrl Pts',(-17.512789428658,20.9402581474269,21.5673128792439));
#204452=CARTESIAN_POINT('Ctrl Pts',(-17.5723564435283,20.9823246650092,
21.5629393069756));
#204453=CARTESIAN_POINT('Ctrl Pts',(-17.6341192541722,21.0213237397462,
21.5585657347073));
#204454=CARTESIAN_POINT('Ctrl Pts',(-17.6977258376919,21.0570294852826,
21.5541921624389));
#204455=CARTESIAN_POINT('Ctrl Pts',(-17.7613339958298,21.0927361147356,
21.5498184819002));
#204456=CARTESIAN_POINT('Ctrl Pts',(-17.826785596102,21.1251490188774,21.5454448013616));
#204457=CARTESIAN_POINT('Ctrl Pts',(-17.8937033322731,21.1540878802069,
21.5410711208229));
#204458=CARTESIAN_POINT('Ctrl Pts',(-17.9606902956987,21.1830566791589,
21.5366929156557));
#204459=CARTESIAN_POINT('Ctrl Pts',(-18.0291459798704,21.2085440679544,
21.5323147104885));
#204460=CARTESIAN_POINT('Ctrl Pts',(-18.0986731480005,21.2304179337444,
21.5279365053214));
#204461=CARTESIAN_POINT('Ctrl Pts',(-18.1682381862999,21.2523037138266,
21.5235559154264));
#204462=CARTESIAN_POINT('Ctrl Pts',(-18.2388754035045,21.2705719312819,
21.5191753255314));
#204463=CARTESIAN_POINT('Ctrl Pts',(-18.3101750846391,21.2851411333656,
21.5147947356365));
#204464=CARTESIAN_POINT('Ctrl Pts',(-18.3816007583693,21.2997360804675,
21.5104064048669));
#204465=CARTESIAN_POINT('Ctrl Pts',(-18.4536907566283,21.3106188870059,
21.5060180740973));
#204466=CARTESIAN_POINT('Ctrl Pts',(-18.5260285057222,21.3177598006341,
21.5016297433277));
#204467=CARTESIAN_POINT('Ctrl Pts',(-18.5750325606489,21.3225972987322,
21.4986569386059));
#204468=CARTESIAN_POINT('Ctrl Pts',(-18.6241502208557,21.3257186676998,
21.4956841338842));
#204469=CARTESIAN_POINT('Ctrl Pts',(-18.6732524671973,21.3271282421579,
21.4927113291624));
#204470=CARTESIAN_POINT('Ctrl Pts',(-18.7457477304191,21.3292093581758,
21.4883222374839));
#204471=CARTESIAN_POINT('Ctrl Pts',(-18.8184908959863,21.3275648466035,
21.4839331458055));
#204472=CARTESIAN_POINT('Ctrl Pts',(-18.8910671061328,21.3221653000585,
21.479544054127));
#204473=CARTESIAN_POINT('Ctrl Pts',(-18.963535950148,21.316773741371,21.4751614554825));
#204474=CARTESIAN_POINT('Ctrl Pts',(-19.0358378521744,21.3076382108716,
21.4707788568379));
#204475=CARTESIAN_POINT('Ctrl Pts',(-19.1075565804157,21.2947812940009,
21.4663962581934));
#204476=CARTESIAN_POINT('Ctrl Pts',(-19.1791914639277,21.2819394078585,
21.462018783145));
#204477=CARTESIAN_POINT('Ctrl Pts',(-19.2502440557653,21.2653848625367,
21.4576413080965));
#204478=CARTESIAN_POINT('Ctrl Pts',(-19.3203035805939,21.2451920045519,
21.4532638330481));
#204479=CARTESIAN_POINT('Ctrl Pts',(-19.3903189251765,21.2250118803879,
21.4488891184798));
#204480=CARTESIAN_POINT('Ctrl Pts',(-19.4593419831433,21.2011981291416,
21.4445144039115));
#204481=CARTESIAN_POINT('Ctrl Pts',(-19.5269738982851,21.1738757975579,
21.4401396893431));
#204482=CARTESIAN_POINT('Ctrl Pts',(-19.5945854490439,21.1465616928952,
21.4357662920281));
#204483=CARTESIAN_POINT('Ctrl Pts',(-19.660806241817,21.1157412858172,21.4313928947131));
#204484=CARTESIAN_POINT('Ctrl Pts',(-19.7252558616825,21.0815883610993,
21.427019497398));
#204485=CARTESIAN_POINT('Ctrl Pts',(-19.7897073112052,21.0474344668156,
21.4226459759268));
#204486=CARTESIAN_POINT('Ctrl Pts',(-19.8523870628952,21.009948094583,21.4182724544556));
#204487=CARTESIAN_POINT('Ctrl Pts',(-19.9129393440597,20.9693489480272,
21.4138989329844));
#204488=CARTESIAN_POINT('Ctrl Pts',(-19.9735546264146,20.9287075603778,
21.4095208611139));
#204489=CARTESIAN_POINT('Ctrl Pts',(-20.0320376175176,20.884947201305,21.4051427892433));
#204490=CARTESIAN_POINT('Ctrl Pts',(-20.0880622982485,20.8383304189568,
21.4007647173728));
#204491=CARTESIAN_POINT('Ctrl Pts',(-20.1441176775265,20.7916880930897,
21.3963842465516));
#204492=CARTESIAN_POINT('Ctrl Pts',(-20.1977117100799,20.742186555063,21.3920037757304));
#204493=CARTESIAN_POINT('Ctrl Pts',(-20.2485542308315,20.6901262562305,
21.3876233049092));
#204494=CARTESIAN_POINT('Ctrl Pts',(-20.2994868807634,20.6379736694469,
21.3832350687719));
#204495=CARTESIAN_POINT('Ctrl Pts',(-20.3476579595779,20.583253625968,21.3788468326346));
#204496=CARTESIAN_POINT('Ctrl Pts',(-20.3928170701038,20.5263003185327,
21.3744585964973));
#204497=CARTESIAN_POINT('Ctrl Pts',(-20.4234260340952,20.4876972168291,
21.3714842384918));
#204498=CARTESIAN_POINT('Ctrl Pts',(-20.4526521165783,20.4480687834689,
21.3685098804864));
#204499=CARTESIAN_POINT('Ctrl Pts',(-20.4804290561878,20.407526034695,21.3655355224809));
#204500=CARTESIAN_POINT('Ctrl Pts',(-20.5219934576021,20.3468593410935,
21.3610848014214));
#204501=CARTESIAN_POINT('Ctrl Pts',(-20.5604706135638,20.283911430233,21.3566340803619));
#204502=CARTESIAN_POINT('Ctrl Pts',(-20.5956058292723,20.2190241745213,
21.3521833593024));
#204503=CARTESIAN_POINT('Ctrl Pts',(-20.6306759483131,20.154257138482,21.3477408843033));
#204504=CARTESIAN_POINT('Ctrl Pts',(-20.6624162151988,20.0875583047225,
21.3432984093041));
#204505=CARTESIAN_POINT('Ctrl Pts',(-20.6906150299305,20.0192985986937,
21.338855934305));
#204506=CARTESIAN_POINT('Ctrl Pts',(-20.7018340902154,19.9921410828813,
21.3370884701295));
#204507=CARTESIAN_POINT('Ctrl Pts',(-20.7124930633451,19.9647368113629,
21.335321005954));
#204508=CARTESIAN_POINT('Ctrl Pts',(-20.7225806064498,19.9371103026755,
21.3335535417785));
#204509=CARTESIAN_POINT('',(-17.1140743056112,17.8480877707428,22.));
#204510=CARTESIAN_POINT('Origin',(-18.734,19.211,22.));
#204511=CARTESIAN_POINT('Ctrl Pts',(-20.7225806064499,19.9371103026755,
21.5555703710623));
#204512=CARTESIAN_POINT('Ctrl Pts',(-20.6978891140345,20.0047322917599,
21.5598847349407));
#204513=CARTESIAN_POINT('Ctrl Pts',(-20.669739933046,20.071105290786,21.564199098819));
#204514=CARTESIAN_POINT('Ctrl Pts',(-20.6382937973645,20.1358535739883,
21.5685134626974));
#204515=CARTESIAN_POINT('Ctrl Pts',(-20.6068209721235,20.2006568115793,
21.5728314883444));
#204516=CARTESIAN_POINT('Ctrl Pts',(-20.5720458189299,20.263832130486,21.5771495139913));
#204517=CARTESIAN_POINT('Ctrl Pts',(-20.5341758702126,20.3250268561863,
21.5814675396383));
#204518=CARTESIAN_POINT('Ctrl Pts',(-20.496290452322,20.3862465787997,21.5857873291188));
#204519=CARTESIAN_POINT('Ctrl Pts',(-20.4553080047756,20.4454836883216,
21.5901071185994));
#204520=CARTESIAN_POINT('Ctrl Pts',(-20.4114788047957,20.5024154480496,
21.5944269080799));
#204521=CARTESIAN_POINT('Ctrl Pts',(-20.3675728312531,20.5594469324823,
21.5987542643339));
#204522=CARTESIAN_POINT('Ctrl Pts',(-20.3208104691955,20.61416462363,21.603081620588));
#204523=CARTESIAN_POINT('Ctrl Pts',(-20.271481140103,20.6662802973406,21.607408976842));
#204524=CARTESIAN_POINT('Ctrl Pts',(-20.2294416062698,20.7106944150369,
21.6110968445466));
#204525=CARTESIAN_POINT('Ctrl Pts',(-20.1855384995037,20.7532192421642,
21.6147847122511));
#204526=CARTESIAN_POINT('Ctrl Pts',(-20.1399695343548,20.7936998036476,
21.6184725799557));
#204527=CARTESIAN_POINT('Ctrl Pts',(-20.0856806209084,20.8419266108937,
21.6228661475946));
#204528=CARTESIAN_POINT('Ctrl Pts',(-20.0288044225739,20.8874484514206,
21.6272597152335));
#204529=CARTESIAN_POINT('Ctrl Pts',(-19.969641252187,20.9299763511735,21.6316532828724));
#204530=CARTESIAN_POINT('Ctrl Pts',(-19.9105643807625,20.9724422171712,
21.636040441789));
#204531=CARTESIAN_POINT('Ctrl Pts',(-19.8492075475796,21.0119225341567,
21.6404276007057));
#204532=CARTESIAN_POINT('Ctrl Pts',(-19.7859054205824,21.0481673810922,
21.6448147596223));
#204533=CARTESIAN_POINT('Ctrl Pts',(-19.7226757606736,21.0843707356065,
21.6491968962016));
#204534=CARTESIAN_POINT('Ctrl Pts',(-19.6575056463759,21.1173457404981,
21.6535790327809));
#204535=CARTESIAN_POINT('Ctrl Pts',(-19.5907587261482,21.1468857107714,
21.6579611693602));
#204536=CARTESIAN_POINT('Ctrl Pts',(-19.5240529471155,21.176407473318,21.6623406048961));
#204537=CARTESIAN_POINT('Ctrl Pts',(-19.455772729471,21.2024982084514,21.6667200404319));
#204538=CARTESIAN_POINT('Ctrl Pts',(-19.386305067273,21.2249977902694,21.6710994759677));
#204539=CARTESIAN_POINT('Ctrl Pts',(-19.3168574801294,21.2474908700645,
21.675477645916));
#204540=CARTESIAN_POINT('Ctrl Pts',(-19.2462235870209,21.2663947090104,
21.6798558158643));
#204541=CARTESIAN_POINT('Ctrl Pts',(-19.1748074790921,21.2815984077982,
21.6842339858126));
#204542=CARTESIAN_POINT('Ctrl Pts',(-19.1033886290298,21.2968026903559,
21.6886123238676));
#204543=CARTESIAN_POINT('Ctrl Pts',(-19.0311879752794,21.3083064524741,
21.6929906619226));
#204544=CARTESIAN_POINT('Ctrl Pts',(-18.9586201563124,21.3160498296663,
21.6973689999776));
#204545=CARTESIAN_POINT('Ctrl Pts',(-18.8859763854438,21.3238013113356,
21.7017519205474));
#204546=CARTESIAN_POINT('Ctrl Pts',(-18.8129651613083,21.3277844990936,
21.7061348411171));
#204547=CARTESIAN_POINT('Ctrl Pts',(-18.7400057927391,21.3279914809591,
21.7105177616869));
#204548=CARTESIAN_POINT('Ctrl Pts',(-18.6670060696851,21.3281985773082,
21.7149031064896));
#204549=CARTESIAN_POINT('Ctrl Pts',(-18.5940587399491,21.324625332556,21.7192884512922));
#204550=CARTESIAN_POINT('Ctrl Pts',(-18.5215799495223,21.3173159122399,
21.7236737960949));
#204551=CARTESIAN_POINT('Ctrl Pts',(-18.4489730689547,21.3099935741492,
21.7280668910191));
#204552=CARTESIAN_POINT('Ctrl Pts',(-18.3768368570159,21.2989219477123,
21.7324599859432));
#204553=CARTESIAN_POINT('Ctrl Pts',(-18.3055786328723,21.284196597573,21.7368530808674));
#204554=CARTESIAN_POINT('Ctrl Pts',(-18.2580238618236,21.2743695121678,
21.7397848494573));
#204555=CARTESIAN_POINT('Ctrl Pts',(-18.2108598781007,21.2629162374029,
21.7427166180472));
#204556=CARTESIAN_POINT('Ctrl Pts',(-18.1642034712006,21.2498773665349,
21.7456483866371));
#204557=CARTESIAN_POINT('Ctrl Pts',(-18.0951059728948,21.230566977725,21.7499902956831));
#204558=CARTESIAN_POINT('Ctrl Pts',(-18.0268401014068,21.2076976293853,
21.754332204729));
#204559=CARTESIAN_POINT('Ctrl Pts',(-17.959804544219,21.1813579360736,21.758674113775));
#204560=CARTESIAN_POINT('Ctrl Pts',(-17.8928699309423,21.1550579057671,
21.7630094846598));
#204561=CARTESIAN_POINT('Ctrl Pts',(-17.8271624114981,21.1252980759476,
21.7673448555445));
#204562=CARTESIAN_POINT('Ctrl Pts',(-17.7630671934661,21.0922172881398,
21.7716802264293));
#204563=CARTESIAN_POINT('Ctrl Pts',(-17.6990456418676,21.0591745210102,
21.7760106145506));
#204564=CARTESIAN_POINT('Ctrl Pts',(-17.6366331495171,21.0228185970339,
21.7803410026719));
#204565=CARTESIAN_POINT('Ctrl Pts',(-17.5761948535926,20.9833363797407,
21.7846713907932));
#204566=CARTESIAN_POINT('Ctrl Pts',(-17.5157937013986,20.9438784271429,
21.7889991175759));
#204567=CARTESIAN_POINT('Ctrl Pts',(-17.4573647522916,20.9012982594394,
21.7933268443586));
#204568=CARTESIAN_POINT('Ctrl Pts',(-17.4012470250051,20.8558278048605,
21.7976545711413));
#204569=CARTESIAN_POINT('Ctrl Pts',(-17.3451443445715,20.81036954228,21.8019811375301));
#204570=CARTESIAN_POINT('Ctrl Pts',(-17.2913520397843,20.7620228406339,
21.8063077039189));
#204571=CARTESIAN_POINT('Ctrl Pts',(-17.2401772158046,20.7110608285729,
21.8106342703077));
#204572=CARTESIAN_POINT('Ctrl Pts',(-17.1889983840908,20.6600948254439,
21.8149611755297));
#204573=CARTESIAN_POINT('Ctrl Pts',(-17.1404377881069,20.6065134551268,
21.8192880807517));
#204574=CARTESIAN_POINT('Ctrl Pts',(-17.0947654083712,20.5506264231522,
21.8236149859736));
#204575=CARTESIAN_POINT('Ctrl Pts',(-17.0490382189606,20.4946723232895,
21.827947083749));
#204576=CARTESIAN_POINT('Ctrl Pts',(-17.0062064773784,20.4364074215726,
21.8322791815243));
#204577=CARTESIAN_POINT('Ctrl Pts',(-16.9664990268283,20.3761735106142,
21.8366112792996));
#204578=CARTESIAN_POINT('Ctrl Pts',(-16.9267670699395,20.3159024249543,
21.8409460507257));
#204579=CARTESIAN_POINT('Ctrl Pts',(-16.8901634882159,20.2536603390498,
21.8452808221518));
#204580=CARTESIAN_POINT('Ctrl Pts',(-16.856871493227,20.1898143690508,21.8496155935779));
#204581=CARTESIAN_POINT('Ctrl Pts',(-16.8235124512874,20.1258398192654,
21.8539590948264));
#204582=CARTESIAN_POINT('Ctrl Pts',(-16.7934785159735,20.060255385527,21.858302596075));
#204583=CARTESIAN_POINT('Ctrl Pts',(-16.7669047947946,19.9934483712413,
21.8626460973235));
#204584=CARTESIAN_POINT('Ctrl Pts',(-16.7461481233425,19.9412655686561,
21.8660387959885));
#204585=CARTESIAN_POINT('Ctrl Pts',(-16.7275016016086,19.8883372861217,
21.8694314946536));
#204586=CARTESIAN_POINT('Ctrl Pts',(-16.7110080073322,19.8348528653473,
21.8728241933186));
#204587=CARTESIAN_POINT('Ctrl Pts',(-16.6890808041098,19.7637486691424,
21.8773345742491));
#204588=CARTESIAN_POINT('Ctrl Pts',(-16.6708715122103,19.691373744136,21.8818449551797));
#204589=CARTESIAN_POINT('Ctrl Pts',(-16.6565194069635,19.6181404985465,
21.8863553361102));
#204590=CARTESIAN_POINT('Ctrl Pts',(-16.6414519418388,19.5412570480063,
21.891090530439));
#204591=CARTESIAN_POINT('Ctrl Pts',(-16.6306364194547,19.4634279279486,
21.8958257247677));
#204592=CARTESIAN_POINT('Ctrl Pts',(-16.6241751632239,19.3851498151671,
21.9005609190965));
#204593=CARTESIAN_POINT('Ctrl Pts',(-16.618041130639,19.3108360165285,21.9050563044009));
#204594=CARTESIAN_POINT('Ctrl Pts',(-16.6158311432077,19.2361181121913,
21.9095516897054));
#204595=CARTESIAN_POINT('Ctrl Pts',(-16.6175804022592,19.1614309945752,
21.9140470750099));
#204596=CARTESIAN_POINT('Ctrl Pts',(-16.6193280165078,19.0868141041766,
21.9185382333685));
#204597=CARTESIAN_POINT('Ctrl Pts',(-16.6250274669155,19.0122283910569,
21.9230293917272));
#204598=CARTESIAN_POINT('Ctrl Pts',(-16.6346619440205,18.9381104129575,
21.9275205500858));
#204599=CARTESIAN_POINT('Ctrl Pts',(-16.644289879149,18.8640427622465,21.9320086588702));
#204600=CARTESIAN_POINT('Ctrl Pts',(-16.6578474702978,18.7904426603016,
21.9364967676547));
#204601=CARTESIAN_POINT('Ctrl Pts',(-16.6752660492705,18.7177419335545,
21.9409848764392));
#204602=CARTESIAN_POINT('Ctrl Pts',(-16.6926773473537,18.6450715953915,
21.9454711092139));
#204603=CARTESIAN_POINT('Ctrl Pts',(-16.7139463177063,18.5733003216091,
21.9499573419886));
#204604=CARTESIAN_POINT('Ctrl Pts',(-16.7389533863518,18.5028488795668,
21.9544435747634));
#204605=CARTESIAN_POINT('Ctrl Pts',(-16.7639635634828,18.432388680109,21.958930365196));
#204606=CARTESIAN_POINT('Ctrl Pts',(-16.7927126236932,18.363249066819,21.9634171556287));
#204607=CARTESIAN_POINT('Ctrl Pts',(-16.8250316763889,18.2958339279402,
21.9679039460613));
#204608=CARTESIAN_POINT('Ctrl Pts',(-16.8573522841798,18.2284155452484,
21.9723909523848));
#204609=CARTESIAN_POINT('Ctrl Pts',(-16.8932430249613,18.1627222047342,
21.9768779587083));
#204610=CARTESIAN_POINT('Ctrl Pts',(-16.9324883220855,18.0991345970228,
21.9813649650317));
#204611=CARTESIAN_POINT('Ctrl Pts',(-16.9717607058636,18.0355031018739,
21.9858550682355));
#204612=CARTESIAN_POINT('Ctrl Pts',(-17.0143920255779,17.9739806203857,
21.9903451714393));
#204613=CARTESIAN_POINT('Ctrl Pts',(-17.0601229488358,17.9149195173194,
21.994835274643));
#204614=CARTESIAN_POINT('Ctrl Pts',(-17.0776568931743,17.8922745755608,
21.996556849762));
#204615=CARTESIAN_POINT('Ctrl Pts',(-17.0956460703827,17.8699911414134,
21.998278424881));
#204616=CARTESIAN_POINT('Ctrl Pts',(-17.1140743056111,17.8480877707428,
22.));
#204617=CARTESIAN_POINT('Origin',(18.734,19.211,0.));
#204618=CARTESIAN_POINT('',(17.1140599594606,17.8481048224249,21.9999997809097));
#204619=CARTESIAN_POINT('Ctrl Pts',(17.1140599594606,17.8481048224249,21.9999997809097));
#204620=CARTESIAN_POINT('Ctrl Pts',(17.1607068911252,17.7926601825033,21.9956147575322));
#204621=CARTESIAN_POINT('Ctrl Pts',(17.2102952620655,17.739504224746,21.9912297341546));
#204622=CARTESIAN_POINT('Ctrl Pts',(17.2625716911555,17.6889659228745,21.9868447107771));
#204623=CARTESIAN_POINT('Ctrl Pts',(17.3147705007786,17.6385026597179,21.9824661982341));
#204624=CARTESIAN_POINT('Ctrl Pts',(17.3696491012488,17.5906496701831,21.9780876856911));
#204625=CARTESIAN_POINT('Ctrl Pts',(17.4269143514077,17.5457023967939,21.9737091731481));
#204626=CARTESIAN_POINT('Ctrl Pts',(17.4841122081179,17.5008080202619,21.9693358135217));
#204627=CARTESIAN_POINT('Ctrl Pts',(17.5436907567674,17.4588128636585,21.9649624538953));
#204628=CARTESIAN_POINT('Ctrl Pts',(17.605321823504,17.4199738768232,21.960589094269));
#204629=CARTESIAN_POINT('Ctrl Pts',(17.6669138937314,17.3811594650113,21.956218501847));
#204630=CARTESIAN_POINT('Ctrl Pts',(17.7305554975065,17.3454975176011,21.951847909425));
#204631=CARTESIAN_POINT('Ctrl Pts',(17.7958885256649,17.3132023654455,21.947477317003));
#204632=CARTESIAN_POINT('Ctrl Pts',(17.8612018513836,17.2809169525184,21.9431080426178));
#204633=CARTESIAN_POINT('Ctrl Pts',(17.9282051559123,17.2519965330214,21.9387387682326));
#204634=CARTESIAN_POINT('Ctrl Pts',(17.9965162100301,17.2266092472671,21.9343694938474));
#204635=CARTESIAN_POINT('Ctrl Pts',(18.0648292857548,17.2012212101981,21.9300000901573));
#204636=CARTESIAN_POINT('Ctrl Pts',(18.1344497342609,17.179366680706,21.9256306864672));
#204637=CARTESIAN_POINT('Ctrl Pts',(18.2049774492685,17.1611648503313,21.9212612827771));
#204638=CARTESIAN_POINT('Ctrl Pts',(18.275576959088,17.142944491113,21.9168874311828));
#204639=CARTESIAN_POINT('Ctrl Pts',(18.3470851103194,17.1283843746466,21.9125135795885));
#204640=CARTESIAN_POINT('Ctrl Pts',(18.4190896618186,17.1175529672556,21.9081397279943));
#204641=CARTESIAN_POINT('Ctrl Pts',(18.4911340360637,17.1067155694601,21.9037634574032));
#204642=CARTESIAN_POINT('Ctrl Pts',(18.5636748760598,17.0996110331389,21.8993871868121));
#204643=CARTESIAN_POINT('Ctrl Pts',(18.6362955339105,17.0962558458986,21.895010916221));
#204644=CARTESIAN_POINT('Ctrl Pts',(18.7090403295018,17.0928949233017,21.8906271648337));
#204645=CARTESIAN_POINT('Ctrl Pts',(18.7818647321215,17.0932961427629,21.8862434134464));
#204646=CARTESIAN_POINT('Ctrl Pts',(18.8543534992707,17.0974238752263,21.8818596620591));
#204647=CARTESIAN_POINT('Ctrl Pts',(18.8963594228442,17.0998158211955,21.879319357775));
#204648=CARTESIAN_POINT('Ctrl Pts',(18.9382527448405,17.103458157136,21.8767790534908));
#204649=CARTESIAN_POINT('Ctrl Pts',(18.9799541720406,17.1083360836178,21.8742387492067));
#204650=CARTESIAN_POINT('Ctrl Pts',(19.0521148556278,17.1167769100605,21.8698429741465));
#204651=CARTESIAN_POINT('Ctrl Pts',(19.1239758590327,17.1289525413789,21.8654471990862));
#204652=CARTESIAN_POINT('Ctrl Pts',(19.1951213352851,17.1448305698358,21.861051424026));
#204653=CARTESIAN_POINT('Ctrl Pts',(19.2661639857042,17.1606856499397,21.8566620021347));
#204654=CARTESIAN_POINT('Ctrl Pts',(19.3364926969102,17.1802323993941,21.8522725802435));
#204655=CARTESIAN_POINT('Ctrl Pts',(19.4056979848776,17.2033867859791,21.8478831583522));
#204656=CARTESIAN_POINT('Ctrl Pts',(19.4748252563206,17.2265150701546,21.8434986847453));
#204657=CARTESIAN_POINT('Ctrl Pts',(19.5428311670215,17.2532427601722,21.8391142111383));
#204658=CARTESIAN_POINT('Ctrl Pts',(19.6093192809603,17.2834354339272,21.8347297375313));
#204659=CARTESIAN_POINT('Ctrl Pts',(19.6757671116488,17.3136098148032,21.8303479203518));
#204660=CARTESIAN_POINT('Ctrl Pts',(19.7406985339571,17.3472448153046,21.8259661031722));
#204661=CARTESIAN_POINT('Ctrl Pts',(19.8037363887647,17.3841576262434,21.8215842859927));
#204662=CARTESIAN_POINT('Ctrl Pts',(19.8667566375372,17.4210601276904,21.8172036926242));
#204663=CARTESIAN_POINT('Ctrl Pts',(19.9278839545639,17.4612383791652,21.8128230992558));
#204664=CARTESIAN_POINT('Ctrl Pts',(19.9867665975567,17.5044640783018,21.8084425058873));
#204665=CARTESIAN_POINT('Ctrl Pts',(20.0456520241437,17.5476918208727,21.8040617054325));
#204666=CARTESIAN_POINT('Ctrl Pts',(20.1022921799,17.5939670112651,21.7996809049776));
#204667=CARTESIAN_POINT('Ctrl Pts',(20.156366438267,17.6430195424395,21.7953001045228));
#204668=CARTESIAN_POINT('Ctrl Pts',(20.2104978161903,17.6921238886346,21.7909146765541));
#204669=CARTESIAN_POINT('Ctrl Pts',(20.2620575288253,17.7440111093862,21.7865292485854));
#204670=CARTESIAN_POINT('Ctrl Pts',(20.3107606507593,17.7983730675734,21.7821438206167));
#204671=CARTESIAN_POINT('Ctrl Pts',(20.3594910179605,17.8527654366668,21.777755939373));
#204672=CARTESIAN_POINT('Ctrl Pts',(20.4053613108282,17.9096349255095,21.7733680581292));
#204673=CARTESIAN_POINT('Ctrl Pts',(20.4481276048669,17.9686411330726,21.7689801768854));
#204674=CARTESIAN_POINT('Ctrl Pts',(20.4909696354496,18.0277518370932,21.7645845249669));
#204675=CARTESIAN_POINT('Ctrl Pts',(20.5306964282269,18.0890064129735,21.7601888730484));
#204676=CARTESIAN_POINT('Ctrl Pts',(20.56710831572,18.1520368737118,21.7557932211298));
#204677=CARTESIAN_POINT('Ctrl Pts',(20.5912144042082,18.1937654950115,21.7528831282617));
#204678=CARTESIAN_POINT('Ctrl Pts',(20.6138685324289,18.2362719576463,21.7499730353935));
#204679=CARTESIAN_POINT('Ctrl Pts',(20.6350243872034,18.2794446987657,21.7470629425253));
#204680=CARTESIAN_POINT('Ctrl Pts',(20.6668849874923,18.3444626081263,21.7426803587599));
#204681=CARTESIAN_POINT('Ctrl Pts',(20.6954698849173,18.4112469909798,21.7382977749946));
#204682=CARTESIAN_POINT('Ctrl Pts',(20.720580017359,18.4794339847767,21.7339151912293));
#204683=CARTESIAN_POINT('Ctrl Pts',(20.7456523700338,18.5475183869707,21.7295392013357));
#204684=CARTESIAN_POINT('Ctrl Pts',(20.7672601692967,18.6170007611369,21.7251632114421));
#204685=CARTESIAN_POINT('Ctrl Pts',(20.7852510315621,18.6874943118595,21.7207872215485));
#204686=CARTESIAN_POINT('Ctrl Pts',(20.8032203398046,18.7579034075081,21.7164164743267));
#204687=CARTESIAN_POINT('Ctrl Pts',(20.8175811995767,18.8293208069692,21.7120457271049));
#204688=CARTESIAN_POINT('Ctrl Pts',(20.8282305540802,18.9013431151147,21.7076749798831));
#204689=CARTESIAN_POINT('Ctrl Pts',(20.838873012161,18.9733187822846,21.7033070631165));
#204690=CARTESIAN_POINT('Ctrl Pts',(20.8458086628383,19.0458981036007,21.6989391463499));
#204691=CARTESIAN_POINT('Ctrl Pts',(20.848985506631,19.1186674123577,21.6945712295833));
#204692=CARTESIAN_POINT('Ctrl Pts',(20.8521613485358,19.1914137717031,21.6902046903359));
#204693=CARTESIAN_POINT('Ctrl Pts',(20.8515807156441,19.2643495165153,21.6858381510884));
#204694=CARTESIAN_POINT('Ctrl Pts',(20.8472435998573,19.3370574776133,21.681471611841));
#204695=CARTESIAN_POINT('Ctrl Pts',(20.8429064110345,19.4097666630956,21.6771049990621));
#204696=CARTESIAN_POINT('Ctrl Pts',(20.8348126445421,19.4822475744202,21.6727383862833));
#204697=CARTESIAN_POINT('Ctrl Pts',(20.8230142986461,19.5540863740405,21.6683717735044));
#204698=CARTESIAN_POINT('Ctrl Pts',(20.8112037407264,19.6259995312979,21.664000641009));
#204699=CARTESIAN_POINT('Ctrl Pts',(20.7956810261304,19.6972687714271,21.6596295085136));
#204700=CARTESIAN_POINT('Ctrl Pts',(20.7765494845939,19.7674895353779,21.6552583760183));
#204701=CARTESIAN_POINT('Ctrl Pts',(20.7574075663198,19.8377483862984,21.6508848726687));
#204702=CARTESIAN_POINT('Ctrl Pts',(20.7346530755002,19.906957168973,21.6465113693192));
#204703=CARTESIAN_POINT('Ctrl Pts',(20.7084387039386,19.9747282267858,21.6421378659696));
#204704=CARTESIAN_POINT('Ctrl Pts',(20.6821775964101,20.0426201093875,21.637756565374));
#204705=CARTESIAN_POINT('Ctrl Pts',(20.6524444880472,20.109068706537,21.6333752647783));
#204706=CARTESIAN_POINT('Ctrl Pts',(20.6194392664437,20.1737085605479,21.6289939641826));
#204707=CARTESIAN_POINT('Ctrl Pts',(20.5965714078508,20.2184946570858,21.6259583547363));
#204708=CARTESIAN_POINT('Ctrl Pts',(20.572133749745,20.2624129761557,21.6229227452901));
#204709=CARTESIAN_POINT('Ctrl Pts',(20.5462048156797,20.3053503579875,21.6198871358438));
#204710=CARTESIAN_POINT('Ctrl Pts',(20.5087128685692,20.3674356733592,21.6154977957915));
#204711=CARTESIAN_POINT('Ctrl Pts',(20.4679537734929,20.4277128557231,21.6111084557392));
#204712=CARTESIAN_POINT('Ctrl Pts',(20.4241273179606,20.4858171041695,21.6067191156869));
#204713=CARTESIAN_POINT('Ctrl Pts',(20.3803658487493,20.5438351950362,21.6023362841933));
#204714=CARTESIAN_POINT('Ctrl Pts',(20.3335463361778,20.5996863665837,21.5979534526998));
#204715=CARTESIAN_POINT('Ctrl Pts',(20.2839130339366,20.6530327968647,21.5935706212063));
#204716=CARTESIAN_POINT('Ctrl Pts',(20.2343380311571,20.70631656623,21.5891929378029));
#204717=CARTESIAN_POINT('Ctrl Pts',(20.1819561311663,20.7571010876826,21.5848152543996));
#204718=CARTESIAN_POINT('Ctrl Pts',(20.1270521616165,20.8050811381531,21.5804375709962));
#204719=CARTESIAN_POINT('Ctrl Pts',(20.0721830041647,20.8530307666663,21.5760626632818));
#204720=CARTESIAN_POINT('Ctrl Pts',(20.0147953122166,20.8981791359674,21.5716877555675));
#204721=CARTESIAN_POINT('Ctrl Pts',(19.9552101005245,20.9402584799205,21.5673128478531));
#204722=CARTESIAN_POINT('Ctrl Pts',(19.8956430411106,20.9823250046532,21.5629392729282));
#204723=CARTESIAN_POINT('Ctrl Pts',(19.8338801846224,21.0213240823263,21.5585656980033));
#204724=CARTESIAN_POINT('Ctrl Pts',(19.7702735544122,21.0570298265266,21.5541921230784));
#204725=CARTESIAN_POINT('Ctrl Pts',(19.7066653494861,21.0927364546977,21.5498184398764));
#204726=CARTESIAN_POINT('Ctrl Pts',(19.6412137015734,21.1251493532758,21.5454447566744));
#204727=CARTESIAN_POINT('Ctrl Pts',(19.574295917344,21.154088204713,21.5410710734725));
#204728=CARTESIAN_POINT('Ctrl Pts',(19.5073089059773,21.1830569936903,21.5366928656502));
#204729=CARTESIAN_POINT('Ctrl Pts',(19.4388531734526,21.2085443681914,21.5323146578279));
#204730=CARTESIAN_POINT('Ctrl Pts',(19.3693259569769,21.2304182153262,21.5279364500056));
#204731=CARTESIAN_POINT('Ctrl Pts',(19.2997608703362,21.2523039767335,21.523555857456));
#204732=CARTESIAN_POINT('Ctrl Pts',(19.2291236047978,21.270572171152,21.5191752649063));
#204733=CARTESIAN_POINT('Ctrl Pts',(19.1578238757517,21.2851413457966,21.5147946723567));
#204734=CARTESIAN_POINT('Ctrl Pts',(19.086398154594,21.2997362652946,21.5104063389627));
#204735=CARTESIAN_POINT('Ctrl Pts',(19.0143081093411,21.3106190398704,21.5060180055687));
#204736=CARTESIAN_POINT('Ctrl Pts',(18.9419703140981,21.3177599171367,21.5016296721748));
#204737=CARTESIAN_POINT('Ctrl Pts',(18.8929666481794,21.3225973491147,21.4986568911707));
#204738=CARTESIAN_POINT('Ctrl Pts',(18.8438493793155,21.3257186793944,21.4956841101665));
#204739=CARTESIAN_POINT('Ctrl Pts',(18.7947475234683,21.3271282424259,21.4927113291624));
#204740=CARTESIAN_POINT('Ctrl Pts',(18.7222522479351,21.3292093584771,21.4883222368506));
#204741=CARTESIAN_POINT('Ctrl Pts',(18.6495090705527,21.3275648456576,21.4839331445389));
#204742=CARTESIAN_POINT('Ctrl Pts',(18.576932849213,21.3221652967363,21.4795440522271));
#204743=CARTESIAN_POINT('Ctrl Pts',(18.5044639937146,21.3167737356532,21.4751614529316));
#204744=CARTESIAN_POINT('Ctrl Pts',(18.4321620808264,21.3076382016009,21.4707788536361));
#204745=CARTESIAN_POINT('Ctrl Pts',(18.3604433424476,21.2947812801727,21.4663962543406));
#204746=CARTESIAN_POINT('Ctrl Pts',(18.2888084484159,21.2819393894075,21.4620187786179));
#204747=CARTESIAN_POINT('Ctrl Pts',(18.2177558467876,21.2653848384199,21.4576413028952));
#204748=CARTESIAN_POINT('Ctrl Pts',(18.1476963129808,21.2451919738775,21.4532638271725));
#204749=CARTESIAN_POINT('Ctrl Pts',(18.0776809591945,21.2250118430934,21.4488891119159));
#204750=CARTESIAN_POINT('Ctrl Pts',(18.0086578928418,21.2011980843124,21.4445143966593));
#204751=CARTESIAN_POINT('Ctrl Pts',(17.9410259701971,21.1738757444266,21.4401396814027));
#204752=CARTESIAN_POINT('Ctrl Pts',(17.8734144117325,21.1465616313814,21.4357662833863));
#204753=CARTESIAN_POINT('Ctrl Pts',(17.8071936121441,21.1157412151327,21.43139288537));
#204754=CARTESIAN_POINT('Ctrl Pts',(17.7427439864028,21.0815882805972,21.4270194873536));
#204755=CARTESIAN_POINT('Ctrl Pts',(17.6782925308258,21.0474343764011,21.4226459651689));
#204756=CARTESIAN_POINT('Ctrl Pts',(17.6156127740304,21.0099479935908,21.4182724429842));
#204757=CARTESIAN_POINT('Ctrl Pts',(17.5550604887456,20.9693488359262,21.4138989207996));
#204758=CARTESIAN_POINT('Ctrl Pts',(17.4944452020835,20.9287074370344,21.4095208482016));
#204759=CARTESIAN_POINT('Ctrl Pts',(17.4359622076729,20.8849470661681,21.4051427756037));
#204760=CARTESIAN_POINT('Ctrl Pts',(17.3799375246599,20.8383302716031,21.4007647030058));
#204761=CARTESIAN_POINT('Ctrl Pts',(17.3238821429895,20.7916879334218,21.3963842314483));
#204762=CARTESIAN_POINT('Ctrl Pts',(17.2702881090797,20.742186382646,21.3920037598908));
#204763=CARTESIAN_POINT('Ctrl Pts',(17.2194455880258,20.690126070749,21.3876232883333));
#204764=CARTESIAN_POINT('Ctrl Pts',(17.1685129377324,20.6379734708179,21.3832350514533));
#204765=CARTESIAN_POINT('Ctrl Pts',(17.1203418596204,20.5832534138692,21.3788468145733));
#204766=CARTESIAN_POINT('Ctrl Pts',(17.0751827508733,20.5263000927544,21.3744585776934));
#204767=CARTESIAN_POINT('Ctrl Pts',(17.0445738577713,20.4876970696618,21.3714842259559));
#204768=CARTESIAN_POINT('Ctrl Pts',(17.0153478403718,20.4480687194866,21.3685098742184));
#204769=CARTESIAN_POINT('Ctrl Pts',(16.9875709596013,20.4075260577406,21.3655355224809));
#204770=CARTESIAN_POINT('Ctrl Pts',(16.9460065700333,20.3468593831467,21.3610848026413));
#204771=CARTESIAN_POINT('Ctrl Pts',(16.9075294235406,20.2839114919535,21.3566340828016));
#204772=CARTESIAN_POINT('Ctrl Pts',(16.8723942149818,20.2190242562492,21.3521833629619));
#204773=CARTESIAN_POINT('Ctrl Pts',(16.837324103298,20.1542572405875,21.3477408892083));
#204774=CARTESIAN_POINT('Ctrl Pts',(16.8055838414173,20.0875584275687,21.3432984154547));
#204775=CARTESIAN_POINT('Ctrl Pts',(16.7773850294157,20.0192987423505,21.3388559417011));
#204776=CARTESIAN_POINT('Ctrl Pts',(16.7661659358305,19.9921411515798,21.3370884726039));
#204777=CARTESIAN_POINT('Ctrl Pts',(16.7555069324745,19.9647368036015,21.3353210035066));
#204778=CARTESIAN_POINT('Ctrl Pts',(16.7454193623258,19.9371102171621,21.3335535344094));
#204779=CARTESIAN_POINT('',(20.3539256943888,17.8480877707428,22.));
#204780=CARTESIAN_POINT('Origin',(18.734,19.211,22.));
#204781=CARTESIAN_POINT('Ctrl Pts',(16.7454193623258,19.9371102171621,21.5555703650724));
#204782=CARTESIAN_POINT('Ctrl Pts',(16.7701108524687,20.0047322090483,21.5598847289556));
#204783=CARTESIAN_POINT('Ctrl Pts',(16.7982600312914,20.0711052106196,21.5641990928389));
#204784=CARTESIAN_POINT('Ctrl Pts',(16.8297061648234,20.1358534961323,21.5685134567221));
#204785=CARTESIAN_POINT('Ctrl Pts',(16.8611789881103,20.2006567364418,21.572831482401));
#204786=CARTESIAN_POINT('Ctrl Pts',(16.8959541394072,20.2638320578116,21.5771495080799));
#204787=CARTESIAN_POINT('Ctrl Pts',(16.9338240862002,20.3250267857529,21.5814675337588));
#204788=CARTESIAN_POINT('Ctrl Pts',(16.9717095022942,20.3862465108161,21.585787323286));
#204789=CARTESIAN_POINT('Ctrl Pts',(17.0126919480371,20.4454836225521,21.5901071128131));
#204790=CARTESIAN_POINT('Ctrl Pts',(17.0565211461299,20.5024153843046,21.5944269023403));
#204791=CARTESIAN_POINT('Ctrl Pts',(17.100427118034,20.5594468710926,21.5987542586658));
#204792=CARTESIAN_POINT('Ctrl Pts',(17.1471894784021,20.6141645643789,21.6030816149914));
#204793=CARTESIAN_POINT('Ctrl Pts',(17.1965188056852,20.6662802400666,21.6074089713169));
#204794=CARTESIAN_POINT('Ctrl Pts',(17.2385583582755,20.7106943808936,21.6110968408632));
#204795=CARTESIAN_POINT('Ctrl Pts',(17.2824614855129,20.7532192292081,21.6147847104095));
#204796=CARTESIAN_POINT('Ctrl Pts',(17.3280304725231,20.7936998097575,21.6184725799557));
#204797=CARTESIAN_POINT('Ctrl Pts',(17.3823193345552,20.8419265709082,21.62286614352));
#204798=CARTESIAN_POINT('Ctrl Pts',(17.4391954779977,20.8874483717554,21.6272597070843));
#204799=CARTESIAN_POINT('Ctrl Pts',(17.4983585908499,20.9299762383447,21.6316532706486));
#204800=CARTESIAN_POINT('Ctrl Pts',(17.5574354044305,20.9724420709446,21.6360404254673));
#204801=CARTESIAN_POINT('Ctrl Pts',(17.618792177104,21.011922361068,21.6404275802861));
#204802=CARTESIAN_POINT('Ctrl Pts',(17.6820942417089,21.0481671877306,21.6448147351048));
#204803=CARTESIAN_POINT('Ctrl Pts',(17.7453238390215,21.0843705218375,21.6491968675719));
#204804=CARTESIAN_POINT('Ctrl Pts',(17.8104938888271,21.1173455129229,21.6535790000389));
#204805=CARTESIAN_POINT('Ctrl Pts',(17.877240743402,21.1468854760118,21.657961132506));
#204806=CARTESIAN_POINT('Ctrl Pts',(17.9439464566845,21.1764072313176,21.662340563923));
#204807=CARTESIAN_POINT('Ctrl Pts',(18.0122266074123,21.2024979658372,21.6667199953401));
#204808=CARTESIAN_POINT('Ctrl Pts',(18.0816942022227,21.2249975536693,21.6710994267571));
#204809=CARTESIAN_POINT('Ctrl Pts',(18.1511417219742,21.2474906394691,21.6754775925863));
#204810=CARTESIAN_POINT('Ctrl Pts',(18.2217755472184,21.2663944910457,21.6798557584155));
#204811=CARTESIAN_POINT('Ctrl Pts',(18.293191587477,21.2815982090809,21.6842339242447));
#204812=CARTESIAN_POINT('Ctrl Pts',(18.3646103699648,21.2968025109076,21.6886122581865));
#204813=CARTESIAN_POINT('Ctrl Pts',(18.4368109563362,21.3083062989017,21.6929905921282));
#204814=CARTESIAN_POINT('Ctrl Pts',(18.5093787087695,21.3160497085641,21.69736892607));
#204815=CARTESIAN_POINT('Ctrl Pts',(18.5820224137337,21.3238012228122,21.7017518425644));
#204816=CARTESIAN_POINT('Ctrl Pts',(18.6550335728178,21.3277844496845,21.7061347590588));
#204817=CARTESIAN_POINT('Ctrl Pts',(18.7279928778285,21.3279914771872,21.7105176755531));
#204818=CARTESIAN_POINT('Ctrl Pts',(18.8009925375781,21.3281986191995,21.7149030162955));
#204819=CARTESIAN_POINT('Ctrl Pts',(18.8739398055028,21.324625426611,21.7192883570379));
#204820=CARTESIAN_POINT('Ctrl Pts',(18.9464185362624,21.3173160649466,21.7236736977803));
#204821=CARTESIAN_POINT('Ctrl Pts',(19.0190253583242,21.3099937854836,21.7280667887137));
#204822=CARTESIAN_POINT('Ctrl Pts',(19.0911615138916,21.2989222240549,21.7324598796471));
#204823=CARTESIAN_POINT('Ctrl Pts',(19.1624196844615,21.2841969452915,21.7368529705805));
#204824=CARTESIAN_POINT('Ctrl Pts',(19.2099750592608,21.2743697753681,21.7397847759327));
#204825=CARTESIAN_POINT('Ctrl Pts',(19.2571396374613,21.2629163751623,21.7427165812849));
#204826=CARTESIAN_POINT('Ctrl Pts',(19.3037966250894,21.2498773396251,21.7456483866371));
#204827=CARTESIAN_POINT('Ctrl Pts',(19.3728942477398,21.2305669125471,21.7499903038977));
#204828=CARTESIAN_POINT('Ctrl Pts',(19.4411602368598,21.2076975140762,21.7543322211583));
#204829=CARTESIAN_POINT('Ctrl Pts',(19.5081959039851,21.1813577599646,21.7586741384189));
#204830=CARTESIAN_POINT('Ctrl Pts',(19.5751306276509,21.1550576687074,21.7630095175459));
#204831=CARTESIAN_POINT('Ctrl Pts',(19.6408382497924,21.1252977672376,21.7673448966729));
#204832=CARTESIAN_POINT('Ctrl Pts',(19.7049335619748,21.0922168982419,21.7716802757999));
#204833=CARTESIAN_POINT('Ctrl Pts',(19.7689552079216,21.0591740498597,21.7760106721746));
#204834=CARTESIAN_POINT('Ctrl Pts',(19.8313677860799,21.0228180350837,21.7803410685494));
#204835=CARTESIAN_POINT('Ctrl Pts',(19.8918061585171,20.9833357185646,21.7846714649241));
#204836=CARTESIAN_POINT('Ctrl Pts',(19.9522073873422,20.9438776666937,21.7889991999671));
#204837=CARTESIAN_POINT('Ctrl Pts',(20.0106364037878,20.9012973912839,21.79332693501));
#204838=CARTESIAN_POINT('Ctrl Pts',(20.0667541884382,20.8558268216443,21.797654670053));
#204839=CARTESIAN_POINT('Ctrl Pts',(20.1228569262381,20.8103684440195,21.8019812447012));
#204840=CARTESIAN_POINT('Ctrl Pts',(20.1766492784224,20.7620216199763,21.8063078193494));
#204841=CARTESIAN_POINT('Ctrl Pts',(20.2278241391937,20.7110594792081,21.8106343939976));
#204842=CARTESIAN_POINT('Ctrl Pts',(20.2790030075947,20.6600933474689,21.8149613074705));
#204843=CARTESIAN_POINT('Ctrl Pts',(20.3275636296709,20.6065118422404,21.8192882209435));
#204844=CARTESIAN_POINT('Ctrl Pts',(20.3732360242913,20.550624670072,21.8236151344164));
#204845=CARTESIAN_POINT('Ctrl Pts',(20.4189632278337,20.4946704307904,21.8279472403796));
#204846=CARTESIAN_POINT('Ctrl Pts',(20.4617949724119,20.436405384436,21.8322793463428));
#204847=CARTESIAN_POINT('Ctrl Pts',(20.5015024142213,20.3761713246222,21.836611452306));
#204848=CARTESIAN_POINT('Ctrl Pts',(20.541234362149,20.3159000903411,21.8409462319015));
#204849=CARTESIAN_POINT('Ctrl Pts',(20.5778379231948,20.253657851612,21.845281011497));
#204850=CARTESIAN_POINT('Ctrl Pts',(20.6111298851782,20.1898117255995,21.8496157910926));
#204851=CARTESIAN_POINT('Ctrl Pts',(20.6444888929844,20.1258370215219,21.8539593003889));
#204852=CARTESIAN_POINT('Ctrl Pts',(20.6745227819993,20.0602524303901,21.8583028096851));
#204853=CARTESIAN_POINT('Ctrl Pts',(20.7010964440932,19.9934452566384,21.8626463189814));
#204854=CARTESIAN_POINT('Ctrl Pts',(20.7218525789006,19.9412635626139,21.8660389437605));
#204855=CARTESIAN_POINT('Ctrl Pts',(20.7404986559915,19.8883364226189,21.8694315685395));
#204856=CARTESIAN_POINT('Ctrl Pts',(20.7569919001287,19.8348531654274,21.8728241933186));
#204857=CARTESIAN_POINT('Ctrl Pts',(20.7789190860527,19.7637490627714,21.8773345682141));
#204858=CARTESIAN_POINT('Ctrl Pts',(20.7971283710036,19.6913742316258,21.8818449431095));
#204859=CARTESIAN_POINT('Ctrl Pts',(20.8114804792732,19.6181410790364,21.886355318005));
#204860=CARTESIAN_POINT('Ctrl Pts',(20.8265479701327,19.54125761101,21.8910905130881));
#204861=CARTESIAN_POINT('Ctrl Pts',(20.8373635164913,19.4634284696821,21.8958257081712));
#204862=CARTESIAN_POINT('Ctrl Pts',(20.8438247940449,19.3851503328552,21.9005609032544));
#204863=CARTESIAN_POINT('Ctrl Pts',(20.8499588376022,19.3108366237006,21.9050562824811));
#204864=CARTESIAN_POINT('Ctrl Pts',(20.8521688454906,19.2361188075755,21.9095516617078));
#204865=CARTESIAN_POINT('Ctrl Pts',(20.8504196160406,19.1614317759201,21.9140470409345));
#204866=CARTESIAN_POINT('Ctrl Pts',(20.8486720313618,19.0868149712324,21.9185381932313));
#204867=CARTESIAN_POINT('Ctrl Pts',(20.8429726196327,19.0122293415783,21.923029345528));
#204868=CARTESIAN_POINT('Ctrl Pts',(20.8333381899733,18.9381114437731,21.9275204978248));
#204869=CARTESIAN_POINT('Ctrl Pts',(20.823710302195,18.8640438728158,21.9320086005809));
#204870=CARTESIAN_POINT('Ctrl Pts',(20.8101527670998,18.7904438474655,21.9364967033371));
#204871=CARTESIAN_POINT('Ctrl Pts',(20.7927342525461,18.7177431932619,21.9409848060932));
#204872=CARTESIAN_POINT('Ctrl Pts',(20.7753230186655,18.6450729268217,21.945471032891));
#204873=CARTESIAN_POINT('Ctrl Pts',(20.7540541207903,18.5733017207355,21.9499572596887));
#204874=CARTESIAN_POINT('Ctrl Pts',(20.7290471325623,18.502850341485,21.9544434864864));
#204875=CARTESIAN_POINT('Ctrl Pts',(20.7040370351564,18.432390202848,21.9589302710673));
#204876=CARTESIAN_POINT('Ctrl Pts',(20.6752880624039,18.3632506455487,21.9634170556482));
#204877=CARTESIAN_POINT('Ctrl Pts',(20.6429691045691,18.2958355569623,21.9679038402291));
#204878=CARTESIAN_POINT('Ctrl Pts',(20.6106485910926,18.228417223416,21.9723908407771));
#204879=CARTESIAN_POINT('Ctrl Pts',(20.5747579519087,18.1627239264085,21.976877841325));
#204880=CARTESIAN_POINT('Ctrl Pts',(20.5355127633241,18.099136355671,21.9813648418729));
#204881=CARTESIAN_POINT('Ctrl Pts',(20.4962404866784,18.0355048951203,21.9858549394666));
#204882=CARTESIAN_POINT('Ctrl Pts',(20.4536092807961,17.9739824418484,21.9903450370603));
#204883=CARTESIAN_POINT('Ctrl Pts',(20.4078784777144,17.914921359699,21.994835134654));
#204884=CARTESIAN_POINT('Ctrl Pts',(20.3903440822918,17.892275783879,21.996556756436));
#204885=CARTESIAN_POINT('Ctrl Pts',(20.3723544291116,17.8699917351007,21.998278378218));
#204886=CARTESIAN_POINT('Ctrl Pts',(20.3539256943888,17.8480877707428,22.));
#204887=CARTESIAN_POINT('Origin',(18.734,-18.952,0.));
#204888=CARTESIAN_POINT('',(17.1140599642913,-20.3148951833168,21.9999997809128));
#204889=CARTESIAN_POINT('Ctrl Pts',(17.1140599642913,-20.3148951833168,
21.9999997809128));
#204890=CARTESIAN_POINT('Ctrl Pts',(17.1607068994597,-20.3703398270043,
21.9956147572469));
#204891=CARTESIAN_POINT('Ctrl Pts',(17.210295274204,-20.4234957880638,21.9912297335811));
#204892=CARTESIAN_POINT('Ctrl Pts',(17.2625717073312,-20.4740340927633,
21.9868447099152));
#204893=CARTESIAN_POINT('Ctrl Pts',(17.3147705210273,-20.5244973587843,
21.9824661970807));
#204894=CARTESIAN_POINT('Ctrl Pts',(17.3696491258074,-20.5723503507068,
21.9780876842462));
#204895=CARTESIAN_POINT('Ctrl Pts',(17.4269143804502,-20.6172976260014,
21.9737091714118));
#204896=CARTESIAN_POINT('Ctrl Pts',(17.4841122416856,-20.6621920044732,
21.9693358114907));
#204897=CARTESIAN_POINT('Ctrl Pts',(17.5436907950378,-20.7041871625307,
21.9649624515697));
#204898=CARTESIAN_POINT('Ctrl Pts',(17.605321866596,-20.7430261503327,21.9605890916486));
#204899=CARTESIAN_POINT('Ctrl Pts',(17.6669139416705,-20.7818405631288,
21.9562184989301));
#204900=CARTESIAN_POINT('Ctrl Pts',(17.7305555504131,-20.8175025110335,
21.9518479062116));
#204901=CARTESIAN_POINT('Ctrl Pts',(17.7958885836047,-20.8497976631951,
21.9474773134931));
#204902=CARTESIAN_POINT('Ctrl Pts',(17.8612019143776,-20.8820830761394,
21.94310803881));
#204903=CARTESIAN_POINT('Ctrl Pts',(17.9282052240273,-20.9110034951629,
21.9387387641268));
#204904=CARTESIAN_POINT('Ctrl Pts',(17.9965162832812,-20.9363907799561,
21.9343694894437));
#204905=CARTESIAN_POINT('Ctrl Pts',(18.0648293641575,-20.9617788160697,
21.9300000854546));
#204906=CARTESIAN_POINT('Ctrl Pts',(18.1344498178311,-20.9836333441171,
21.9256306814655));
#204907=CARTESIAN_POINT('Ctrl Pts',(18.2049775379727,-21.0018351725616,
21.9212612774765));
#204908=CARTESIAN_POINT('Ctrl Pts',(18.2755770529193,-21.0200555298444,
21.9168874255837));
#204909=CARTESIAN_POINT('Ctrl Pts',(18.347085209244,-21.0346156438901,21.912513573691));
#204910=CARTESIAN_POINT('Ctrl Pts',(18.4190897657556,-21.0454470483793,
21.9081397217982));
#204911=CARTESIAN_POINT('Ctrl Pts',(18.4911341450163,-21.0562844432714,
21.9037634509084));
#204912=CARTESIAN_POINT('Ctrl Pts',(18.5636749899472,-21.0633889762076,
21.8993871800187));
#204913=CARTESIAN_POINT('Ctrl Pts',(18.6362956526055,-21.0667441595853,
21.8950109091289));
#204914=CARTESIAN_POINT('Ctrl Pts',(18.7090404529568,-21.0701050783104,
21.8906271574457));
#204915=CARTESIAN_POINT('Ctrl Pts',(18.7818648602089,-21.0697038545041,
21.8862434057626));
#204916=CARTESIAN_POINT('Ctrl Pts',(18.8543536318168,-21.0655761172261,
21.8818596540794));
#204917=CARTESIAN_POINT('Ctrl Pts',(18.896359511156,-21.063184171133,21.8793193524552));
#204918=CARTESIAN_POINT('Ctrl Pts',(18.9382527891111,-21.0595418376991,
21.8767790508309));
#204919=CARTESIAN_POINT('Ctrl Pts',(18.979954172718,-21.054663916303,21.8742387492067));
#204920=CARTESIAN_POINT('Ctrl Pts',(19.0521148572584,-21.0462230897252,
21.8698429740959));
#204921=CARTESIAN_POINT('Ctrl Pts',(19.1239758615628,-21.0340474581782,
21.8654471989851));
#204922=CARTESIAN_POINT('Ctrl Pts',(19.1951213386526,-21.0181694294126,
21.8610514238743));
#204923=CARTESIAN_POINT('Ctrl Pts',(19.2661639899332,-21.0023143489949,
21.856662001931));
#204924=CARTESIAN_POINT('Ctrl Pts',(19.3364927019385,-20.9827675991443,
21.8522725799877));
#204925=CARTESIAN_POINT('Ctrl Pts',(19.4056979906368,-20.959613212094,21.8478831580444));
#204926=CARTESIAN_POINT('Ctrl Pts',(19.4748252628419,-20.936484927443,21.8434986843834));
#204927=CARTESIAN_POINT('Ctrl Pts',(19.5428311742357,-20.9097572368777,
21.8391142107225));
#204928=CARTESIAN_POINT('Ctrl Pts',(19.6093192887935,-20.8795645625156,
21.8347297370615));
#204929=CARTESIAN_POINT('Ctrl Pts',(19.675767120119,-20.8493901810247,21.8303479198267));
#204930=CARTESIAN_POINT('Ctrl Pts',(19.7406985429898,-20.8157551798471,
21.825966102592));
#204931=CARTESIAN_POINT('Ctrl Pts',(19.803736398282,-20.7788423681836,21.8215842853572));
#204932=CARTESIAN_POINT('Ctrl Pts',(19.8667566475552,-20.7419398660025,
21.8172036919325));
#204933=CARTESIAN_POINT('Ctrl Pts',(19.9278839650038,-20.7017616137434,
21.8128230985077));
#204934=CARTESIAN_POINT('Ctrl Pts',(19.9867666083377,-20.6585359137838,
21.808442505083));
#204935=CARTESIAN_POINT('Ctrl Pts',(20.0456520352798,-20.6153081703798,
21.8040617045708));
#204936=CARTESIAN_POINT('Ctrl Pts',(20.1022921913093,-20.5690329791144,
21.7996809040586));
#204937=CARTESIAN_POINT('Ctrl Pts',(20.1563664498668,-20.519980447038,21.7953001035464));
#204938=CARTESIAN_POINT('Ctrl Pts',(20.2104978279948,-20.4708760999272,
21.7909146755192));
#204939=CARTESIAN_POINT('Ctrl Pts',(20.2620575407503,-20.4189888782294,
21.786529247492));
#204940=CARTESIAN_POINT('Ctrl Pts',(20.3107606627202,-20.364626919076,21.7821438194648));
#204941=CARTESIAN_POINT('Ctrl Pts',(20.3594910299654,-20.3102345490068,
21.7777559381617));
#204942=CARTESIAN_POINT('Ctrl Pts',(20.4053613227915,-20.2533650591673,
21.7733680568587));
#204943=CARTESIAN_POINT('Ctrl Pts',(20.4481276167033,-20.1943588505964,
21.7689801755556));
#204944=CARTESIAN_POINT('Ctrl Pts',(20.4909696471634,-20.1352481455596,
21.7645845235772));
#204945=CARTESIAN_POINT('Ctrl Pts',(20.5306964397318,-20.0739935686515,
21.7601888715988));
#204946=CARTESIAN_POINT('Ctrl Pts',(20.5671083269304,-20.0109631068826,
21.7557932196204));
#204947=CARTESIAN_POINT('Ctrl Pts',(20.5912144107273,-19.969234492684,21.7528831272554));
#204948=CARTESIAN_POINT('Ctrl Pts',(20.613868534761,-19.9267280374392,21.7499730348904));
#204949=CARTESIAN_POINT('Ctrl Pts',(20.6350243858782,-19.8835553039387,
21.7470629425253));
#204950=CARTESIAN_POINT('Ctrl Pts',(20.6668849852277,-19.8185373967291,
21.7426803588893));
#204951=CARTESIAN_POINT('Ctrl Pts',(20.6954698819653,-19.7517530160599,
21.7382977752533));
#204952=CARTESIAN_POINT('Ctrl Pts',(20.7205800139613,-19.6835660244499,
21.7339151916173));
#204953=CARTESIAN_POINT('Ctrl Pts',(20.7456523661794,-19.6154816244714,
21.7295392018549));
#204954=CARTESIAN_POINT('Ctrl Pts',(20.7672601652298,-19.5459992525245,
21.7251632120926));
#204955=CARTESIAN_POINT('Ctrl Pts',(20.7852510275153,-19.4755057039971,
21.7207872223302));
#204956=CARTESIAN_POINT('Ctrl Pts',(20.8032203357683,-19.4050966105787,
21.7164164752418));
#204957=CARTESIAN_POINT('Ctrl Pts',(20.8175811957868,-19.3336792133251,
21.7120457281534));
#204958=CARTESIAN_POINT('Ctrl Pts',(20.8282305507602,-19.2616569073388,
21.707674981065));
#204959=CARTESIAN_POINT('Ctrl Pts',(20.8388730093072,-19.1896812423493,
21.7033070644331));
#204960=CARTESIAN_POINT('Ctrl Pts',(20.845808660676,-19.1171019231659,21.6989391478011));
#204961=CARTESIAN_POINT('Ctrl Pts',(20.8489855053725,-19.0443326164712,
21.6945712311692));
#204962=CARTESIAN_POINT('Ctrl Pts',(20.8521613481799,-18.9715862592065,
21.6902046920575));
#204963=CARTESIAN_POINT('Ctrl Pts',(20.8515807164049,-18.8986505164049,
21.6858381529459));
#204964=CARTESIAN_POINT('Ctrl Pts',(20.8472436019355,-18.8259425572265,
21.6814716138342));
#204965=CARTESIAN_POINT('Ctrl Pts',(20.8429064144311,-18.753233373679,21.677105001192));
#204966=CARTESIAN_POINT('Ctrl Pts',(20.8348126494595,-18.6807524641984,
21.6727383885499));
#204967=CARTESIAN_POINT('Ctrl Pts',(20.8230143052733,-18.6089136663121,
21.6683717759077));
#204968=CARTESIAN_POINT('Ctrl Pts',(20.8112037490663,-18.5370005107965,
21.6640006435495));
#204969=CARTESIAN_POINT('Ctrl Pts',(20.7956810363731,-18.4657312722987,
21.6596295111913));
#204970=CARTESIAN_POINT('Ctrl Pts',(20.7765494969166,-18.3955105098514,
21.6552583788331));
#204971=CARTESIAN_POINT('Ctrl Pts',(20.7574075807255,-18.3252516604421,
21.6508848756213));
#204972=CARTESIAN_POINT('Ctrl Pts',(20.734653092167,-18.2560428791505,21.6465113724094));
#204973=CARTESIAN_POINT('Ctrl Pts',(20.7084387230319,-18.1882718225755,
21.6421378691975));
#204974=CARTESIAN_POINT('Ctrl Pts',(20.6821776179286,-18.1203799411991,
21.6377565687388));
#204975=CARTESIAN_POINT('Ctrl Pts',(20.6524445121555,-18.0539313451297,
21.6333752682801));
#204976=CARTESIAN_POINT('Ctrl Pts',(20.619439293294,-17.9892914920377,21.6289939678214));
#204977=CARTESIAN_POINT('Ctrl Pts',(20.5965714267485,-17.9445053768408,
21.6259583571622));
#204978=CARTESIAN_POINT('Ctrl Pts',(20.57213375941,-17.9005870397827,21.622922746503));
#204979=CARTESIAN_POINT('Ctrl Pts',(20.546204814931,-17.8576496407728,21.6198871358438));
#204980=CARTESIAN_POINT('Ctrl Pts',(20.5087128672688,-17.7955643245834,
21.6154977957359));
#204981=CARTESIAN_POINT('Ctrl Pts',(20.4679537715697,-17.7352871414802,
21.6111084556279));
#204982=CARTESIAN_POINT('Ctrl Pts',(20.4241273153556,-17.6771828923768,
21.60671911552));
#204983=CARTESIAN_POINT('Ctrl Pts',(20.3803658454572,-17.6191648008458,
21.6023362839703));
#204984=CARTESIAN_POINT('Ctrl Pts',(20.3335463321389,-17.5633136287167,
21.5979534524206));
#204985=CARTESIAN_POINT('Ctrl Pts',(20.283913029103,-17.5099671979401,21.5935706208709));
#204986=CARTESIAN_POINT('Ctrl Pts',(20.2343380255226,-17.456683428072,21.5891929374108));
#204987=CARTESIAN_POINT('Ctrl Pts',(20.1819561246821,-17.4058989062031,
21.5848152539507));
#204988=CARTESIAN_POINT('Ctrl Pts',(20.1270521542449,-17.3579188554049,
21.5804375704906));
#204989=CARTESIAN_POINT('Ctrl Pts',(20.0721829959018,-17.3099692265604,
21.5760626627192));
#204990=CARTESIAN_POINT('Ctrl Pts',(20.0147953030245,-17.2648208570169,
21.5716877549478));
#204991=CARTESIAN_POINT('Ctrl Pts',(19.9552100903752,-17.222741512912,21.5673128471764));
#204992=CARTESIAN_POINT('Ctrl Pts',(19.8956430300011,-17.1806749880252,
21.5629392721942));
#204993=CARTESIAN_POINT('Ctrl Pts',(19.8338801725247,-17.1416759102888,
21.558565697212));
#204994=CARTESIAN_POINT('Ctrl Pts',(19.7702735413081,-17.1059701661173,
21.5541921222299));
#204995=CARTESIAN_POINT('Ctrl Pts',(19.7066653353733,-17.0702635379739,
21.5498184389705));
#204996=CARTESIAN_POINT('Ctrl Pts',(19.6412136864337,-17.0378506395157,
21.5454447557111));
#204997=CARTESIAN_POINT('Ctrl Pts',(19.5742959011684,-17.0089117882917,
21.5410710724518));
#204998=CARTESIAN_POINT('Ctrl Pts',(19.5073088887682,-16.9799429995295,
21.5366928645722));
#204999=CARTESIAN_POINT('Ctrl Pts',(19.4388531552012,-16.9544556253366,
21.5323146566927));
#205000=CARTESIAN_POINT('Ctrl Pts',(19.3693259376834,-16.9325817786039,
21.5279364488132));
#205001=CARTESIAN_POINT('Ctrl Pts',(19.2997608500006,-16.9106960175991,
21.5235558562063));
#205002=CARTESIAN_POINT('Ctrl Pts',(19.2291235834203,-16.8924278236772,
21.5191752635995));
#205003=CARTESIAN_POINT('Ctrl Pts',(19.1578238533414,-16.8778586496242,
21.5147946709926));
#205004=CARTESIAN_POINT('Ctrl Pts',(19.0863981311614,-16.8632637307212,
21.5104063375421));
#205005=CARTESIAN_POINT('Ctrl Pts',(19.0143080848955,-16.8523809568344,
21.5060180040915));
#205006=CARTESIAN_POINT('Ctrl Pts',(18.9419702886576,-16.8452400803519,
21.5016296706409));
#205007=CARTESIAN_POINT('Ctrl Pts',(18.8929666311248,-16.8404026497993,
21.4986568901481));
#205008=CARTESIAN_POINT('Ctrl Pts',(18.8438493706969,-16.8372813203535,
21.4956841096553));
#205009=CARTESIAN_POINT('Ctrl Pts',(18.7947475232676,-16.8358717575684,
21.4927113291624));
#205010=CARTESIAN_POINT('Ctrl Pts',(18.7222522474693,-16.8337906415164,
21.488322236837));
#205011=CARTESIAN_POINT('Ctrl Pts',(18.6495090698324,-16.8354351543627,
21.4839331445116));
#205012=CARTESIAN_POINT('Ctrl Pts',(18.5769328482517,-16.8408347033352,
21.4795440521862));
#205013=CARTESIAN_POINT('Ctrl Pts',(18.5044639925059,-16.8462262644699,
21.4751614528767));
#205014=CARTESIAN_POINT('Ctrl Pts',(18.4321620793838,-16.8553617985987,
21.4707788535672));
#205015=CARTESIAN_POINT('Ctrl Pts',(18.3604433407868,-16.868218720125,21.4663962542577));
#205016=CARTESIAN_POINT('Ctrl Pts',(18.2888084465286,-16.8810606109898,
21.4620187785205));
#205017=CARTESIAN_POINT('Ctrl Pts',(18.2177558446894,-16.8976151620993,
21.4576413027833));
#205018=CARTESIAN_POINT('Ctrl Pts',(18.1476963106892,-16.917808026783,21.4532638270461));
#205019=CARTESIAN_POINT('Ctrl Pts',(18.0776809567047,-16.9379881577097,
21.4488891117746));
#205020=CARTESIAN_POINT('Ctrl Pts',(18.0086578901714,-16.9618019166529,
21.4445143965032));
#205021=CARTESIAN_POINT('Ctrl Pts',(17.9410259673652,-16.9891242567175,
21.4401396812318));
#205022=CARTESIAN_POINT('Ctrl Pts',(17.8734144087345,-17.0164383699432,
21.4357662832003));
#205023=CARTESIAN_POINT('Ctrl Pts',(17.8071936089994,-17.0472587863894,
21.4313928851688));
#205024=CARTESIAN_POINT('Ctrl Pts',(17.7427439831315,-17.0814117211363,
21.4270194871373));
#205025=CARTESIAN_POINT('Ctrl Pts',(17.6782925274241,-17.1155656255459,
21.4226459649373));
#205026=CARTESIAN_POINT('Ctrl Pts',(17.6156127705188,-17.1530520085839,
21.4182724427373));
#205027=CARTESIAN_POINT('Ctrl Pts',(17.5550604851453,-17.1936511664877,
21.4138989205372));
#205028=CARTESIAN_POINT('Ctrl Pts',(17.4944451983905,-17.2342925656217,
21.4095208479236));
#205029=CARTESIAN_POINT('Ctrl Pts',(17.4359622039086,-17.2780529367419,
21.4051427753101));
#205030=CARTESIAN_POINT('Ctrl Pts',(17.3799375208465,-17.32466973157,21.4007647026965));
#205031=CARTESIAN_POINT('Ctrl Pts',(17.3238821391245,-17.3713120700164,
21.3963842311231));
#205032=CARTESIAN_POINT('Ctrl Pts',(17.2702881051855,-17.4208136210668,
21.3920037595497));
#205033=CARTESIAN_POINT('Ctrl Pts',(17.2194455841251,-17.4728739332451,
21.3876232879764));
#205034=CARTESIAN_POINT('Ctrl Pts',(17.1685129338239,-17.5250265334593,
21.3832350510804));
#205035=CARTESIAN_POINT('Ctrl Pts',(17.120341855727,-17.5797465906982,21.3788468141844));
#205036=CARTESIAN_POINT('Ctrl Pts',(17.0751827470182,-17.6366999121075,
21.3744585772885));
#205037=CARTESIAN_POINT('Ctrl Pts',(17.0445738554429,-17.6753029335071,
21.371484225686));
#205038=CARTESIAN_POINT('Ctrl Pts',(17.015347839445,-17.7149312818909,21.3685098740835));
#205039=CARTESIAN_POINT('Ctrl Pts',(16.9875709599417,-17.7554739417626,
21.365535522481));
#205040=CARTESIAN_POINT('Ctrl Pts',(16.9460065706275,-17.8161406159491,
21.3610848026675));
#205041=CARTESIAN_POINT('Ctrl Pts',(16.9075294243376,-17.8790885067208,
21.3566340828539));
#205042=CARTESIAN_POINT('Ctrl Pts',(16.8723942159318,-17.9439757419964,
21.3521833630404));
#205043=CARTESIAN_POINT('Ctrl Pts',(16.8373241044052,-18.0087427572218,
21.3477408893134));
#205044=CARTESIAN_POINT('Ctrl Pts',(16.8055838426314,-18.0754415697969,
21.3432984155865));
#205045=CARTESIAN_POINT('Ctrl Pts',(16.777385030688,-18.1437012545698,21.3388559418595));
#205046=CARTESIAN_POINT('Ctrl Pts',(16.7661659391973,-18.1708588401492,
21.3370884730992));
#205047=CARTESIAN_POINT('Ctrl Pts',(16.7555069377213,-18.1982631828448,
21.3353210043389));
#205048=CARTESIAN_POINT('Ctrl Pts',(16.7454193692319,-18.2258897639242,
21.3335535355786));
#205049=CARTESIAN_POINT('',(20.3539256943886,-20.3149122292574,22.));
#205050=CARTESIAN_POINT('Origin',(18.734,-18.952,22.));
#205051=CARTESIAN_POINT('Ctrl Pts',(16.7454193692319,-18.2258897639242,
21.5555703664997));
#205052=CARTESIAN_POINT('Ctrl Pts',(16.7701108597548,-18.1582677729935,
21.5598847303809));
#205053=CARTESIAN_POINT('Ctrl Pts',(16.7982600389245,-18.0918947722405,
21.5641990942621));
#205054=CARTESIAN_POINT('Ctrl Pts',(16.8297061728116,-18.0271464874196,
21.5685134581433));
#205055=CARTESIAN_POINT('Ctrl Pts',(16.861178996372,-17.9623432479715,21.572831483809));
#205056=CARTESIAN_POINT('Ctrl Pts',(16.8959541479334,-17.8991679273281,
21.5771495094746));
#205057=CARTESIAN_POINT('Ctrl Pts',(16.9338240950207,-17.8379731999939,
21.5814675351402));
#205058=CARTESIAN_POINT('Ctrl Pts',(16.9717095113551,-17.7767534756255,
21.5857873246479));
#205059=CARTESIAN_POINT('Ctrl Pts',(17.0126919573595,-17.7175163644594,
21.5901071141556));
#205060=CARTESIAN_POINT('Ctrl Pts',(17.0565211557699,-17.6605846031735,
21.5944269036633));
#205061=CARTESIAN_POINT('Ctrl Pts',(17.1004271278893,-17.6035531169866,
21.5987542599592));
#205062=CARTESIAN_POINT('Ctrl Pts',(17.1471894885155,-17.5488354241871,
21.6030816162551));
#205063=CARTESIAN_POINT('Ctrl Pts',(17.1965188161309,-17.4967197488976,
21.607408972551));
#205064=CARTESIAN_POINT('Ctrl Pts',(17.2385583646031,-17.45230561306,21.6110968416859));
#205065=CARTESIAN_POINT('Ctrl Pts',(17.2824614873855,-17.4097807692747,
21.6147847108208));
#205066=CARTESIAN_POINT('Ctrl Pts',(17.3280304696825,-17.3693001927659,
21.6184725799558));
#205067=CARTESIAN_POINT('Ctrl Pts',(17.3823193529476,-17.3210734125788,
21.6228661452028));
#205068=CARTESIAN_POINT('Ctrl Pts',(17.4391955190593,-17.2755515953447,
21.6272597104498));
#205069=CARTESIAN_POINT('Ctrl Pts',(17.4983586556721,-17.2330237150596,
21.6316532756968));
#205070=CARTESIAN_POINT('Ctrl Pts',(17.5574354931409,-17.1905578686671,
21.6360404322079));
#205071=CARTESIAN_POINT('Ctrl Pts',(17.6187922908035,-17.1510775674503,
21.640427588719));
#205072=CARTESIAN_POINT('Ctrl Pts',(17.6820943811751,-17.1148327324153,
21.64481474523));
#205073=CARTESIAN_POINT('Ctrl Pts',(17.7453240043386,-17.0786293898806,
21.6491968793954));
#205074=CARTESIAN_POINT('Ctrl Pts',(17.810494080778,-17.0456543930935,21.6535790135607));
#205075=CARTESIAN_POINT('Ctrl Pts',(17.8772409624661,-17.0161144270376,
21.6579611477261));
#205076=CARTESIAN_POINT('Ctrl Pts',(17.9439467029022,-16.9865926687415,
21.6623405808441));
#205077=CARTESIAN_POINT('Ctrl Pts',(18.0122268812651,-16.9605019339683,
21.6667200139621));
#205078=CARTESIAN_POINT('Ctrl Pts',(18.0816945039053,-16.9380023486199,
21.6710994470801));
#205079=CARTESIAN_POINT('Ctrl Pts',(18.1511420514884,-16.9155092652999,
21.6754776146104));
#205080=CARTESIAN_POINT('Ctrl Pts',(18.2217759047592,-16.8966054189395,
21.6798557821407));
#205081=CARTESIAN_POINT('Ctrl Pts',(18.2931919729642,-16.881401708853,21.684233949671));
#205082=CARTESIAN_POINT('Ctrl Pts',(18.364610783359,-16.866197414984,21.6886122853114));
#205083=CARTESIAN_POINT('Ctrl Pts',(18.4368113975566,-16.8546936376761,
21.6929906209519));
#205084=CARTESIAN_POINT('Ctrl Pts',(18.5093791774671,-16.8469502414231,
21.6973689565923));
#205085=CARTESIAN_POINT('Ctrl Pts',(18.5820229096485,-16.8391987406294,
21.7017518747697));
#205086=CARTESIAN_POINT('Ctrl Pts',(18.6550340955975,-16.8352155299105,
21.7061347929472));
#205087=CARTESIAN_POINT('Ctrl Pts',(18.7279934268567,-16.835008521255,21.7105177111246));
#205088=CARTESIAN_POINT('Ctrl Pts',(18.8009931127498,-16.8348013981006,
21.7149030535438));
#205089=CARTESIAN_POINT('Ctrl Pts',(18.8739404062014,-16.8383746122317,
21.719288395963));
#205090=CARTESIAN_POINT('Ctrl Pts',(18.9464191616025,-16.845683998118,21.7236737383821));
#205091=CARTESIAN_POINT('Ctrl Pts',(19.019026007826,-16.8530063017931,21.7280668309636));
#205092=CARTESIAN_POINT('Ctrl Pts',(19.0911621866738,-16.8640778900689,
21.7324599235451));
#205093=CARTESIAN_POINT('Ctrl Pts',(19.1624203793687,-16.8788031983091,
21.7368530161266));
#205094=CARTESIAN_POINT('Ctrl Pts',(19.2099755048328,-16.8886303333286,
21.7397848062968));
#205095=CARTESIAN_POINT('Ctrl Pts',(19.2571398375277,-16.9000836817304,
21.742716596467));
#205096=CARTESIAN_POINT('Ctrl Pts',(19.3037965853284,-16.9131226492631,
21.7456483866372));
#205097=CARTESIAN_POINT('Ctrl Pts',(19.3728941566259,-16.932433060537,21.7499903005052));
#205098=CARTESIAN_POINT('Ctrl Pts',(19.4411600971652,-16.9553024383045,
21.7543322143732));
#205099=CARTESIAN_POINT('Ctrl Pts',(19.5081957188875,-16.9816421673066,
21.7586741282413));
#205100=CARTESIAN_POINT('Ctrl Pts',(19.5751303969638,-17.007942233392,21.7630095039643));
#205101=CARTESIAN_POINT('Ctrl Pts',(19.6408379766924,-17.0377021052713,
21.7673448796873));
#205102=CARTESIAN_POINT('Ctrl Pts',(19.7049332499917,-17.0707829407374,
21.7716802554104));
#205103=CARTESIAN_POINT('Ctrl Pts',(19.7689548569736,-17.1038257555634,
21.7760106483765));
#205104=CARTESIAN_POINT('Ctrl Pts',(19.8313673996942,-17.1401817328403,
21.7803410413427));
#205105=CARTESIAN_POINT('Ctrl Pts',(19.8918057405323,-17.1796640083804,
21.7846714343088));
#205106=CARTESIAN_POINT('Ctrl Pts',(19.9522069377095,-17.2191220192527,
21.7889991659403));
#205107=CARTESIAN_POINT('Ctrl Pts',(20.0106359263449,-17.2617022501812,
21.7933268975719));
#205108=CARTESIAN_POINT('Ctrl Pts',(20.0667536873044,-17.307172772302,21.7976546292034));
#205109=CARTESIAN_POINT('Ctrl Pts',(20.1228564014125,-17.3526311024149,
21.8019812004406));
#205110=CARTESIAN_POINT('Ctrl Pts',(20.1766487340221,-17.4009778759096,
21.8063077716777));
#205111=CARTESIAN_POINT('Ctrl Pts',(20.2278235795987,-17.4519399635232,
21.8106343429149));
#205112=CARTESIAN_POINT('Ctrl Pts',(20.2790024328481,-17.5029060421478,
21.8149612529802));
#205113=CARTESIAN_POINT('Ctrl Pts',(20.3275630441483,-17.5564874916594,
21.8192881630456));
#205114=CARTESIAN_POINT('Ctrl Pts',(20.3732354326212,-17.6123746059293,
21.823615073111));
#205115=CARTESIAN_POINT('Ctrl Pts',(20.4189626303271,-17.6683287876325,
21.8279471756927));
#205116=CARTESIAN_POINT('Ctrl Pts',(20.4617943736678,-17.7265937742531,
21.8322792782743));
#205117=CARTESIAN_POINT('Ctrl Pts',(20.5015018190868,-17.7868277725912,
21.836611380856));
#205118=CARTESIAN_POINT('Ctrl Pts',(20.5412337707152,-17.8470989454934,
21.8409461570777));
#205119=CARTESIAN_POINT('Ctrl Pts',(20.5778373403004,-17.9093411211074,
21.8452809332993));
#205120=CARTESIAN_POINT('Ctrl Pts',(20.6111293159145,-17.973187182688,21.8496157095209));
#205121=CARTESIAN_POINT('Ctrl Pts',(20.6444883378172,-18.0371618230444,
21.8539592154936));
#205122=CARTESIAN_POINT('Ctrl Pts',(20.674522245953,-18.1027463491743,21.8583027214662));
#205123=CARTESIAN_POINT('Ctrl Pts',(20.7010959324481,-18.1695534570681,
21.8626462274389));
#205124=CARTESIAN_POINT('Ctrl Pts',(20.7218522888838,-18.2217356089171,
21.8660388827321));
#205125=CARTESIAN_POINT('Ctrl Pts',(20.7404985496073,-18.2746632207694,
21.8694315380253));
#205126=CARTESIAN_POINT('Ctrl Pts',(20.7569919383483,-18.3281469585088,
21.8728241933186));
#205127=CARTESIAN_POINT('Ctrl Pts',(20.7789191314163,-18.3992510998001,
21.8773345707065));
#205128=CARTESIAN_POINT('Ctrl Pts',(20.7971284192367,-18.4716259697097,
21.8818449480945));
#205129=CARTESIAN_POINT('Ctrl Pts',(20.8114805262578,-18.5448591607076,
21.8863553254824));
#205130=CARTESIAN_POINT('Ctrl Pts',(20.8265480064888,-18.621742621512,21.891090520254));
#205131=CARTESIAN_POINT('Ctrl Pts',(20.8373635429458,-18.6995717540552,
21.8958257150255));
#205132=CARTESIAN_POINT('Ctrl Pts',(20.843824811693,-18.7778498809511,21.9005609097971));
#205133=CARTESIAN_POINT('Ctrl Pts',(20.8499588507186,-18.8521636270621,
21.9050562915339));
#205134=CARTESIAN_POINT('Ctrl Pts',(20.8521688501583,-18.9268814796183,
21.9095516732707));
#205135=CARTESIAN_POINT('Ctrl Pts',(20.8504196084828,-19.0015685467751,
21.9140470550075));
#205136=CARTESIAN_POINT('Ctrl Pts',(20.8486720115918,-19.0761853868609,
21.9185382098078));
#205137=CARTESIAN_POINT('Ctrl Pts',(20.8429725838885,-19.1507710509859,
21.9230293646081));
#205138=CARTESIAN_POINT('Ctrl Pts',(20.8333381346341,-19.2248889819521,
21.9275205194084));
#205139=CARTESIAN_POINT('Ctrl Pts',(20.8237102273003,-19.2989565858473,
21.9320086246542));
#205140=CARTESIAN_POINT('Ctrl Pts',(20.8101526690551,-19.3725566428308,
21.9364967299001));
#205141=CARTESIAN_POINT('Ctrl Pts',(20.7927341278966,-19.4452573269945,
21.9409848351459));
#205142=CARTESIAN_POINT('Ctrl Pts',(20.7753228675005,-19.5179276230559,
21.9454710644121));
#205143=CARTESIAN_POINT('Ctrl Pts',(20.7540539396924,-19.5896988571003,
21.9499572936783));
#205144=CARTESIAN_POINT('Ctrl Pts',(20.7290469182522,-19.6601502622835,
21.9544435229445));
#205145=CARTESIAN_POINT('Ctrl Pts',(20.7040367879202,-19.7306104260392,
21.9589303099422));
#205146=CARTESIAN_POINT('Ctrl Pts',(20.6752877790479,-19.7997500064623,
21.9634170969398));
#205147=CARTESIAN_POINT('Ctrl Pts',(20.6429687820359,-19.8671651158193,
21.9679038839375));
#205148=CARTESIAN_POINT('Ctrl Pts',(20.6106482296079,-19.9345834696624,
21.9723908868707));
#205149=CARTESIAN_POINT('Ctrl Pts',(20.5747575484645,-20.0002767846379,
21.9768778898039));
#205150=CARTESIAN_POINT('Ctrl Pts',(20.5355123150534,-20.0638643706455,
21.9813648927371));
#205151=CARTESIAN_POINT('Ctrl Pts',(20.4962399941625,-20.1274958454851,
21.9858549926477));
#205152=CARTESIAN_POINT('Ctrl Pts',(20.4536087412679,-20.1890183104101,
21.9903450925584));
#205153=CARTESIAN_POINT('Ctrl Pts',(20.407877888554,-20.2480794011981,21.994835192469));
#205154=CARTESIAN_POINT('Ctrl Pts',(20.3903436794274,-20.2707247151527,
21.9965567949793));
#205155=CARTESIAN_POINT('Ctrl Pts',(20.372354222822,-20.2930085100904,21.9982783974897));
#205156=CARTESIAN_POINT('Ctrl Pts',(20.3539256943887,-20.3149122292573,
22.));
#205157=CARTESIAN_POINT('Origin',(-18.734,-18.952,0.));
#205158=CARTESIAN_POINT('',(-20.3539401105369,-20.3148950943758,21.9999997808643));
#205159=CARTESIAN_POINT('Ctrl Pts',(-20.3539401105369,-20.3148950943758,
21.9999997808643));
#205160=CARTESIAN_POINT('Ctrl Pts',(-20.3072932296543,-20.3703396797185,
21.9956147616661));
#205161=CARTESIAN_POINT('Ctrl Pts',(-20.2577049138449,-20.4234955896159,
21.9912297424679));
#205162=CARTESIAN_POINT('Ctrl Pts',(-20.2054285432655,-20.4740338504986,
21.9868447232696));
#205163=CARTESIAN_POINT('Ctrl Pts',(-20.1532297926735,-20.5244970721403,
21.9824662149506));
#205164=CARTESIAN_POINT('Ctrl Pts',(-20.0983512546661,-20.5723500270703,
21.9780877066316));
#205165=CARTESIAN_POINT('Ctrl Pts',(-20.0410860694924,-20.6172972728431,
21.9737091983125));
#205166=CARTESIAN_POINT('Ctrl Pts',(-19.983888278367,-20.6621916212607,
21.9693358429569));
#205167=CARTESIAN_POINT('Ctrl Pts',(-19.9243097978752,-20.7041867567888,
21.9649624876012));
#205168=CARTESIAN_POINT('Ctrl Pts',(-19.8626788010172,-20.7430257296126,
21.9605891322455));
#205169=CARTESIAN_POINT('Ctrl Pts',(-19.8010868010387,-20.7818401271607,
21.956218544121));
#205170=CARTESIAN_POINT('Ctrl Pts',(-19.7374452692593,-20.8175020674031,
21.9518479559964));
#205171=CARTESIAN_POINT('Ctrl Pts',(-19.6721123140465,-20.8497972194717,
21.9474773678718));
#205172=CARTESIAN_POINT('Ctrl Pts',(-19.6067990615792,-20.8820826321498,
21.9431080978047));
#205173=CARTESIAN_POINT('Ctrl Pts',(-19.5397958312689,-20.911003058507,
21.9387388277375));
#205174=CARTESIAN_POINT('Ctrl Pts',(-19.4714848515874,-20.9363903581904,
21.9343695576704));
#205175=CARTESIAN_POINT('Ctrl Pts',(-19.4031718505269,-20.9617784091052,
21.9300001583129));
#205176=CARTESIAN_POINT('Ctrl Pts',(-19.3335514769124,-20.9836329595348,
21.9256307589554));
#205177=CARTESIAN_POINT('Ctrl Pts',(-19.2630238363122,-21.001834817885,
21.9212613595979));
#205178=CARTESIAN_POINT('Ctrl Pts',(-19.192424400798,-21.0200552051529,
21.9168875123296));
#205179=CARTESIAN_POINT('Ctrl Pts',(-19.1209163233831,-21.0346153567022,
21.9125136650614));
#205180=CARTESIAN_POINT('Ctrl Pts',(-19.0489118445282,-21.0454468061491,
21.9081398177931));
#205181=CARTESIAN_POINT('Ctrl Pts',(-18.9768675429743,-21.0562842460226,
21.9037635515308));
#205182=CARTESIAN_POINT('Ctrl Pts',(-18.904326774497,-21.0633888314031,
21.8993872852686));
#205183=CARTESIAN_POINT('Ctrl Pts',(-18.8317061863209,-21.0667440746234,
21.8950110190063));
#205184=CARTESIAN_POINT('Ctrl Pts',(-18.7589614597164,-21.0701050533332,
21.8906272719066));
#205185=CARTESIAN_POINT('Ctrl Pts',(-18.6861371242322,-21.0697038968461,
21.8862435248068));
#205186=CARTESIAN_POINT('Ctrl Pts',(-18.6136484217024,-21.0655762341589,
21.8818597777071));
#205187=CARTESIAN_POINT('Ctrl Pts',(-18.5716418570464,-21.063184289987,
21.8793194348736));
#205188=CARTESIAN_POINT('Ctrl Pts',(-18.5297478967642,-21.0595419177169,
21.8767790920401));
#205189=CARTESIAN_POINT('Ctrl Pts',(-18.4880458377735,-21.0546639175302,
21.8742387492067));
#205190=CARTESIAN_POINT('Ctrl Pts',(-18.4158851680032,-21.0462230930451,
21.8698429748793));
#205191=CARTESIAN_POINT('Ctrl Pts',(-18.3440241776343,-21.0340474650401,
21.8654472005519));
#205192=CARTESIAN_POINT('Ctrl Pts',(-18.2728787135213,-21.0181694410566,
21.8610514262245));
#205193=CARTESIAN_POINT('Ctrl Pts',(-18.2018360755882,-21.0023143655011,
21.8566620050875));
#205194=CARTESIAN_POINT('Ctrl Pts',(-18.1315073759669,-20.9827676217893,
21.8522725839506));
#205195=CARTESIAN_POINT('Ctrl Pts',(-18.0623020985936,-20.9596132419483,
21.8478831628136));
#205196=CARTESIAN_POINT('Ctrl Pts',(-17.9931748381961,-20.9364849646642,
21.8434986899895));
#205197=CARTESIAN_POINT('Ctrl Pts',(-17.9251689375377,-20.9097572825852,
21.8391142171653));
#205198=CARTESIAN_POINT('Ctrl Pts',(-17.8586808325707,-20.8795646176279,
21.8347297443412));
#205199=CARTESIAN_POINT('Ctrl Pts',(-17.7922330111159,-20.8493902456658,
21.8303479279616));
#205200=CARTESIAN_POINT('Ctrl Pts',(-17.7273015969599,-20.8157552549639,
21.8259661115821));
#205201=CARTESIAN_POINT('Ctrl Pts',(-17.6642637491768,-20.7788424545304,
21.8215842952025));
#205202=CARTESIAN_POINT('Ctrl Pts',(-17.6012435076605,-20.7419399637226,
21.8172037026501));
#205203=CARTESIAN_POINT('Ctrl Pts',(-17.5401161967491,-20.7017617236165,
21.8128231100976));
#205204=CARTESIAN_POINT('Ctrl Pts',(-17.4812335587017,-20.6585360364073,
21.8084425175452));
#205205=CARTESIAN_POINT('Ctrl Pts',(-17.4223481372602,-20.6153083059113,
21.8040617179213));
#205206=CARTESIAN_POINT('Ctrl Pts',(-17.3657079854645,-20.5690331281733,
21.7996809182973));
#205207=CARTESIAN_POINT('Ctrl Pts',(-17.3116337298584,-20.5199806100726,
21.7953001186734));
#205208=CARTESIAN_POINT('Ctrl Pts',(-17.2575023549029,-20.47087627715,21.790914691553));
#205209=CARTESIAN_POINT('Ctrl Pts',(-17.2059426440142,-20.4189890701121,
21.7865292644327));
#205210=CARTESIAN_POINT('Ctrl Pts',(-17.1572395226006,-20.3646271259293,
21.7821438373123));
#205211=CARTESIAN_POINT('Ctrl Pts',(-17.1085091560373,-20.3102347709788,
21.7777559569279));
#205212=CARTESIAN_POINT('Ctrl Pts',(-17.0626388625667,-20.253365296582,
21.7733680765434));
#205213=CARTESIAN_POINT('Ctrl Pts',(-17.0198725666879,-20.1943591036278,
21.768980196159));
#205214=CARTESIAN_POINT('Ctrl Pts',(-16.9770305343292,-20.1352484143348,
21.7645845451083));
#205215=CARTESIAN_POINT('Ctrl Pts',(-16.9373037385248,-20.0739938533524,
21.7601888940575));
#205216=CARTESIAN_POINT('Ctrl Pts',(-16.9008918467625,-20.010963407552,
21.7557932430068));
#205217=CARTESIAN_POINT('Ctrl Pts',(-16.8767856902822,-19.9692346833373,
21.7528831428463));
#205218=CARTESIAN_POINT('Ctrl Pts',(-16.8541315013796,-19.9267281135982,
21.7499730426858));
#205219=CARTESIAN_POINT('Ctrl Pts',(-16.8329755935997,-19.8835552620593,
21.7470629425253));
#205220=CARTESIAN_POINT('Ctrl Pts',(-16.8011149796973,-19.8185373215268,
21.7426803568856));
#205221=CARTESIAN_POINT('Ctrl Pts',(-16.7725300723094,-19.7517529070192,
21.7382977712459));
#205222=CARTESIAN_POINT('Ctrl Pts',(-16.7474199334088,-19.6835658815327,
21.7339151856062));
#205223=CARTESIAN_POINT('Ctrl Pts',(-16.722347574114,-19.6154814472323,
21.7295391938112));
#205224=CARTESIAN_POINT('Ctrl Pts',(-16.7007397717712,-19.5459990409051,
21.7251632020162));
#205225=CARTESIAN_POINT('Ctrl Pts',(-16.6827489097976,-19.4755054583704,
21.7207872102213));
#205226=CARTESIAN_POINT('Ctrl Pts',(-16.6647796017072,-19.4050963304016,
21.7164164610665));
#205227=CARTESIAN_POINT('Ctrl Pts',(-16.6504187455061,-19.3336788989525,
21.7120457119117));
#205228=CARTESIAN_POINT('Ctrl Pts',(-16.6397693978102,-19.2616565595166,
21.7076749627569));
#205229=CARTESIAN_POINT('Ctrl Pts',(-16.6291269464843,-19.1896808607495,
21.7033070440387));
#205230=CARTESIAN_POINT('Ctrl Pts',(-16.6221913058276,-19.117101508527,
21.6989391253204));
#205231=CARTESIAN_POINT('Ctrl Pts',(-16.6190144751312,-19.0443321698839,
21.6945712066022));
#205232=CARTESIAN_POINT('Ctrl Pts',(-16.6158386463066,-18.9715857803861,
21.6902046653873));
#205233=CARTESIAN_POINT('Ctrl Pts',(-16.6164192953802,-18.8986500064394,
21.6858381241723));
#205234=CARTESIAN_POINT('Ctrl Pts',(-16.6207564302585,-18.8259420175236,
21.6814715829573));
#205235=CARTESIAN_POINT('Ctrl Pts',(-16.6250936381862,-18.7532328040023,
21.6771049681976));
#205236=CARTESIAN_POINT('Ctrl Pts',(-16.6331874267156,-18.6807518659564,
21.6727383534379));
#205237=CARTESIAN_POINT('Ctrl Pts',(-16.64498579739,-18.6089130412075,21.6683717386782));
#205238=CARTESIAN_POINT('Ctrl Pts',(-16.6567963801275,-18.5369998587107,
21.6640006041948));
#205239=CARTESIAN_POINT('Ctrl Pts',(-16.672319122297,-18.465730594939,21.6596294697114));
#205240=CARTESIAN_POINT('Ctrl Pts',(-16.6914506939752,-18.3955098091991,
21.655258335228));
#205241=CARTESIAN_POINT('Ctrl Pts',(-16.7105926424343,-18.325250936379,
21.6508848298832));
#205242=CARTESIAN_POINT('Ctrl Pts',(-16.7333471660201,-18.2560421336627,
21.6465113245384));
#205243=CARTESIAN_POINT('Ctrl Pts',(-16.7595615727462,-18.1882710579117,
21.6421378191936));
#205244=CARTESIAN_POINT('Ctrl Pts',(-16.7858227154186,-18.1203791575545,
21.6377565166129));
#205245=CARTESIAN_POINT('Ctrl Pts',(-16.8155558613104,-18.0539305447508,
21.6333752140323));
#205246=CARTESIAN_POINT('Ctrl Pts',(-16.8485611226492,-17.9892906774244,
21.6289939114516));
#205247=CARTESIAN_POINT('Ctrl Pts',(-16.8714288660015,-17.9445048512745,
21.6259583195824));
#205248=CARTESIAN_POINT('Ctrl Pts',(-16.8958663903147,-17.9005867928719,
21.6229227277131));
#205249=CARTESIAN_POINT('Ctrl Pts',(-16.9217951734766,-17.8576496599694,
21.6198871358438));
#205250=CARTESIAN_POINT('Ctrl Pts',(-16.9592871125939,-17.7955643564438,
21.6154977965973));
#205251=CARTESIAN_POINT('Ctrl Pts',(-17.0000461986468,-17.7352871847913,
21.6111084573508));
#205252=CARTESIAN_POINT('Ctrl Pts',(-17.0438726443021,-17.6771829458619,
21.6067191181042));
#205253=CARTESIAN_POINT('Ctrl Pts',(-17.0876341035589,-17.6191648646202,
21.6023362874245));
#205254=CARTESIAN_POINT('Ctrl Pts',(-17.134453605312,-17.5633137014982,
21.5979534567447));
#205255=CARTESIAN_POINT('Ctrl Pts',(-17.1840868960386,-17.5099672783988,
21.593570626065));
#205256=CARTESIAN_POINT('Ctrl Pts',(-17.2336618872153,-17.4566835163159,
21.5891929434835));
#205257=CARTESIAN_POINT('Ctrl Pts',(-17.2860437748972,-17.4058990008948,
21.5848152609019));
#205258=CARTESIAN_POINT('Ctrl Pts',(-17.3409477315906,-17.3579189551721,
21.5804375783204));
#205259=CARTESIAN_POINT('Ctrl Pts',(-17.3958168761313,-17.3099693314588,
21.5760626714324));
#205260=CARTESIAN_POINT('Ctrl Pts',(-17.4532045546155,-17.2648209656694,
21.5716877645444));
#205261=CARTESIAN_POINT('Ctrl Pts',(-17.5127897524411,-17.2227416239159,
21.5673128576563));
#205262=CARTESIAN_POINT('Ctrl Pts',(-17.5723567979443,-17.1806751014162,
21.5629392835611));
#205263=CARTESIAN_POINT('Ctrl Pts',(-17.6341196401156,-17.14167602466,21.5585657094658));
#205264=CARTESIAN_POINT('Ctrl Pts',(-17.6977262557446,-17.1059702800424,
21.5541921353705));
#205265=CARTESIAN_POINT('Ctrl Pts',(-17.761334446059,-17.0702636514709,
21.5498184530003));
#205266=CARTESIAN_POINT('Ctrl Pts',(-17.8267860790938,-17.0378507511553,
21.5454447706301));
#205267=CARTESIAN_POINT('Ctrl Pts',(-17.8937038483149,-17.0089118966287,
21.5410710882598));
#205268=CARTESIAN_POINT('Ctrl Pts',(-17.9606908447099,-16.9799431045363,
21.5366928812667));
#205269=CARTESIAN_POINT('Ctrl Pts',(-18.0291465621343,-16.9544557255711,
21.5323146742736));
#205270=CARTESIAN_POINT('Ctrl Pts',(-18.0986737635119,-16.9325818726103,
21.5279364672805));
#205271=CARTESIAN_POINT('Ctrl Pts',(-18.168238835056,-16.9106961053709,
21.5235558755599));
#205272=CARTESIAN_POINT('Ctrl Pts',(-18.2388760855,-16.8924279037581,21.5191752838393));
#205273=CARTESIAN_POINT('Ctrl Pts',(-18.3101757995837,-16.8778587205445,
21.5147946921187));
#205274=CARTESIAN_POINT('Ctrl Pts',(-18.38160150593,-16.8632637924259,21.5104063595443));
#205275=CARTESIAN_POINT('Ctrl Pts',(-18.453691536507,-16.8523810078683,
21.5060180269699));
#205276=CARTESIAN_POINT('Ctrl Pts',(-18.5260293173379,-16.8452401192464,
21.5016296943955));
#205277=CARTESIAN_POINT('Ctrl Pts',(-18.5750331047421,-16.8404026666194,
21.4986569059845));
#205278=CARTESIAN_POINT('Ctrl Pts',(-18.6241504958208,-16.8372813242577,
21.4956841175734));
#205279=CARTESIAN_POINT('Ctrl Pts',(-18.6732524736177,-16.8358717576578,
21.4927113291624));
#205280=CARTESIAN_POINT('Ctrl Pts',(-18.7457477453063,-16.833790641617,
21.4883222370484));
#205281=CARTESIAN_POINT('Ctrl Pts',(-18.8184909189991,-16.8354351540471,
21.4839331449344));
#205282=CARTESIAN_POINT('Ctrl Pts',(-18.8910671368434,-16.8408347022263,
21.4795440528204));
#205283=CARTESIAN_POINT('Ctrl Pts',(-18.9635359887558,-16.8462262625614,
21.4751614537282));
#205284=CARTESIAN_POINT('Ctrl Pts',(-19.0358378982521,-16.8553617955042,
21.470778854636));
#205285=CARTESIAN_POINT('Ctrl Pts',(-19.107556633465,-16.8682187155092,
21.4663962555438));
#205286=CARTESIAN_POINT('Ctrl Pts',(-19.1791915242117,-16.8810606048308,
21.4620187800316));
#205287=CARTESIAN_POINT('Ctrl Pts',(-19.2502441227826,-16.8976151540491,
21.4576413045195));
#205288=CARTESIAN_POINT('Ctrl Pts',(-19.3203036537857,-16.9178080165438,
21.4532638290073));
#205289=CARTESIAN_POINT('Ctrl Pts',(-19.3903190046979,-16.9379881452606,
21.4488891139657));
#205290=CARTESIAN_POINT('Ctrl Pts',(-19.4593420684319,-16.9618019016887,
21.444514398924));
#205291=CARTESIAN_POINT('Ctrl Pts',(-19.5269739887336,-16.989124238982,
21.4401396838823));
#205292=CARTESIAN_POINT('Ctrl Pts',(-19.5945855447919,-17.0164383494096,
21.435766286085));
#205293=CARTESIAN_POINT('Ctrl Pts',(-19.6608063422521,-17.0472587627945,
21.4313928882876));
#205294=CARTESIAN_POINT('Ctrl Pts',(-19.7252559661585,-17.0814116942643,
21.4270194904902));
#205295=CARTESIAN_POINT('Ctrl Pts',(-19.7897074198449,-17.115565595365,
21.4226459685284));
#205296=CARTESIAN_POINT('Ctrl Pts',(-19.852387175046,-17.1530519748722,
21.4182724465665));
#205297=CARTESIAN_POINT('Ctrl Pts',(-19.9129394590442,-17.1936511290678,
21.4138989246046));
#205298=CARTESIAN_POINT('Ctrl Pts',(-19.9735547443612,-17.2342925244489,
21.4095208522338));
#205299=CARTESIAN_POINT('Ctrl Pts',(-20.0320377377389,-17.2780528916324,
21.4051427798631));
#205300=CARTESIAN_POINT('Ctrl Pts',(-20.0880624200393,-17.3246696823824,
21.4007647074923));
#205301=CARTESIAN_POINT('Ctrl Pts',(-20.1441178009626,-17.3713120167183,
21.3963842361647));
#205302=CARTESIAN_POINT('Ctrl Pts',(-20.1977118344489,-17.420813563513,
21.3920037648371));
#205303=CARTESIAN_POINT('Ctrl Pts',(-20.2485543554084,-17.4728738713303,
21.3876232935095));
#205304=CARTESIAN_POINT('Ctrl Pts',(-20.2994870055889,-17.5250264671557,
21.3832350568615));
#205305=CARTESIAN_POINT('Ctrl Pts',(-20.3476580839202,-17.5797465198983,
21.3788468202134));
#205306=CARTESIAN_POINT('Ctrl Pts',(-20.3928171932228,-17.6366998367413,
21.3744585835654));
#205307=CARTESIAN_POINT('Ctrl Pts',(-20.4234261084619,-17.6753028843823,
21.3714842298706));
#205308=CARTESIAN_POINT('Ctrl Pts',(-20.4526521461855,-17.7149312605343,
21.3685098761757));
#205309=CARTESIAN_POINT('Ctrl Pts',(-20.4804290453301,-17.7554739494572,
21.3655355224809));
#205310=CARTESIAN_POINT('Ctrl Pts',(-20.5219934386079,-17.8161406300021,
21.3610848022592));
#205311=CARTESIAN_POINT('Ctrl Pts',(-20.5604705880664,-17.8790885273535,
21.3566340820375));
#205312=CARTESIAN_POINT('Ctrl Pts',(-20.5956057988651,-17.943975769323,
21.3521833618158));
#205313=CARTESIAN_POINT('Ctrl Pts',(-20.6306759128556,-18.0087427913695,
21.3477408876718));
#205314=CARTESIAN_POINT('Ctrl Pts',(-20.6624161763064,-18.0754416108878,
21.3432984135279));
#205315=CARTESIAN_POINT('Ctrl Pts',(-20.6906149891654,-18.1437013026279,
21.3388559393839));
#205316=CARTESIAN_POINT('Ctrl Pts',(-20.701834052255,-18.1708588213483,
21.3370884749894));
#205317=CARTESIAN_POINT('Ctrl Pts',(-20.712493028082,-18.198263095923,21.3353210105949));
#205318=CARTESIAN_POINT('Ctrl Pts',(-20.7225805737622,-18.2258896078036,
21.3335535462005));
#205319=CARTESIAN_POINT('',(-17.1140743056113,-20.3149122292574,22.));
#205320=CARTESIAN_POINT('Origin',(-18.734,-18.952,22.));
#205321=CARTESIAN_POINT('Ctrl Pts',(-20.7225805737622,-18.2258896078036,
21.5555703780636));
#205322=CARTESIAN_POINT('Ctrl Pts',(-20.6978890798413,-18.1582676240448,
21.5598847419305));
#205323=CARTESIAN_POINT('Ctrl Pts',(-20.669739897526,-18.0918946295011,
21.5641991057974));
#205324=CARTESIAN_POINT('Ctrl Pts',(-20.6382937604498,-18.0271463500035,
21.5685134696643));
#205325=CARTESIAN_POINT('Ctrl Pts',(-20.606820934294,-17.962343117111,21.5728314952338));
#205326=CARTESIAN_POINT('Ctrl Pts',(-20.5720457802183,-17.8991678020743,
21.5771495208033));
#205327=CARTESIAN_POINT('Ctrl Pts',(-20.5341758304195,-17.8379730795113,
21.5814675463728));
#205328=CARTESIAN_POINT('Ctrl Pts',(-20.4962904117645,-17.7767533605497,
21.5857873357396));
#205329=CARTESIAN_POINT('Ctrl Pts',(-20.4553079633058,-17.7175162539135,
21.5901071251064));
#205330=CARTESIAN_POINT('Ctrl Pts',(-20.4114787620569,-17.6605844964351,
21.5944269144732));
#205331=CARTESIAN_POINT('Ctrl Pts',(-20.3675727878446,-17.6035530150371,
21.598754270554));
#205332=CARTESIAN_POINT('Ctrl Pts',(-20.3208104248372,-17.5488353262228,
21.6030816266348));
#205333=CARTESIAN_POINT('Ctrl Pts',(-20.2714810943291,-17.4967196543001,
21.6074089827156));
#205334=CARTESIAN_POINT('Ctrl Pts',(-20.2294415799254,-17.4523055599289,
21.6110968484623));
#205335=CARTESIAN_POINT('Ctrl Pts',(-20.1855384940817,-17.4097807538747,
21.614784714209));
#205336=CARTESIAN_POINT('Ctrl Pts',(-20.1399695509607,-17.369300211104,
21.6184725799558));
#205337=CARTESIAN_POINT('Ctrl Pts',(-20.0856805133166,-17.3210732925096,
21.6228661574372));
#205338=CARTESIAN_POINT('Ctrl Pts',(-20.0288041823845,-17.2755513561322,
21.6272597349186));
#205339=CARTESIAN_POINT('Ctrl Pts',(-19.969640873017,-17.2330233762701,
21.6316533124001));
#205340=CARTESIAN_POINT('Ctrl Pts',(-19.9105638618643,-17.1905574295968,
21.6360404812154));
#205341=CARTESIAN_POINT('Ctrl Pts',(-19.849206882515,-17.1510770477242,
21.6404276500308));
#205342=CARTESIAN_POINT('Ctrl Pts',(-19.7859046048043,-17.1148321518186,
21.6448148188462));
#205343=CARTESIAN_POINT('Ctrl Pts',(-19.7226747936877,-17.0786287480086,
21.6491969653592));
#205344=CARTESIAN_POINT('Ctrl Pts',(-19.6575045236034,-17.0456537097674,
21.6535791118721));
#205345=CARTESIAN_POINT('Ctrl Pts',(-19.5907574447862,-17.0161137221408,
21.6579612583851));
#205346=CARTESIAN_POINT('Ctrl Pts',(-19.524051506928,-16.9865919421039,
21.6623407038703));
#205347=CARTESIAN_POINT('Ctrl Pts',(-19.4557711276412,-16.960501205489,
21.6667201493556));
#205348=CARTESIAN_POINT('Ctrl Pts',(-19.3863033026644,-16.9380016382,21.6710995948408));
#205349=CARTESIAN_POINT('Ctrl Pts',(-19.3168555527303,-16.9155085729106,
21.6754777747394));
#205350=CARTESIAN_POINT('Ctrl Pts',(-19.2462214956912,-16.8966047644762,
21.6798559546379));
#205351=CARTESIAN_POINT('Ctrl Pts',(-19.1748052243022,-16.8814011121833,
21.6842341345365));
#205352=CARTESIAN_POINT('Ctrl Pts',(-19.10338621101,-16.8661968761726,21.6886124825276));
#205353=CARTESIAN_POINT('Ctrl Pts',(-19.0311853945028,-16.8546931765608,
21.6929908305188));
#205354=CARTESIAN_POINT('Ctrl Pts',(-18.958617414822,-16.8469498778037,
21.6973691785099));
#205355=CARTESIAN_POINT('Ctrl Pts',(-18.8859734847581,-16.8391984748317,
21.7017521089244));
#205356=CARTESIAN_POINT('Ctrl Pts',(-18.8129621034892,-16.835215381558,
21.7061350393389));
#205357=CARTESIAN_POINT('Ctrl Pts',(-18.7400025813939,-16.8350085099329,
21.7105179697534));
#205358=CARTESIAN_POINT('Ctrl Pts',(-18.6670027054265,-16.8348015238872,
21.7149033243644));
#205359=CARTESIAN_POINT('Ctrl Pts',(-18.5940552263849,-16.8383748946447,
21.7192886789753));
#205360=CARTESIAN_POINT('Ctrl Pts',(-18.5215762918332,-16.8456844566379,
21.7236740335863));
#205361=CARTESIAN_POINT('Ctrl Pts',(-18.4489692699444,-16.8530069363477,
21.728067138151));
#205362=CARTESIAN_POINT('Ctrl Pts',(-18.3768329218414,-16.8640787198162,
21.7324602427158));
#205363=CARTESIAN_POINT('Ctrl Pts',(-18.3055745682925,-16.8788042423673,
21.7368533472805));
#205364=CARTESIAN_POINT('Ctrl Pts',(-18.2580212556926,-16.8886311235987,
21.739785027066));
#205365=CARTESIAN_POINT('Ctrl Pts',(-18.2108587080193,-16.900084095337,
21.7427167068516));
#205366=CARTESIAN_POINT('Ctrl Pts',(-18.1642037039559,-16.913122568418,
21.7456483866372));
#205367=CARTESIAN_POINT('Ctrl Pts',(-18.0951065059757,-16.932432864793,
21.7499902758433));
#205368=CARTESIAN_POINT('Ctrl Pts',(-18.0268409185985,-16.9553020920462,
21.7543321650495));
#205369=CARTESIAN_POINT('Ctrl Pts',(-17.9598056269363,-16.9816416385042,
21.7586740542557));
#205370=CARTESIAN_POINT('Ctrl Pts',(-17.8928712802768,-17.007941521592,
21.7630094052339));
#205371=CARTESIAN_POINT('Ctrl Pts',(-17.8271640088704,-17.0377011783514,
21.7673447562122));
#205372=CARTESIAN_POINT('Ctrl Pts',(-17.7630690182321,-17.0707817700641,
21.7716801071904));
#205373=CARTESIAN_POINT('Ctrl Pts',(-17.6990476945068,-17.1038243409416,
21.7760104753779));
#205374=CARTESIAN_POINT('Ctrl Pts',(-17.6366354094004,-17.140180045608,
21.7803408435655));
#205375=CARTESIAN_POINT('Ctrl Pts',(-17.576197298269,-17.1796620232404,
21.784671211753));
#205376=CARTESIAN_POINT('Ctrl Pts',(-17.5157963311547,-17.2191197360633,
21.7889989185855));
#205377=CARTESIAN_POINT('Ctrl Pts',(-17.4573675446825,-17.2616996436244,
21.793326625418));
#205378=CARTESIAN_POINT('Ctrl Pts',(-17.4012499559382,-17.3071698202996,
21.7976543322506));
#205379=CARTESIAN_POINT('Ctrl Pts',(-17.3451474140536,-17.3526278050152,
21.8019808786911));
#205380=CARTESIAN_POINT('Ctrl Pts',(-17.2913552237362,-17.4009742110386,
21.8063074251317));
#205381=CARTESIAN_POINT('Ctrl Pts',(-17.2401804886106,-17.4519359122383,
21.8106339715723));
#205382=CARTESIAN_POINT('Ctrl Pts',(-17.1890017454992,-17.502901604739,
21.8149608568663));
#205383=CARTESIAN_POINT('Ctrl Pts',(-17.1404412125279,-17.5564826492106,
21.8192877421603));
#205384=CARTESIAN_POINT('Ctrl Pts',(-17.0947688687351,-17.6123693425829,
21.8236146274544));
#205385=CARTESIAN_POINT('Ctrl Pts',(-17.0490417134499,-17.6683231057134,
21.8279467054541));
#205386=CARTESIAN_POINT('Ctrl Pts',(-17.0062099790967,-17.7265876580954,
21.8322787834538));
#205387=CARTESIAN_POINT('Ctrl Pts',(-16.9665025074284,-17.7868212095334,
21.8366108614535));
#205388=CARTESIAN_POINT('Ctrl Pts',(-16.9267705288898,-17.8470919362378,
21.8409456131484));
#205389=CARTESIAN_POINT('Ctrl Pts',(-16.8901668972173,-17.9093336530359,
21.8452803648433));
#205390=CARTESIAN_POINT('Ctrl Pts',(-16.8568748225048,-17.9731792462286,
21.8496151165381));
#205391=CARTESIAN_POINT('Ctrl Pts',(-16.8235156981184,-18.0371534233633,
21.8539585983494));
#205392=CARTESIAN_POINT('Ctrl Pts',(-16.7934816509746,-18.1027374769631,
21.8583020801606));
#205393=CARTESIAN_POINT('Ctrl Pts',(-16.7669077870852,-18.1695441061056,
21.8626455619719));
#205394=CARTESIAN_POINT('Ctrl Pts',(-16.7461498194961,-18.221729586104,
21.8660384390875));
#205395=CARTESIAN_POINT('Ctrl Pts',(-16.7275022238381,-18.2746606281223,
21.869431316203));
#205396=CARTESIAN_POINT('Ctrl Pts',(-16.7110077838934,-18.328147859207,
21.8728241933186));
#205397=CARTESIAN_POINT('Ctrl Pts',(-16.6890805388882,-18.3992522813377,
21.8773345888236));
#205398=CARTESIAN_POINT('Ctrl Pts',(-16.6708712302021,-18.471627433023,
21.8818449843287));
#205399=CARTESIAN_POINT('Ctrl Pts',(-16.65651913225,-18.5448609032129,21.8863553798337));
#205400=CARTESIAN_POINT('Ctrl Pts',(-16.6414517292682,-18.6217443115328,
21.8910905723407));
#205401=CARTESIAN_POINT('Ctrl Pts',(-16.6306362647773,-18.699573380232,
21.8958257648476));
#205402=CARTESIAN_POINT('Ctrl Pts',(-16.6241750600365,-18.7778514349529,
21.9005609573545));
#205403=CARTESIAN_POINT('Ctrl Pts',(-16.6180410539461,-18.8521654497015,
21.9050563573367));
#205404=CARTESIAN_POINT('Ctrl Pts',(-16.6158311159158,-18.9268835670766,
21.9095517573189));
#205405=CARTESIAN_POINT('Ctrl Pts',(-16.6175804464527,-19.001570892293,
21.9140471573011));
#205406=CARTESIAN_POINT('Ctrl Pts',(-16.6193281321099,-19.0761879896894,
21.9185383302991));
#205407=CARTESIAN_POINT('Ctrl Pts',(-16.6250276759246,-19.1507739043837,
21.9230295032971));
#205408=CARTESIAN_POINT('Ctrl Pts',(-16.6346622676094,-19.2248920763987,
21.9275206762951));
#205409=CARTESIAN_POINT('Ctrl Pts',(-16.6442903170874,-19.2989599197204,
21.932008799638));
#205410=CARTESIAN_POINT('Ctrl Pts',(-16.6578480436051,-19.3725602066461,
21.9364969229808));
#205411=CARTESIAN_POINT('Ctrl Pts',(-16.6752667781491,-19.4452611085899,
21.9409850463236));
#205412=CARTESIAN_POINT('Ctrl Pts',(-16.6926782312815,-19.5179316199686,
21.9454712935328));
#205413=CARTESIAN_POINT('Ctrl Pts',(-16.7139473766674,-19.5897030572418,
21.949957540742));
#205414=CARTESIAN_POINT('Ctrl Pts',(-16.7389546395216,-19.6601546509298,
21.9544437879513));
#205415=CARTESIAN_POINT('Ctrl Pts',(-16.7639650091895,-19.7306149972742,
21.9589305925159));
#205416=CARTESIAN_POINT('Ctrl Pts',(-16.792714280612,-19.7997547457854,
21.9634173970806));
#205417=CARTESIAN_POINT('Ctrl Pts',(-16.8250335623977,-19.8671700061235,
21.9679042016453));
#205418=CARTESIAN_POINT('Ctrl Pts',(-16.8573543979593,-19.9345885075052,
21.9723912219168));
#205419=CARTESIAN_POINT('Ctrl Pts',(-16.8932453841005,-20.0002819530908,
21.9768782421882));
#205420=CARTESIAN_POINT('Ctrl Pts',(-16.9324909433493,-20.0638696500964,
21.9813652624597));
#205421=CARTESIAN_POINT('Ctrl Pts',(-16.971763585854,-20.1275012288023,
21.9858553792119));
#205422=CARTESIAN_POINT('Ctrl Pts',(-17.0143951804746,-20.1890237784353,
21.9903454959641));
#205423=CARTESIAN_POINT('Ctrl Pts',(-17.0601263939598,-20.2480849320172,
21.9948356127163));
#205424=CARTESIAN_POINT('Ctrl Pts',(-17.0776592489258,-20.2707283425231,
21.9965570751442));
#205425=CARTESIAN_POINT('Ctrl Pts',(-17.0956472766607,-20.2930102923405,
21.9982785375721));
#205426=CARTESIAN_POINT('Ctrl Pts',(-17.1140743056112,-20.3149122292573,
22.));
#205427=CARTESIAN_POINT('Origin',(-23.734,10.1295,7.));
#205428=CARTESIAN_POINT('',(-17.7339261105301,14.3917184061412,6.91639119908484));
#205429=CARTESIAN_POINT('Ctrl Pts',(-17.7339050342228,14.3916804139849,
6.91641101362463));
#205430=CARTESIAN_POINT('Ctrl Pts',(-17.747271947537,14.3963166964844,7.15281383796445));
#205431=CARTESIAN_POINT('Ctrl Pts',(-17.7606435542079,14.381276775214,7.3891987374152));
#205432=CARTESIAN_POINT('Ctrl Pts',(-17.7868173786296,14.3129820114568,
7.85141300883512));
#205433=CARTESIAN_POINT('Ctrl Pts',(-17.7995847185911,14.2607676448875,
8.0765946212184));
#205434=CARTESIAN_POINT('Ctrl Pts',(-17.8351210560246,14.0658910059837,
8.68704183225604));
#205435=CARTESIAN_POINT('Ctrl Pts',(-17.8583311393401,13.8854986826804,
9.05760511570486));
#205436=CARTESIAN_POINT('Ctrl Pts',(-17.896785360625,13.501055669657,9.62312009133906));
#205437=CARTESIAN_POINT('Ctrl Pts',(-17.9119488674433,13.3256514205499,
9.83421379898093));
#205438=CARTESIAN_POINT('Ctrl Pts',(-17.9585784805536,12.7284406416945,
10.4264305443397));
#205439=CARTESIAN_POINT('Ctrl Pts',(-17.9907455843245,12.249980031746,10.7414542056046));
#205440=CARTESIAN_POINT('Ctrl Pts',(-18.0356184383294,11.5020306423617,
11.0430893364069));
#205441=CARTESIAN_POINT('Ctrl Pts',(-18.0487838384663,11.2730044491194,
11.1137338665646));
#205442=CARTESIAN_POINT('Ctrl Pts',(-18.0792554367816,10.7400986580418,
11.2301431695451));
#205443=CARTESIAN_POINT('Ctrl Pts',(-18.0966642257857,10.4350814532254,
11.2629999729017));
#205444=CARTESIAN_POINT('Ctrl Pts',(-18.1138504934428,10.1295003780333,
11.263));
#205445=CARTESIAN_POINT('Origin',(-17.734,10.1295,7.));
#205446=CARTESIAN_POINT('Origin',(23.734,10.1295,7.));
#205447=CARTESIAN_POINT('',(23.5339999818689,7.33961491412,10.2235360410646));
#205448=CARTESIAN_POINT('Ctrl Pts',(23.533999981869,7.33961491412,10.2235360410646));
#205449=CARTESIAN_POINT('Ctrl Pts',(23.5009788547464,6.89416391178422,9.83730563779939));
#205450=CARTESIAN_POINT('Ctrl Pts',(23.4291758459878,6.10016038128925,8.79502345374907));
#205451=CARTESIAN_POINT('Ctrl Pts',(23.3185909555934,5.6985094017683,6.80076298606476));
#205452=CARTESIAN_POINT('Ctrl Pts',(23.2022453106851,6.3076790998453,4.74899581907506));
#205453=CARTESIAN_POINT('Ctrl Pts',(23.085899665777,7.80672899094502,3.22136567669558));
#205454=CARTESIAN_POINT('Ctrl Pts',(22.9695540208687,9.84662493401956,2.57356512891912));
#205455=CARTESIAN_POINT('Ctrl Pts',(22.8532083759605,11.9523856169729,2.95643327596383));
#205456=CARTESIAN_POINT('Ctrl Pts',(22.7368627310523,13.6336979697146,4.28082124831138));
#205457=CARTESIAN_POINT('Ctrl Pts',(22.6205170861441,14.4990821903827,6.2383517396752));
#205458=CARTESIAN_POINT('Ctrl Pts',(22.5041714412359,14.3470299002299,8.3732307562808));
#205459=CARTESIAN_POINT('Ctrl Pts',(22.3878257963277,13.2129653049274,10.1883541012585));
#205460=CARTESIAN_POINT('Ctrl Pts',(22.2878747590527,11.6218855899156,11.109940009747));
#205461=CARTESIAN_POINT('Ctrl Pts',(22.2267056034138,10.5292997601409,11.262549287517));
#205462=CARTESIAN_POINT('Ctrl Pts',(22.2043183294109,10.1294634667828,11.26269919276));
#205463=CARTESIAN_POINT('',(23.534,7.33966741897454,3.77664721604215));
#205464=CARTESIAN_POINT('Origin',(23.534,10.1295,7.));
#205465=CARTESIAN_POINT('Ctrl Pts',(23.534,7.33966741897454,3.77664721604215));
#205466=CARTESIAN_POINT('Ctrl Pts',(23.5171384228933,7.56733156584535,3.57960243160758));
#205467=CARTESIAN_POINT('Ctrl Pts',(23.5006043298958,7.81523356358243,3.40722905341181));
#205468=CARTESIAN_POINT('Ctrl Pts',(23.4677316209677,8.33075529092307,3.12443663545715));
#205469=CARTESIAN_POINT('Ctrl Pts',(23.4515038045768,8.5955661823329,3.0122045914911));
#205470=CARTESIAN_POINT('Ctrl Pts',(23.41251419603,9.25346884470398,2.80867864495278));
#205471=CARTESIAN_POINT('Ctrl Pts',(23.3905041575587,9.65217768291865,2.74479412039573));
#205472=CARTESIAN_POINT('Ctrl Pts',(23.3528764260495,10.3266429480868,2.73283385968559));
#205473=CARTESIAN_POINT('Ctrl Pts',(23.3374995684002,10.5991983511286,2.75418468589991));
#205474=CARTESIAN_POINT('Ctrl Pts',(23.28999893921,11.4262024328021,2.89961566339959));
#205475=CARTESIAN_POINT('Ctrl Pts',(23.2592781393447,11.9594174069227,3.10821363505845));
#205476=CARTESIAN_POINT('Ctrl Pts',(23.2141339367492,12.6330052456083,3.54161899737083));
#205477=CARTESIAN_POINT('Ctrl Pts',(23.2008471051019,12.8190500942101,3.68424101884531));
#205478=CARTESIAN_POINT('Ctrl Pts',(23.16494641965,13.2927988981491,4.11364698227542));
#205479=CARTESIAN_POINT('Ctrl Pts',(23.142856411777,13.5527887079619,4.4273370726122));
#205480=CARTESIAN_POINT('Ctrl Pts',(23.1071703914128,13.8847096290569,4.96912126006405));
#205481=CARTESIAN_POINT('Ctrl Pts',(23.0941377991731,13.9887911184171,5.17464059795072));
#205482=CARTESIAN_POINT('Ctrl Pts',(23.0660637765397,14.1768533050884,5.63489940988804));
#205483=CARTESIAN_POINT('Ctrl Pts',(23.0512908040241,14.2544426432218,5.89120750097675));
#205484=CARTESIAN_POINT('Ctrl Pts',(23.0104953092479,14.4005588632585,6.61204200382184));
#205485=CARTESIAN_POINT('Ctrl Pts',(22.9840977251256,14.4173311561388,7.0831920722925));
#205486=CARTESIAN_POINT('Ctrl Pts',(22.9428531767094,14.3231670213471,7.81023920356386));
#205487=CARTESIAN_POINT('Ctrl Pts',(22.928285381263,14.2647372016801,8.06918027130044));
#205488=CARTESIAN_POINT('Ctrl Pts',(22.8916271555053,14.0602543447828,8.69657156102269));
#205489=CARTESIAN_POINT('Ctrl Pts',(22.8693565843284,13.886253987401,9.05328041975969));
#205490=CARTESIAN_POINT('Ctrl Pts',(22.8320314201182,13.5168336638794,9.60195233611007));
#205491=CARTESIAN_POINT('Ctrl Pts',(22.8173170927165,13.3476009303476,9.80856107552979));
#205492=CARTESIAN_POINT('Ctrl Pts',(22.776903461955,12.8353140666472,10.3264293462766));
#205493=CARTESIAN_POINT('Ctrl Pts',(22.7508427647092,12.4592147251802,10.5998547238669));
#205494=CARTESIAN_POINT('Ctrl Pts',(22.6994960602955,11.643957736814,11.0103447464061));
#205495=CARTESIAN_POINT('Ctrl Pts',(22.6749861462296,11.2116364346642,11.1479431088793));
#205496=CARTESIAN_POINT('Ctrl Pts',(22.6376197358264,10.555150792154,11.2470440165433));
#205497=CARTESIAN_POINT('Ctrl Pts',(22.6255433575552,10.3424480415559,11.2630000045993));
#205498=CARTESIAN_POINT('Ctrl Pts',(22.6135314140065,10.129499907926,11.263));
#205499=CARTESIAN_POINT('Origin',(-18.734,-18.952,-1.76670989022851));
#205500=CARTESIAN_POINT('',(-21.2939992553327,-18.9539526125931,21.7667098902285));
#205501=CARTESIAN_POINT('Ctrl Pts',(-17.1722616776481,-20.9849677398537,
21.4832513321535));
#205502=CARTESIAN_POINT('Ctrl Pts',(-17.2221126184485,-21.0237381697153,
21.4864046644898));
#205503=CARTESIAN_POINT('Ctrl Pts',(-17.963685564347,-21.5551355225752,
21.5319499323866));
#205504=CARTESIAN_POINT('Ctrl Pts',(-19.9618261650098,-21.7191790573139,
21.6198871358439));
#205505=CARTESIAN_POINT('Ctrl Pts',(-21.2281784624135,-20.0656258695291,
21.7112199895325));
#205506=CARTESIAN_POINT('Ctrl Pts',(-21.297142385429,-19.0852910214283,
21.7601609076607));
#205507=CARTESIAN_POINT('Ctrl Pts',(-21.2960080465361,-18.9539541447775,
21.7667098902285));
#205508=CARTESIAN_POINT('',(-18.072232390111,-16.4790132166747,21.9999999999826));
#205509=CARTESIAN_POINT('Ctrl Pts',(-21.2939992553327,-18.9539526125931,
21.7667098902285));
#205510=CARTESIAN_POINT('Ctrl Pts',(-21.2940622837578,-18.8713183400037,
21.7708336287807));
#205511=CARTESIAN_POINT('Ctrl Pts',(-21.290120073806,-18.7885361132696,
21.7749573673329));
#205512=CARTESIAN_POINT('Ctrl Pts',(-21.2821561914378,-18.7060324736127,
21.7790811058851));
#205513=CARTESIAN_POINT('Ctrl Pts',(-21.2742021133718,-18.6236304038401,
21.7831997677201));
#205514=CARTESIAN_POINT('Ctrl Pts',(-21.2622362429578,-18.5415067083406,
21.7873184295551));
#205515=CARTESIAN_POINT('Ctrl Pts',(-21.2462941819498,-18.4600874637281,
21.7914370913901));
#205516=CARTESIAN_POINT('Ctrl Pts',(-21.2303628128015,-18.3787228245485,
21.7955529909627));
#205517=CARTESIAN_POINT('Ctrl Pts',(-21.2104606337788,-18.2980621623454,
21.7996688905354));
#205518=CARTESIAN_POINT('Ctrl Pts',(-21.1866748711293,-18.2185247267081,
21.803784790108));
#205519=CARTESIAN_POINT('Ctrl Pts',(-21.1628974701717,-18.1390152518109,
21.8078992427696));
#205520=CARTESIAN_POINT('Ctrl Pts',(-21.1352393308965,-18.0606286731435,
21.8120136954312));
#205521=CARTESIAN_POINT('Ctrl Pts',(-21.1038380346635,-17.9837708486818,
21.8161281480927));
#205522=CARTESIAN_POINT('Ctrl Pts',(-21.0724377570491,-17.9069155173914,
21.8202424672866));
#205523=CARTESIAN_POINT('Ctrl Pts',(-21.0372947445442,-17.8315892795539,
21.8243567864805));
#205524=CARTESIAN_POINT('Ctrl Pts',(-20.9985948099081,-17.758178259983,
21.8284711056744));
#205525=CARTESIAN_POINT('Ctrl Pts',(-20.959859225451,-17.6846996152406,
21.8325892149197));
#205526=CARTESIAN_POINT('Ctrl Pts',(-20.9175603979486,-17.613140131245,
21.836707324165));
#205527=CARTESIAN_POINT('Ctrl Pts',(-20.8719298849008,-17.5438608707773,
21.8408254334103));
#205528=CARTESIAN_POINT('Ctrl Pts',(-20.8262774812034,-17.4745483744787,
21.8449455182654));
#205529=CARTESIAN_POINT('Ctrl Pts',(-20.7772904911253,-17.4075186609022,
21.8490656031205));
#205530=CARTESIAN_POINT('Ctrl Pts',(-20.7252420557879,-17.3431012849587,
21.8531856879756));
#205531=CARTESIAN_POINT('Ctrl Pts',(-20.6731075913472,-17.2785774357072,
21.85731258278));
#205532=CARTESIAN_POINT('Ctrl Pts',(-20.6179018945763,-17.2166748979188,
21.8614394775843));
#205533=CARTESIAN_POINT('Ctrl Pts',(-20.5599360513378,-17.1576874473981,
21.8655663723887));
#205534=CARTESIAN_POINT('Ctrl Pts',(-20.5193323481527,-17.1163681324571,
21.8684571646614));
#205535=CARTESIAN_POINT('Ctrl Pts',(-20.4773751065851,-17.076478372295,
21.871347956934));
#205536=CARTESIAN_POINT('Ctrl Pts',(-20.4341804678598,-17.0381070101209,
21.8742387492067));
#205537=CARTESIAN_POINT('Ctrl Pts',(-20.3717052812394,-16.9826080388726,
21.8784198881639));
#205538=CARTESIAN_POINT('Ctrl Pts',(-20.3063943198782,-16.9300688092441,
21.8826010271211));
#205539=CARTESIAN_POINT('Ctrl Pts',(-20.2385599097816,-16.8807927486903,
21.8867821660783));
#205540=CARTESIAN_POINT('Ctrl Pts',(-20.1708205215985,-16.8315857136584,
21.8909574481286));
#205541=CARTESIAN_POINT('Ctrl Pts',(-20.1005650755227,-16.7856330369313,
21.8951327301788));
#205542=CARTESIAN_POINT('Ctrl Pts',(-20.0281405702344,-16.7431993787412,
21.8993080122291));
#205543=CARTESIAN_POINT('Ctrl Pts',(-19.9553653729372,-16.7005602494225,
21.9035035117188));
#205544=CARTESIAN_POINT('Ctrl Pts',(-19.880400404287,-16.6614746253178,
21.9076990112086));
#205545=CARTESIAN_POINT('Ctrl Pts',(-19.8036290904368,-16.6261681898961,
21.9118945106983));
#205546=CARTESIAN_POINT('Ctrl Pts',(-19.7273611982937,-16.5910932735809,
21.916062498538));
#205547=CARTESIAN_POINT('Ctrl Pts',(-19.6493110036014,-16.5597483260403,
21.9202304863778));
#205548=CARTESIAN_POINT('Ctrl Pts',(-19.5698794212801,-16.5323087814598,
21.9243984742175));
#205549=CARTESIAN_POINT('Ctrl Pts',(-19.4904728949047,-16.5048778924257,
21.9285651473047));
#205550=CARTESIAN_POINT('Ctrl Pts',(-19.4096862815083,-16.4813501100524,
21.9327318203918));
#205551=CARTESIAN_POINT('Ctrl Pts',(-19.3279387681294,-16.4618520646932,
21.936898493479));
#205552=CARTESIAN_POINT('Ctrl Pts',(-19.2461924230011,-16.4423542979797,
21.9410651070204));
#205553=CARTESIAN_POINT('Ctrl Pts',(-19.1634856536714,-16.4268862595724,
21.9452317205618));
#205554=CARTESIAN_POINT('Ctrl Pts',(-19.0802496942046,-16.415523871734,
21.9493983341032));
#205555=CARTESIAN_POINT('Ctrl Pts',(-18.9960110559548,-16.4040246100579,
21.9536151395932));
#205556=CARTESIAN_POINT('Ctrl Pts',(-18.9112308686983,-16.39673065975,21.9578319450831));
#205557=CARTESIAN_POINT('Ctrl Pts',(-18.8263615920593,-16.3936666878,21.962048750573));
#205558=CARTESIAN_POINT('Ctrl Pts',(-18.742380245673,-16.3906347721311,
21.9662214384587));
#205559=CARTESIAN_POINT('Ctrl Pts',(-18.6583121305892,-16.3917446684187,
21.9703941263443));
#205560=CARTESIAN_POINT('Ctrl Pts',(-18.5745939384244,-16.3969677678094,
21.97456681423));
#205561=CARTESIAN_POINT('Ctrl Pts',(-18.4895480243537,-16.402273702523,
21.9788056785221));
#205562=CARTESIAN_POINT('Ctrl Pts',(-18.4048637212048,-16.4118243850528,
21.9830445428142));
#205563=CARTESIAN_POINT('Ctrl Pts',(-18.3209897195339,-16.4255355715488,
21.9872834071063));
#205564=CARTESIAN_POINT('Ctrl Pts',(-18.237115717863,-16.4392467580448,
21.9915222713984));
#205565=CARTESIAN_POINT('Ctrl Pts',(-18.1540524839651,-16.4571182804316,
21.9957611356905));
#205566=CARTESIAN_POINT('Ctrl Pts',(-18.072232390111,-16.4790132166747,
21.9999999999825));
#205567=CARTESIAN_POINT('',(-19.3957372685685,-16.4790050975816,22.));
#205568=CARTESIAN_POINT('Origin',(-18.734,-18.952,22.));
#205569=CARTESIAN_POINT('',(-21.2914666104891,-18.9488558930302,21.8332901097715));
#205570=CARTESIAN_POINT('Ctrl Pts',(-21.2914666104891,-18.9488558930302,
21.8332901097715));
#205571=CARTESIAN_POINT('Ctrl Pts',(-21.2935045175504,-18.6834066038016,
21.8464681376205));
#205572=CARTESIAN_POINT('Ctrl Pts',(-21.1334434961762,-17.5672072134799,
21.90203810103));
#205573=CARTESIAN_POINT('Ctrl Pts',(-20.2191097516036,-16.6993275322964,
21.9576080644395));
#205574=CARTESIAN_POINT('Ctrl Pts',(-19.3957372685685,-16.4790050975816,
22.));
#205575=CARTESIAN_POINT('Ctrl Pts',(-17.176996236551,-20.9788220778502,
21.5499224931685));
#205576=CARTESIAN_POINT('Ctrl Pts',(-17.5432452950599,-21.2588471679196,
21.5727725220976));
#205577=CARTESIAN_POINT('Ctrl Pts',(-18.7954429833719,-21.7916144582144,
21.6380144865871));
#205578=CARTESIAN_POINT('Ctrl Pts',(-20.7940987275605,-20.9887402433146,
21.7324703587881));
#205579=CARTESIAN_POINT('Ctrl Pts',(-21.2869488458059,-19.5373211115314,
21.80407620206));
#205580=CARTESIAN_POINT('Ctrl Pts',(-21.2914666104891,-18.9488558930302,
21.8332901097715));
#205581=CARTESIAN_POINT('Origin',(18.734,-18.952,-1.76670989022851));
#205582=CARTESIAN_POINT('',(16.1740007447319,-18.9539526972956,21.7667098902285));
#205583=CARTESIAN_POINT('Ctrl Pts',(20.2957383325669,-20.9849679853861,
21.4832513385096));
#205584=CARTESIAN_POINT('Ctrl Pts',(20.245887419744,-21.0237383877019,21.4864046687272));
#205585=CARTESIAN_POINT('Ctrl Pts',(19.5043144385534,-21.5551357017593,
21.5319499345053));
#205586=CARTESIAN_POINT('Ctrl Pts',(17.5061736134544,-21.7191789276414,
21.6198871358439));
#205587=CARTESIAN_POINT('Ctrl Pts',(16.2398215663958,-20.0656261776283,
21.7112199895325));
#205588=CARTESIAN_POINT('Ctrl Pts',(16.1708575232621,-19.0852911366623,
21.7601609076608));
#205589=CARTESIAN_POINT('Ctrl Pts',(16.1719918438157,-18.9539542296302,
21.7667098902285));
#205590=CARTESIAN_POINT('',(19.3957679668415,-16.4790133121946,21.9999999999819));
#205591=CARTESIAN_POINT('Ctrl Pts',(16.1740007447319,-18.9539526972956,
21.7667098902285));
#205592=CARTESIAN_POINT('Ctrl Pts',(16.1739377135638,-18.8713184130896,
21.770833628584));
#205593=CARTESIAN_POINT('Ctrl Pts',(16.1778799218946,-18.788536175973,21.7749573669396));
#205594=CARTESIAN_POINT('Ctrl Pts',(16.1858438033836,-18.7060325272615,
21.7790811052951));
#205595=CARTESIAN_POINT('Ctrl Pts',(16.1937978807278,-18.6236304468261,
21.7831997670146));
#205596=CARTESIAN_POINT('Ctrl Pts',(16.2057637513171,-18.5415067419994,
21.787318428734));
#205597=CARTESIAN_POINT('Ctrl Pts',(16.2217058130157,-18.4600874894405,
21.7914370904535));
#205598=CARTESIAN_POINT('Ctrl Pts',(16.2376371830466,-18.3787228413373,
21.7955529899605));
#205599=CARTESIAN_POINT('Ctrl Pts',(16.2575393635618,-18.2980621716067,
21.7996688894674));
#205600=CARTESIAN_POINT('Ctrl Pts',(16.2813251279379,-18.2185247298273,
21.8037847889744));
#205601=CARTESIAN_POINT('Ctrl Pts',(16.3051025309066,-18.1390152478367,
21.8078992416196));
#205602=CARTESIAN_POINT('Ctrl Pts',(16.3327606725192,-18.0606286634871,
21.8120136942648));
#205603=CARTESIAN_POINT('Ctrl Pts',(16.3641619710533,-17.9837708346894,
21.81612814691));
#205604=CARTESIAN_POINT('Ctrl Pts',(16.3955622513427,-17.9069154981479,
21.8202424661365));
#205605=CARTESIAN_POINT('Ctrl Pts',(16.4307052665747,-17.8315892564417,
21.824356785363));
#205606=CARTESIAN_POINT('Ctrl Pts',(16.4694052036476,-17.7581782342687,
21.8284711045895));
#205607=CARTESIAN_POINT('Ctrl Pts',(16.5081407912399,-17.6846995856018,
21.8325892139415));
#205608=CARTESIAN_POINT('Ctrl Pts',(16.5504396217143,-17.6131400990192,
21.8367073232935));
#205609=CARTESIAN_POINT('Ctrl Pts',(16.5960701372503,-17.543860837146,21.8408254326455));
#205610=CARTESIAN_POINT('Ctrl Pts',(16.6417225438979,-17.4745483387419,
21.8449455176489));
#205611=CARTESIAN_POINT('Ctrl Pts',(16.6907095365087,-17.407518624288,21.8490656026523));
#205612=CARTESIAN_POINT('Ctrl Pts',(16.7427579736743,-17.3431012484951,
21.8531856876557));
#205613=CARTESIAN_POINT('Ctrl Pts',(16.794892440757,-17.2785773983907,21.8573125826728));
#205614=CARTESIAN_POINT('Ctrl Pts',(16.850098139558,-17.2166748608617,21.8614394776899));
#205615=CARTESIAN_POINT('Ctrl Pts',(16.9080639839603,-17.1576874114779,
21.865566372707));
#205616=CARTESIAN_POINT('Ctrl Pts',(16.9486676843771,-17.1163681009799,
21.8684571648736));
#205617=CARTESIAN_POINT('Ctrl Pts',(16.9906249225133,-17.0764783454379,
21.8713479570401));
#205618=CARTESIAN_POINT('Ctrl Pts',(17.0338195571032,-17.0381069879455,
21.8742387492067));
#205619=CARTESIAN_POINT('Ctrl Pts',(17.0962945700832,-16.9826081724059,
21.8784198767899));
#205620=CARTESIAN_POINT('Ctrl Pts',(17.1616053466634,-16.9300690778322,
21.8826010043731));
#205621=CARTESIAN_POINT('Ctrl Pts',(17.2294395634032,-16.8807931313779,
21.8867821319562));
#205622=CARTESIAN_POINT('Ctrl Pts',(17.2971787572344,-16.8315862112052,
21.8909574025704));
#205623=CARTESIAN_POINT('Ctrl Pts',(17.3674340003121,-16.7856336283223,
21.8951326731846));
#205624=CARTESIAN_POINT('Ctrl Pts',(17.4398582963668,-16.7432000428021,
21.8993079437988));
#205625=CARTESIAN_POINT('Ctrl Pts',(17.5126335322061,-16.7005608407393,
21.9035034461398));
#205626=CARTESIAN_POINT('Ctrl Pts',(17.5875985480893,-16.6614751468356,
21.9076989484807));
#205627=CARTESIAN_POINT('Ctrl Pts',(17.6643699161775,-16.6261686467455,
21.9118944508217));
#205628=CARTESIAN_POINT('Ctrl Pts',(17.7406375998076,-16.5910937868593,
21.9160624271542));
#205629=CARTESIAN_POINT('Ctrl Pts',(17.8186875806148,-16.5597488751243,
21.9202304034868));
#205630=CARTESIAN_POINT('Ctrl Pts',(17.8981189457526,-16.532309345567,21.9243983798194));
#205631=CARTESIAN_POINT('Ctrl Pts',(17.9775252548952,-16.5048784715921,
21.9285650413968));
#205632=CARTESIAN_POINT('Ctrl Pts',(18.0583116477558,-16.4813506834989,
21.9327317029742));
#205633=CARTESIAN_POINT('Ctrl Pts',(18.1400589392981,-16.4618526115082,
21.9368983645517));
#205634=CARTESIAN_POINT('Ctrl Pts',(18.2218050628271,-16.442354818108,21.9410649665955));
#205635=CARTESIAN_POINT('Ctrl Pts',(18.3045116092594,-16.426886732127,21.9452315686392));
#205636=CARTESIAN_POINT('Ctrl Pts',(18.3877473464946,-16.4155242757045,
21.949398170683));
#205637=CARTESIAN_POINT('Ctrl Pts',(18.4719862643408,-16.4040248757484,
21.9536149897912));
#205638=CARTESIAN_POINT('Ctrl Pts',(18.5567667383605,-16.3967308160666,
21.9578318088995));
#205639=CARTESIAN_POINT('Ctrl Pts',(18.6416363028403,-16.3936667637997,
21.9620486280077));
#205640=CARTESIAN_POINT('Ctrl Pts',(18.7256174343069,-16.3906347866968,
21.9662213045387));
#205641=CARTESIAN_POINT('Ctrl Pts',(18.8096853344826,-16.3917446006535,
21.9703939810697));
#205642=CARTESIAN_POINT('Ctrl Pts',(18.8934033137617,-16.3969675963773,
21.9745666576007));
#205643=CARTESIAN_POINT('Ctrl Pts',(18.9784497667459,-16.4022734728939,
21.9788055479976));
#205644=CARTESIAN_POINT('Ctrl Pts',(19.0631346044503,-16.4118241506696,
21.9830444383944));
#205645=CARTESIAN_POINT('Ctrl Pts',(19.1470091266727,-16.4255353829343,
21.9872833287913));
#205646=CARTESIAN_POINT('Ctrl Pts',(19.2308836488952,-16.439246615199,21.9915222191882));
#205647=CARTESIAN_POINT('Ctrl Pts',(19.3139473893182,-16.4571182338667,
21.9957611095851));
#205648=CARTESIAN_POINT('Ctrl Pts',(19.3957679668415,-16.4790133121946,
21.9999999999819));
#205649=CARTESIAN_POINT('',(18.0722627314314,-16.4790050975816,22.));
#205650=CARTESIAN_POINT('Origin',(18.734,-18.952,22.));
#205651=CARTESIAN_POINT('',(16.1765333501007,-18.9488555363839,21.8332901097715));
#205652=CARTESIAN_POINT('Ctrl Pts',(16.1765333501007,-18.9488555363839,
21.8332901097715));
#205653=CARTESIAN_POINT('Ctrl Pts',(16.1744954273233,-18.6834061757001,
21.8464681376205));
#205654=CARTESIAN_POINT('Ctrl Pts',(16.3345563979949,-17.5672065717878,
21.90203810103));
#205655=CARTESIAN_POINT('Ctrl Pts',(17.2488902483963,-16.6993275322964,
21.9576080644395));
#205656=CARTESIAN_POINT('Ctrl Pts',(18.0722627314314,-16.4790050975816,
22.));
#205657=CARTESIAN_POINT('Ctrl Pts',(20.2910035915388,-20.9788220864065,
21.5499225011608));
#205658=CARTESIAN_POINT('Ctrl Pts',(19.9247545666378,-21.2588470681592,
21.5727725274258));
#205659=CARTESIAN_POINT('Ctrl Pts',(18.672556959445,-21.7916141725372,21.6380144892512));
#205660=CARTESIAN_POINT('Ctrl Pts',(16.6739013977444,-20.9887406839414,
21.7324703587881));
#205661=CARTESIAN_POINT('Ctrl Pts',(16.1810511496244,-19.5373209132916,
21.80407620206));
#205662=CARTESIAN_POINT('Ctrl Pts',(16.1765333501007,-18.9488555363839,
21.8332901097715));
#205663=CARTESIAN_POINT('Origin',(18.734,19.211,-1.76670989022852));
#205664=CARTESIAN_POINT('',(16.1740007447408,19.2090472910618,21.7667098902285));
#205665=CARTESIAN_POINT('Ctrl Pts',(20.2957383339893,17.178031980842,21.4832513393832));
#205666=CARTESIAN_POINT('Ctrl Pts',(20.245887425011,17.1392615823117,21.4864046693096));
#205667=CARTESIAN_POINT('Ctrl Pts',(19.5043144389604,16.6078642735819,21.5319499347965));
#205668=CARTESIAN_POINT('Ctrl Pts',(17.5061735829933,16.443821090153,21.6198871358438));
#205669=CARTESIAN_POINT('Ctrl Pts',(16.2398215703271,18.0973737800013,21.7112199895325));
#205670=CARTESIAN_POINT('Ctrl Pts',(16.1708575106781,19.0777088474958,21.7601609076608));
#205671=CARTESIAN_POINT('Ctrl Pts',(16.1719918287103,19.2090457587065,21.7667098902285));
#205672=CARTESIAN_POINT('',(19.3957680159044,21.6839866746762,21.9999999999818));
#205673=CARTESIAN_POINT('Ctrl Pts',(16.1740007447408,19.2090472910617,21.7667098902285));
#205674=CARTESIAN_POINT('Ctrl Pts',(16.1739377131957,19.291681576866,21.770833628557));
#205675=CARTESIAN_POINT('Ctrl Pts',(16.1778799213038,19.3744638154111,21.7749573668856));
#205676=CARTESIAN_POINT('Ctrl Pts',(16.1858438026722,19.4569674653686,21.7790811052141));
#205677=CARTESIAN_POINT('Ctrl Pts',(16.1937978799175,19.539369547271,21.7831997669178));
#205678=CARTESIAN_POINT('Ctrl Pts',(16.2057637505312,19.6214932533812,21.7873184286214));
#205679=CARTESIAN_POINT('Ctrl Pts',(16.2217058123253,19.7029125070335,21.7914370903251));
#205680=CARTESIAN_POINT('Ctrl Pts',(16.237637182478,19.7842771563645,21.795552989823));
#205681=CARTESIAN_POINT('Ctrl Pts',(16.257539363199,19.864937827131,21.799668889321));
#205682=CARTESIAN_POINT('Ctrl Pts',(16.2813251278132,19.9444752697558,21.803784788819));
#205683=CARTESIAN_POINT('Ctrl Pts',(16.3051025310591,20.0239847527225,21.807899241462));
#205684=CARTESIAN_POINT('Ctrl Pts',(16.3327606729939,20.1023713378542,21.812013694105));
#205685=CARTESIAN_POINT('Ctrl Pts',(16.3641619718452,20.1792291672488,21.816128146748));
#205686=CARTESIAN_POINT('Ctrl Pts',(16.3955622525032,20.2560845045131,21.820242465979));
#205687=CARTESIAN_POINT('Ctrl Pts',(16.4307052681111,20.331410746752,21.8243567852101));
#205688=CARTESIAN_POINT('Ctrl Pts',(16.4694052055202,20.4048217692834,21.8284711044412));
#205689=CARTESIAN_POINT('Ctrl Pts',(16.5081407935446,20.4783004184906,21.8325892138079));
#205690=CARTESIAN_POINT('Ctrl Pts',(16.5504396244287,20.5498599054295,21.8367073231746));
#205691=CARTESIAN_POINT('Ctrl Pts',(16.596070140308,20.6191391674964,21.8408254325413));
#205692=CARTESIAN_POINT('Ctrl Pts',(16.6417225473624,20.6884516661905,21.8449455175651));
#205693=CARTESIAN_POINT('Ctrl Pts',(16.6907095403228,20.7554813807654,21.849065602589));
#205694=CARTESIAN_POINT('Ctrl Pts',(16.7427579777409,20.819898756538,21.8531856876128));
#205695=CARTESIAN_POINT('Ctrl Pts',(16.7948924451882,20.88442260676,21.8573125826592));
#205696=CARTESIAN_POINT('Ctrl Pts',(16.8500981442698,20.9463251442536,21.8614394777056));
#205697=CARTESIAN_POINT('Ctrl Pts',(16.9080639888335,21.0053125934813,21.865566372752));
#205698=CARTESIAN_POINT('Ctrl Pts',(16.9486676888643,21.0466319033619,21.8684571649036));
#205699=CARTESIAN_POINT('Ctrl Pts',(16.990624926523,21.0865216582628,21.8713479570551));
#205700=CARTESIAN_POINT('Ctrl Pts',(17.0338195605382,21.124893015106,21.8742387492067));
#205701=CARTESIAN_POINT('Ctrl Pts',(17.096294549636,21.1803918092294,21.8784198752255));
#205702=CARTESIAN_POINT('Ctrl Pts',(17.1616053008015,21.2329308852276,21.8826010012442));
#205703=CARTESIAN_POINT('Ctrl Pts',(17.2294394909469,21.2822068159887,21.886782127263));
#205704=CARTESIAN_POINT('Ctrl Pts',(17.2971786580471,21.3314137203636,21.8909573963043));
#205705=CARTESIAN_POINT('Ctrl Pts',(17.3674338732044,21.377366290339,21.8951326653455));
#205706=CARTESIAN_POINT('Ctrl Pts',(17.4398581404809,21.4197998658639,21.8993079343868));
#205707=CARTESIAN_POINT('Ctrl Pts',(17.5126333816213,21.462439077932,21.9035034371199));
#205708=CARTESIAN_POINT('Ctrl Pts',(17.5875984040009,21.5015247814357,21.907698939853));
#205709=CARTESIAN_POINT('Ctrl Pts',(17.6643697795486,21.5368312904201,21.9118944425862));
#205710=CARTESIAN_POINT('Ctrl Pts',(17.7406374344996,21.5719061425448,21.916062417336));
#205711=CARTESIAN_POINT('Ctrl Pts',(17.8186873858889,21.603251049355,21.9202303920859));
#205712=CARTESIAN_POINT('Ctrl Pts',(17.8981187211547,21.6306905768457,21.9243983668358));
#205713=CARTESIAN_POINT('Ctrl Pts',(17.9775250004187,21.6581214487492,21.9285650268302));
#205714=CARTESIAN_POINT('Ctrl Pts',(18.0583113629463,21.681649237629,21.9327316868246));
#205715=CARTESIAN_POINT('Ctrl Pts',(18.1400586239765,21.7011473132823,21.936898346819));
#205716=CARTESIAN_POINT('Ctrl Pts',(18.2218047170262,21.720645110353,21.9410649472815));
#205717=CARTESIAN_POINT('Ctrl Pts',(18.3045112328003,21.7361132028771,21.9452315477439));
#205718=CARTESIAN_POINT('Ctrl Pts',(18.3877469394689,21.7474756687327,21.9493981482063));
#205719=CARTESIAN_POINT('Ctrl Pts',(18.471985895769,21.7589750877077,21.9536149691876));
#205720=CARTESIAN_POINT('Ctrl Pts',(18.5567664092282,21.7662691624329,21.9578317901689));
#205721=CARTESIAN_POINT('Ctrl Pts',(18.6416360132955,21.7693332257468,21.9620486111502));
#205722=CARTESIAN_POINT('Ctrl Pts',(18.7256171152011,21.7723652112997,21.9662212861195));
#205723=CARTESIAN_POINT('Ctrl Pts',(18.8096849858173,21.7712554086671,21.9703939610888));
#205724=CARTESIAN_POINT('Ctrl Pts',(18.8934029358148,21.766032427202,21.9745666360581));
#205725=CARTESIAN_POINT('Ctrl Pts',(18.9784494629181,21.7607265586906,21.9788055300454));
#205726=CARTESIAN_POINT('Ctrl Pts',(19.0631343741421,21.7511758815698,21.9830444240327));
#205727=CARTESIAN_POINT('Ctrl Pts',(19.1470089679579,21.7374646430113,21.98728331802));
#205728=CARTESIAN_POINT('Ctrl Pts',(19.2308835617738,21.7237534044529,21.9915222120073));
#205729=CARTESIAN_POINT('Ctrl Pts',(19.3139473718607,21.7058817725444,21.9957611059945));
#205730=CARTESIAN_POINT('Ctrl Pts',(19.3957680159044,21.6839866746762,21.9999999999818));
#205731=CARTESIAN_POINT('',(18.0722627314313,21.6839949024184,22.));
#205732=CARTESIAN_POINT('Origin',(18.734,19.211,22.));
#205733=CARTESIAN_POINT('',(16.1765333526442,19.2141444406009,21.8332901097715));
#205734=CARTESIAN_POINT('Ctrl Pts',(16.1765333526442,19.2141444406009,21.8332901097715));
#205735=CARTESIAN_POINT('Ctrl Pts',(16.1744954308812,19.4795937966726,21.8464681376205));
#205736=CARTESIAN_POINT('Ctrl Pts',(16.3345564048251,20.5957933867983,21.90203810103));
#205737=CARTESIAN_POINT('Ctrl Pts',(17.2488902483962,21.4636724677035,21.9576080644395));
#205738=CARTESIAN_POINT('Ctrl Pts',(18.0722627314313,21.6839949024184,22.));
#205739=CARTESIAN_POINT('Ctrl Pts',(20.2910035798173,17.1841778967012,21.5499225020685));
#205740=CARTESIAN_POINT('Ctrl Pts',(19.9247545573495,16.9041529176524,21.5727725280309));
#205741=CARTESIAN_POINT('Ctrl Pts',(18.6725569530959,16.3713858130565,21.6380144895538));
#205742=CARTESIAN_POINT('Ctrl Pts',(16.6739013896572,17.1742593445012,21.7324703587881));
#205743=CARTESIAN_POINT('Ctrl Pts',(16.1810511499193,18.6256790739174,21.80407620206));
#205744=CARTESIAN_POINT('Ctrl Pts',(16.1765333526442,19.2141444406009,21.8332901097715));
#205745=CARTESIAN_POINT('Origin',(-18.734,19.211,-1.76670989022852));
#205746=CARTESIAN_POINT('',(-21.2939992552807,19.2090473192565,21.7667098902285));
#205747=CARTESIAN_POINT('Ctrl Pts',(-17.1722616694474,17.1780320626177,
21.4832513372676));
#205748=CARTESIAN_POINT('Ctrl Pts',(-17.2221125877366,17.1392616549198,
21.4864046678992));
#205749=CARTESIAN_POINT('Ctrl Pts',(-17.9636855620214,16.6078643332858,
21.5319499340913));
#205750=CARTESIAN_POINT('Ctrl Pts',(-19.9618263432431,16.4438210470481,
21.6198871358438));
#205751=CARTESIAN_POINT('Ctrl Pts',(-21.2281784392051,18.0973738826004,
21.7112199895325));
#205752=CARTESIAN_POINT('Ctrl Pts',(-21.2971424588611,19.0777088858588,
21.7601609076608));
#205753=CARTESIAN_POINT('Ctrl Pts',(-21.2960081347233,19.2090457869513,
21.7667098902285));
#205754=CARTESIAN_POINT('',(-18.0722321029123,21.6839867064714,21.999999999982));
#205755=CARTESIAN_POINT('Ctrl Pts',(-21.2939992552807,19.2090473192565,
21.7667098902285));
#205756=CARTESIAN_POINT('Ctrl Pts',(-21.2940622859128,19.291681601191,21.7708336286224));
#205757=CARTESIAN_POINT('Ctrl Pts',(-21.2901200772654,19.3744638362772,
21.7749573670163));
#205758=CARTESIAN_POINT('Ctrl Pts',(-21.2821561956048,19.456967483218,21.7790811054102));
#205759=CARTESIAN_POINT('Ctrl Pts',(-21.2742021181198,19.5393695615683,
21.7831997671522));
#205760=CARTESIAN_POINT('Ctrl Pts',(-21.2622362475653,19.621493264571,21.7873184288942));
#205761=CARTESIAN_POINT('Ctrl Pts',(-21.2462941860021,19.7029125155758,
21.7914370906363));
#205762=CARTESIAN_POINT('Ctrl Pts',(-21.2303628161442,19.7842771619339,
21.795552990156));
#205763=CARTESIAN_POINT('Ctrl Pts',(-21.2104606359213,19.8649378301924,
21.7996688896757));
#205764=CARTESIAN_POINT('Ctrl Pts',(-21.1866748718834,19.9444752707705,
21.8037847891954));
#205765=CARTESIAN_POINT('Ctrl Pts',(-21.1628974693084,20.0239847513738,
21.8078992418438));
#205766=CARTESIAN_POINT('Ctrl Pts',(-21.1352393281534,20.102371334612,21.8120136944921));
#205767=CARTESIAN_POINT('Ctrl Pts',(-21.1038380300699,20.1792291625614,
21.8161281471405));
#205768=CARTESIAN_POINT('Ctrl Pts',(-21.0724377503042,20.2560844980759,
21.8202424663606));
#205769=CARTESIAN_POINT('Ctrl Pts',(-21.0372947356062,20.3314107390252,
21.8243567855807));
#205770=CARTESIAN_POINT('Ctrl Pts',(-20.9985947990105,20.404821760689,21.8284711048008));
#205771=CARTESIAN_POINT('Ctrl Pts',(-20.959859212032,20.4783004085882,21.8325892141319));
#205772=CARTESIAN_POINT('Ctrl Pts',(-20.9175603821396,20.5498598946646,
21.836707323463));
#205773=CARTESIAN_POINT('Ctrl Pts',(-20.8719298670911,20.6191391562625,
21.8408254327941));
#205774=CARTESIAN_POINT('Ctrl Pts',(-20.8262774610213,20.6884516542547,
21.8449455177684));
#205775=CARTESIAN_POINT('Ctrl Pts',(-20.7772904689067,20.7554813685366,
21.8490656027427));
#205776=CARTESIAN_POINT('Ctrl Pts',(-20.7252420320998,20.8198987443587,
21.8531856877171));
#205777=CARTESIAN_POINT('Ctrl Pts',(-20.6731075655348,20.884422594296,21.8573125826926));
#205778=CARTESIAN_POINT('Ctrl Pts',(-20.617901867132,20.9463251318754,21.861439477668));
#205779=CARTESIAN_POINT('Ctrl Pts',(-20.5599360229587,21.0053125814812,
21.8655663726435));
#205780=CARTESIAN_POINT('Ctrl Pts',(-20.5193323219955,21.0466318928538,
21.8684571648312));
#205781=CARTESIAN_POINT('Ctrl Pts',(-20.477375083183,21.0865216493047,21.871347957019));
#205782=CARTESIAN_POINT('Ctrl Pts',(-20.4341804477789,21.1248930077176,
21.8742387492067));
#205783=CARTESIAN_POINT('Ctrl Pts',(-20.3717054008517,21.1803918536987,
21.8784198790135));
#205784=CARTESIAN_POINT('Ctrl Pts',(-20.3063945881463,21.2329309746761,
21.8826010088204));
#205785=CARTESIAN_POINT('Ctrl Pts',(-20.2385603336045,21.2822069434375,
21.8867821386272));
#205786=CARTESIAN_POINT('Ctrl Pts',(-20.1708211017769,21.3314138860656,
21.8909574114772));
#205787=CARTESIAN_POINT('Ctrl Pts',(-20.1005658190123,21.3773664872955,
21.8951326843272));
#205788=CARTESIAN_POINT('Ctrl Pts',(-20.0281414820515,21.4198000870231,
21.8993079571772));
#205789=CARTESIAN_POINT('Ctrl Pts',(-19.9553662537474,21.4624392748643,
21.9035034589607));
#205790=CARTESIAN_POINT('Ctrl Pts',(-19.8804012470982,21.5015249551222,
21.9076989607443));
#205791=CARTESIAN_POINT('Ctrl Pts',(-19.8036298896135,21.5368314425696,
21.9118944625278));
#205792=CARTESIAN_POINT('Ctrl Pts',(-19.7273621652182,21.571906313488,21.9160624411101));
#205793=CARTESIAN_POINT('Ctrl Pts',(-19.6493121425953,21.6032512322234,
21.9202304196923));
#205794=CARTESIAN_POINT('Ctrl Pts',(-19.5698807349969,21.6306907647179,
21.9243983982746));
#205795=CARTESIAN_POINT('Ctrl Pts',(-19.4904743833841,21.6581216416371,
21.9285650621022));
#205796=CARTESIAN_POINT('Ctrl Pts',(-19.4096879474075,21.6816494286122,
21.9327317259298));
#205797=CARTESIAN_POINT('Ctrl Pts',(-19.3279406124946,21.7011474953965,
21.9368983897574));
#205798=CARTESIAN_POINT('Ctrl Pts',(-19.2461944456416,21.7206452835795,
21.941064994049));
#205799=CARTESIAN_POINT('Ctrl Pts',(-19.1634878556314,21.7361133602598,
21.9452315983405));
#205800=CARTESIAN_POINT('Ctrl Pts',(-19.0802520749481,21.7474758032739,
21.9493982026321));
#205801=CARTESIAN_POINT('Ctrl Pts',(-18.9960132117624,21.7589751761959,
21.9536150190779));
#205802=CARTESIAN_POINT('Ctrl Pts',(-18.9112327938041,21.7662692144946,
21.9578318355238));
#205803=CARTESIAN_POINT('Ctrl Pts',(-18.8263632855961,21.7693332510589,
21.9620486519696));
#205804=CARTESIAN_POINT('Ctrl Pts',(-18.742382112111,21.7723652161511,21.9662213307204));
#205805=CARTESIAN_POINT('Ctrl Pts',(-18.6583141699189,21.7712553860981,
21.9703940094712));
#205806=CARTESIAN_POINT('Ctrl Pts',(-18.5745961490186,21.7660323701065,
21.9745666882221));
#205807=CARTESIAN_POINT('Ctrl Pts',(-18.489549801391,21.7607264822116,21.9788055735154));
#205808=CARTESIAN_POINT('Ctrl Pts',(-18.404865068191,21.7511758035055,21.9830444588087));
#205809=CARTESIAN_POINT('Ctrl Pts',(-18.3209906477349,21.7374645801874,
21.987283344102));
#205810=CARTESIAN_POINT('Ctrl Pts',(-18.2371162272788,21.7237533568693,
21.9915222293954));
#205811=CARTESIAN_POINT('Ctrl Pts',(-18.15405258588,21.7058817570232,21.9957611146887));
#205812=CARTESIAN_POINT('Ctrl Pts',(-18.0722321029123,21.6839867064714,
21.999999999982));
#205813=CARTESIAN_POINT('',(-19.3957372685686,21.6839949024184,22.));
#205814=CARTESIAN_POINT('Origin',(-18.734,19.211,22.));
#205815=CARTESIAN_POINT('',(-21.2914665292272,19.2141433713253,21.8332901097715));
#205816=CARTESIAN_POINT('Ctrl Pts',(-21.2914665292272,19.2141433713253,
21.8332901097715));
#205817=CARTESIAN_POINT('Ctrl Pts',(-21.2935044038853,19.4795925132556,
21.8464681376205));
#205818=CARTESIAN_POINT('Ctrl Pts',(-21.1334432779756,20.5957914633395,
21.90203810103));
#205819=CARTESIAN_POINT('Ctrl Pts',(-20.2191097516038,21.4636724677035,
21.9576080644395));
#205820=CARTESIAN_POINT('Ctrl Pts',(-19.3957372685686,21.6839949024184,
22.));
#205821=CARTESIAN_POINT('Ctrl Pts',(-17.1769962058593,17.1841776921994,
21.549922496891));
#205822=CARTESIAN_POINT('Ctrl Pts',(-17.5432452683728,16.9041525164483,
21.5727725245792));
#205823=CARTESIAN_POINT('Ctrl Pts',(-18.7954430079984,16.371385010207,21.6380144878279));
#205824=CARTESIAN_POINT('Ctrl Pts',(-20.7940989859098,17.1742606647151,
21.7324703587881));
#205825=CARTESIAN_POINT('Ctrl Pts',(-21.2869488363774,18.6256784793645,
21.80407620206));
#205826=CARTESIAN_POINT('Ctrl Pts',(-21.2914665292272,19.2141433713253,
21.8332901097715));
#205827=CARTESIAN_POINT('Origin',(26.8463464956315,10.1295,7.));
#205828=CARTESIAN_POINT('',(18.7216535115672,10.1295873228123,12.0987228108905));
#205829=CARTESIAN_POINT('Ctrl Pts',(18.9778214339751,14.6099559957068,9.43455988473872));
#205830=CARTESIAN_POINT('Ctrl Pts',(18.9452723572074,14.27750379166,10.0450302603514));
#205831=CARTESIAN_POINT('Ctrl Pts',(18.8739413988038,13.2738298860402,11.2340275217565));
#205832=CARTESIAN_POINT('Ctrl Pts',(18.7885520913344,11.5585268032384,12.0007214198279));
#205833=CARTESIAN_POINT('Ctrl Pts',(18.7357118606328,10.4298968038467,12.0989142199688));
#205834=CARTESIAN_POINT('Ctrl Pts',(18.7216535115672,10.1295873228123,12.0987228108905));
#205835=CARTESIAN_POINT('',(17.734,14.4077184404108,4.2257166734219));
#205836=CARTESIAN_POINT('Ctrl Pts',(18.7216535043684,10.1295871737727,12.0989999992548));
#205837=CARTESIAN_POINT('Ctrl Pts',(18.7147113410273,9.98128307520553,12.0990025346986));
#205838=CARTESIAN_POINT('Ctrl Pts',(18.7077691776862,9.8329749558716,12.0925306029392));
#205839=CARTESIAN_POINT('Ctrl Pts',(18.7008270143451,9.68523504562768,12.0796092025191));
#205840=CARTESIAN_POINT('Ctrl Pts',(18.6938850789891,9.53749998725783,12.0666882264461));
#205841=CARTESIAN_POINT('Ctrl Pts',(18.6869431436331,9.3903334278217,12.0473182361383));
#205842=CARTESIAN_POINT('Ctrl Pts',(18.6800012082771,9.244302805183,12.0215761396486));
#205843=CARTESIAN_POINT('Ctrl Pts',(18.6730576317816,9.0982376595178,11.9958279574827));
#205844=CARTESIAN_POINT('Ctrl Pts',(18.6661140552862,8.95330931088689,11.9637047165393));
#205845=CARTESIAN_POINT('Ctrl Pts',(18.6591704787908,8.81007598055744,11.9253346340039));
#205846=CARTESIAN_POINT('Ctrl Pts',(18.6552746238124,8.72971159148627,11.9038062073836));
#205847=CARTESIAN_POINT('Ctrl Pts',(18.6513787688341,8.64988059910993,11.8803121723026));
#205848=CARTESIAN_POINT('Ctrl Pts',(18.6474829138558,8.57067970016459,11.8548821069951));
#205849=CARTESIAN_POINT('Ctrl Pts',(18.6405493036326,8.4297226661706,11.8096231941828));
#205850=CARTESIAN_POINT('Ctrl Pts',(18.6336156934094,8.29071373380833,11.7582135060853));
#205851=CARTESIAN_POINT('Ctrl Pts',(18.6266820831862,8.15419024687287,11.7008459216614));
#205852=CARTESIAN_POINT('Ctrl Pts',(18.6197497891957,8.01769267669309,11.6434892275371));
#205853=CARTESIAN_POINT('Ctrl Pts',(18.6128174952052,7.88367991517738,11.5801770216112));
#205854=CARTESIAN_POINT('Ctrl Pts',(18.6058852012147,7.75266950923779,11.5111503874492));
#205855=CARTESIAN_POINT('Ctrl Pts',(18.5989526626174,7.62165448058108,11.4421213176745));
#205856=CARTESIAN_POINT('Ctrl Pts',(18.5920201240202,7.49364231349697,11.3673775673167));
#205857=CARTESIAN_POINT('Ctrl Pts',(18.5850875854229,7.36912660488231,11.2872065170139));
#205858=CARTESIAN_POINT('Ctrl Pts',(18.5781554218558,7.24461763220445,11.2070398037311));
#205859=CARTESIAN_POINT('Ctrl Pts',(18.5712232582886,7.12360501695346,11.121446557744));
#205860=CARTESIAN_POINT('Ctrl Pts',(18.5642910947215,7.00655398674484,11.030757893783));
#205861=CARTESIAN_POINT('Ctrl Pts',(18.5573573897854,6.8894769301988,10.9400490651659));
#205862=CARTESIAN_POINT('Ctrl Pts',(18.5504236848492,6.77636348017962,10.8442427572896));
#205863=CARTESIAN_POINT('Ctrl Pts',(18.5434899799131,6.6676468407924,10.7437112207119));
#205864=CARTESIAN_POINT('Ctrl Pts',(18.5393724095913,6.60308562684493,10.6840107178447));
#205865=CARTESIAN_POINT('Ctrl Pts',(18.5352548392694,6.54007433979697,10.622644599298));
#205866=CARTESIAN_POINT('Ctrl Pts',(18.5311372689476,6.47869775743707,10.5596971761229));
#205867=CARTESIAN_POINT('Ctrl Pts',(18.5242037115753,6.37534601797689,10.4537003051742));
#205868=CARTESIAN_POINT('Ctrl Pts',(18.5172701542029,6.27659580949282,10.3431810703944));
#205869=CARTESIAN_POINT('Ctrl Pts',(18.5103365968306,6.18283159101337,10.2285615170703));
#205870=CARTESIAN_POINT('Ctrl Pts',(18.5034043559565,6.089085175867,10.113963726953));
#205871=CARTESIAN_POINT('Ctrl Pts',(18.4964721150824,6.0003230711042,9.99526742733144));
#205872=CARTESIAN_POINT('Ctrl Pts',(18.4895398742083,5.91688967035563,9.87292798562261));
#205873=CARTESIAN_POINT('Ctrl Pts',(18.4826073886049,5.83345332415193,9.75058422495596));
#205874=CARTESIAN_POINT('Ctrl Pts',(18.4756749030014,5.75534624741186,9.62459733606426));
#205875=CARTESIAN_POINT('Ctrl Pts',(18.4687424173979,5.68286999196541,9.49545237815638));
#205876=CARTESIAN_POINT('Ctrl Pts',(18.4618103066269,5.61039765523575,9.36631440298387));
#205877=CARTESIAN_POINT('Ctrl Pts',(18.4548781958558,5.5435556915652,9.23401898922316));
#205878=CARTESIAN_POINT('Ctrl Pts',(18.4479460850847,5.48260010633888,9.09907655369981));
#205879=CARTESIAN_POINT('Ctrl Pts',(18.4410124321748,5.42163096074452,8.96410409846483));
#205880=CARTESIAN_POINT('Ctrl Pts',(18.434078779265,5.36655094628959,8.82648374621635));
#205881=CARTESIAN_POINT('Ctrl Pts',(18.4271451263551,5.3175685098331,8.68674726439385));
#205882=CARTESIAN_POINT('Ctrl Pts',(18.4230272922499,5.28847828134614,8.6037590245624));
#205883=CARTESIAN_POINT('Ctrl Pts',(18.4189094581446,5.26153778917509,8.52002479046549));
#205884=CARTESIAN_POINT('Ctrl Pts',(18.4147916240394,5.23678246616714,8.43565878053404));
#205885=CARTESIAN_POINT('Ctrl Pts',(18.4078580499257,5.19509966341243,8.29360400912006));
#205886=CARTESIAN_POINT('Ctrl Pts',(18.400924475812,5.15960044824281,8.1497081866558));
#205887=CARTESIAN_POINT('Ctrl Pts',(18.3939909016982,5.13042688503271,8.00452426113619));
#205888=CARTESIAN_POINT('Ctrl Pts',(18.3870586444984,5.10125886284241,7.85936791082228));
#205889=CARTESIAN_POINT('Ctrl Pts',(18.3801263872986,5.07841416062936,7.71292426949538));
#205890=CARTESIAN_POINT('Ctrl Pts',(18.3731941300988,5.06198383767688,7.56575696601455));
#205891=CARTESIAN_POINT('Ctrl Pts',(18.3662616289537,5.04555293654322,7.41858448373312));
#205892=CARTESIAN_POINT('Ctrl Pts',(18.3593291278085,5.03553690634891,7.27068861649685));
#205893=CARTESIAN_POINT('Ctrl Pts',(18.3523966266634,5.03197504813123,7.12263916615529));
#205894=CARTESIAN_POINT('Ctrl Pts',(18.3454645008326,5.02841338274678,6.97459773097103));
#205895=CARTESIAN_POINT('Ctrl Pts',(18.3385323750019,5.0313051971733,6.82640305983149));
#205896=CARTESIAN_POINT('Ctrl Pts',(18.3316002491711,5.04063767405535,6.67862603157506));
#205897=CARTESIAN_POINT('Ctrl Pts',(18.3246665820787,5.0499722258837,6.53081614715388));
#205898=CARTESIAN_POINT('Ctrl Pts',(18.3177329149862,5.06575028063441,6.38342442119573));
#205899=CARTESIAN_POINT('Ctrl Pts',(18.3107992478938,5.08790700112659,6.23701832675314));
#205900=CARTESIAN_POINT('Ctrl Pts',(18.3066814916396,5.10106540246934,6.15007088566497));
#205901=CARTESIAN_POINT('Ctrl Pts',(18.3025637353854,5.11647251715666,6.06347097260691));
#205902=CARTESIAN_POINT('Ctrl Pts',(18.2984459791312,5.13410616806531,5.97733609437465));
#205903=CARTESIAN_POINT('Ctrl Pts',(18.2915124969837,5.16379772730853,5.83230209924856));
#205904=CARTESIAN_POINT('Ctrl Pts',(18.2845790148362,5.19981494209206,5.6885370247223));
#205905=CARTESIAN_POINT('Ctrl Pts',(18.2776455326886,5.24202440558095,5.54659595639818));
#205906=CARTESIAN_POINT('Ctrl Pts',(18.2707133673131,5.28422585286128,5.4046818448063));
#205907=CARTESIAN_POINT('Ctrl Pts',(18.2637812019376,5.33261710836953,5.26459136499318));
#205908=CARTESIAN_POINT('Ctrl Pts',(18.256849036562,5.38701469658392,5.12686515517903));
#205909=CARTESIAN_POINT('Ctrl Pts',(18.2499166261359,5.44141420774157,4.98913407677243));
#205910=CARTESIAN_POINT('Ctrl Pts',(18.2429842157098,5.5018203581369,4.85376774430463));
#205911=CARTESIAN_POINT('Ctrl Pts',(18.2360518052837,5.5680010490493,4.72128801282926));
#205912=CARTESIAN_POINT('Ctrl Pts',(18.2291197693284,5.63417816505214,4.58881543756594));
#205913=CARTESIAN_POINT('Ctrl Pts',(18.2221877333731,5.70612904882591,4.45922944662038));
#205914=CARTESIAN_POINT('Ctrl Pts',(18.2152556974179,5.78357504674778,4.33302844021544));
#205915=CARTESIAN_POINT('Ctrl Pts',(18.2083221181144,5.86103828724344,4.20679933642362));
#205916=CARTESIAN_POINT('Ctrl Pts',(18.201388538811,5.94399891348856,4.08395700490077));
#205917=CARTESIAN_POINT('Ctrl Pts',(18.1944549595075,6.03213390326059,3.96497247635372));
#205918=CARTESIAN_POINT('Ctrl Pts',(18.1903367510793,6.08448179484874,3.8943014611626));
#205919=CARTESIAN_POINT('Ctrl Pts',(18.1862185426512,6.13865425945979,3.82499084626316));
#205920=CARTESIAN_POINT('Ctrl Pts',(18.182100334223,6.19457664874617,3.75713410395105));
#205921=CARTESIAN_POINT('Ctrl Pts',(18.1751666155273,6.28873169768777,3.6428855002175));
#205922=CARTESIAN_POINT('Ctrl Pts',(18.1682328968315,6.38788205597123,3.53272058770171));
#205923=CARTESIAN_POINT('Ctrl Pts',(18.1612991781358,6.49164988118888,3.42706737915953));
#205924=CARTESIAN_POINT('Ctrl Pts',(18.1543667758962,6.59539800474326,3.32143423024503));
#205925=CARTESIAN_POINT('Ctrl Pts',(18.1474343736566,6.7037616146166,3.22031131194666));
#205926=CARTESIAN_POINT('Ctrl Pts',(18.140501971417,6.81632539466401,3.12409042487357));
#205927=CARTESIAN_POINT('Ctrl Pts',(18.133569325952,6.92889312404455,3.02786616186255));
#205928=CARTESIAN_POINT('Ctrl Pts',(18.1266366804871,7.04566106939944,2.93654449155148));
#205929=CARTESIAN_POINT('Ctrl Pts',(18.1197040350221,7.16617974834542,2.85047784845847));
#205930=CARTESIAN_POINT('Ctrl Pts',(18.1127717656245,7.28669188965198,2.76441587412456));
#205931=CARTESIAN_POINT('Ctrl Pts',(18.1058394962268,7.41095408788013,2.68360854794937));
#205932=CARTESIAN_POINT('Ctrl Pts',(18.0989072268292,7.53848670899882,2.60836577959238));
#205933=CARTESIAN_POINT('Ctrl Pts',(18.0919734185825,7.66604764024739,2.53310630858688));
#205934=CARTESIAN_POINT('Ctrl Pts',(18.0850396103359,7.79688016019581,2.46341403160105));
#205935=CARTESIAN_POINT('Ctrl Pts',(18.0781058020892,7.93047824811586,2.39955389828982));
#205936=CARTESIAN_POINT('Ctrl Pts',(18.0739887644978,8.00980382657889,2.36163612495559));
#205937=CARTESIAN_POINT('Ctrl Pts',(18.0698717269063,8.09010394201902,2.32577362636113));
#205938=CARTESIAN_POINT('Ctrl Pts',(18.0657546893148,8.17126896360323,2.29201399661252));
#205939=CARTESIAN_POINT('Ctrl Pts',(18.0588213573683,8.30795560407876,2.2351608068521));
#205940=CARTESIAN_POINT('Ctrl Pts',(18.0518880254217,8.44714343822144,2.18425443098161));
#205941=CARTESIAN_POINT('Ctrl Pts',(18.0449546934752,8.58829824151367,2.13949610229159));
#205942=CARTESIAN_POINT('Ctrl Pts',(18.0380226783627,8.72942623555296,2.09474627446251));
#205943=CARTESIAN_POINT('Ctrl Pts',(18.0310906632502,8.87252013840123,2.0561422639854));
#205944=CARTESIAN_POINT('Ctrl Pts',(18.0241586481377,9.01702957132649,2.02383575981188));
#205945=CARTESIAN_POINT('Ctrl Pts',(18.0172263866156,9.16154414107234,1.99152810725164));
#205946=CARTESIAN_POINT('Ctrl Pts',(18.0102941250934,9.30747401965934,1.96551848432784));
#205947=CARTESIAN_POINT('Ctrl Pts',(18.0033618635713,9.45425707373931,1.94590779758275));
#205948=CARTESIAN_POINT('Ctrl Pts',(17.9964299753957,9.60103222261469,1.92629816699833));
#205949=CARTESIAN_POINT('Ctrl Pts',(17.9894980872201,9.74866012719367,1.9130868258486));
#205950=CARTESIAN_POINT('Ctrl Pts',(17.9825661990445,9.89657192712221,1.9063229869901));
#205951=CARTESIAN_POINT('Ctrl Pts',(17.9756327645019,10.0445167232454,1.89955763925304));
#205952=CARTESIAN_POINT('Ctrl Pts',(17.9686993299592,10.1927452108641,1.89924268284508));
#205953=CARTESIAN_POINT('Ctrl Pts',(17.9617658954166,10.3406862695542,1.90537524840624));
#205954=CARTESIAN_POINT('Ctrl Pts',(17.9576469450799,10.4285737183722,1.90901842594365));
#205955=CARTESIAN_POINT('Ctrl Pts',(17.9535279947433,10.5163597158814,1.9149360686311));
#205956=CARTESIAN_POINT('Ctrl Pts',(17.9494090444066,10.6039249349976,1.92311887266872));
#205957=CARTESIAN_POINT('Ctrl Pts',(17.9424753834828,10.7513283966681,1.93689344724857));
#205958=CARTESIAN_POINT('Ctrl Pts',(17.9355417225589,10.8981569837258,1.9570943475134));
#205959=CARTESIAN_POINT('Ctrl Pts',(17.9286080616351,11.043844383057,1.98364919994901));
#205960=CARTESIAN_POINT('Ctrl Pts',(17.921675718497,11.1895040935834,2.01019900546824));
#205961=CARTESIAN_POINT('Ctrl Pts',(17.914743375359,11.3340227240848,2.04310029455465));
#205962=CARTESIAN_POINT('Ctrl Pts',(17.9078110322209,11.4768428889456,2.08222935268351));
#205963=CARTESIAN_POINT('Ctrl Pts',(17.9008784472619,11.6196680358023,2.12135977575131));
#205964=CARTESIAN_POINT('Ctrl Pts',(17.893945862303,11.760794278772,2.16671831846166));
#205965=CARTESIAN_POINT('Ctrl Pts',(17.887013277344,11.8996776268284,2.2181308916412));
#205966=CARTESIAN_POINT('Ctrl Pts',(17.8800810690987,12.0385534280233,2.26954067108361));
#205967=CARTESIAN_POINT('Ctrl Pts',(17.8731488608534,12.1751862684927,2.32700370709501));
#205968=CARTESIAN_POINT('Ctrl Pts',(17.8662166526081,12.3090504196554,2.3902970846073));
#205969=CARTESIAN_POINT('Ctrl Pts',(17.8592829059654,12.4429442779832,2.45360450820139));
#205970=CARTESIAN_POINT('Ctrl Pts',(17.8523491593228,12.5740679203451,2.52274471727729));
#205971=CARTESIAN_POINT('Ctrl Pts',(17.8454154126802,12.7019180096239,2.59744771936065));
#205972=CARTESIAN_POINT('Ctrl Pts',(17.8412980749529,12.7778368487668,2.64180721281625));
#205973=CARTESIAN_POINT('Ctrl Pts',(17.8371807372257,12.8526018488398,2.68812732988671));
#205974=CARTESIAN_POINT('Ctrl Pts',(17.8330633994984,12.9261120521225,2.73634405352367));
#205975=CARTESIAN_POINT('Ctrl Pts',(17.8261558289376,13.0494385678835,2.8172362325956));
#205976=CARTESIAN_POINT('Ctrl Pts',(17.8192482583768,13.1692774271192,2.90349891677528));
#205977=CARTESIAN_POINT('Ctrl Pts',(17.812340687816,13.2851650747901,2.99480600522892));
#205978=CARTESIAN_POINT('Ctrl Pts',(17.805433747039,13.4010421566397,3.08610476894398));
#205979=CARTESIAN_POINT('Ctrl Pts',(17.7985268062619,13.512968479376,3.18244681517665));
#205980=CARTESIAN_POINT('Ctrl Pts',(17.7916198654848,13.6205122246208,3.28346469846606));
#205981=CARTESIAN_POINT('Ctrl Pts',(17.7847138003811,13.728042335292,3.38446977454133));
#205982=CARTESIAN_POINT('Ctrl Pts',(17.7778077352774,13.8311907337587,3.49014927375184));
#205983=CARTESIAN_POINT('Ctrl Pts',(17.7709016701737,13.929561225329,3.60009769496956));
#205984=CARTESIAN_POINT('Ctrl Pts',(17.7639943665765,14.0279493580916,3.71006583369829));
#205985=CARTESIAN_POINT('Ctrl Pts',(17.7570870629792,14.1215576465777,3.82430417516951));
#205986=CARTESIAN_POINT('Ctrl Pts',(17.7501797593819,14.2100286837041,3.94237238018294));
#205987=CARTESIAN_POINT('Ctrl Pts',(17.7447865062546,14.2791072598717,4.03456055563452));
#205988=CARTESIAN_POINT('Ctrl Pts',(17.7393932531273,14.3450546292517,4.12908289781627));
#205989=CARTESIAN_POINT('Ctrl Pts',(17.734,14.4077184404108,4.2257166734219));
#205990=CARTESIAN_POINT('',(17.734,12.4414757859806,2.45527019889635));
#205991=CARTESIAN_POINT('Origin',(17.734,10.1295,7.));
#205992=CARTESIAN_POINT('',(18.5963464936207,10.1294413854624,12.0988853698432));
#205993=CARTESIAN_POINT('Ctrl Pts',(18.5963464895963,10.1294413021288,12.0986559623714));
#205994=CARTESIAN_POINT('Ctrl Pts',(18.5803708311834,9.78816223566316,12.0988021887428));
#205995=CARTESIAN_POINT('Ctrl Pts',(18.5256132911343,8.61850505157706,11.9829820583334));
#205996=CARTESIAN_POINT('Ctrl Pts',(18.4320738694491,6.76024937160752,11.0980785162391));
#205997=CARTESIAN_POINT('Ctrl Pts',(18.3157282245409,5.23345505271711,9.04320502425034));
#205998=CARTESIAN_POINT('Ctrl Pts',(18.1993825796327,4.8466304876897,6.51259606632921));
#205999=CARTESIAN_POINT('Ctrl Pts',(18.0830369347246,5.6899815760821,4.09545078585546));
#206000=CARTESIAN_POINT('Ctrl Pts',(17.9666912898163,7.56685261371754,2.35466742666588));
#206001=CARTESIAN_POINT('Ctrl Pts',(17.8503456449082,10.0408176861101,1.69542432103654));
#206002=CARTESIAN_POINT('Ctrl Pts',(17.772781881636,11.703188220458,2.0796916608358));
#206003=CARTESIAN_POINT('Ctrl Pts',(17.734,12.4414757859806,2.45527019889635));
#206004=CARTESIAN_POINT('Ctrl Pts',(18.8525174992326,14.6098038194187,9.43447708670712));
#206005=CARTESIAN_POINT('Ctrl Pts',(18.8455850997365,14.5391009597508,9.5645954985597));
#206006=CARTESIAN_POINT('Ctrl Pts',(18.8386527002405,14.4627231589996,9.6916367681177));
#206007=CARTESIAN_POINT('Ctrl Pts',(18.8317203007445,14.3809644182859,9.81511124114998));
#206008=CARTESIAN_POINT('Ctrl Pts',(18.8247881779579,14.2992089410048,9.93858078564965));
#206009=CARTESIAN_POINT('Ctrl Pts',(18.8178560551714,14.2120731373499,10.0584835437482));
#206010=CARTESIAN_POINT('Ctrl Pts',(18.8109239323848,14.1198943495422,10.1743588226824));
#206011=CARTESIAN_POINT('Ctrl Pts',(18.803990345741,14.0276960963278,10.2902585710145));
#206012=CARTESIAN_POINT('Ctrl Pts',(18.7970567590971,13.9304529376542,10.4021288826212));
#206013=CARTESIAN_POINT('Ctrl Pts',(18.7901231724533,13.8285428792875,10.5095416762296));
#206014=CARTESIAN_POINT('Ctrl Pts',(18.7871190496934,13.7843881954961,10.5560805362101));
#206015=CARTESIAN_POINT('Ctrl Pts',(18.7841149269336,13.7393579185255,10.6017830545718));
#206016=CARTESIAN_POINT('Ctrl Pts',(18.7811108041737,13.6934849922401,10.6466165105598));
#206017=CARTESIAN_POINT('Ctrl Pts',(18.7741773221436,13.5876107868587,10.7500916300169));
#206018=CARTESIAN_POINT('Ctrl Pts',(18.7672438401135,13.4772089013386,10.8489706438041));
#206019=CARTESIAN_POINT('Ctrl Pts',(18.7603103580834,13.3627009182632,10.9428686032053));
#206020=CARTESIAN_POINT('Ctrl Pts',(18.7533781928252,13.2482146819651,11.0367487299806));
#206021=CARTESIAN_POINT('Ctrl Pts',(18.7464460275669,13.1296241594456,11.1256494802232));
#206022=CARTESIAN_POINT('Ctrl Pts',(18.7395138623087,13.0073843026661,11.2092259312691));
#206023=CARTESIAN_POINT('Ctrl Pts',(18.7325814519985,12.8851401247099,11.292805336741));
#206024=CARTESIAN_POINT('Ctrl Pts',(18.7256490416884,12.7592466253653,11.3710598770508));
#206025=CARTESIAN_POINT('Ctrl Pts',(18.7187166313782,12.6301884988536,11.4436874363192));
#206026=CARTESIAN_POINT('Ctrl Pts',(18.7117845955379,12.5011373437085,11.5163110724457));
#206027=CARTESIAN_POINT('Ctrl Pts',(18.7048525596975,12.3689221920305,11.5833081744226));
#206028=CARTESIAN_POINT('Ctrl Pts',(18.6979205238572,12.2340531491345,11.6444221430085));
#206029=CARTESIAN_POINT('Ctrl Pts',(18.6909869446661,12.0991540789496,11.7055497180289));
#206030=CARTESIAN_POINT('Ctrl Pts',(18.6840533654749,11.9616002381555,11.7607914059618));
#206031=CARTESIAN_POINT('Ctrl Pts',(18.6771197862838,11.8219231385114,11.8099381409984));
#206032=CARTESIAN_POINT('Ctrl Pts',(18.6730015772777,11.7389617308685,11.839128912643));
#206033=CARTESIAN_POINT('Ctrl Pts',(18.6688833682716,11.6552516632411,11.8661704363264));
#206034=CARTESIAN_POINT('Ctrl Pts',(18.6647651592656,11.5709071450112,11.891027135716));
#206035=CARTESIAN_POINT('Ctrl Pts',(18.6577998246933,11.4282510078553,11.9330685249111));
#206036=CARTESIAN_POINT('Ctrl Pts',(18.650834490121,11.2837317271447,11.9688711473952));
#206037=CARTESIAN_POINT('Ctrl Pts',(18.6438691555487,11.1379071299167,11.9982913140726));
#206038=CARTESIAN_POINT('Ctrl Pts',(18.6369053523104,10.9921145923347,12.0277050127044));
#206039=CARTESIAN_POINT('Ctrl Pts',(18.6299415490721,10.8450176285976,12.0507389918283));
#206040=CARTESIAN_POINT('Ctrl Pts',(18.6229777458338,10.6971847677683,12.0673005638549));
#206041=CARTESIAN_POINT('Ctrl Pts',(18.6160146892149,10.5493677567394,12.0838603602436));
#206042=CARTESIAN_POINT('Ctrl Pts',(18.609051632596,10.4008153280418,12.0939490974492));
#206043=CARTESIAN_POINT('Ctrl Pts',(18.6020885759772,10.2521021089812,12.0975258432767));
#206044=CARTESIAN_POINT('Ctrl Pts',(18.6001745491953,10.2112233541923,12.0985090303568));
#206045=CARTESIAN_POINT('Ctrl Pts',(18.5982605224134,10.1703324708191,12.0990004693845));
#206046=CARTESIAN_POINT('Ctrl Pts',(18.5963464956315,10.1294414271024,12.0989999996636));
#206047=CARTESIAN_POINT('Origin',(-26.8463464956315,10.1295,7.));
#206048=CARTESIAN_POINT('',(-18.7216535115683,10.1294126732152,12.0987227687564));
#206049=CARTESIAN_POINT('Ctrl Pts',(-18.977821433234,5.64904402747702,9.43455986027809));
#206050=CARTESIAN_POINT('Ctrl Pts',(-18.9452723567134,5.9814962272458,10.0450302244706));
#206051=CARTESIAN_POINT('Ctrl Pts',(-18.8739413985567,6.98517016733519,
11.2340275234321));
#206052=CARTESIAN_POINT('Ctrl Pts',(-18.7885520913348,8.70047320199483,
12.0007213768745));
#206053=CARTESIAN_POINT('Ctrl Pts',(-18.7357118606335,9.829103193625,12.0989141769127));
#206054=CARTESIAN_POINT('Ctrl Pts',(-18.7216535115683,10.1294126732152,
12.0987227687564));
#206055=CARTESIAN_POINT('',(-17.734,5.85128156875001,4.22571665929507));
#206056=CARTESIAN_POINT('Ctrl Pts',(-18.7216535043684,10.1294128222767,
12.0989999992548));
#206057=CARTESIAN_POINT('Ctrl Pts',(-18.7147113419131,10.2777169024359,
12.0990025348131));
#206058=CARTESIAN_POINT('Ctrl Pts',(-18.7077691794578,10.4260250034406,
12.0925306047745));
#206059=CARTESIAN_POINT('Ctrl Pts',(-18.7008270170026,10.5737648955722,
12.0796092076618));
#206060=CARTESIAN_POINT('Ctrl Pts',(-18.6938850825327,10.7214999358232,
12.0666882348967));
#206061=CARTESIAN_POINT('Ctrl Pts',(-18.6869431480629,10.8686664773571,
12.0473182494839));
#206062=CARTESIAN_POINT('Ctrl Pts',(-18.680001213593,11.0146970824474,12.021576159457));
#206063=CARTESIAN_POINT('Ctrl Pts',(-18.6730576379768,11.1607622107104,
11.9958279837289));
#206064=CARTESIAN_POINT('Ctrl Pts',(-18.6661140623605,11.3056905422907,
11.9637047507785));
#206065=CARTESIAN_POINT('Ctrl Pts',(-18.6591704867443,11.4489238560583,
11.9253346777721));
#206066=CARTESIAN_POINT('Ctrl Pts',(-18.6552746291148,11.5292883007021,
11.9038062391219));
#206067=CARTESIAN_POINT('Ctrl Pts',(-18.6513787714853,11.6091193479438,
11.8803121893208));
#206068=CARTESIAN_POINT('Ctrl Pts',(-18.6474829138558,11.6883203008384,
11.854882106673));
#206069=CARTESIAN_POINT('Ctrl Pts',(-18.6405493032985,11.8292773417162,
11.8096231916184));
#206070=CARTESIAN_POINT('Ctrl Pts',(-18.6336156927412,11.9682862806913,
11.7582135007032));
#206071=CARTESIAN_POINT('Ctrl Pts',(-18.626682082184,12.1048097739243,11.7008459129224));
#206072=CARTESIAN_POINT('Ctrl Pts',(-18.6197497878564,12.2413073504607,
11.6434892154165));
#206073=CARTESIAN_POINT('Ctrl Pts',(-18.6128174935289,12.3753201180157,
11.5801770055648));
#206074=CARTESIAN_POINT('Ctrl Pts',(-18.6058851992013,12.5063305296346,
11.5111503669682));
#206075=CARTESIAN_POINT('Ctrl Pts',(-18.5989526602658,12.6373455639937,
11.4421212927467));
#206076=CARTESIAN_POINT('Ctrl Pts',(-18.5920201213302,12.7653577364192,
11.3673775374312));
#206077=CARTESIAN_POINT('Ctrl Pts',(-18.5850875823947,12.8898734499727,
11.2872064816948));
#206078=CARTESIAN_POINT('Ctrl Pts',(-18.5781554184894,13.0143824275872,
11.20703976298));
#206079=CARTESIAN_POINT('Ctrl Pts',(-18.5712232545841,13.1353950473725,
11.121446511085));
#206080=CARTESIAN_POINT('Ctrl Pts',(-18.5642910906788,13.2524460816721,
11.0307578407749));
#206081=CARTESIAN_POINT('Ctrl Pts',(-18.5573573854077,13.3695231422555,
10.9400490058497));
#206082=CARTESIAN_POINT('Ctrl Pts',(-18.5504236801366,13.4826365958723,
10.8442426912284));
#206083=CARTESIAN_POINT('Ctrl Pts',(-18.5434899748654,13.5913532383767,
10.7437111475033));
#206084=CARTESIAN_POINT('Ctrl Pts',(-18.5393724062262,13.6559144246746,
10.6840106676712));
#206085=CARTESIAN_POINT('Ctrl Pts',(-18.5352548375869,13.7189256853204,
10.6226445735402));
#206086=CARTESIAN_POINT('Ctrl Pts',(-18.5311372689476,13.7803022426319,
10.5596971760522));
#206087=CARTESIAN_POINT('Ctrl Pts',(-18.5242037116084,13.8836539816517,
10.453700305551));
#206088=CARTESIAN_POINT('Ctrl Pts',(-18.5172701542692,13.9824041897261,
10.3431810712656));
#206089=CARTESIAN_POINT('Ctrl Pts',(-18.51033659693,14.0761684078321,10.2285615184816));
#206090=CARTESIAN_POINT('Ctrl Pts',(-18.5034043560879,14.1699148226197,
10.1139637288865));
#206091=CARTESIAN_POINT('Ctrl Pts',(-18.4964721152459,14.2586769270584,
9.99526742983162));
#206092=CARTESIAN_POINT('Ctrl Pts',(-18.4895398744039,14.3421103275237,
9.87292798873217));
#206093=CARTESIAN_POINT('Ctrl Pts',(-18.4826073888305,14.4255466734673,
9.75058422864091));
#206094=CARTESIAN_POINT('Ctrl Pts',(-18.4756749032572,14.5036537499851,
9.62459734036535));
#206095=CARTESIAN_POINT('Ctrl Pts',(-18.4687424176839,14.5761300052532,
9.49545238311256));
#206096=CARTESIAN_POINT('Ctrl Pts',(-18.4618103069418,14.6486023418167,
9.36631440857343));
#206097=CARTESIAN_POINT('Ctrl Pts',(-18.4548781961996,14.7154443053631,
9.23401899548399));
#206098=CARTESIAN_POINT('Ctrl Pts',(-18.4479460854575,14.7763998905137,
9.09907656066754));
#206099=CARTESIAN_POINT('Ctrl Pts',(-18.4410124325745,14.8373690360505,
8.96410410609937));
#206100=CARTESIAN_POINT('Ctrl Pts',(-18.4340787796916,14.8924490504929,
8.82648375455177));
#206101=CARTESIAN_POINT('Ctrl Pts',(-18.4271451268086,14.9414314869883,
8.6867472734616));
#206102=CARTESIAN_POINT('Ctrl Pts',(-18.4230272925522,14.9705217166792,
8.60375903069658));
#206103=CARTESIAN_POINT('Ctrl Pts',(-18.4189094582958,14.9974622098978,
8.52002479361661));
#206104=CARTESIAN_POINT('Ctrl Pts',(-18.4147916240394,15.0222175337942,
8.43565878066583));
#206105=CARTESIAN_POINT('Ctrl Pts',(-18.4078580498408,15.0639003370249,
8.29360400764394));
#206106=CARTESIAN_POINT('Ctrl Pts',(-18.4009244756422,15.099399552533,8.14970818352137));
#206107=CARTESIAN_POINT('Ctrl Pts',(-18.3939909014436,15.1285731159382,
8.00452425630458));
#206108=CARTESIAN_POINT('Ctrl Pts',(-18.3870586441602,15.1577411383182,
7.85936790432009));
#206109=CARTESIAN_POINT('Ctrl Pts',(-18.3801263868768,15.1805858405798,
7.71292426128421));
#206110=CARTESIAN_POINT('Ctrl Pts',(-18.3731941295934,15.1970161634336,
7.56575695606789));
#206111=CARTESIAN_POINT('Ctrl Pts',(-18.3662616283674,15.2134470644621,
7.41858447210896));
#206112=CARTESIAN_POINT('Ctrl Pts',(-18.3593291271414,15.2234630944089,
7.27068860316925));
#206113=CARTESIAN_POINT('Ctrl Pts',(-18.3523966259154,15.2270249522307,
7.12263915111047));
#206114=CARTESIAN_POINT('Ctrl Pts',(-18.3454645000055,15.2305866172184,
6.97459771424611));
#206115=CARTESIAN_POINT('Ctrl Pts',(-18.3385323740956,15.2276948022499,
6.82640304141277));
#206116=CARTESIAN_POINT('Ctrl Pts',(-18.3316002481857,15.2183623246744,
6.67862601146172));
#206117=CARTESIAN_POINT('Ctrl Pts',(-18.3246665810175,15.2090277721571,
6.53081612541791));
#206118=CARTESIAN_POINT('Ctrl Pts',(-18.3177329138493,15.1932497165721,
6.3834243978359));
#206119=CARTESIAN_POINT('Ctrl Pts',(-18.3107992466811,15.1710929950943,
6.23701830178168));
#206120=CARTESIAN_POINT('Ctrl Pts',(-18.3066814908311,15.1579345946017,
6.15007086922187));
#206121=CARTESIAN_POINT('Ctrl Pts',(-18.3025637349812,15.1425274812018,
6.06347096462066));
#206122=CARTESIAN_POINT('Ctrl Pts',(-18.2984459791312,15.1248938320092,
5.97733609473846));
#206123=CARTESIAN_POINT('Ctrl Pts',(-18.2915124972733,15.0952022739807,
5.83230210549236));
#206124=CARTESIAN_POINT('Ctrl Pts',(-18.2845790154154,15.0591850609188,
5.68853703671448));
#206125=CARTESIAN_POINT('Ctrl Pts',(-18.2776455335575,15.0169755996428,
5.54659597396457));
#206126=CARTESIAN_POINT('Ctrl Pts',(-18.2707133684712,14.9747741545734,
5.40468186794047));
#206127=CARTESIAN_POINT('Ctrl Pts',(-18.263781203385,14.9263829017666,5.26459139352123));
#206128=CARTESIAN_POINT('Ctrl Pts',(-18.2568490382987,14.8719853167288,
5.12686518888486));
#206129=CARTESIAN_POINT('Ctrl Pts',(-18.2499166281586,14.8175858087221,
4.98913411559094));
#206130=CARTESIAN_POINT('Ctrl Pts',(-18.2429842180185,14.7571796619472,
4.85376778802202));
#206131=CARTESIAN_POINT('Ctrl Pts',(-18.2360518078784,14.6909989751094,
4.72128806118977));
#206132=CARTESIAN_POINT('Ctrl Pts',(-18.2291197722066,14.6248218631567,
4.58881549052106));
#206133=CARTESIAN_POINT('Ctrl Pts',(-18.2221877365348,14.552870983883,4.45922950391654));
#206134=CARTESIAN_POINT('Ctrl Pts',(-18.215255700863,14.4754249908955,4.33302850155644));
#206135=CARTESIAN_POINT('Ctrl Pts',(-18.2083221218366,14.3979617552632,
4.20679940169296));
#206136=CARTESIAN_POINT('Ctrl Pts',(-18.2013885428103,14.3150011343056,
4.08395707380847));
#206137=CARTESIAN_POINT('Ctrl Pts',(-18.1944549637839,14.2268661502294,
3.96497254856659));
#206138=CARTESIAN_POINT('Ctrl Pts',(-18.1903367539303,14.1745182418128,
3.89430150805252));
#206139=CARTESIAN_POINT('Ctrl Pts',(-18.1862185440766,14.120345759108,3.82499086876333));
#206140=CARTESIAN_POINT('Ctrl Pts',(-18.182100334223,14.0644233505464,3.75713410309268));
#206141=CARTESIAN_POINT('Ctrl Pts',(-18.1751666150798,13.9702682956653,
3.64288549220289));
#206142=CARTESIAN_POINT('Ctrl Pts',(-18.1682328959365,13.8711179308502,
3.53272057308594));
#206143=CARTESIAN_POINT('Ctrl Pts',(-18.1612991767932,13.7673500985625,
3.42706735854301));
#206144=CARTESIAN_POINT('Ctrl Pts',(-18.154366774106,13.6636019679364,3.32143420362576));
#206145=CARTESIAN_POINT('Ctrl Pts',(-18.1474343714188,13.5552383504529,
3.22031127992502));
#206146=CARTESIAN_POINT('Ctrl Pts',(-18.1405019687316,13.4426745623103,
3.12409038809465));
#206147=CARTESIAN_POINT('Ctrl Pts',(-18.1335693228231,13.3301068249018,
3.02786612038391));
#206148=CARTESIAN_POINT('Ctrl Pts',(-18.1266366769147,13.2133388710388,
2.93654444601232));
#206149=CARTESIAN_POINT('Ctrl Pts',(-18.1197040310062,13.0928201831575,
2.85047779954232));
#206150=CARTESIAN_POINT('Ctrl Pts',(-18.1127717611685,12.972308032975,2.76441582187359));
#206151=CARTESIAN_POINT('Ctrl Pts',(-18.1058394913308,12.8480458254472,
2.68360849304188));
#206152=CARTESIAN_POINT('Ctrl Pts',(-18.0989072214931,12.7205131946589,
2.60836572275157));
#206153=CARTESIAN_POINT('Ctrl Pts',(-18.0919734128154,12.5929522539073,
2.53310624991183));
#206154=CARTESIAN_POINT('Ctrl Pts',(-18.0850396041378,12.4621197240941,
2.46341397180051));
#206155=CARTESIAN_POINT('Ctrl Pts',(-18.0781057954601,12.328521626002,2.39955383811791));
#206156=CARTESIAN_POINT('Ctrl Pts',(-18.0739887600783,12.249196089006,2.36163608727154));
#206157=CARTESIAN_POINT('Ctrl Pts',(-18.0698717246966,12.1688960160921,
2.32577360896849));
#206158=CARTESIAN_POINT('Ctrl Pts',(-18.0657546893148,12.0877310379076,
2.29201399724091));
#206159=CARTESIAN_POINT('Ctrl Pts',(-18.0588213575568,11.9510444008739,
2.23516080886065));
#206160=CARTESIAN_POINT('Ctrl Pts',(-18.0518880257988,11.8118565702988,
2.18425443407282));
#206161=CARTESIAN_POINT('Ctrl Pts',(-18.0449546940409,11.6707017706744,
2.13949610615628));
#206162=CARTESIAN_POINT('Ctrl Pts',(-18.0380226791153,11.52957378027,2.09474627909029));
#206163=CARTESIAN_POINT('Ctrl Pts',(-18.0310906641897,11.3864798811559,
2.05614226907002));
#206164=CARTESIAN_POINT('Ctrl Pts',(-18.0241586492642,11.2419704520384,
2.02383576503533));
#206165=CARTESIAN_POINT('Ctrl Pts',(-18.0172263879248,11.0974558860127,
1.99152811259429));
#206166=CARTESIAN_POINT('Ctrl Pts',(-18.0102941265854,10.9515260112177,
1.96551848947931));
#206167=CARTESIAN_POINT('Ctrl Pts',(-18.0033618652459,10.8047429609757,
1.94590780222078));
#206168=CARTESIAN_POINT('Ctrl Pts',(-17.9964299772503,10.6579678158787,
1.92629817111502));
#206169=CARTESIAN_POINT('Ctrl Pts',(-17.9894980892546,10.5103399151234,
1.9130868291269));
#206170=CARTESIAN_POINT('Ctrl Pts',(-17.9825662012589,10.3624281190368,
1.9063229891009));
#206171=CARTESIAN_POINT('Ctrl Pts',(-17.9756327668903,10.2144833266306,
1.89955764019033));
#206172=CARTESIAN_POINT('Ctrl Pts',(-17.9686993325218,10.0662548427467,
1.89924268229057));
#206173=CARTESIAN_POINT('Ctrl Pts',(-17.9617658981532,9.91831378778123,
1.90537524602953));
#206174=CARTESIAN_POINT('Ctrl Pts',(-17.9576469469043,9.8304263195057,1.90901842338271));
#206175=CARTESIAN_POINT('Ctrl Pts',(-17.9535279956555,9.74264030258537,
1.91493606689122));
#206176=CARTESIAN_POINT('Ctrl Pts',(-17.9494090444066,9.65507506418636,
1.92311887274498));
#206177=CARTESIAN_POINT('Ctrl Pts',(-17.9424753846608,9.50767162774376,
1.93689344499123));
#206178=CARTESIAN_POINT('Ctrl Pts',(-17.9355417249149,9.36084306546452,
1.95709434074805));
#206179=CARTESIAN_POINT('Ctrl Pts',(-17.9286080651691,9.21515569028204,
1.98364918658131));
#206180=CARTESIAN_POINT('Ctrl Pts',(-17.921675723217,9.06949600407137,2.01019898546813));
#206181=CARTESIAN_POINT('Ctrl Pts',(-17.9147433812648,8.9249773972537,2.04310026581364));
#206182=CARTESIAN_POINT('Ctrl Pts',(-17.9078110393127,8.78215725526951,
2.08222931317227));
#206183=CARTESIAN_POINT('Ctrl Pts',(-17.9008784555401,8.63933213129698,
2.12135972546763));
#206184=CARTESIAN_POINT('Ctrl Pts',(-17.8939458717674,8.49820591040426,
2.16671825537547));
#206185=CARTESIAN_POINT('Ctrl Pts',(-17.8870132879947,8.35932258344625,
2.21813081380062));
#206186=CARTESIAN_POINT('Ctrl Pts',(-17.8800810809331,8.22044680329677,
2.26954057850861));
#206187=CARTESIAN_POINT('Ctrl Pts',(-17.8731488738714,8.08381398289625,
2.32700359783838));
#206188=CARTESIAN_POINT('Ctrl Pts',(-17.8662166668098,7.94994985065518,
2.39029695679961));
#206189=CARTESIAN_POINT('Ctrl Pts',(-17.8592829213363,7.81605601096829,
2.45360436197322));
#206190=CARTESIAN_POINT('Ctrl Pts',(-17.8523491758629,7.68493238611156,
2.52274455078309));
#206191=CARTESIAN_POINT('Ctrl Pts',(-17.8454154303894,7.55708231303193,
2.59744753083239));
#206192=CARTESIAN_POINT('Ctrl Pts',(-17.8412980867591,7.48116336186096,
2.64180708228259));
#206193=CARTESIAN_POINT('Ctrl Pts',(-17.8371807431287,7.40639825299786,
2.68812726300884));
#206194=CARTESIAN_POINT('Ctrl Pts',(-17.8330633994984,7.33288794460905,
2.73634405566748));
#206195=CARTESIAN_POINT('Ctrl Pts',(-17.8261558247304,7.20956135421445,
2.81723628382821));
#206196=CARTESIAN_POINT('Ctrl Pts',(-17.8192482499625,7.08972242521831,
2.90349902317069));
#206197=CARTESIAN_POINT('Ctrl Pts',(-17.8123406751945,6.9738347131051,2.9948061723449));
#206198=CARTESIAN_POINT('Ctrl Pts',(-17.805433730195,6.85795756655736,3.08610499698111));
#206199=CARTESIAN_POINT('Ctrl Pts',(-17.7985267851956,6.74603118445736,
3.18244710971482));
#206200=CARTESIAN_POINT('Ctrl Pts',(-17.7916198401962,6.63848738561534,
3.28346506457867));
#206201=CARTESIAN_POINT('Ctrl Pts',(-17.7847137708704,6.53095722135077,
3.38447021222218));
#206202=CARTESIAN_POINT('Ctrl Pts',(-17.7778077015447,6.4278087750554,3.49014978807379));
#206203=CARTESIAN_POINT('Ctrl Pts',(-17.7709016322189,6.32943824184797,
3.60009829050449));
#206204=CARTESIAN_POINT('Ctrl Pts',(-17.763994324437,6.23105006798389,3.71006650985363));
#206205=CARTESIAN_POINT('Ctrl Pts',(-17.757087016655,6.13744174453664,3.82430493647222));
#206206=CARTESIAN_POINT('Ctrl Pts',(-17.7501797088731,6.04897067901331,
3.94237323066272));
#206207=CARTESIAN_POINT('Ctrl Pts',(-17.7447864725821,5.97989233816772,
4.03456113210717));
#206208=CARTESIAN_POINT('Ctrl Pts',(-17.739393236291,5.91394518475807,4.12908318533048));
#206209=CARTESIAN_POINT('Ctrl Pts',(-17.734,5.85128156875001,4.22571665929507));
#206210=CARTESIAN_POINT('',(-17.734,7.81752421401937,2.45527019889639));
#206211=CARTESIAN_POINT('Origin',(-17.734,10.1295,7.));
#206212=CARTESIAN_POINT('',(-18.5963464936225,10.1295586128697,12.0988854733127));
#206213=CARTESIAN_POINT('Ctrl Pts',(-18.5963464895958,10.1295586962519,
12.098655931404));
#206214=CARTESIAN_POINT('Ctrl Pts',(-18.580370831183,10.4708377603055,12.0988021573896));
#206215=CARTESIAN_POINT('Ctrl Pts',(-18.5256132911341,11.6404949371434,
11.9829820272798));
#206216=CARTESIAN_POINT('Ctrl Pts',(-18.4320738694491,13.4987506203882,
11.0980785037433));
#206217=CARTESIAN_POINT('Ctrl Pts',(-18.3157282245409,15.0255448975692,
9.04320498956965));
#206218=CARTESIAN_POINT('Ctrl Pts',(-18.1993825796327,15.4123695196911,
6.51259611415262));
#206219=CARTESIAN_POINT('Ctrl Pts',(-18.0830369347245,14.5690183264701,
4.09545070325184));
#206220=CARTESIAN_POINT('Ctrl Pts',(-17.9666912898164,12.6921474590521,
2.35466759323519));
#206221=CARTESIAN_POINT('Ctrl Pts',(-17.8503456449082,10.2181819306684,
1.69542365644608));
#206222=CARTESIAN_POINT('Ctrl Pts',(-17.772781881636,8.55581177954194,2.07969166083582));
#206223=CARTESIAN_POINT('Ctrl Pts',(-17.734,7.81752421401937,2.45527019889639));
#206224=CARTESIAN_POINT('Ctrl Pts',(-18.8525174996886,5.6491961756188,9.4344770775744));
#206225=CARTESIAN_POINT('Ctrl Pts',(-18.8455851001287,5.71989903564874,
9.56459549072555));
#206226=CARTESIAN_POINT('Ctrl Pts',(-18.8386527005687,5.79627683687807,
9.69163676155592));
#206227=CARTESIAN_POINT('Ctrl Pts',(-18.8317203010087,5.87803557818646,
9.81511123582243));
#206228=CARTESIAN_POINT('Ctrl Pts',(-18.8247881781597,5.95979105604538,
9.93858078153081));
#206229=CARTESIAN_POINT('Ctrl Pts',(-18.8178560553106,6.04692686039238,
10.0584835408014));
#206230=CARTESIAN_POINT('Ctrl Pts',(-18.8109239324616,6.13910564900675,
10.1743588208583));
#206231=CARTESIAN_POINT('Ctrl Pts',(-18.8039903457579,6.23130390299313,
10.2902585702695));
#206232=CARTESIAN_POINT('Ctrl Pts',(-18.7970567590541,6.32854706254942,
10.4021288829091));
#206233=CARTESIAN_POINT('Ctrl Pts',(-18.7901231723504,6.4304571219091,10.5095416774908));
#206234=CARTESIAN_POINT('Ctrl Pts',(-18.7871190496248,6.47461180524522,
10.5560805369597));
#206235=CARTESIAN_POINT('Ctrl Pts',(-18.7841149268993,6.51964208174608,
10.601783054832));
#206236=CARTESIAN_POINT('Ctrl Pts',(-18.7811108041737,6.56551500754935,
10.646616510354));
#206237=CARTESIAN_POINT('Ctrl Pts',(-18.7741773223733,6.6713892095192,10.7500916264889));
#206238=CARTESIAN_POINT('Ctrl Pts',(-18.7672438405729,6.78179109135341,
10.8489706372656));
#206239=CARTESIAN_POINT('Ctrl Pts',(-18.7603103587725,6.8962990704977,10.9428685939891));
#206240=CARTESIAN_POINT('Ctrl Pts',(-18.7533781937436,7.01078530286897,
11.0367487180902));
#206241=CARTESIAN_POINT('Ctrl Pts',(-18.7464460287148,7.12937582121679,
11.1256494659908));
#206242=CARTESIAN_POINT('Ctrl Pts',(-18.739513863686,7.2516156736085,11.2092259150478));
#206243=CARTESIAN_POINT('Ctrl Pts',(-18.7325814536027,7.37385984722273,
11.2928053185622));
#206244=CARTESIAN_POINT('Ctrl Pts',(-18.7256490435193,7.49975334201189,
11.3710598572636));
#206245=CARTESIAN_POINT('Ctrl Pts',(-18.718716633436,7.62881146378363,11.4436874152933));
#206246=CARTESIAN_POINT('Ctrl Pts',(-18.7117845978205,7.75786261422604,
11.516311050202));
#206247=CARTESIAN_POINT('Ctrl Pts',(-18.704852562205,7.8900777610185,11.5833081513277));
#206248=CARTESIAN_POINT('Ctrl Pts',(-18.6979205265895,8.02494679887543,
11.64442211945));
#206249=CARTESIAN_POINT('Ctrl Pts',(-18.6909869476181,8.15984586411983,
11.7055496940518));
#206250=CARTESIAN_POINT('Ctrl Pts',(-18.6840533686468,8.29739969982356,
11.7607913819451));
#206251=CARTESIAN_POINT('Ctrl Pts',(-18.6771197896754,8.43707679425738,
11.8099381173425));
#206252=CARTESIAN_POINT('Ctrl Pts',(-18.6730015795388,8.5200382242095,11.8391288981399));
#206253=CARTESIAN_POINT('Ctrl Pts',(-18.6688833694022,8.60374831456234,
11.8661704298008));
#206254=CARTESIAN_POINT('Ctrl Pts',(-18.6647651592655,8.68809285583543,
11.8910271359655));
#206255=CARTESIAN_POINT('Ctrl Pts',(-18.6577998241514,8.83074900390097,
11.9330685283489));
#206256=CARTESIAN_POINT('Ctrl Pts',(-18.6508344890373,8.97526829574175,
11.9688711530495));
#206257=CARTESIAN_POINT('Ctrl Pts',(-18.6438691539232,9.12109290423389,
11.9982913209625));
#206258=CARTESIAN_POINT('Ctrl Pts',(-18.6369053501428,9.26688545308524,
12.0277050208312));
#206259=CARTESIAN_POINT('Ctrl Pts',(-18.6299415463624,9.41398242822589,
12.0507390002111));
#206260=CARTESIAN_POINT('Ctrl Pts',(-18.622977742582,9.56181530050721,12.0673005715037));
#206261=CARTESIAN_POINT('Ctrl Pts',(-18.6160146854246,9.70963232291145,
12.0838603671502));
#206262=CARTESIAN_POINT('Ctrl Pts',(-18.6090516282673,9.85818476303232,
12.0939491026305));
#206263=CARTESIAN_POINT('Ctrl Pts',(-18.60208857111,10.0068979934788,12.097525845741));
#206264=CARTESIAN_POINT('Ctrl Pts',(-18.6001745459505,10.0477767135858,
12.0985090311648));
#206265=CARTESIAN_POINT('Ctrl Pts',(-18.598260520791,10.0886675622518,12.099000469371));
#206266=CARTESIAN_POINT('Ctrl Pts',(-18.5963464956315,10.1295585712674,
12.0989999996636));
#206267=CARTESIAN_POINT('Origin',(11.,-13.5,22.));
#206268=CARTESIAN_POINT('',(7.,-13.5,16.));
#206269=CARTESIAN_POINT('Origin',(11.,-13.5,16.));
#206270=CARTESIAN_POINT('',(7.,-13.5,22.));
#206271=CARTESIAN_POINT('',(7.,-13.5,22.));
#206272=CARTESIAN_POINT('Origin',(11.,-13.5,22.));
#206273=CARTESIAN_POINT('Origin',(2.22044604925031E-15,2.25,16.));
#206274=CARTESIAN_POINT('Origin',(11.,17.5,22.));
#206275=CARTESIAN_POINT('',(6.55407155365721,16.8045,22.));
#206276=CARTESIAN_POINT('',(9.25758668237251,21.6489752747581,22.));
#206277=CARTESIAN_POINT('Origin',(11.,17.5,22.));
#206278=CARTESIAN_POINT('',(9.25758668237251,21.6489752747581,16.));
#206279=CARTESIAN_POINT('',(9.25758668237251,21.6489752747581,22.));
#206280=CARTESIAN_POINT('',(6.55407155365721,16.8045,16.));
#206281=CARTESIAN_POINT('Origin',(11.,17.5,16.));
#206282=CARTESIAN_POINT('',(6.55407155365721,16.8045,22.));
#206283=CARTESIAN_POINT('Origin',(2.22044604925031E-15,2.25,16.));
#206284=CARTESIAN_POINT('',(9.25758668237251,21.5062266006623,16.));
#206285=CARTESIAN_POINT('',(9.25758668237251,11.8781133003311,16.));
#206286=CARTESIAN_POINT('',(7.0995,19.4175,16.));
#206287=CARTESIAN_POINT('Origin',(10.7505,17.8045,16.));
#206288=CARTESIAN_POINT('',(7.0995,16.8045,16.));
#206289=CARTESIAN_POINT('',(7.0995,9.52725,16.));
#206290=CARTESIAN_POINT('',(-3.54975,16.8045,16.));
#206291=CARTESIAN_POINT('Origin',(-11.,-13.5,22.));
#206292=CARTESIAN_POINT('',(-15.,-13.5,16.));
#206293=CARTESIAN_POINT('Origin',(-11.,-13.5,16.));
#206294=CARTESIAN_POINT('',(-15.,-13.5,22.));
#206295=CARTESIAN_POINT('',(-15.,-13.5,22.));
#206296=CARTESIAN_POINT('Origin',(-11.,-13.5,22.));
#206297=CARTESIAN_POINT('Origin',(2.22044604925031E-15,2.25,16.));
#206298=CARTESIAN_POINT('Origin',(-11.,17.5,22.));
#206299=CARTESIAN_POINT('',(-9.25758668237251,21.6489752747581,22.));
#206300=CARTESIAN_POINT('',(-6.55407155365721,16.8045,22.));
#206301=CARTESIAN_POINT('Origin',(-11.,17.5,22.));
#206302=CARTESIAN_POINT('',(-6.55407155365721,16.8045,16.));
#206303=CARTESIAN_POINT('',(-6.55407155365721,16.8045,22.));
#206304=CARTESIAN_POINT('',(-9.25758668237251,21.6489752747581,16.));
#206305=CARTESIAN_POINT('Origin',(-11.,17.5,16.));
#206306=CARTESIAN_POINT('',(-9.25758668237251,21.6489752747581,22.));
#206307=CARTESIAN_POINT('Origin',(2.22044604925031E-15,2.25,16.));
#206308=CARTESIAN_POINT('',(-7.0995,16.8045,16.));
#206309=CARTESIAN_POINT('',(-7.0995,19.4175,16.));
#206310=CARTESIAN_POINT('',(-7.0995,10.83375,16.));
#206311=CARTESIAN_POINT('',(-9.25758668237251,21.5062266006622,16.));
#206312=CARTESIAN_POINT('Origin',(-10.7505,17.8045,16.));
#206313=CARTESIAN_POINT('',(-9.25758668237251,13.2726133003311,16.));
#206314=CARTESIAN_POINT('',(-3.54975,16.8045,16.));
#206315=CARTESIAN_POINT('Origin',(1.5089639216641E-15,6.00000008940697,
22.));
#206316=CARTESIAN_POINT('',(-5.,6.00000008940697,16.));
#206317=CARTESIAN_POINT('Origin',(1.5089639216641E-15,6.00000008940697,
16.));
#206318=CARTESIAN_POINT('',(-5.,6.00000008940697,22.));
#206319=CARTESIAN_POINT('',(-5.,6.00000008940697,22.));
#206320=CARTESIAN_POINT('Origin',(1.5089639216641E-15,6.00000008940697,
22.));
#206321=CARTESIAN_POINT('Origin',(2.22044604925031E-15,2.25,16.));
#206322=CARTESIAN_POINT('Origin',(7.0995,16.8045,0.));
#206323=CARTESIAN_POINT('',(7.0995,19.4175,0.));
#206324=CARTESIAN_POINT('',(7.0995,19.4175,0.));
#206325=CARTESIAN_POINT('',(7.0995,16.8045,0.));
#206326=CARTESIAN_POINT('',(7.0995,16.8045,0.));
#206327=CARTESIAN_POINT('',(7.0995,16.8045,0.));
#206328=CARTESIAN_POINT('Origin',(-9.25758668237251,24.2952266006623,0.));
#206329=CARTESIAN_POINT('',(-9.25758668237251,21.5062266006623,0.));
#206330=CARTESIAN_POINT('',(-9.25758668237251,21.5062266006623,0.));
#206331=CARTESIAN_POINT('',(-9.25758668237251,24.2952266006623,0.));
#206332=CARTESIAN_POINT('',(-9.25758668237251,21.5062266006623,0.));
#206333=CARTESIAN_POINT('',(-9.25758668237251,24.2952266006623,22.));
#206334=CARTESIAN_POINT('',(-9.25758668237251,24.2952266006623,0.));
#206335=CARTESIAN_POINT('',(-9.25758668237251,21.5062266006623,22.));
#206336=CARTESIAN_POINT('Origin',(-7.0995,16.8045,0.));
#206337=CARTESIAN_POINT('',(-7.0995,16.8045,0.));
#206338=CARTESIAN_POINT('',(7.0995,16.8045,0.));
#206339=CARTESIAN_POINT('',(-7.0995,16.8045,0.));
#206340=CARTESIAN_POINT('',(7.0995,16.8045,22.));
#206341=CARTESIAN_POINT('Origin',(0.,1.05261330033112,22.));
#206342=CARTESIAN_POINT('',(-9.06658668237251,24.4862266006622,22.));
#206343=CARTESIAN_POINT('Origin',(-9.06658668237251,24.2952266006623,22.));
#206344=CARTESIAN_POINT('',(-7.30158668237251,24.4862266006622,22.));
#206345=CARTESIAN_POINT('',(-9.06658668237251,24.4862266006622,22.));
#206346=CARTESIAN_POINT('',(-7.11058668237251,24.6772266006623,22.));
#206347=CARTESIAN_POINT('Origin',(-7.30158668237251,24.6772266006623,22.));
#206348=CARTESIAN_POINT('',(-7.11058668237251,25.8032266006623,22.));
#206349=CARTESIAN_POINT('',(-7.11058668237251,24.6772266006623,22.));
#206350=CARTESIAN_POINT('',(-7.36458668237251,26.0572266006623,22.));
#206351=CARTESIAN_POINT('Origin',(-7.36458668237251,25.8032266006623,22.));
#206352=CARTESIAN_POINT('',(-18.734,24.211,22.));
#206353=CARTESIAN_POINT('',(-7.36458668237251,26.0572266006622,22.));
#206354=CARTESIAN_POINT('',(-23.734,19.211,22.));
#206355=CARTESIAN_POINT('Origin',(-18.734,19.211,22.));
#206356=CARTESIAN_POINT('',(-23.734,6.1295,22.));
#206357=CARTESIAN_POINT('',(-23.734,19.211,22.));
#206358=CARTESIAN_POINT('',(-23.534,6.1295,22.));
#206359=CARTESIAN_POINT('',(-11.867,6.1295,22.));
#206360=CARTESIAN_POINT('',(-23.534,-5.8705,22.));
#206361=CARTESIAN_POINT('',(-23.534,0.591056650165565,22.));
#206362=CARTESIAN_POINT('',(-23.734,-5.8705,22.));
#206363=CARTESIAN_POINT('',(-11.867,-5.8705,22.));
#206364=CARTESIAN_POINT('',(-23.734,-18.952,22.));
#206365=CARTESIAN_POINT('',(-23.734,19.211,22.));
#206366=CARTESIAN_POINT('',(-18.734,-23.952,22.));
#206367=CARTESIAN_POINT('Origin',(-18.734,-18.952,22.));
#206368=CARTESIAN_POINT('',(18.734,-23.952,22.));
#206369=CARTESIAN_POINT('',(-18.734,-23.952,22.));
#206370=CARTESIAN_POINT('',(23.734,-18.952,22.));
#206371=CARTESIAN_POINT('Origin',(18.734,-18.952,22.));
#206372=CARTESIAN_POINT('',(23.734,-5.8705,22.));
#206373=CARTESIAN_POINT('',(23.734,19.211,22.));
#206374=CARTESIAN_POINT('',(23.534,-5.8705,22.));
#206375=CARTESIAN_POINT('',(11.867,-5.8705,22.));
#206376=CARTESIAN_POINT('',(23.534,6.1295,22.));
#206377=CARTESIAN_POINT('',(23.534,0.591056650165565,22.));
#206378=CARTESIAN_POINT('',(23.734,6.1295,22.));
#206379=CARTESIAN_POINT('',(11.867,6.1295,22.));
#206380=CARTESIAN_POINT('',(23.734,19.211,22.));
#206381=CARTESIAN_POINT('',(23.734,19.211,22.));
#206382=CARTESIAN_POINT('',(18.734,24.211,22.));
#206383=CARTESIAN_POINT('Origin',(18.734,19.211,22.));
#206384=CARTESIAN_POINT('',(7.36458668237251,26.0572266006622,22.));
#206385=CARTESIAN_POINT('',(7.36458668237251,26.0572266006622,22.));
#206386=CARTESIAN_POINT('',(7.11058668237251,25.8032266006622,22.));
#206387=CARTESIAN_POINT('Origin',(7.36458668237251,25.8032266006622,22.));
#206388=CARTESIAN_POINT('',(7.11058668237251,24.6772266006623,22.));
#206389=CARTESIAN_POINT('',(7.11058668237251,24.6772266006623,22.));
#206390=CARTESIAN_POINT('',(7.30158668237251,24.4862266006622,22.));
#206391=CARTESIAN_POINT('Origin',(7.30158668237251,24.6772266006623,22.));
#206392=CARTESIAN_POINT('',(9.06658668237251,24.4862266006622,22.));
#206393=CARTESIAN_POINT('',(9.06658668237251,24.4862266006622,22.));
#206394=CARTESIAN_POINT('',(9.25758668237251,24.2952266006623,22.));
#206395=CARTESIAN_POINT('Origin',(9.06658668237251,24.2952266006623,22.));
#206396=CARTESIAN_POINT('',(9.25758668237251,21.5062266006623,22.));
#206397=CARTESIAN_POINT('',(-21.234,0.12950000000008,22.));
#206398=CARTESIAN_POINT('Origin',(-18.734,0.12950000000008,22.));
#206399=CARTESIAN_POINT('',(16.234,0.12950000000008,22.));
#206400=CARTESIAN_POINT('Origin',(18.734,0.12950000000008,22.));
#206401=CARTESIAN_POINT('Ctrl Pts',(-17.1140743056112,17.8480877707428,
22.));
#206402=CARTESIAN_POINT('Ctrl Pts',(-17.0603911270984,17.8998883320905,
22.));
#206403=CARTESIAN_POINT('Ctrl Pts',(-17.0098645090452,17.9545614843891,
22.));
#206404=CARTESIAN_POINT('Ctrl Pts',(-16.9624881824911,18.0117359214698,
22.));
#206405=CARTESIAN_POINT('Ctrl Pts',(-16.913424543523,18.0709466316106,22.));
#206406=CARTESIAN_POINT('Ctrl Pts',(-16.8677390829926,18.1328404012223,
22.));
#206407=CARTESIAN_POINT('Ctrl Pts',(-16.8254531773348,18.1970544302611,
22.));
#206408=CARTESIAN_POINT('Ctrl Pts',(-16.785318687812,18.2580013873046,22.));
#206409=CARTESIAN_POINT('Ctrl Pts',(-16.7482465752263,18.3210394462862,
22.));
#206410=CARTESIAN_POINT('Ctrl Pts',(-16.7142835835435,18.3858911656733,
22.));
#206411=CARTESIAN_POINT('Ctrl Pts',(-16.6991852702862,18.414721122225,22.));
#206412=CARTESIAN_POINT('Ctrl Pts',(-16.6847017945038,18.443909871674,22.));
#206413=CARTESIAN_POINT('Ctrl Pts',(-16.6708392558117,18.4734345779294,
22.));
#206414=CARTESIAN_POINT('Ctrl Pts',(-16.6640109132328,18.4879777156138,
22.));
#206415=CARTESIAN_POINT('Ctrl Pts',(-16.6573332485221,18.5026023792008,
22.));
#206416=CARTESIAN_POINT('Ctrl Pts',(-16.6508071085471,18.5173059065043,
22.));
#206417=CARTESIAN_POINT('Ctrl Pts',(-16.6447949281281,18.53085147238,22.));
#206418=CARTESIAN_POINT('Ctrl Pts',(-16.638910878667,18.5444653615358,22.));
#206419=CARTESIAN_POINT('Ctrl Pts',(-16.6331635636444,18.5581259521741,
22.));
#206420=CARTESIAN_POINT('Ctrl Pts',(-16.6020947551997,18.6319723086221,
22.));
#206421=CARTESIAN_POINT('Ctrl Pts',(-16.5749611536669,18.7073070289838,
22.));
#206422=CARTESIAN_POINT('Ctrl Pts',(-16.5517843887068,18.7837489743025,
22.));
#206423=CARTESIAN_POINT('Ctrl Pts',(-16.5281812491796,18.8615971944571,
22.));
#206424=CARTESIAN_POINT('Ctrl Pts',(-16.5086813563667,18.9405945618219,
22.));
#206425=CARTESIAN_POINT('Ctrl Pts',(-16.4933484509597,19.0203740751758,
22.));
#206426=CARTESIAN_POINT('Ctrl Pts',(-16.47941621323,19.0928656947682,22.));
#206427=CARTESIAN_POINT('Ctrl Pts',(-16.4689246908343,19.1660040425421,
22.));
#206428=CARTESIAN_POINT('Ctrl Pts',(-16.461955492605,19.2395296145576,22.));
#206429=CARTESIAN_POINT('Ctrl Pts',(-16.4592975702873,19.2675708974063,
22.));
#206430=CARTESIAN_POINT('Ctrl Pts',(-16.4571523310073,19.2956686091404,
22.));
#206431=CARTESIAN_POINT('Ctrl Pts',(-16.4555256621827,19.3238086400899,
22.));
#206432=CARTESIAN_POINT('Ctrl Pts',(-16.4546321787531,19.3392651675542,
22.));
#206433=CARTESIAN_POINT('Ctrl Pts',(-16.4538951614737,19.3547344644167,
22.));
#206434=CARTESIAN_POINT('Ctrl Pts',(-16.4533156881431,19.3702141998337,
22.));
#206435=CARTESIAN_POINT('Ctrl Pts',(-16.4528679850542,19.3821738966753,
22.));
#206436=CARTESIAN_POINT('Ctrl Pts',(-16.4525144924858,19.3941365263619,
22.));
#206437=CARTESIAN_POINT('Ctrl Pts',(-16.452255631388,19.4060924704157,22.));
#206438=CARTESIAN_POINT('Ctrl Pts',(-16.4504487968614,19.4895442238956,
22.));
#206439=CARTESIAN_POINT('Ctrl Pts',(-16.4532437926239,19.5727897376045,
22.));
#206440=CARTESIAN_POINT('Ctrl Pts',(-16.4606968610006,19.6554483758565,
22.));
#206441=CARTESIAN_POINT('Ctrl Pts',(-16.4681356985408,19.7379491862843,
22.));
#206442=CARTESIAN_POINT('Ctrl Pts',(-16.4802144629511,19.8198663642554,
22.));
#206443=CARTESIAN_POINT('Ctrl Pts',(-16.4970384375915,19.9008370756969,
22.));
#206444=CARTESIAN_POINT('Ctrl Pts',(-16.5135067566735,19.9800960820144,
22.));
#206445=CARTESIAN_POINT('Ctrl Pts',(-16.5345215459181,20.058449172967,22.));
#206446=CARTESIAN_POINT('Ctrl Pts',(-16.5598157066501,20.135668594405,22.));
#206447=CARTESIAN_POINT('Ctrl Pts',(-16.5701726792028,20.1672869365531,
22.));
#206448=CARTESIAN_POINT('Ctrl Pts',(-16.5812477391057,20.1987151389825,
22.));
#206449=CARTESIAN_POINT('Ctrl Pts',(-16.5930250010084,20.2299370972628,
22.));
#206450=CARTESIAN_POINT('Ctrl Pts',(-16.5995762661519,20.2473047442324,
22.));
#206451=CARTESIAN_POINT('Ctrl Pts',(-16.6063470587533,20.2646137128558,
22.));
#206452=CARTESIAN_POINT('Ctrl Pts',(-16.6133222512795,20.2818311531004,
22.));
#206453=CARTESIAN_POINT('Ctrl Pts',(-16.644281419466,20.3582502091005,22.));
#206454=CARTESIAN_POINT('Ctrl Pts',(-16.6792964912941,20.4329625137279,
22.));
#206455=CARTESIAN_POINT('Ctrl Pts',(-16.7180394494848,20.5057444546796,
22.));
#206456=CARTESIAN_POINT('Ctrl Pts',(-16.7588463546244,20.5824036954548,
22.));
#206457=CARTESIAN_POINT('Ctrl Pts',(-16.8037889572456,20.6569222708542,
22.));
#206458=CARTESIAN_POINT('Ctrl Pts',(-16.8525444691545,20.7290332608009,
22.));
#206459=CARTESIAN_POINT('Ctrl Pts',(-16.9012999810634,20.8011442507476,
22.));
#206460=CARTESIAN_POINT('Ctrl Pts',(-16.9538690009003,20.8708485410036,
22.));
#206461=CARTESIAN_POINT('Ctrl Pts',(-17.0099819921104,20.9378605149736,
22.));
#206462=CARTESIAN_POINT('Ctrl Pts',(-17.0318957015214,20.9640305852723,
22.));
#206463=CARTESIAN_POINT('Ctrl Pts',(-17.0543504354563,20.9897897710343,
22.));
#206464=CARTESIAN_POINT('Ctrl Pts',(-17.0773320398146,21.0151198306805,
22.));
#206465=CARTESIAN_POINT('Ctrl Pts',(-17.08646379095,21.0251847416122,22.));
#206466=CARTESIAN_POINT('Ctrl Pts',(-17.0956794941242,21.0351826951285,
22.));
#206467=CARTESIAN_POINT('Ctrl Pts',(-17.1049759541041,21.045110003522,22.));
#206468=CARTESIAN_POINT('Ctrl Pts',(-17.1654855277221,21.1097256958789,
22.));
#206469=CARTESIAN_POINT('Ctrl Pts',(-17.2292148909451,21.1711403001169,
22.));
#206470=CARTESIAN_POINT('Ctrl Pts',(-17.2958559579295,21.2290794537635,
22.));
#206471=CARTESIAN_POINT('Ctrl Pts',(-17.3510488196552,21.277065295534,22.));
#206472=CARTESIAN_POINT('Ctrl Pts',(-17.4082400388152,21.3226671775257,
22.));
#206473=CARTESIAN_POINT('Ctrl Pts',(-17.4672777521355,21.3657152682276,
22.));
#206474=CARTESIAN_POINT('Ctrl Pts',(-17.4867746843808,21.3799317014277,
22.0000000000001));
#206475=CARTESIAN_POINT('Ctrl Pts',(-17.5064731515178,21.3938694861353,
22.));
#206476=CARTESIAN_POINT('Ctrl Pts',(-17.5263681121617,21.4075220975473,
22.));
#206477=CARTESIAN_POINT('Ctrl Pts',(-17.542293137778,21.4184504019736,22.));
#206478=CARTESIAN_POINT('Ctrl Pts',(-17.55834542777,21.429196741247,22.));
#206479=CARTESIAN_POINT('Ctrl Pts',(-17.5745064519429,21.439747587913,22.));
#206480=CARTESIAN_POINT('Ctrl Pts',(-17.6490342197562,21.4884036039023,
22.0000000000001));
#206481=CARTESIAN_POINT('Ctrl Pts',(-17.7259441256673,21.5329559340006,
22.));
#206482=CARTESIAN_POINT('Ctrl Pts',(-17.8049553049308,21.5731139747841,
22.));
#206483=CARTESIAN_POINT('Ctrl Pts',(-17.8827965257828,21.6126773751883,
22.));
#206484=CARTESIAN_POINT('Ctrl Pts',(-17.9626779315913,21.6479763829434,
22.));
#206485=CARTESIAN_POINT('Ctrl Pts',(-18.0443633906767,21.6786957524571,
22.));
#206486=CARTESIAN_POINT('Ctrl Pts',(-18.0530581575348,21.6819655847986,
22.));
#206487=CARTESIAN_POINT('Ctrl Pts',(-18.0617733892786,21.6851834888842,
22.));
#206488=CARTESIAN_POINT('Ctrl Pts',(-18.0705086704292,21.6883495949495,
22.));
#206489=CARTESIAN_POINT('Ctrl Pts',(-19.3957372685686,21.6839949024184,
22.));
#206490=CARTESIAN_POINT('Ctrl Pts',(-19.477389057327,21.6544306829991,22.));
#206491=CARTESIAN_POINT('Ctrl Pts',(-19.5571491338509,21.6204660242301,
22.));
#206492=CARTESIAN_POINT('Ctrl Pts',(-19.6348154715246,21.5824187572536,
22.));
#206493=CARTESIAN_POINT('Ctrl Pts',(-19.7143271161632,21.5434675093651,
22.));
#206494=CARTESIAN_POINT('Ctrl Pts',(-19.7916450683047,21.5002366972975,
22.));
#206495=CARTESIAN_POINT('Ctrl Pts',(-19.8665231149463,21.4530209100354,
22.));
#206496=CARTESIAN_POINT('Ctrl Pts',(-19.9365885412779,21.4088398127381,
22.));
#206497=CARTESIAN_POINT('Ctrl Pts',(-20.0045177600369,21.3611685582522,
22.));
#206498=CARTESIAN_POINT('Ctrl Pts',(-20.0700782126376,21.3102210028104,
22.));
#206499=CARTESIAN_POINT('Ctrl Pts',(-20.0997466183463,21.2871654459197,
22.));
#206500=CARTESIAN_POINT('Ctrl Pts',(-20.1289294820831,21.2634386377592,
22.));
#206501=CARTESIAN_POINT('Ctrl Pts',(-20.1576028623549,21.2390591151444,
22.));
#206502=CARTESIAN_POINT('Ctrl Pts',(-20.1753080822265,21.2240052636568,
22.));
#206503=CARTESIAN_POINT('Ctrl Pts',(-20.1928190152043,21.2087025308569,
22.));
#206504=CARTESIAN_POINT('Ctrl Pts',(-20.2101297112266,21.1931551680194,
22.));
#206505=CARTESIAN_POINT('Ctrl Pts',(-20.222291744835,21.182232005305,22.));
#206506=CARTESIAN_POINT('Ctrl Pts',(-20.2343567146449,21.1711862914419,
22.));
#206507=CARTESIAN_POINT('Ctrl Pts',(-20.2463056588354,21.1600355900683,
22.));
#206508=CARTESIAN_POINT('Ctrl Pts',(-20.3097374358009,21.1008413389894,
22.));
#206509=CARTESIAN_POINT('Ctrl Pts',(-20.3700068738241,21.038599740636,22.));
#206510=CARTESIAN_POINT('Ctrl Pts',(-20.426883413529,20.9735889911137,22.));
#206511=CARTESIAN_POINT('Ctrl Pts',(-20.4830375565956,20.9094039519309,
22.));
#206512=CARTESIAN_POINT('Ctrl Pts',(-20.535884892703,20.8425188203227,22.));
#206513=CARTESIAN_POINT('Ctrl Pts',(-20.5851610183447,20.7731751876268,
22.));
#206514=CARTESIAN_POINT('Ctrl Pts',(-20.6305982452024,20.7092338300444,
22.));
#206515=CARTESIAN_POINT('Ctrl Pts',(-20.6729988898147,20.6432013951179,
22.));
#206516=CARTESIAN_POINT('Ctrl Pts',(-20.7121179614365,20.5752560755747,
22.));
#206517=CARTESIAN_POINT('Ctrl Pts',(-20.7284900120376,20.5468197103046,
22.0000000000001));
#206518=CARTESIAN_POINT('Ctrl Pts',(-20.7442868026563,20.5180482040854,
22.));
#206519=CARTESIAN_POINT('Ctrl Pts',(-20.7594882606863,20.4889543859677,
22.));
#206520=CARTESIAN_POINT('Ctrl Pts',(-20.769344952432,20.4700898272965,22.));
#206521=CARTESIAN_POINT('Ctrl Pts',(-20.7789513234994,20.4510897578356,
22.));
#206522=CARTESIAN_POINT('Ctrl Pts',(-20.7883016018661,20.4319576715327,
22.));
#206523=CARTESIAN_POINT('Ctrl Pts',(-20.7942275528717,20.4198322778685,
22.));
#206524=CARTESIAN_POINT('Ctrl Pts',(-20.800046810587,20.4076616313445,22.));
#206525=CARTESIAN_POINT('Ctrl Pts',(-20.8057567064001,20.3954502940177,
22.));
#206526=CARTESIAN_POINT('Ctrl Pts',(-20.8408822399145,20.3203298798152,
22.));
#206527=CARTESIAN_POINT('Ctrl Pts',(-20.8718943362061,20.2436277257691,
22.));
#206528=CARTESIAN_POINT('Ctrl Pts',(-20.898546197771,20.1655724028405,22.));
#206529=CARTESIAN_POINT('Ctrl Pts',(-20.9251980593358,20.0875170799122,
22.));
#206530=CARTESIAN_POINT('Ctrl Pts',(-20.9474901582818,20.008107858314,22.));
#206531=CARTESIAN_POINT('Ctrl Pts',(-20.9651213884777,19.9275640466204,
22.));
#206532=CARTESIAN_POINT('Ctrl Pts',(-20.982945860616,19.8461374580334,22.));
#206533=CARTESIAN_POINT('Ctrl Pts',(-20.9960059981342,19.7635500467728,
22.));
#206534=CARTESIAN_POINT('Ctrl Pts',(-21.0043774598022,19.6801932612386,
22.));
#206535=CARTESIAN_POINT('Ctrl Pts',(-21.0078359299807,19.6457563888755,
22.));
#206536=CARTESIAN_POINT('Ctrl Pts',(-21.0104935728588,19.6111883610475,
22.));
#206537=CARTESIAN_POINT('Ctrl Pts',(-21.0123533015418,19.5765177064329,
22.));
#206538=CARTESIAN_POINT('Ctrl Pts',(-21.01308526083,19.5628718945969,22.));
#206539=CARTESIAN_POINT('Ctrl Pts',(-21.0136936024307,19.5492081941022,
22.));
#206540=CARTESIAN_POINT('Ctrl Pts',(-21.0141780332164,19.535546001816,22.));
#206541=CARTESIAN_POINT('Ctrl Pts',(-21.0170628012175,19.4541881354373,
22.));
#206542=CARTESIAN_POINT('Ctrl Pts',(-21.0155662532645,19.372753622897,22.));
#206543=CARTESIAN_POINT('Ctrl Pts',(-21.009821014486,19.2915996489842,22.));
#206544=CARTESIAN_POINT('Ctrl Pts',(-21.0040551149971,19.2101538336328,
22.));
#206545=CARTESIAN_POINT('Ctrl Pts',(-20.9940095377668,19.1289895605332,
22.));
#206546=CARTESIAN_POINT('Ctrl Pts',(-20.9797676620055,19.0484794558067,
22.));
#206547=CARTESIAN_POINT('Ctrl Pts',(-20.9656474978483,18.9686573934531,
22.));
#206548=CARTESIAN_POINT('Ctrl Pts',(-20.9474020142679,18.8894774430081,
22.));
#206549=CARTESIAN_POINT('Ctrl Pts',(-20.9250689442011,18.8113285395616,
22.));
#206550=CARTESIAN_POINT('Ctrl Pts',(-20.915771730189,18.7787953017227,22.));
#206551=CARTESIAN_POINT('Ctrl Pts',(-20.9057656352848,18.7464411369984,
22.));
#206552=CARTESIAN_POINT('Ctrl Pts',(-20.8950513997073,18.714296014732,22.));
#206553=CARTESIAN_POINT('Ctrl Pts',(-20.8895107302012,18.6976727570651,
22.));
#206554=CARTESIAN_POINT('Ctrl Pts',(-20.8837798036466,18.681103370745,22.));
#206555=CARTESIAN_POINT('Ctrl Pts',(-20.8778666056241,18.6646133670345,
22.));
#206556=CARTESIAN_POINT('Ctrl Pts',(-20.8511334433403,18.5900631923957,
22.));
#206557=CARTESIAN_POINT('Ctrl Pts',(-20.8206474037361,18.5170371727757,
22.));
#206558=CARTESIAN_POINT('Ctrl Pts',(-20.7864673395051,18.4458945668894,
22.));
#206559=CARTESIAN_POINT('Ctrl Pts',(-20.7601551393027,18.3911281838788,
22.));
#206560=CARTESIAN_POINT('Ctrl Pts',(-20.7316529155262,18.3374783045939,
21.9999999999999));
#206561=CARTESIAN_POINT('Ctrl Pts',(-20.7009723139099,18.2851235072403,
22.));
#206562=CARTESIAN_POINT('Ctrl Pts',(-20.6917380438118,18.2693657217269,
22.));
#206563=CARTESIAN_POINT('Ctrl Pts',(-20.6823063515041,18.2537253600017,
22.));
#206564=CARTESIAN_POINT('Ctrl Pts',(-20.6726773431573,18.2382075723836,
22.));
#206565=CARTESIAN_POINT('Ctrl Pts',(-20.6644524248536,18.2249525692911,
21.9999999999999));
#206566=CARTESIAN_POINT('Ctrl Pts',(-20.6560858067932,18.2117907655657,
22.));
#206567=CARTESIAN_POINT('Ctrl Pts',(-20.6475820990968,18.1987316736659,
22.));
#206568=CARTESIAN_POINT('Ctrl Pts',(-20.6064305731469,18.1355355269517,
22.));
#206569=CARTESIAN_POINT('Ctrl Pts',(-20.5620419258381,18.0746943297043,
22.));
#206570=CARTESIAN_POINT('Ctrl Pts',(-20.5144495325811,18.0165478115783,
22.));
#206571=CARTESIAN_POINT('Ctrl Pts',(-20.4703173158397,17.9626288013104,
22.));
#206572=CARTESIAN_POINT('Ctrl Pts',(-20.4234297243619,17.9110267653547,
22.));
#206573=CARTESIAN_POINT('Ctrl Pts',(-20.3737908005412,17.8620457668345,
22.));
#206574=CARTESIAN_POINT('Ctrl Pts',(-20.368202240041,17.8565312783541,22.));
#206575=CARTESIAN_POINT('Ctrl Pts',(-20.3625787852046,17.8510500502091,
22.));
#206576=CARTESIAN_POINT('Ctrl Pts',(-20.3569208045551,17.8456022314362,
21.9999999999999));
#206577=CARTESIAN_POINT('Ctrl Pts',(20.3539256943888,17.8480877707428,22.));
#206578=CARTESIAN_POINT('Ctrl Pts',(20.4076088569716,17.8998883167192,22.));
#206579=CARTESIAN_POINT('Ctrl Pts',(20.4581354582059,17.954561454772,22.));
#206580=CARTESIAN_POINT('Ctrl Pts',(20.5055117676561,18.011735878447,22.));
#206581=CARTESIAN_POINT('Ctrl Pts',(20.5545753925315,18.0709465790738,22.));
#206582=CARTESIAN_POINT('Ctrl Pts',(20.6002608381634,18.1328403404668,22.));
#206583=CARTESIAN_POINT('Ctrl Pts',(20.6425467287697,18.1970543621783,22.));
#206584=CARTESIAN_POINT('Ctrl Pts',(20.6826812143694,18.2580013280037,22.));
#206585=CARTESIAN_POINT('Ctrl Pts',(20.7197533213128,18.321039397649,22.));
#206586=CARTESIAN_POINT('Ctrl Pts',(20.7537163061537,18.3858911290265,22.));
#206587=CARTESIAN_POINT('Ctrl Pts',(20.7688146169019,18.4147210919254,22.));
#206588=CARTESIAN_POINT('Ctrl Pts',(20.7832980898944,18.4439098480094,22.));
#206589=CARTESIAN_POINT('Ctrl Pts',(20.79716062556,18.4734345611379,22.));
#206590=CARTESIAN_POINT('Ctrl Pts',(20.8039889483082,18.4879776631471,22.));
#206591=CARTESIAN_POINT('Ctrl Pts',(20.8106665939401,18.5026022906791,22.));
#206592=CARTESIAN_POINT('Ctrl Pts',(20.8171927156004,18.5173057815627,22.));
#206593=CARTESIAN_POINT('Ctrl Pts',(20.8232049158819,18.5308513966511,22.));
#206594=CARTESIAN_POINT('Ctrl Pts',(20.8290889843231,18.5444653356248,22.));
#206595=CARTESIAN_POINT('Ctrl Pts',(20.834836317356,18.5581259764514,22.));
#206596=CARTESIAN_POINT('Ctrl Pts',(20.8659051086395,18.6319723320065,22.));
#206597=CARTESIAN_POINT('Ctrl Pts',(20.8930386939032,18.7073070517053,22.));
#206598=CARTESIAN_POINT('Ctrl Pts',(20.9162154441631,18.7837489961396,22.));
#206599=CARTESIAN_POINT('Ctrl Pts',(20.939818572744,18.8615972286665,22.));
#206600=CARTESIAN_POINT('Ctrl Pts',(20.9593184548383,18.9405946085653,22.));
#206601=CARTESIAN_POINT('Ctrl Pts',(20.9746513504446,19.0203741339557,22.));
#206602=CARTESIAN_POINT('Ctrl Pts',(20.9885835808428,19.0928657726744,22.));
#206603=CARTESIAN_POINT('Ctrl Pts',(20.9990750958871,19.1660041393111,22.));
#206604=CARTESIAN_POINT('Ctrl Pts',(21.0060442872368,19.2395297293499,22.));
#206605=CARTESIAN_POINT('Ctrl Pts',(21.0087022058165,19.2675710073175,22.));
#206606=CARTESIAN_POINT('Ctrl Pts',(21.0108474418568,19.2956687140012,22.));
#206607=CARTESIAN_POINT('Ctrl Pts',(21.0124741079748,19.3238087397167,22.));
#206608=CARTESIAN_POINT('Ctrl Pts',(21.0133675811686,19.3392651129519,22.));
#206609=CARTESIAN_POINT('Ctrl Pts',(21.0141045914371,19.3547342552799,22.));
#206610=CARTESIAN_POINT('Ctrl Pts',(21.0146840610199,19.370213835923,22.));
#206611=CARTESIAN_POINT('Ctrl Pts',(21.0151317606382,19.3821733978234,22.));
#206612=CARTESIAN_POINT('Ctrl Pts',(21.0154852519447,19.3941358929903,22.));
#206613=CARTESIAN_POINT('Ctrl Pts',(21.0157441139737,19.4060917025175,22.));
#206614=CARTESIAN_POINT('Ctrl Pts',(21.0175509756949,19.4895434728017,22.));
#206615=CARTESIAN_POINT('Ctrl Pts',(21.0147560087132,19.5727890030198,22.));
#206616=CARTESIAN_POINT('Ctrl Pts',(21.0073029715582,19.655447656657,22.));
#206617=CARTESIAN_POINT('Ctrl Pts',(20.9998641358153,19.737948808113,22.));
#206618=CARTESIAN_POINT('Ctrl Pts',(20.987785339035,19.819866321382,22.));
#206619=CARTESIAN_POINT('Ctrl Pts',(20.9709612973755,19.9008373573407,22.));
#206620=CARTESIAN_POINT('Ctrl Pts',(20.9545235681866,19.9799491420218,22.));
#206621=CARTESIAN_POINT('Ctrl Pts',(20.933556230191,20.0581583683546,22.));
#206622=CARTESIAN_POINT('Ctrl Pts',(20.9083249440286,20.1352385562694,22.));
#206623=CARTESIAN_POINT('Ctrl Pts',(20.8979275365846,20.1670020626737,22.));
#206624=CARTESIAN_POINT('Ctrl Pts',(20.886805437583,20.198573773065,22.));
#206625=CARTESIAN_POINT('Ctrl Pts',(20.8749747526326,20.2299373637517,22.));
#206626=CARTESIAN_POINT('Ctrl Pts',(20.8684234889834,20.2473050100404,22.));
#206627=CARTESIAN_POINT('Ctrl Pts',(20.8616526979763,20.2646139778576,22.));
#206628=CARTESIAN_POINT('Ctrl Pts',(20.854677507136,20.2818314171768,22.));
#206629=CARTESIAN_POINT('Ctrl Pts',(20.8237183426601,20.3582504783803,22.));
#206630=CARTESIAN_POINT('Ctrl Pts',(20.7887032753635,20.4329627854486,22.));
#206631=CARTESIAN_POINT('Ctrl Pts',(20.7499603220884,20.505744726553,22.));
#206632=CARTESIAN_POINT('Ctrl Pts',(20.7091534306779,20.5824039514245,22.));
#206633=CARTESIAN_POINT('Ctrl Pts',(20.6642108439443,20.6569225092783,22.));
#206634=CARTESIAN_POINT('Ctrl Pts',(20.6154553493761,20.7290334807154,22.));
#206635=CARTESIAN_POINT('Ctrl Pts',(20.5666998548079,20.8011444521524,22.));
#206636=CARTESIAN_POINT('Ctrl Pts',(20.5141308537666,20.8708487229331,22.));
#206637=CARTESIAN_POINT('Ctrl Pts',(20.4580178821339,20.9378606771181,22.));
#206638=CARTESIAN_POINT('Ctrl Pts',(20.4361041795504,20.9640307406671,22.));
#206639=CARTESIAN_POINT('Ctrl Pts',(20.4136494525221,20.9897899196015,22.));
#206640=CARTESIAN_POINT('Ctrl Pts',(20.3906678551117,21.0151199723788,22.));
#206641=CARTESIAN_POINT('Ctrl Pts',(20.3815361086865,21.0251848784325,22.));
#206642=CARTESIAN_POINT('Ctrl Pts',(20.3723204102617,21.0351828270963,22.));
#206643=CARTESIAN_POINT('Ctrl Pts',(20.3630239550768,21.0451101306559,22.));
#206644=CARTESIAN_POINT('Ctrl Pts',(20.3025143985113,21.1097258066671,22.));
#206645=CARTESIAN_POINT('Ctrl Pts',(20.2387850522983,21.1711403943428,22.));
#206646=CARTESIAN_POINT('Ctrl Pts',(20.1721440016478,21.2290795318308,22.));
#206647=CARTESIAN_POINT('Ctrl Pts',(20.11695115458,21.2770653592361,22.));
#206648=CARTESIAN_POINT('Ctrl Pts',(20.0597599496963,21.3226672272365,22.));
#206649=CARTESIAN_POINT('Ctrl Pts',(20.0007222499054,21.3657153046774,22.));
#206650=CARTESIAN_POINT('Ctrl Pts',(19.9812253064434,21.3799317449347,22.));
#206651=CARTESIAN_POINT('Ctrl Pts',(19.9615268276842,21.3938695363309,22.));
#206652=CARTESIAN_POINT('Ctrl Pts',(19.9416318550109,21.4075221540601,22.));
#206653=CARTESIAN_POINT('Ctrl Pts',(19.9257068576964,21.4184504375137,22.));
#206654=CARTESIAN_POINT('Ctrl Pts',(19.9096545963614,21.4291967564363,22.));
#206655=CARTESIAN_POINT('Ctrl Pts',(19.8934936011196,21.4397475834371,22.));
#206656=CARTESIAN_POINT('Ctrl Pts',(19.8189658486552,21.4884035858209,22.));
#206657=CARTESIAN_POINT('Ctrl Pts',(19.7420559565434,21.5329559037425,22.));
#206658=CARTESIAN_POINT('Ctrl Pts',(19.6630447888977,21.5731139344032,22.));
#206659=CARTESIAN_POINT('Ctrl Pts',(19.5852035756509,21.6126773267864,22.));
#206660=CARTESIAN_POINT('Ctrl Pts',(19.5053221751299,21.6479763280926,22.));
#206661=CARTESIAN_POINT('Ctrl Pts',(19.423636718432,21.6786956932901,22.));
#206662=CARTESIAN_POINT('Ctrl Pts',(19.414941951073,21.6819655254561,22.));
#206663=CARTESIAN_POINT('Ctrl Pts',(19.4062267187917,21.6851834293815,22.));
#206664=CARTESIAN_POINT('Ctrl Pts',(19.3974914370684,21.688349535301,22.));
#206665=CARTESIAN_POINT('Ctrl Pts',(18.0722627314313,21.6839949024184,22.));
#206666=CARTESIAN_POINT('Ctrl Pts',(17.9906108868453,21.6544306627852,22.));
#206667=CARTESIAN_POINT('Ctrl Pts',(17.910850754587,21.6204659928942,22.));
#206668=CARTESIAN_POINT('Ctrl Pts',(17.8331843622586,21.5824187212756,22.));
#206669=CARTESIAN_POINT('Ctrl Pts',(17.7536727057626,21.5434674902368,22.));
#206670=CARTESIAN_POINT('Ctrl Pts',(17.6763547404621,21.5002367065575,22.));
#206671=CARTESIAN_POINT('Ctrl Pts',(17.601476680063,21.4530209559562,22.));
#206672=CARTESIAN_POINT('Ctrl Pts',(17.53141126819,21.4088399101981,22.));
#206673=CARTESIAN_POINT('Ctrl Pts',(17.463482061701,21.3611687172218,22.));
#206674=CARTESIAN_POINT('Ctrl Pts',(17.3979216194972,21.3102212303572,22.));
#206675=CARTESIAN_POINT('Ctrl Pts',(17.3682532365539,21.287165718535,22.));
#206676=CARTESIAN_POINT('Ctrl Pts',(17.3390703946074,21.2634389577077,22.));
#206677=CARTESIAN_POINT('Ctrl Pts',(17.3103970351346,21.2390594843875,22.));
#206678=CARTESIAN_POINT('Ctrl Pts',(17.2926918259638,21.2240056615169,22.));
#206679=CARTESIAN_POINT('Ctrl Pts',(17.2751809033557,21.2087029580218,22.));
#206680=CARTESIAN_POINT('Ctrl Pts',(17.2578702173692,21.1931556251064,22.));
#206681=CARTESIAN_POINT('Ctrl Pts',(17.2457081795529,21.1822324733025,22.));
#206682=CARTESIAN_POINT('Ctrl Pts',(17.2336432055526,21.1711867704329,22.));
#206683=CARTESIAN_POINT('Ctrl Pts',(17.2216942572027,21.160036080102,22.));
#206684=CARTESIAN_POINT('Ctrl Pts',(17.1582624698647,21.1008418985699,22.));
#206685=CARTESIAN_POINT('Ctrl Pts',(17.0979930211184,21.0386003723497,22.));
#206686=CARTESIAN_POINT('Ctrl Pts',(17.0411164708952,20.973589694329,22.));
#206687=CARTESIAN_POINT('Ctrl Pts',(16.9849623314314,20.9094047417274,22.));
#206688=CARTESIAN_POINT('Ctrl Pts',(16.9321149974797,20.8425196974351,22.));
#206689=CARTESIAN_POINT('Ctrl Pts',(16.8828388728811,20.7731761494878,22.));
#206690=CARTESIAN_POINT('Ctrl Pts',(16.8374016308483,20.7092348473427,22.));
#206691=CARTESIAN_POINT('Ctrl Pts',(16.7950009722696,20.6432024641904,22.));
#206692=CARTESIAN_POINT('Ctrl Pts',(16.7558818883965,20.5752571902803,22.));
#206693=CARTESIAN_POINT('Ctrl Pts',(16.7395098281522,20.5468208362648,22.));
#206694=CARTESIAN_POINT('Ctrl Pts',(16.7237130285085,20.5180493400384,22.));
#206695=CARTESIAN_POINT('Ctrl Pts',(16.7085115621276,20.4889555304732,22.));
#206696=CARTESIAN_POINT('Ctrl Pts',(16.6986548604459,20.4700909686944,22.));
#206697=CARTESIAN_POINT('Ctrl Pts',(16.6890484799558,20.4510908953963,22.));
#206698=CARTESIAN_POINT('Ctrl Pts',(16.6796981927033,20.4319588044811,22.));
#206699=CARTESIAN_POINT('Ctrl Pts',(16.6737722459446,20.4198334281067,22.));
#206700=CARTESIAN_POINT('Ctrl Pts',(16.6679529923645,20.4076627987652,22.));
#206701=CARTESIAN_POINT('Ctrl Pts',(16.6622431005404,20.3954514784257,22.));
#206702=CARTESIAN_POINT('Ctrl Pts',(16.6271175635218,20.3203311087503,22.));
#206703=CARTESIAN_POINT('Ctrl Pts',(16.5961054651676,20.2436289901797,22.));
#206704=CARTESIAN_POINT('Ctrl Pts',(16.5694536034806,20.1655736906577,22.));
#206705=CARTESIAN_POINT('Ctrl Pts',(16.5428017417936,20.087518391136,22.));
#206706=CARTESIAN_POINT('Ctrl Pts',(16.5205096446651,20.0081091808815,22.));
#206707=CARTESIAN_POINT('Ctrl Pts',(16.5028784187468,19.9275653652902,22.));
#206708=CARTESIAN_POINT('Ctrl Pts',(16.4850539498385,19.8461387677624,22.));
#206709=CARTESIAN_POINT('Ctrl Pts',(16.4719938186516,19.7635513318282,22.));
#206710=CARTESIAN_POINT('Ctrl Pts',(16.4636223658545,19.6801945089039,22.));
#206711=CARTESIAN_POINT('Ctrl Pts',(16.4601638998612,19.6457576262764,22.));
#206712=CARTESIAN_POINT('Ctrl Pts',(16.457506261361,19.6111895860526,22.));
#206713=CARTESIAN_POINT('Ctrl Pts',(16.4556465372103,19.5765189171097,22.));
#206714=CARTESIAN_POINT('Ctrl Pts',(16.4549145796191,19.5628730980147,22.));
#206715=CARTESIAN_POINT('Ctrl Pts',(16.4543062397689,19.5492093899537,22.));
#206716=CARTESIAN_POINT('Ctrl Pts',(16.4538218107824,19.535547189819,22.));
#206717=CARTESIAN_POINT('Ctrl Pts',(16.450937053514,19.4541892772202,22.));
#206718=CARTESIAN_POINT('Ctrl Pts',(16.4524336138896,19.3727547084355,22.));
#206719=CARTESIAN_POINT('Ctrl Pts',(16.4581788662374,19.291600671179,22.));
#206720=CARTESIAN_POINT('Ctrl Pts',(16.4639447791349,19.2101547952154,22.));
#206721=CARTESIAN_POINT('Ctrl Pts',(16.4739903706192,19.1289904543258,22.));
#206722=CARTESIAN_POINT('Ctrl Pts',(16.4882322609474,19.048480277483,22.));
#206723=CARTESIAN_POINT('Ctrl Pts',(16.5023524377413,18.9686581538369,22.));
#206724=CARTESIAN_POINT('Ctrl Pts',(16.5205979332128,18.8894781376779,22.));
#206725=CARTESIAN_POINT('Ctrl Pts',(16.5429310139029,18.8113291667476,22.));
#206726=CARTESIAN_POINT('Ctrl Pts',(16.5522282344977,18.7787958932563,22.));
#206727=CARTESIAN_POINT('Ctrl Pts',(16.5622343360937,18.7464416926568,21.9999999999999));
#206728=CARTESIAN_POINT('Ctrl Pts',(16.5729485784318,18.7142965345088,22.));
#206729=CARTESIAN_POINT('Ctrl Pts',(16.5784892537261,18.6976732514091,22.));
#206730=CARTESIAN_POINT('Ctrl Pts',(16.5842201862524,18.6811038396758,22.));
#206731=CARTESIAN_POINT('Ctrl Pts',(16.5901333904085,18.6646138106646,22.));
#206732=CARTESIAN_POINT('Ctrl Pts',(16.6168665610553,18.5900635756494,22.));
#206733=CARTESIAN_POINT('Ctrl Pts',(16.6473526068873,18.5170374956828,22.));
#206734=CARTESIAN_POINT('Ctrl Pts',(16.6815326747322,18.4458948319454,22.));
#206735=CARTESIAN_POINT('Ctrl Pts',(16.7078448953081,18.3911283677854,22.));
#206736=CARTESIAN_POINT('Ctrl Pts',(16.7363471408355,18.3374784103201,22.));
#206737=CARTESIAN_POINT('Ctrl Pts',(16.7670277653193,18.2851235392682,22.));
#206738=CARTESIAN_POINT('Ctrl Pts',(16.7762620345021,18.2693657448798,22.));
#206739=CARTESIAN_POINT('Ctrl Pts',(16.7856937256623,18.2537253744878,22.));
#206740=CARTESIAN_POINT('Ctrl Pts',(16.7953227326228,18.2382075784408,22.));
#206741=CARTESIAN_POINT('Ctrl Pts',(16.8035476401832,18.2249525835537,22.));
#206742=CARTESIAN_POINT('Ctrl Pts',(16.8119142470167,18.2117907879613,22.));
#206743=CARTESIAN_POINT('Ctrl Pts',(16.8204179429878,18.198731704156,22.));
#206744=CARTESIAN_POINT('Ctrl Pts',(16.8615694556779,18.1355355298381,22.));
#206745=CARTESIAN_POINT('Ctrl Pts',(16.9059580849723,18.0746943089278,21.9999999999999));
#206746=CARTESIAN_POINT('Ctrl Pts',(16.9535504550158,18.0165477730384,22.));
#206747=CARTESIAN_POINT('Ctrl Pts',(16.9976827241167,17.9626286560282,22.));
#206748=CARTESIAN_POINT('Ctrl Pts',(17.0445703727031,17.9110265261487,22.));
#206749=CARTESIAN_POINT('Ctrl Pts',(17.0942093579555,17.8620454496849,22.));
#206750=CARTESIAN_POINT('Ctrl Pts',(17.0997979190133,17.8565309587036,22.));
#206751=CARTESIAN_POINT('Ctrl Pts',(17.1054213743828,17.8510497281848,22.));
#206752=CARTESIAN_POINT('Ctrl Pts',(17.1110793555412,17.8456019071633,22.));
#206753=CARTESIAN_POINT('Ctrl Pts',(20.3539256943887,-20.3149122292573,
22.));
#206754=CARTESIAN_POINT('Ctrl Pts',(20.408139566195,-20.2625995855167,22.));
#206755=CARTESIAN_POINT('Ctrl Pts',(20.4591341972937,-20.2073573541925,
22.));
#206756=CARTESIAN_POINT('Ctrl Pts',(20.5069159265706,-20.1495677196682,
22.));
#206757=CARTESIAN_POINT('Ctrl Pts',(20.5546976558475,-20.091778085144,22.));
#206758=CARTESIAN_POINT('Ctrl Pts',(20.5992668013762,-20.0314403792713,
22.));
#206759=CARTESIAN_POINT('Ctrl Pts',(20.6406036312651,-19.9688911346062,
22.));
#206760=CARTESIAN_POINT('Ctrl Pts',(20.6814854208042,-19.9070304388754,
22.));
#206761=CARTESIAN_POINT('Ctrl Pts',(20.7192059247084,-19.8430059080155,
22.));
#206762=CARTESIAN_POINT('Ctrl Pts',(20.7537163516506,-19.7771088559497,
22.));
#206763=CARTESIAN_POINT('Ctrl Pts',(20.7688146634378,-19.748278895671,22.));
#206764=CARTESIAN_POINT('Ctrl Pts',(20.7832981375853,-19.7190901423257,
22.));
#206765=CARTESIAN_POINT('Ctrl Pts',(20.7971606745034,-19.6895654320343,
22.));
#206766=CARTESIAN_POINT('Ctrl Pts',(20.8039890054239,-19.6750223153312,
22.));
#206767=CARTESIAN_POINT('Ctrl Pts',(20.8106666589183,-19.660397672949,22.));
#206768=CARTESIAN_POINT('Ctrl Pts',(20.8171927881263,-19.6456941670648,
22.));
#206769=CARTESIAN_POINT('Ctrl Pts',(20.8232049803476,-19.6321485719831,
22.));
#206770=CARTESIAN_POINT('Ctrl Pts',(20.8290890410869,-19.618534653263,22.));
#206771=CARTESIAN_POINT('Ctrl Pts',(20.8348363668121,-19.6048740328408,
22.));
#206772=CARTESIAN_POINT('Ctrl Pts',(20.8661434568434,-19.5304612896112,
22.));
#206773=CARTESIAN_POINT('Ctrl Pts',(20.8934547915536,-19.4545373140852,
21.9999999999999));
#206774=CARTESIAN_POINT('Ctrl Pts',(20.916748098317,-19.3774919314298,22.));
#206775=CARTESIAN_POINT('Ctrl Pts',(20.9400414050804,-19.3004465487744,
22.));
#206776=CARTESIAN_POINT('Ctrl Pts',(20.9593170648394,-19.2222788660794,
21.9999999999999));
#206777=CARTESIAN_POINT('Ctrl Pts',(20.9745132363111,-19.1433443390627,
21.9999999999999));
#206778=CARTESIAN_POINT('Ctrl Pts',(20.9885143247977,-19.0706175144489,
21.9999999999999));
#206779=CARTESIAN_POINT('Ctrl Pts',(20.9990521599664,-18.9972388060651,
22.));
#206780=CARTESIAN_POINT('Ctrl Pts',(21.0060443782249,-18.923470317406,22.));
#206781=CARTESIAN_POINT('Ctrl Pts',(21.0087022983456,-18.8954290373673,
22.));
#206782=CARTESIAN_POINT('Ctrl Pts',(21.010847535719,-18.8673313285427,22.));
#206783=CARTESIAN_POINT('Ctrl Pts',(21.012474202948,-18.8391913006101,22.));
#206784=CARTESIAN_POINT('Ctrl Pts',(21.0133676804257,-18.8237348626051,
22.));
#206785=CARTESIAN_POINT('Ctrl Pts',(21.0141046936245,-18.8082656553794,
22.));
#206786=CARTESIAN_POINT('Ctrl Pts',(21.0146841647679,-18.7927860097385,
22.));
#206787=CARTESIAN_POINT('Ctrl Pts',(21.0151318658524,-18.7808263906625,
22.));
#206788=CARTESIAN_POINT('Ctrl Pts',(21.01548535769,-18.768863838497,22.));
#206789=CARTESIAN_POINT('Ctrl Pts',(21.0157442193216,-18.7569079719692,
22.));
#206790=CARTESIAN_POINT('Ctrl Pts',(21.017551069503,-18.6734562086591,22.));
#206791=CARTESIAN_POINT('Ctrl Pts',(21.0147560903276,-18.5902106853063,
22.));
#206792=CARTESIAN_POINT('Ctrl Pts',(21.0073030399704,-18.5075520380821,
22.));
#206793=CARTESIAN_POINT('Ctrl Pts',(20.9998642034238,-18.4250510302545,
22.));
#206794=CARTESIAN_POINT('Ctrl Pts',(20.9877854202568,-18.3431336582205,
22.));
#206795=CARTESIAN_POINT('Ctrl Pts',(20.9709614068361,-18.2621627589815,
22.));
#206796=CARTESIAN_POINT('Ctrl Pts',(20.9545236784523,-18.1830509789684,
22.));
#206797=CARTESIAN_POINT('Ctrl Pts',(20.9335563404747,-18.104841755941,22.));
#206798=CARTESIAN_POINT('Ctrl Pts',(20.9083250537327,-18.0277615701596,
22.));
#206799=CARTESIAN_POINT('Ctrl Pts',(20.8979276440165,-17.9959980584227,
22.));
#206800=CARTESIAN_POINT('Ctrl Pts',(20.8868055423579,-17.9644263425748,
22.));
#206801=CARTESIAN_POINT('Ctrl Pts',(20.874974854388,-17.9330627463293,22.));
#206802=CARTESIAN_POINT('Ctrl Pts',(20.8684235902148,-17.9156951000059,
22.));
#206803=CARTESIAN_POINT('Ctrl Pts',(20.8616527986486,-17.8983861321004,
22.));
#206804=CARTESIAN_POINT('Ctrl Pts',(20.854677607217,-17.8811686926409,22.));
#206805=CARTESIAN_POINT('Ctrl Pts',(20.8226256793881,-17.8020522795121,
22.));
#206806=CARTESIAN_POINT('Ctrl Pts',(20.7862268153504,-17.724765227739,22.));
#206807=CARTESIAN_POINT('Ctrl Pts',(20.7458439642001,-17.6495556859564,
22.));
#206808=CARTESIAN_POINT('Ctrl Pts',(20.7054483430734,-17.5743223612055,
22.));
#206809=CARTESIAN_POINT('Ctrl Pts',(20.6610656710241,-17.501167065488,22.));
#206810=CARTESIAN_POINT('Ctrl Pts',(20.6130013967575,-17.4303438070485,
22.));
#206811=CARTESIAN_POINT('Ctrl Pts',(20.5649371224908,-17.359520548609,22.));
#206812=CARTESIAN_POINT('Ctrl Pts',(20.5131906957729,-17.2910285130232,
22.));
#206813=CARTESIAN_POINT('Ctrl Pts',(20.4580179345364,-17.2251393904043,
22.));
#206814=CARTESIAN_POINT('Ctrl Pts',(20.4361042290218,-17.1989693239199,
22.));
#206815=CARTESIAN_POINT('Ctrl Pts',(20.4136494990236,-17.1732101420222,
22.));
#206816=CARTESIAN_POINT('Ctrl Pts',(20.3906678986206,-17.1478800862692,
22.));
#206817=CARTESIAN_POINT('Ctrl Pts',(20.3815361507949,-17.1378151788001,
22.));
#206818=CARTESIAN_POINT('Ctrl Pts',(20.3723204509639,-17.1278172287239,
22.));
#206819=CARTESIAN_POINT('Ctrl Pts',(20.3630239943621,-17.1178899237497,
22.));
#206820=CARTESIAN_POINT('Ctrl Pts',(20.3025144308281,-17.0532742409372,
22.));
#206821=CARTESIAN_POINT('Ctrl Pts',(20.2387850776619,-16.9918596463669,
22.));
#206822=CARTESIAN_POINT('Ctrl Pts',(20.1721440203357,-16.933920502147,22.));
#206823=CARTESIAN_POINT('Ctrl Pts',(20.1169511671352,-16.8859346686413,
22.));
#206824=CARTESIAN_POINT('Ctrl Pts',(20.0597599562651,-16.8403327947037,
22.));
#206825=CARTESIAN_POINT('Ctrl Pts',(20.0007222507865,-16.7972847116374,
22.));
#206826=CARTESIAN_POINT('Ctrl Pts',(19.9812253134723,-16.7830682753746,
22.));
#206827=CARTESIAN_POINT('Ctrl Pts',(19.9615268410592,-16.7691304877775,
22.));
#206828=CARTESIAN_POINT('Ctrl Pts',(19.94163187493,-16.7554778736493,22.));
#206829=CARTESIAN_POINT('Ctrl Pts',(19.9257068621322,-16.7445495788584,
22.));
#206830=CARTESIAN_POINT('Ctrl Pts',(19.9096545851051,-16.733803248942,22.));
#206831=CARTESIAN_POINT('Ctrl Pts',(19.8934935740057,-16.7232524113246,
22.));
#206832=CARTESIAN_POINT('Ctrl Pts',(19.818965815021,-16.6745964034672,22.));
#206833=CARTESIAN_POINT('Ctrl Pts',(19.7420559170314,-16.6300440806761,
22.));
#206834=CARTESIAN_POINT('Ctrl Pts',(19.6630447444112,-16.5898860460099,
22.));
#206835=CARTESIAN_POINT('Ctrl Pts',(19.585203529837,-16.5503226514967,22.));
#206836=CARTESIAN_POINT('Ctrl Pts',(19.5053221290521,-16.5150236485074,
22.));
#206837=CARTESIAN_POINT('Ctrl Pts',(19.4236366733768,-16.4843042822826,
22.));
#206838=CARTESIAN_POINT('Ctrl Pts',(19.4149419062245,-16.481034450044,22.));
#206839=CARTESIAN_POINT('Ctrl Pts',(19.4062266741651,-16.4778165460524,
22.));
#206840=CARTESIAN_POINT('Ctrl Pts',(19.3974913926779,-16.4746504400725,
22.));
#206841=CARTESIAN_POINT('Ctrl Pts',(18.0722627314314,-16.4790050975816,
22.));
#206842=CARTESIAN_POINT('Ctrl Pts',(17.9909906838445,-16.5084318215279,
22.));
#206843=CARTESIAN_POINT('Ctrl Pts',(17.9115928093154,-16.5422181704993,
22.));
#206844=CARTESIAN_POINT('Ctrl Pts',(17.8342682750801,-16.580050621616,22.));
#206845=CARTESIAN_POINT('Ctrl Pts',(17.7547379110741,-16.6189623155344,
22.));
#206846=CARTESIAN_POINT('Ctrl Pts',(17.6774001286651,-16.6621548599535,
22.));
#206847=CARTESIAN_POINT('Ctrl Pts',(17.6025009734493,-16.7093334978469,
22.));
#206848=CARTESIAN_POINT('Ctrl Pts',(17.5320732406115,-16.7536956070808,
22.));
#206849=CARTESIAN_POINT('Ctrl Pts',(17.463801490032,-16.8015830463496,22.));
#206850=CARTESIAN_POINT('Ctrl Pts',(17.3979216159377,-16.8527787647009,
22.));
#206851=CARTESIAN_POINT('Ctrl Pts',(17.368253233471,-16.875834275562,22.));
#206852=CARTESIAN_POINT('Ctrl Pts',(17.3390703919806,-16.89956103538,22.));
#206853=CARTESIAN_POINT('Ctrl Pts',(17.3103970329429,-16.9239405076492,
22.));
#206854=CARTESIAN_POINT('Ctrl Pts',(17.2926918239748,-16.938994329927,22.));
#206855=CARTESIAN_POINT('Ctrl Pts',(17.2751809015629,-16.9542970328152,
22.));
#206856=CARTESIAN_POINT('Ctrl Pts',(17.257870215766,-16.9698443651112,22.));
#206857=CARTESIAN_POINT('Ctrl Pts',(17.2457081778958,-16.9807675166481,
22.));
#206858=CARTESIAN_POINT('Ctrl Pts',(17.2336432038411,-16.9918132192483,
22.));
#206859=CARTESIAN_POINT('Ctrl Pts',(17.2216942554371,-17.0029639093079,
22.));
#206860=CARTESIAN_POINT('Ctrl Pts',(17.1582584279828,-17.0621618593448,
22.));
#206861=CARTESIAN_POINT('Ctrl Pts',(17.0979853415003,-17.1244075418476,
22.));
#206862=CARTESIAN_POINT('Ctrl Pts',(17.0411056012962,-17.1894227118676,
22.));
#206863=CARTESIAN_POINT('Ctrl Pts',(16.9845622276698,-17.2540534052679,
22.));
#206864=CARTESIAN_POINT('Ctrl Pts',(16.9313716722725,-17.3214217543552,
22.));
#206865=CARTESIAN_POINT('Ctrl Pts',(16.8818040512577,-17.3912811757792,
22.));
#206866=CARTESIAN_POINT('Ctrl Pts',(16.8334273399218,-17.4594621575398,
22.));
#206867=CARTESIAN_POINT('Ctrl Pts',(16.7885012591782,-17.530016710817,22.));
#206868=CARTESIAN_POINT('Ctrl Pts',(16.7473243285968,-17.6027294194584,
22.));
#206869=CARTESIAN_POINT('Ctrl Pts',(16.7339893719953,-17.626277090458,22.0000000000001));
#206870=CARTESIAN_POINT('Ctrl Pts',(16.7210480077412,-17.6500511631493,
22.));
#206871=CARTESIAN_POINT('Ctrl Pts',(16.7085115583106,-17.6740444448892,
22.));
#206872=CARTESIAN_POINT('Ctrl Pts',(16.6986548564673,-17.6929090066348,
22.));
#206873=CARTESIAN_POINT('Ctrl Pts',(16.6890484758239,-17.7119090799142,
22.));
#206874=CARTESIAN_POINT('Ctrl Pts',(16.679698188427,-17.7310411708259,22.));
#206875=CARTESIAN_POINT('Ctrl Pts',(16.6737722417175,-17.7431665469103,
22.));
#206876=CARTESIAN_POINT('Ctrl Pts',(16.6679529881854,-17.7553371759649,
22.));
#206877=CARTESIAN_POINT('Ctrl Pts',(16.6622430964078,-17.7675484960222,
22.));
#206878=CARTESIAN_POINT('Ctrl Pts',(16.6271175593077,-17.8426688647472,
22.));
#206879=CARTESIAN_POINT('Ctrl Pts',(16.5961054609041,-17.9193709825623,
22.));
#206880=CARTESIAN_POINT('Ctrl Pts',(16.5694535992104,-17.9974262815892,
22.));
#206881=CARTESIAN_POINT('Ctrl Pts',(16.5428017375166,-18.0754815806163,
22.));
#206882=CARTESIAN_POINT('Ctrl Pts',(16.5205096404242,-18.1548907906356,
22.));
#206883=CARTESIAN_POINT('Ctrl Pts',(16.502878414596,-18.2354346063206,22.));
#206884=CARTESIAN_POINT('Ctrl Pts',(16.4850539457493,-18.3168612040769,
22.));
#206885=CARTESIAN_POINT('Ctrl Pts',(16.4719938146952,-18.3994486405796,
22.));
#206886=CARTESIAN_POINT('Ctrl Pts',(16.4636223620895,-18.4828054643466,
22.));
#206887=CARTESIAN_POINT('Ctrl Pts',(16.4601638961884,-18.5172423471919,
22.));
#206888=CARTESIAN_POINT('Ctrl Pts',(16.4575062577843,-18.5518103876793,
22.));
#206889=CARTESIAN_POINT('Ctrl Pts',(16.455646533733,-18.5864810569274,22.));
#206890=CARTESIAN_POINT('Ctrl Pts',(16.4549145761463,-18.6001268767863,
22.));
#206891=CARTESIAN_POINT('Ctrl Pts',(16.4543062363129,-18.6137905856188,
22.));
#206892=CARTESIAN_POINT('Ctrl Pts',(16.4538218073552,-18.6274527865309,
22.));
#206893=CARTESIAN_POINT('Ctrl Pts',(16.4509320250045,-18.7089524294447,
22.));
#206894=CARTESIAN_POINT('Ctrl Pts',(16.4524388232547,-18.790528997647,22.));
#206895=CARTESIAN_POINT('Ctrl Pts',(16.4582089280278,-18.8718234286523,
22.));
#206896=CARTESIAN_POINT('Ctrl Pts',(16.46400738077,-18.9535172513681,22.));
#206897=CARTESIAN_POINT('Ctrl Pts',(16.4741115013859,-19.0349271916877,
22.));
#206898=CARTESIAN_POINT('Ctrl Pts',(16.4884372996282,-19.115677127894,22.));
#206899=CARTESIAN_POINT('Ctrl Pts',(16.5025241469637,-19.1950801743737,
22.));
#206900=CARTESIAN_POINT('Ctrl Pts',(16.5206935045672,-19.2738459260412,
22.));
#206901=CARTESIAN_POINT('Ctrl Pts',(16.5429083125862,-19.351591380106,22.));
#206902=CARTESIAN_POINT('Ctrl Pts',(16.5522119455795,-19.3841514261301,
22.));
#206903=CARTESIAN_POINT('Ctrl Pts',(16.5622256149131,-19.4165321317305,
22.));
#206904=CARTESIAN_POINT('Ctrl Pts',(16.5729485780652,-19.4487034546206,
22.));
#206905=CARTESIAN_POINT('Ctrl Pts',(16.578489253474,-19.4653267382297,22.));
#206906=CARTESIAN_POINT('Ctrl Pts',(16.5842201861179,-19.481896150472,22.));
#206907=CARTESIAN_POINT('Ctrl Pts',(16.5901333903942,-19.4983861799902,
22.));
#206908=CARTESIAN_POINT('Ctrl Pts',(16.6168665612538,-19.5729364163756,
22.));
#206909=CARTESIAN_POINT('Ctrl Pts',(16.6473526072598,-19.6459624977086,
22.));
#206910=CARTESIAN_POINT('Ctrl Pts',(16.6815326752298,-19.7171051627546,
22.));
#206911=CARTESIAN_POINT('Ctrl Pts',(16.7078448962084,-19.7718716285596,
22.));
#206912=CARTESIAN_POINT('Ctrl Pts',(16.7363471421602,-19.8255215876092,
22.));
#206913=CARTESIAN_POINT('Ctrl Pts',(16.7670277670848,-19.8778764601534,
22.));
#206914=CARTESIAN_POINT('Ctrl Pts',(16.7762620361372,-19.8936342545421,
22.));
#206915=CARTESIAN_POINT('Ctrl Pts',(16.7856937271573,-19.9092746249327,
22.));
#206916=CARTESIAN_POINT('Ctrl Pts',(16.7953227339677,-19.9247924209762,
22.));
#206917=CARTESIAN_POINT('Ctrl Pts',(16.8035476416632,-19.9380474162847,
21.9999999999999));
#206918=CARTESIAN_POINT('Ctrl Pts',(16.8119142486341,-19.9512092122917,
22.));
#206919=CARTESIAN_POINT('Ctrl Pts',(16.8204179447442,-19.9642682965029,
22.));
#206920=CARTESIAN_POINT('Ctrl Pts',(16.8615694572081,-20.0274644714053,
22.));
#206921=CARTESIAN_POINT('Ctrl Pts',(16.905958086176,-20.0883056928112,21.9999999999999));
#206922=CARTESIAN_POINT('Ctrl Pts',(16.9535504557832,-20.1464522290649,
22.));
#206923=CARTESIAN_POINT('Ctrl Pts',(16.9976827257099,-20.2003713479159,
22.));
#206924=CARTESIAN_POINT('Ctrl Pts',(17.0445703751811,-20.251973479394,22.));
#206925=CARTESIAN_POINT('Ctrl Pts',(17.0942093613684,-20.3009545571532,
22.));
#206926=CARTESIAN_POINT('Ctrl Pts',(17.0997979224383,-20.3064690481884,
22.));
#206927=CARTESIAN_POINT('Ctrl Pts',(17.1054213778192,-20.3119502787582,
22.));
#206928=CARTESIAN_POINT('Ctrl Pts',(17.1110793589886,-20.3173980998282,
22.));
#206929=CARTESIAN_POINT('Ctrl Pts',(-17.1140743056112,-20.3149122292573,
22.));
#206930=CARTESIAN_POINT('Ctrl Pts',(-17.0603910881415,-20.2631116303188,
22.));
#206931=CARTESIAN_POINT('Ctrl Pts',(-17.0098644290427,-20.2084384430962,
22.));
#206932=CARTESIAN_POINT('Ctrl Pts',(-16.9624880608117,-20.1512639730764,
22.));
#206933=CARTESIAN_POINT('Ctrl Pts',(-16.9134243877974,-20.0920532398234,
22.));
#206934=CARTESIAN_POINT('Ctrl Pts',(-16.8677388912856,-20.0301594502243,
22.));
#206935=CARTESIAN_POINT('Ctrl Pts',(-16.8254529492875,-19.9659454033464,
22.));
#206936=CARTESIAN_POINT('Ctrl Pts',(-16.7853184507886,-19.9049984681181,
22.));
#206937=CARTESIAN_POINT('Ctrl Pts',(-16.7482463250095,-19.8419604355437,
22.));
#206938=CARTESIAN_POINT('Ctrl Pts',(-16.71428331717,-19.777108745806,22.));
#206939=CARTESIAN_POINT('Ctrl Pts',(-16.6991849978544,-19.7482788045816,
22.));
#206940=CARTESIAN_POINT('Ctrl Pts',(-16.6847015153359,-19.7190900711551,
22.));
#206941=CARTESIAN_POINT('Ctrl Pts',(-16.6708389693358,-19.6895653814969,
22.));
#206942=CARTESIAN_POINT('Ctrl Pts',(-16.6640105788719,-19.6750221576682,
22.));
#206943=CARTESIAN_POINT('Ctrl Pts',(-16.6573328680918,-19.6603974070189,
22.));
#206944=CARTESIAN_POINT('Ctrl Pts',(-16.6508066838924,-19.6456937917726,
22.));
#206945=CARTESIAN_POINT('Ctrl Pts',(-16.6447945515434,-19.6321483449743,
22.));
#206946=CARTESIAN_POINT('Ctrl Pts',(-16.6389105480172,-19.6185345763601,
22.));
#206947=CARTESIAN_POINT('Ctrl Pts',(-16.6331632765825,-19.6048741071589,
22.));
#206948=CARTESIAN_POINT('Ctrl Pts',(-16.6018561398417,-19.530461373728,
22.));
#206949=CARTESIAN_POINT('Ctrl Pts',(-16.5745447598008,-19.4545374092054,
22.));
#206950=CARTESIAN_POINT('Ctrl Pts',(-16.5512514111518,-19.3774920371772,
22.));
#206951=CARTESIAN_POINT('Ctrl Pts',(-16.5279580625028,-19.3004466651491,
22.));
#206952=CARTESIAN_POINT('Ctrl Pts',(-16.5086823642981,-19.2222789927081,
22.));
#206953=CARTESIAN_POINT('Ctrl Pts',(-16.4934861598923,-19.1433444740215,
22.));
#206954=CARTESIAN_POINT('Ctrl Pts',(-16.4781825851218,-19.0638522352736,
22.));
#206955=CARTESIAN_POINT('Ctrl Pts',(-16.4670158957966,-18.9835813665496,
22.));
#206956=CARTESIAN_POINT('Ctrl Pts',(-16.4600957863878,-18.90287356738,22.));
#206957=CARTESIAN_POINT('Ctrl Pts',(-16.4582781144994,-18.8816744375601,
22.));
#206958=CARTESIAN_POINT('Ctrl Pts',(-16.4567536954935,-18.8604450906499,
22.));
#206959=CARTESIAN_POINT('Ctrl Pts',(-16.4555251072067,-18.8391916010845,
22.));
#206960=CARTESIAN_POINT('Ctrl Pts',(-16.4546315989448,-18.8237346992684,
22.));
#206961=CARTESIAN_POINT('Ctrl Pts',(-16.45389456466,-18.8082650273129,22.));
#206962=CARTESIAN_POINT('Ctrl Pts',(-16.4533150822428,-18.7927849162226,
22.));
#206963=CARTESIAN_POINT('Ctrl Pts',(-16.4528673708036,-18.7808248936061,
22.));
#206964=CARTESIAN_POINT('Ctrl Pts',(-16.4525138752178,-18.7688619391664,
22.));
#206965=CARTESIAN_POINT('Ctrl Pts',(-16.4522550163972,-18.7569056703414,
22.));
#206966=CARTESIAN_POINT('Ctrl Pts',(-16.4504482477209,-18.6734539573408,
22.));
#206967=CARTESIAN_POINT('Ctrl Pts',(-16.4532433131771,-18.5902084834056,
22.));
#206968=CARTESIAN_POINT('Ctrl Pts',(-16.4606964571555,-18.5075498822213,
22.));
#206969=CARTESIAN_POINT('Ctrl Pts',(-16.4681352990784,-18.4250498970387,
22.));
#206970=CARTESIAN_POINT('Ctrl Pts',(-16.4802139851741,-18.3431335304585,
22.));
#206971=CARTESIAN_POINT('Ctrl Pts',(-16.4970377976341,-18.2621636043343,
22.));
#206972=CARTESIAN_POINT('Ctrl Pts',(-16.5135061122501,-18.1829046241824,
22.));
#206973=CARTESIAN_POINT('Ctrl Pts',(-16.5345209017836,-18.104551551424,
22.));
#206974=CARTESIAN_POINT('Ctrl Pts',(-16.5598150664328,-18.0273321413391,
22.));
#206975=CARTESIAN_POINT('Ctrl Pts',(-16.5701720519776,-17.9957137690736,
22.));
#206976=CARTESIAN_POINT('Ctrl Pts',(-16.5812471270599,-17.964285535797,
22.));
#206977=CARTESIAN_POINT('Ctrl Pts',(-16.5930244062011,-17.9330635460661,
22.));
#206978=CARTESIAN_POINT('Ctrl Pts',(-16.5995756745648,-17.9156958984863,
22.));
#206979=CARTESIAN_POINT('Ctrl Pts',(-16.606346470602,-17.8983869289424,
22.));
#206980=CARTESIAN_POINT('Ctrl Pts',(-16.613321666761,-17.8811694874779,
22.));
#206981=CARTESIAN_POINT('Ctrl Pts',(-16.6442808434086,-17.804750444978,
22.));
#206982=CARTESIAN_POINT('Ctrl Pts',(-16.6792959255798,-17.7300381471314,
22.));
#206983=CARTESIAN_POINT('Ctrl Pts',(-16.7180388949535,-17.6572562073792,
22.));
#206984=CARTESIAN_POINT('Ctrl Pts',(-16.7588458333273,-17.5805969275614,
22.));
#206985=CARTESIAN_POINT('Ctrl Pts',(-16.8037884744597,-17.506078309178,
22.));
#206986=CARTESIAN_POINT('Ctrl Pts',(-16.852544028446,-17.4339672739468,
22.));
#206987=CARTESIAN_POINT('Ctrl Pts',(-16.9012995824323,-17.3618562387157,
22.));
#206988=CARTESIAN_POINT('Ctrl Pts',(-16.9538686479157,-17.2921519008718,
22.));
#206989=CARTESIAN_POINT('Ctrl Pts',(-17.0099816867116,-17.2251398785991,
22.));
#206990=CARTESIAN_POINT('Ctrl Pts',(-17.0318954130067,-17.1989697914665,
22.));
#206991=CARTESIAN_POINT('Ctrl Pts',(-17.0543501640382,-17.1732105886975,
22.));
#206992=CARTESIAN_POINT('Ctrl Pts',(-17.0773317856131,-17.1478805119615,
22.));
#206993=CARTESIAN_POINT('Ctrl Pts',(-17.0864635488618,-17.1378155884281,
22.));
#206994=CARTESIAN_POINT('Ctrl Pts',(-17.095679264258,-17.127817622382,22.));
#206995=CARTESIAN_POINT('Ctrl Pts',(-17.1049757365821,-17.1178903015161,
22.));
#206996=CARTESIAN_POINT('Ctrl Pts',(-17.165485351815,-17.0532745693386,
22.));
#206997=CARTESIAN_POINT('Ctrl Pts',(-17.2292147565865,-16.9918599247989,
22.));
#206998=CARTESIAN_POINT('Ctrl Pts',(-17.2958558635168,-16.9339207318737,
22.));
#206999=CARTESIAN_POINT('Ctrl Pts',(-17.3510487599443,-16.8859348561654,
22.));
#207000=CARTESIAN_POINT('Ctrl Pts',(-17.4082400128264,-16.8403329410748,
22.));
#207001=CARTESIAN_POINT('Ctrl Pts',(-17.4672777580112,-16.797284818969,
22.));
#207002=CARTESIAN_POINT('Ctrl Pts',(-17.4896865553589,-16.7809451596297,
22.));
#207003=CARTESIAN_POINT('Ctrl Pts',(-17.5123617016702,-16.7649735008075,
22.));
#207004=CARTESIAN_POINT('Ctrl Pts',(-17.5352952134256,-16.7493800153535,
22.));
#207005=CARTESIAN_POINT('Ctrl Pts',(-17.5482870635507,-16.7405462951581,
22.));
#207006=CARTESIAN_POINT('Ctrl Pts',(-17.561360861439,-16.7318346842869,
22.));
#207007=CARTESIAN_POINT('Ctrl Pts',(-17.5745065855726,-16.7232523975405,
22.));
#207008=CARTESIAN_POINT('Ctrl Pts',(-17.6490343908001,-16.674596348734,
22.));
#207009=CARTESIAN_POINT('Ctrl Pts',(-17.7259443303904,-16.6300439893023,
22.));
#207010=CARTESIAN_POINT('Ctrl Pts',(-17.8049555380687,-16.5898859241834,
22.));
#207011=CARTESIAN_POINT('Ctrl Pts',(-17.8827967752858,-16.5503225057146,
22.));
#207012=CARTESIAN_POINT('Ctrl Pts',(-17.962678191744,-16.51502348347,22.));
#207013=CARTESIAN_POINT('Ctrl Pts',(-18.0443636543755,-16.484304104371,
22.));
#207014=CARTESIAN_POINT('Ctrl Pts',(-18.0530584200154,-16.4810342716093,
22.));
#207015=CARTESIAN_POINT('Ctrl Pts',(-18.0617736504531,-16.47781636714,22.));
#207016=CARTESIAN_POINT('Ctrl Pts',(-18.0705089302109,-16.4746502607264,
22.));
#207017=CARTESIAN_POINT('Ctrl Pts',(-19.3957372685685,-16.4790050975816,
22.));
#207018=CARTESIAN_POINT('Ctrl Pts',(-19.4773890957418,-16.5085693309101,
22.));
#207019=CARTESIAN_POINT('Ctrl Pts',(-19.5571492106159,-16.5425339973348,
22.));
#207020=CARTESIAN_POINT('Ctrl Pts',(-19.6348155858967,-16.5805812675104,
22.));
#207021=CARTESIAN_POINT('Ctrl Pts',(-19.7143272388332,-16.6195325038781,
22.));
#207022=CARTESIAN_POINT('Ctrl Pts',(-19.7916452001604,-16.6627632965025,
22.));
#207023=CARTESIAN_POINT('Ctrl Pts',(-19.8665232563899,-16.7099790586442,
22.));
#207024=CARTESIAN_POINT('Ctrl Pts',(-19.936588672608,-16.754160120401,22.));
#207025=CARTESIAN_POINT('Ctrl Pts',(-20.0045178827681,-16.8018313324713,
22.));
#207026=CARTESIAN_POINT('Ctrl Pts',(-20.0700783280693,-16.8527788406207,
22.));
#207027=CARTESIAN_POINT('Ctrl Pts',(-20.0997467181299,-16.8758343665167,
22.));
#207028=CARTESIAN_POINT('Ctrl Pts',(-20.1289295668893,-16.8995611421252,
22.));
#207029=CARTESIAN_POINT('Ctrl Pts',(-20.1576029328649,-16.9239406308391,
22.));
#207030=CARTESIAN_POINT('Ctrl Pts',(-20.1753081453826,-16.9389944626467,
22.));
#207031=CARTESIAN_POINT('Ctrl Pts',(-20.1928190712341,-16.9542971752936,
22.));
#207032=CARTESIAN_POINT('Ctrl Pts',(-20.2101297603596,-16.9698445175537,
22.));
#207033=CARTESIAN_POINT('Ctrl Pts',(-20.2222917967556,-16.9807676726665,
22.));
#207034=CARTESIAN_POINT('Ctrl Pts',(-20.2343567693431,-16.9918133788689,
22.));
#207035=CARTESIAN_POINT('Ctrl Pts',(-20.2463057162916,-17.002964072546,
22.));
#207036=CARTESIAN_POINT('Ctrl Pts',(-20.3097375002003,-17.0621582755838,
22.));
#207037=CARTESIAN_POINT('Ctrl Pts',(-20.3700069454281,-17.1243998240974,
22.));
#207038=CARTESIAN_POINT('Ctrl Pts',(-20.4268834922198,-17.1894105241983,
22.));
#207039=CARTESIAN_POINT('Ctrl Pts',(-20.4830376328431,-17.2535955037972,
22.));
#207040=CARTESIAN_POINT('Ctrl Pts',(-20.5358849675036,-17.3204805753177,
22.));
#207041=CARTESIAN_POINT('Ctrl Pts',(-20.5851610924645,-17.3898241496929,
22.));
#207042=CARTESIAN_POINT('Ctrl Pts',(-20.6305983299647,-17.4537654693584,
22.0000000000001));
#207043=CARTESIAN_POINT('Ctrl Pts',(-20.6729989843666,-17.5197978689047,
22.));
#207044=CARTESIAN_POINT('Ctrl Pts',(-20.7121180645734,-17.5877431573068,
22.));
#207045=CARTESIAN_POINT('Ctrl Pts',(-20.7391058385126,-17.6346177789475,
22.));
#207046=CARTESIAN_POINT('Ctrl Pts',(-20.7645310103452,-17.6824030516845,
22.));
#207047=CARTESIAN_POINT('Ctrl Pts',(-20.788301742955,-17.7310415486134,
22.0000000000001));
#207048=CARTESIAN_POINT('Ctrl Pts',(-20.7942276911041,-17.7431669305097,
22.0000000000001));
#207049=CARTESIAN_POINT('Ctrl Pts',(-20.8000469460378,-17.755337565341,
22.));
#207050=CARTESIAN_POINT('Ctrl Pts',(-20.8057568391674,-17.7675488911101,
22.));
#207051=CARTESIAN_POINT('Ctrl Pts',(-20.8408823751017,-17.8426692746921,
22.));
#207052=CARTESIAN_POINT('Ctrl Pts',(-20.8718944728201,-17.9193714043448,
22.));
#207053=CARTESIAN_POINT('Ctrl Pts',(-20.8985463344755,-17.9974267111826,
22.));
#207054=CARTESIAN_POINT('Ctrl Pts',(-20.9251981961308,-18.0754820180205,
22.));
#207055=CARTESIAN_POINT('Ctrl Pts',(-20.9474902938315,-18.1548912318264,
22.));
#207056=CARTESIAN_POINT('Ctrl Pts',(-20.9651215210881,-18.2354350462128,
22.));
#207057=CARTESIAN_POINT('Ctrl Pts',(-20.9829459910005,-18.3168616409281,
22.));
#207058=CARTESIAN_POINT('Ctrl Pts',(-20.9960061241615,-18.3994490691394,
22.));
#207059=CARTESIAN_POINT('Ctrl Pts',(-21.0043775797276,-18.4828058803714,
22.));
#207060=CARTESIAN_POINT('Ctrl Pts',(-21.007836047032,-18.5172427598331,
22.));
#207061=CARTESIAN_POINT('Ctrl Pts',(-21.0104936869016,-18.5518107962264,
22.));
#207062=CARTESIAN_POINT('Ctrl Pts',(-21.012353412468,-18.5864814607357,
22.));
#207063=CARTESIAN_POINT('Ctrl Pts',(-21.0130853706128,-18.6001272780164,
22.));
#207064=CARTESIAN_POINT('Ctrl Pts',(-21.013693711025,-18.613790984168,22.));
#207065=CARTESIAN_POINT('Ctrl Pts',(-21.0141781405805,-18.6274531823049,
22.));
#207066=CARTESIAN_POINT('Ctrl Pts',(-21.0170629011428,-18.7088110803349,
22.));
#207067=CARTESIAN_POINT('Ctrl Pts',(-21.0155663446046,-18.7902456314198,
22.));
#207068=CARTESIAN_POINT('Ctrl Pts',(-21.0098210964673,-18.8713996487605,
22.));
#207069=CARTESIAN_POINT('Ctrl Pts',(-21.0040551877172,-18.9528455058409,
22.));
#207070=CARTESIAN_POINT('Ctrl Pts',(-20.9940096006406,-19.0340098256051,
22.));
#207071=CARTESIAN_POINT('Ctrl Pts',(-20.9797677148141,-19.1145199799703,
22.));
#207072=CARTESIAN_POINT('Ctrl Pts',(-20.9656475419077,-19.1943420845851,
22.));
#207073=CARTESIAN_POINT('Ctrl Pts',(-20.9474020500803,-19.2735220803298,
22.));
#207074=CARTESIAN_POINT('Ctrl Pts',(-20.9250689726277,-19.3516710302886,
22.));
#207075=CARTESIAN_POINT('Ctrl Pts',(-20.9157717541756,-19.3842042922679,
22.));
#207076=CARTESIAN_POINT('Ctrl Pts',(-20.9057656547729,-19.4165584812898,
22.));
#207077=CARTESIAN_POINT('Ctrl Pts',(-20.8950514146661,-19.4487036278629,
22.));
#207078=CARTESIAN_POINT('Ctrl Pts',(-20.8895107411906,-19.4653269029819,
22.));
#207079=CARTESIAN_POINT('Ctrl Pts',(-20.8837798105413,-19.4818963067406,
22.));
#207080=CARTESIAN_POINT('Ctrl Pts',(-20.8778666083137,-19.4983863278128,
22.));
#207081=CARTESIAN_POINT('Ctrl Pts',(-20.8511334402601,-19.5729365440179,
22.));
#207082=CARTESIAN_POINT('Ctrl Pts',(-20.8206473963515,-19.6459626051822,
22.));
#207083=CARTESIAN_POINT('Ctrl Pts',(-20.7864673296103,-19.7171052508947,
22.));
#207084=CARTESIAN_POINT('Ctrl Pts',(-20.7601551154116,-19.7718716896741,
22.));
#207085=CARTESIAN_POINT('Ctrl Pts',(-20.7316528766953,-19.8255216226873,
22.));
#207086=CARTESIAN_POINT('Ctrl Pts',(-20.7009722593753,-19.8778764706885,
22.));
#207087=CARTESIAN_POINT('Ctrl Pts',(-20.691737989898,-19.893634262321,22.));
#207088=CARTESIAN_POINT('Ctrl Pts',(-20.6823062983705,-19.9092746300216,
22.));
#207089=CARTESIAN_POINT('Ctrl Pts',(-20.6726772909679,-19.9247924234514,
22.));
#207090=CARTESIAN_POINT('Ctrl Pts',(-20.6644523795805,-19.9380474216617,
22.));
#207091=CARTESIAN_POINT('Ctrl Pts',(-20.6560857687532,-19.9512092205436,
22.));
#207092=CARTESIAN_POINT('Ctrl Pts',(-20.6475820686168,-19.9642683076145,
22.));
#207093=CARTESIAN_POINT('Ctrl Pts',(-20.6064305516755,-20.0274644733087,
22.));
#207094=CARTESIAN_POINT('Ctrl Pts',(-20.5620419166415,-20.0883056868183,
22.));
#207095=CARTESIAN_POINT('Ctrl Pts',(-20.5144495392311,-20.1464522171398,
22.));
#207096=CARTESIAN_POINT('Ctrl Pts',(-20.4703172870206,-20.2003713000043,
22.));
#207097=CARTESIAN_POINT('Ctrl Pts',(-20.4234296568856,-20.2519733998006,
22.));
#207098=CARTESIAN_POINT('Ctrl Pts',(-20.3737906915119,-20.3009544512441,
22.));
#207099=CARTESIAN_POINT('Ctrl Pts',(-20.368202130628,-20.3064689414452,
22.));
#207100=CARTESIAN_POINT('Ctrl Pts',(-20.3625786754248,-20.3119501712233,
22.));
#207101=CARTESIAN_POINT('Ctrl Pts',(-20.3569206944252,-20.3173979915434,
22.));
#207102=CARTESIAN_POINT('Ctrl Pts',(-23.5309290705171,12.9159954693336,
3.78082017782678));
#207103=CARTESIAN_POINT('Ctrl Pts',(-23.4921433079708,12.3929904264528,
3.32811049525756));
#207104=CARTESIAN_POINT('Ctrl Pts',(-23.4145756637886,11.1227341693237,
2.68282848235636));
#207105=CARTESIAN_POINT('Ctrl Pts',(-23.2982261379702,8.98514974237196,
2.72043101044529));
#207106=CARTESIAN_POINT('Ctrl Pts',(-23.181880493062,7.11443374085103,3.7545041503849));
#207107=CARTESIAN_POINT('Ctrl Pts',(-23.0655348481538,5.94558822129673,
5.54427718926393));
#207108=CARTESIAN_POINT('Ctrl Pts',(-22.9491892032456,5.75102063216925,
7.67300413669454));
#207109=CARTESIAN_POINT('Ctrl Pts',(-22.8328435583374,6.57591665960292,
9.64502733133667));
#207110=CARTESIAN_POINT('Ctrl Pts',(-22.7164979134292,8.2282608210192,11.0011717427377));
#207111=CARTESIAN_POINT('Ctrl Pts',(-22.600152268521,10.323288213565,11.4256682689063));
#207112=CARTESIAN_POINT('Ctrl Pts',(-22.4838066236128,12.3731970142136,
10.8196752010624));
#207113=CARTESIAN_POINT('Ctrl Pts',(-22.3674609787046,13.9006736370829,
9.32429434527451));
#207114=CARTESIAN_POINT('Ctrl Pts',(-22.2511153337964,14.5500550456883,
7.28771604356662));
#207115=CARTESIAN_POINT('Ctrl Pts',(-22.1347696888882,14.1701406045664,
5.18414452104409));
#207116=CARTESIAN_POINT('Ctrl Pts',(-22.01842404398,12.8493807879515,3.50338441272897));
#207117=CARTESIAN_POINT('Ctrl Pts',(-21.9020783990718,10.8953289008482,
2.63678819422404));
#207118=CARTESIAN_POINT('Ctrl Pts',(-21.7857327541637,8.76292617796746,
2.78614191158665));
#207119=CARTESIAN_POINT('Ctrl Pts',(-21.6693871092554,6.94878938547822,
3.9166601151248));
#207120=CARTESIAN_POINT('Ctrl Pts',(-21.5530414643472,5.87511984341867,
5.76512820704877));
#207121=CARTESIAN_POINT('Ctrl Pts',(-21.436695819439,5.79235256012249,7.90110085502655));
#207122=CARTESIAN_POINT('Ctrl Pts',(-21.3203501745309,6.71884383786294,
9.82731569971233));
#207123=CARTESIAN_POINT('Ctrl Pts',(-21.2040045296227,8.44078094673926,
11.0950863074763));
#207124=CARTESIAN_POINT('Ctrl Pts',(-21.0876588847145,10.5532155549212,
11.4095949826005));
#207125=CARTESIAN_POINT('Ctrl Pts',(-20.9713132398063,12.5726553215346,
10.6968254724326));
#207126=CARTESIAN_POINT('Ctrl Pts',(-20.8549675948981,14.0113681472882,
9.12439137309156));
#207127=CARTESIAN_POINT('Ctrl Pts',(-20.6998400683538,14.7564835991063,
6.36487657912614));
#207128=CARTESIAN_POINT('Ctrl Pts',(-20.5059306601735,12.9941084081549,
2.90529953905878));
#207129=CARTESIAN_POINT('Ctrl Pts',(-20.2732393703571,8.33351686037291,
2.33663235857614));
#207130=CARTESIAN_POINT('Ctrl Pts',(-20.0793299621768,5.79098465748635,
5.27094140963515));
#207131=CARTESIAN_POINT('Ctrl Pts',(-19.9242024356325,5.85070730033819,
8.1286594049214));
#207132=CARTESIAN_POINT('Ctrl Pts',(-19.8078567907243,6.8691141699218,10.0009016541358));
#207133=CARTESIAN_POINT('Ctrl Pts',(-19.6915111458161,8.65791837240851,
11.1783382217567));
#207134=CARTESIAN_POINT('Ctrl Pts',(-19.5751655009079,10.7840004919133,
11.3809968058206));
#207135=CARTESIAN_POINT('Ctrl Pts',(-19.4588198559997,12.7602560148627,
10.5644652210994));
#207136=CARTESIAN_POINT('Ctrl Pts',(-19.3424742110915,14.1227278031238,
8.91754071104751));
#207137=CARTESIAN_POINT('Ctrl Pts',(-19.2261285661833,14.5559884821405,
6.82433389849613));
#207138=CARTESIAN_POINT('Ctrl Pts',(-19.1097829212752,13.9582878934289,
4.77193175011942));
#207139=CARTESIAN_POINT('Ctrl Pts',(-18.993437276367,12.4692119255032,3.23836842500364));
#207140=CARTESIAN_POINT('Ctrl Pts',(-18.8770916314588,10.4352843405056,
2.58065535350108));
#207141=CARTESIAN_POINT('Ctrl Pts',(-18.7607459865506,8.3301873937482,2.95197008276899));
#207142=CARTESIAN_POINT('Ctrl Pts',(-18.6444003416424,6.64403470258783,
4.26583846924497));
#207143=CARTESIAN_POINT('Ctrl Pts',(-18.5280546967342,5.76945787151179,
6.21634186567518));
#207144=CARTESIAN_POINT('Ctrl Pts',(-18.411709051826,5.91008699804141,8.34931416779286));
#207145=CARTESIAN_POINT('Ctrl Pts',(-18.2953634069178,7.03318105231844,
10.1681073068047));
#207146=CARTESIAN_POINT('Ctrl Pts',(-18.1790177620096,8.87723500286934,
11.2492265031511));
#207147=CARTESIAN_POINT('Ctrl Pts',(-18.0626721171014,11.0128674555704,
11.3409385700576));
#207148=CARTESIAN_POINT('Ctrl Pts',(-17.9463264721932,12.9428215115083,
10.4218921978272));
#207149=CARTESIAN_POINT('Ctrl Pts',(-17.829980827285,14.2176934838242,8.70607449466463));
#207150=CARTESIAN_POINT('Ctrl Pts',(-17.7136351823768,14.5406917268196,
6.59301815408165));
#207151=CARTESIAN_POINT('Ctrl Pts',(-17.5972895374686,13.8364941704587,
4.57470371354082));
#207152=CARTESIAN_POINT('Ctrl Pts',(-17.4809438925604,12.2693085317063,
3.12115124087976));
#207153=CARTESIAN_POINT('Ctrl Pts',(-17.3645982476522,10.2035493395539,
2.57068309301411));
#207154=CARTESIAN_POINT('Ctrl Pts',(-17.2870344843801,8.81547162341348,
2.89154656229486));
#207155=CARTESIAN_POINT('Ctrl Pts',(-17.248252602744,8.19900211022411,3.20515433429992));
#207156=CARTESIAN_POINT('Ctrl Pts',(-23.6935174548172,13.1003005986416,
3.5678963242189));
#207157=CARTESIAN_POINT('Ctrl Pts',(-23.654731692271,12.5427028162004,3.08524339662984));
#207158=CARTESIAN_POINT('Ctrl Pts',(-23.5771640480887,11.1884289296508,
2.39728096808227));
#207159=CARTESIAN_POINT('Ctrl Pts',(-23.4608145222703,8.90945982127682,
2.43737061265066));
#207160=CARTESIAN_POINT('Ctrl Pts',(-23.3444688773622,6.91501042117213,
3.53983969504486));
#207161=CARTESIAN_POINT('Ctrl Pts',(-23.2281232324539,5.66885480835072,
5.44799238140327));
#207162=CARTESIAN_POINT('Ctrl Pts',(-23.1117775875458,5.46141807765529,
7.71751815647438));
#207163=CARTESIAN_POINT('Ctrl Pts',(-22.9954319426376,6.34087459896918,
9.81997543718874));
#207164=CARTESIAN_POINT('Ctrl Pts',(-22.8790862977294,8.10250855026048,
11.2658183153034));
#207165=CARTESIAN_POINT('Ctrl Pts',(-22.7627406528212,10.3361058054659,
11.7183920043482));
#207166=CARTESIAN_POINT('Ctrl Pts',(-22.646395007913,12.5216002227899,11.0723171807799));
#207167=CARTESIAN_POINT('Ctrl Pts',(-22.5300493630048,14.1501076133713,
9.47802844409872));
#207168=CARTESIAN_POINT('Ctrl Pts',(-22.4137037180966,14.8424405809512,
7.30674623514494));
#207169=CARTESIAN_POINT('Ctrl Pts',(-22.2973580731884,14.4373977371574,
5.06403972183058));
#207170=CARTESIAN_POINT('Ctrl Pts',(-22.1810124282802,13.02927987117,3.27211032847339));
#207171=CARTESIAN_POINT('Ctrl Pts',(-22.064666783372,10.9459825610289,2.34819547088681));
#207172=CARTESIAN_POINT('Ctrl Pts',(-21.9483211384638,8.67253788638379,
2.50742778180684));
#207173=CARTESIAN_POINT('Ctrl Pts',(-21.8319754935556,6.73840997250145,
3.71272102301552));
#207174=CARTESIAN_POINT('Ctrl Pts',(-21.7156298486474,5.59372549215789,
5.68345098633069));
#207175=CARTESIAN_POINT('Ctrl Pts',(-21.5992842037392,5.50548379305222,
7.96070170901428));
#207176=CARTESIAN_POINT('Ctrl Pts',(-21.482938558831,6.49325530491686,10.0143207716261));
#207177=CARTESIAN_POINT('Ctrl Pts',(-21.3665929139228,8.3290852390299,11.3659446023248));
#207178=CARTESIAN_POINT('Ctrl Pts',(-21.2502472690146,10.581241062588,11.7012555944365));
#207179=CARTESIAN_POINT('Ctrl Pts',(-21.1339016241064,12.734251154871,10.9413418925109));
#207180=CARTESIAN_POINT('Ctrl Pts',(-21.0175559791982,14.2681237095048,
9.26490343601343));
#207181=CARTESIAN_POINT('Ctrl Pts',(-20.862428452654,15.0625227870125,6.32286807579321));
#207182=CARTESIAN_POINT('Ctrl Pts',(-20.6685190444737,13.1835801043741,
2.63446676497503));
#207183=CARTESIAN_POINT('Ctrl Pts',(-20.4358277546573,8.21472646274736,
2.02818664760248));
#207184=CARTESIAN_POINT('Ctrl Pts',(-20.2419183464769,5.50402541423371,
5.15657755346331));
#207185=CARTESIAN_POINT('Ctrl Pts',(-20.0867908199327,5.56769824811748,
8.2033114974362));
#207186=CARTESIAN_POINT('Ctrl Pts',(-19.9704451750245,6.65346485750777,
10.1993880947178));
#207187=CARTESIAN_POINT('Ctrl Pts',(-19.8540995301163,8.56058462643782,
11.454702987007));
#207188=CARTESIAN_POINT('Ctrl Pts',(-19.7377538852081,10.8272906386664,
11.6707658693921));
#207189=CARTESIAN_POINT('Ctrl Pts',(-19.6214082402999,12.9342601834799,
10.8002270339997));
#207190=CARTESIAN_POINT('Ctrl Pts',(-19.5050625953917,14.3868489455089,
9.04437120210426));
#207191=CARTESIAN_POINT('Ctrl Pts',(-19.3887169504835,14.8487664683456,
6.81271494418272));
#207192=CARTESIAN_POINT('Ctrl Pts',(-19.2723713055753,14.2115326072846,
4.62456226345754));
#207193=CARTESIAN_POINT('Ctrl Pts',(-19.1560256606671,12.6239657780463,
2.98956558234025));
#207194=CARTESIAN_POINT('Ctrl Pts',(-19.0396800157589,10.4555096102171,
2.28834987678537));
#207195=CARTESIAN_POINT('Ctrl Pts',(-18.9233343708507,8.2111767776498,2.68422420428154));
#207196=CARTESIAN_POINT('Ctrl Pts',(-18.8069887259426,6.41349812378914,
4.08499482531277));
#207197=CARTESIAN_POINT('Ctrl Pts',(-18.6906430810343,5.48107479781828,
6.1645089395608));
#207198=CARTESIAN_POINT('Ctrl Pts',(-18.5742974361261,5.63100545368278,
8.43856086670521));
#207199=CARTESIAN_POINT('Ctrl Pts',(-18.457951791218,6.82838349556238,10.3776531084284));
#207200=CARTESIAN_POINT('Ctrl Pts',(-18.3416061463098,8.79440735618407,
11.530279980087));
#207201=CARTESIAN_POINT('Ctrl Pts',(-18.2252605014016,11.071295382304,11.6280580910751));
#207202=CARTESIAN_POINT('Ctrl Pts',(-18.1089148564934,13.1289009760795,
10.6482239076538));
#207203=CARTESIAN_POINT('Ctrl Pts',(-17.9925692115852,14.4880958716855,
8.81891813062558));
#207204=CARTESIAN_POINT('Ctrl Pts',(-17.876223566677,14.8324579509393,6.56609945187542));
#207205=CARTESIAN_POINT('Ctrl Pts',(-17.7598779217688,14.0816831712841,
4.41428911728345));
#207206=CARTESIAN_POINT('Ctrl Pts',(-17.6435322768606,12.4108403204606,
2.86459538784371));
#207207=CARTESIAN_POINT('Ctrl Pts',(-17.5271866319524,10.2084471307945,
2.27771802837559));
#207208=CARTESIAN_POINT('Ctrl Pts',(-17.4496228686803,8.7285588067495,2.61980413514017));
#207209=CARTESIAN_POINT('Ctrl Pts',(-17.4108409870442,8.07131460198311,
2.95415463635743));
#207210=CARTESIAN_POINT('Ctrl Pts',(-23.8561058391174,13.2846057279496,
3.35497247061101));
#207211=CARTESIAN_POINT('Ctrl Pts',(-23.8173200765711,12.692415205948,2.84237629800212));
#207212=CARTESIAN_POINT('Ctrl Pts',(-23.7397524323889,11.2541236899778,
2.11173345380816));
#207213=CARTESIAN_POINT('Ctrl Pts',(-23.6234029065705,8.83376990018168,
2.15431021485603));
#207214=CARTESIAN_POINT('Ctrl Pts',(-23.5070572616623,6.71558710149322,
3.32517523970482));
#207215=CARTESIAN_POINT('Ctrl Pts',(-23.3907116167541,5.39212139540471,
5.35170757354262));
#207216=CARTESIAN_POINT('Ctrl Pts',(-23.2743659718459,5.17181552314134,
7.76203217625421));
#207217=CARTESIAN_POINT('Ctrl Pts',(-23.1580203269378,6.10583253833545,
9.99492354304081));
#207218=CARTESIAN_POINT('Ctrl Pts',(-23.0416746820295,7.97675627950178,
11.5304648878691));
#207219=CARTESIAN_POINT('Ctrl Pts',(-22.9253290371214,10.3489233973667,
12.0111157397901));
#207220=CARTESIAN_POINT('Ctrl Pts',(-22.8089833922131,12.6700034313663,
11.3249591604974));
#207221=CARTESIAN_POINT('Ctrl Pts',(-22.692637747305,14.3995415896597,9.63176254292293));
#207222=CARTESIAN_POINT('Ctrl Pts',(-22.5762921023967,15.1348261162141,
7.32577642672326));
#207223=CARTESIAN_POINT('Ctrl Pts',(-22.4599464574886,14.7046548697485,
4.94393492261707));
#207224=CARTESIAN_POINT('Ctrl Pts',(-22.3436008125804,13.2091789543886,
3.04083624421781));
#207225=CARTESIAN_POINT('Ctrl Pts',(-22.2272551676722,10.9966362212096,
2.05960274754957));
#207226=CARTESIAN_POINT('Ctrl Pts',(-22.110909522764,8.58214959480014,2.22871365202703));
#207227=CARTESIAN_POINT('Ctrl Pts',(-21.9945638778558,6.52803055952468,
3.50878193090623));
#207228=CARTESIAN_POINT('Ctrl Pts',(-21.8782182329476,5.31233114089711,
5.60177376561261));
#207229=CARTESIAN_POINT('Ctrl Pts',(-21.7618725880394,5.21861502598196,
8.02030256300201));
#207230=CARTESIAN_POINT('Ctrl Pts',(-21.6455269431312,6.26766677197077,
10.2013258435399));
#207231=CARTESIAN_POINT('Ctrl Pts',(-21.529181298223,8.21738953132054,11.6368028971734));
#207232=CARTESIAN_POINT('Ctrl Pts',(-21.4128356533148,10.6092665702549,
11.9929162062726));
#207233=CARTESIAN_POINT('Ctrl Pts',(-21.2964900084066,12.8958469882074,
11.1858583125893));
#207234=CARTESIAN_POINT('Ctrl Pts',(-21.1801443634984,14.5248792717214,
9.4054154989353));
#207235=CARTESIAN_POINT('Ctrl Pts',(-21.0250168369542,15.3685619749188,
6.28085957246028));
#207236=CARTESIAN_POINT('Ctrl Pts',(-20.8311074287738,13.3730518005934,
2.36363399089129));
#207237=CARTESIAN_POINT('Ctrl Pts',(-20.5984161389574,8.09593606512178,
1.71974093662882));
#207238=CARTESIAN_POINT('Ctrl Pts',(-20.4045067307771,5.21706617098109,
5.04221369729146));
#207239=CARTESIAN_POINT('Ctrl Pts',(-20.2493792042329,5.28468919589676,
8.277963589951));
#207240=CARTESIAN_POINT('Ctrl Pts',(-20.1330335593247,6.43781554509373,
10.3978745352999));
#207241=CARTESIAN_POINT('Ctrl Pts',(-20.0166879144165,8.46325088046714,
11.7310677522574));
#207242=CARTESIAN_POINT('Ctrl Pts',(-19.9003422695083,10.8705807854194,
11.9605349329635));
#207243=CARTESIAN_POINT('Ctrl Pts',(-19.7839966246001,13.1082643520972,
11.0359888469001));
#207244=CARTESIAN_POINT('Ctrl Pts',(-19.6676509796919,14.6509700878939,
9.17120169316103));
#207245=CARTESIAN_POINT('Ctrl Pts',(-19.5513053347837,15.1415444545508,
6.80109598986931));
#207246=CARTESIAN_POINT('Ctrl Pts',(-19.4349596898755,14.4647773211402,
4.47719277679566));
#207247=CARTESIAN_POINT('Ctrl Pts',(-19.3186140449673,12.7787196305894,
2.74076273967685));
#207248=CARTESIAN_POINT('Ctrl Pts',(-19.2022684000591,10.4757348799287,
1.99604440006967));
#207249=CARTESIAN_POINT('Ctrl Pts',(-19.0859227551509,8.09216616155139,
2.41647832579409));
#207250=CARTESIAN_POINT('Ctrl Pts',(-18.9695771102427,6.18296154499045,
3.90415118138058));
#207251=CARTESIAN_POINT('Ctrl Pts',(-18.8532314653345,5.19269172412475,
6.11267601344642));
#207252=CARTESIAN_POINT('Ctrl Pts',(-18.7368858204263,5.35192390932415,
8.52780756561754));
#207253=CARTESIAN_POINT('Ctrl Pts',(-18.6205401755181,6.62358593880632,
10.5871989100521));
#207254=CARTESIAN_POINT('Ctrl Pts',(-18.5041945306099,8.7115797094988,11.811333457023));
#207255=CARTESIAN_POINT('Ctrl Pts',(-18.3878488857017,11.1297233090374,
11.9151776120927));
#207256=CARTESIAN_POINT('Ctrl Pts',(-18.2715032407935,13.3149804406506,
10.8745556174806));
#207257=CARTESIAN_POINT('Ctrl Pts',(-18.1551575958854,14.7584982595467,
8.93176176658652));
#207258=CARTESIAN_POINT('Ctrl Pts',(-18.0388119509771,15.124224175059,6.53918074966919));
#207259=CARTESIAN_POINT('Ctrl Pts',(-17.922466306069,14.3268721721096,4.25387452102607));
#207260=CARTESIAN_POINT('Ctrl Pts',(-17.8061206611608,12.5523721092149,
2.60803953480767));
#207261=CARTESIAN_POINT('Ctrl Pts',(-17.6897750162526,10.2133449220351,
1.98475296373708));
#207262=CARTESIAN_POINT('Ctrl Pts',(-17.6122112529804,8.64164599008553,
2.34806170798548));
#207263=CARTESIAN_POINT('Ctrl Pts',(-17.5734293713444,7.94362709374212,
2.70315493841493));
#207264=CARTESIAN_POINT('Ctrl Pts',(-24.0186942234176,13.4689108572577,
3.14204861700312));
#207265=CARTESIAN_POINT('Ctrl Pts',(-23.9799084608713,12.8421275956956,
2.59950919937439));
#207266=CARTESIAN_POINT('Ctrl Pts',(-23.9023408166891,11.3198184503049,
1.82618593953407));
#207267=CARTESIAN_POINT('Ctrl Pts',(-23.7859912908707,8.75807997908655,
1.8712498170614));
#207268=CARTESIAN_POINT('Ctrl Pts',(-23.6696456459625,6.51616378181432,
3.11051078436478));
#207269=CARTESIAN_POINT('Ctrl Pts',(-23.5533000010543,5.1153879824587,5.25542276568198));
#207270=CARTESIAN_POINT('Ctrl Pts',(-23.4369543561461,4.88221296862737,
7.80654619603404));
#207271=CARTESIAN_POINT('Ctrl Pts',(-23.3206087112379,5.87079047770171,
10.1698716488929));
#207272=CARTESIAN_POINT('Ctrl Pts',(-23.2042630663297,7.85100400874307,
11.7951114604348));
#207273=CARTESIAN_POINT('Ctrl Pts',(-23.0879174214215,10.3617409892675,
12.3038394752319));
#207274=CARTESIAN_POINT('Ctrl Pts',(-22.9715717765133,12.8184066399426,
11.5776011402149));
#207275=CARTESIAN_POINT('Ctrl Pts',(-22.8552261316051,14.6489755659482,
9.78549664174713));
#207276=CARTESIAN_POINT('Ctrl Pts',(-22.7388804866969,15.427211651477,7.34480661830159));
#207277=CARTESIAN_POINT('Ctrl Pts',(-22.6225348417888,14.9719120023394,
4.82383012340355));
#207278=CARTESIAN_POINT('Ctrl Pts',(-22.5061891968806,13.3890780376071,
2.80956215996224));
#207279=CARTESIAN_POINT('Ctrl Pts',(-22.3898435519723,11.0472898813903,
1.77101002421233));
#207280=CARTESIAN_POINT('Ctrl Pts',(-22.2734979070642,8.49176130321648,
1.94999952224723));
#207281=CARTESIAN_POINT('Ctrl Pts',(-22.157152262156,6.3176511465479,3.30484283879696));
#207282=CARTESIAN_POINT('Ctrl Pts',(-22.0408066172478,5.03093678963633,
5.52009654489452));
#207283=CARTESIAN_POINT('Ctrl Pts',(-21.9244609723396,4.93174625891169,
8.07990341698975));
#207284=CARTESIAN_POINT('Ctrl Pts',(-21.8081153274314,6.04207823902469,
10.3883309154536));
#207285=CARTESIAN_POINT('Ctrl Pts',(-21.6917696825232,8.10569382361118,
11.9076611920219));
#207286=CARTESIAN_POINT('Ctrl Pts',(-21.575424037615,10.6372920779218,12.2845768181086));
#207287=CARTESIAN_POINT('Ctrl Pts',(-21.4590783927068,13.0574428215438,
11.4303747326676));
#207288=CARTESIAN_POINT('Ctrl Pts',(-21.3427327477986,14.7816348339379,
9.54592756185717));
#207289=CARTESIAN_POINT('Ctrl Pts',(-21.1876052212543,15.6746011628252,
6.23885106912733));
#207290=CARTESIAN_POINT('Ctrl Pts',(-20.993695813074,13.5625234968125,2.09280121680755));
#207291=CARTESIAN_POINT('Ctrl Pts',(-20.7610045232576,7.9771456674962,1.41129522565514));
#207292=CARTESIAN_POINT('Ctrl Pts',(-20.5670951150773,4.93010692772846,
4.92784984111965));
#207293=CARTESIAN_POINT('Ctrl Pts',(-20.411967588533,5.00168014367605,8.35261568246579));
#207294=CARTESIAN_POINT('Ctrl Pts',(-20.2956219436248,6.22216623267968,
10.5963609758821));
#207295=CARTESIAN_POINT('Ctrl Pts',(-20.1792762987167,8.36591713449647,
12.0074325175077));
#207296=CARTESIAN_POINT('Ctrl Pts',(-20.0629306538084,10.9138709321725,
12.250303996535));
#207297=CARTESIAN_POINT('Ctrl Pts',(-19.9465850089003,13.2822685207144,
11.2717506598004));
#207298=CARTESIAN_POINT('Ctrl Pts',(-19.8302393639921,14.915091230279,9.29803218421779));
#207299=CARTESIAN_POINT('Ctrl Pts',(-19.7138937190839,15.4343224407561,
6.7894770355559));
#207300=CARTESIAN_POINT('Ctrl Pts',(-19.5975480741757,14.7180220349959,
4.32982329013379));
#207301=CARTESIAN_POINT('Ctrl Pts',(-19.4812024292675,12.9334734831326,
2.49195989701346));
#207302=CARTESIAN_POINT('Ctrl Pts',(-19.3648567843593,10.4959601496402,
1.70373892335395));
#207303=CARTESIAN_POINT('Ctrl Pts',(-19.2485111394511,7.97315554545298,
2.14873244730664));
#207304=CARTESIAN_POINT('Ctrl Pts',(-19.1321654945429,5.95242496619178,
3.72330753744839));
#207305=CARTESIAN_POINT('Ctrl Pts',(-19.0158198496347,4.90430865043124,
6.06084308733203));
#207306=CARTESIAN_POINT('Ctrl Pts',(-18.8994742047265,5.07284236496551,
8.61705426452988));
#207307=CARTESIAN_POINT('Ctrl Pts',(-18.7831285598183,6.41878838205027,
10.7967447116758));
#207308=CARTESIAN_POINT('Ctrl Pts',(-18.6667829149101,8.62875206281352,
12.0923869339589));
#207309=CARTESIAN_POINT('Ctrl Pts',(-18.5504372700019,11.1881512357709,
12.2022971331103));
#207310=CARTESIAN_POINT('Ctrl Pts',(-18.4340916250937,13.5010599052218,
11.1008873273073));
#207311=CARTESIAN_POINT('Ctrl Pts',(-18.3177459801855,15.0289006474081,
9.04460540254747));
#207312=CARTESIAN_POINT('Ctrl Pts',(-18.2014003352773,15.4159903991786,
6.51226204746295));
#207313=CARTESIAN_POINT('Ctrl Pts',(-18.0850546903691,14.572061172935,4.09345992476871));
#207314=CARTESIAN_POINT('Ctrl Pts',(-17.968709045461,12.6939038979692,2.35148368177163));
#207315=CARTESIAN_POINT('Ctrl Pts',(-17.8523634005528,10.2182427132757,
1.69178789909856));
#207316=CARTESIAN_POINT('Ctrl Pts',(-17.7747996372806,8.55473317342155,
2.07631928083078));
#207317=CARTESIAN_POINT('Ctrl Pts',(-17.7360177556446,7.81593958550113,
2.45215524047243));
#207318=CARTESIAN_POINT('Ctrl Pts',(-17.734,7.81752421401937,2.45527019889639));
#207319=CARTESIAN_POINT('Ctrl Pts',(-17.734,7.95501332932839,2.39880616079669));
#207320=CARTESIAN_POINT('Ctrl Pts',(-17.734,8.09483307093976,2.34855996252215));
#207321=CARTESIAN_POINT('Ctrl Pts',(-17.734,8.23654961332729,2.30458248664204));
#207322=CARTESIAN_POINT('Ctrl Pts',(-17.734,8.37832975980054,2.26058527314275));
#207323=CARTESIAN_POINT('Ctrl Pts',(-17.734,8.5220092129709,2.22286236358206));
#207324=CARTESIAN_POINT('Ctrl Pts',(-17.734,8.66715872383441,2.19151622076045));
#207325=CARTESIAN_POINT('Ctrl Pts',(-17.734,8.73062405339664,2.17781039927443));
#207326=CARTESIAN_POINT('Ctrl Pts',(-17.734,8.79437042278305,2.16532435435612));
#207327=CARTESIAN_POINT('Ctrl Pts',(-17.734,8.85836166295589,2.15406978045215));
#207328=CARTESIAN_POINT('Ctrl Pts',(-17.734,8.89040869116538,2.1484334520045));
#207329=CARTESIAN_POINT('Ctrl Pts',(-17.734,8.92251712887927,2.14310601138362));
#207330=CARTESIAN_POINT('Ctrl Pts',(-17.734,8.95468239459414,2.13808910834503));
#207331=CARTESIAN_POINT('Ctrl Pts',(-17.734,8.98448154611367,2.13344125450384));
#207332=CARTESIAN_POINT('Ctrl Pts',(-17.734,9.01432763207528,2.12906034005483));
#207333=CARTESIAN_POINT('Ctrl Pts',(-17.734,9.04419731217815,2.12495001471572));
#207334=CARTESIAN_POINT('Ctrl Pts',(-17.734,9.18914015359341,2.10500463091048));
#207335=CARTESIAN_POINT('Ctrl Pts',(-17.734,9.33476319047707,2.09140666582529));
#207336=CARTESIAN_POINT('Ctrl Pts',(-17.734,9.48065042400814,2.08424512748072));
#207337=CARTESIAN_POINT('Ctrl Pts',(-17.734,9.62430709149771,2.07719308661478));
#207338=CARTESIAN_POINT('Ctrl Pts',(-17.734,9.76822064463766,2.07638225413551));
#207339=CARTESIAN_POINT('Ctrl Pts',(-17.734,9.91198516113969,2.08194693816168));
#207340=CARTESIAN_POINT('Ctrl Pts',(-17.734,9.99104601856735,2.085007141758));
#207341=CARTESIAN_POINT('Ctrl Pts',(-17.734,10.0700615881095,2.08999633226591));
#207342=CARTESIAN_POINT('Ctrl Pts',(-17.734,10.1489620547016,2.09694320736949));
#207343=CARTESIAN_POINT('Ctrl Pts',(-17.734,10.1675473093435,2.09857956578842));
#207344=CARTESIAN_POINT('Ctrl Pts',(-17.734,10.1861239058425,2.10032440268515));
#207345=CARTESIAN_POINT('Ctrl Pts',(-17.734,10.204682003642,2.10217705470482));
#207346=CARTESIAN_POINT('Ctrl Pts',(-17.734,10.2069686559161,2.10240533084603));
#207347=CARTESIAN_POINT('Ctrl Pts',(-17.734,10.2092550663573,2.10263524723068));
#207348=CARTESIAN_POINT('Ctrl Pts',(-17.734,10.2115412333789,2.10286680408659));
#207349=CARTESIAN_POINT('Ctrl Pts',(-17.734,10.3540154766321,2.11729745919824));
#207350=CARTESIAN_POINT('Ctrl Pts',(-17.734,10.4955450211138,2.13809494422707));
#207351=CARTESIAN_POINT('Ctrl Pts',(-17.734,10.6357416460623,2.16507440736953));
#207352=CARTESIAN_POINT('Ctrl Pts',(-17.734,10.7763962044029,2.19214199529445));
#207353=CARTESIAN_POINT('Ctrl Pts',(-17.734,10.9157098757399,2.22543235083154));
#207354=CARTESIAN_POINT('Ctrl Pts',(-17.734,11.0532754222464,2.26480926967513));
#207355=CARTESIAN_POINT('Ctrl Pts',(-17.734,11.1892331875549,2.30372597539589));
#207356=CARTESIAN_POINT('Ctrl Pts',(-17.734,11.3234841067246,2.34858822550377));
#207357=CARTESIAN_POINT('Ctrl Pts',(-17.734,11.4556098131053,2.39930790766024));
#207358=CARTESIAN_POINT('Ctrl Pts',(-17.734,11.585893305135,2.44932041080583));
#207359=CARTESIAN_POINT('Ctrl Pts',(-17.734,11.7141110086898,2.50502853560071));
#207360=CARTESIAN_POINT('Ctrl Pts',(-17.734,11.8398280865206,2.56638422249516));
#207361=CARTESIAN_POINT('Ctrl Pts',(-17.734,11.8635810775125,2.57797676905487));
#207362=CARTESIAN_POINT('Ctrl Pts',(-17.734,11.8872446880899,2.58977102047971));
#207363=CARTESIAN_POINT('Ctrl Pts',(-17.734,11.9108158217838,2.60176678408464));
#207364=CARTESIAN_POINT('Ctrl Pts',(-17.734,11.9371259496047,2.61515646986953));
#207365=CARTESIAN_POINT('Ctrl Pts',(-17.734,11.9633250773611,2.62879964621102));
#207366=CARTESIAN_POINT('Ctrl Pts',(-17.734,11.989373711485,2.64267686049565));
#207367=CARTESIAN_POINT('Ctrl Pts',(-17.734,12.1092335086399,2.7065312676527));
#207368=CARTESIAN_POINT('Ctrl Pts',(-17.734,12.2260636232258,2.77541414480518));
#207369=CARTESIAN_POINT('Ctrl Pts',(-17.734,12.3395155043836,2.84921040440292));
#207370=CARTESIAN_POINT('Ctrl Pts',(-17.734,12.3590922141296,2.86194433124259));
#207371=CARTESIAN_POINT('Ctrl Pts',(-17.734,12.3785682723977,2.87482464861868));
#207372=CARTESIAN_POINT('Ctrl Pts',(-17.734,12.397941804336,2.88785087941439));
#207373=CARTESIAN_POINT('Ctrl Pts',(-17.734,12.5137183308796,2.96569583614642));
#207374=CARTESIAN_POINT('Ctrl Pts',(-17.734,12.6258364718941,3.04874887784061));
#207375=CARTESIAN_POINT('Ctrl Pts',(-17.734,12.7340053685887,3.13669684221419));
#207376=CARTESIAN_POINT('Ctrl Pts',(-17.734,12.8413651891311,3.22398697792551));
#207377=CARTESIAN_POINT('Ctrl Pts',(-17.734,12.9448350524763,3.31609977176641));
#207378=CARTESIAN_POINT('Ctrl Pts',(-17.734,13.0440889096738,3.41275801814899));
#207379=CARTESIAN_POINT('Ctrl Pts',(-17.734,13.1288759098258,3.49532773364548));
#207380=CARTESIAN_POINT('Ctrl Pts',(-17.734,13.2105858345473,3.58121510520998));
#207381=CARTESIAN_POINT('Ctrl Pts',(-17.734,13.2889874920904,3.67025872512399));
#207382=CARTESIAN_POINT('Ctrl Pts',(-17.734,13.3046808407887,3.68808223320354));
#207383=CARTESIAN_POINT('Ctrl Pts',(-17.734,13.3202415499158,3.70603222587404));
#207384=CARTESIAN_POINT('Ctrl Pts',(-17.734,13.3356676287495,3.72410744241816));
#207385=CARTESIAN_POINT('Ctrl Pts',(-17.734,13.3480960124007,3.73867016624531));
#207386=CARTESIAN_POINT('Ctrl Pts',(-17.734,13.3604375218648,3.75331488553882));
#207387=CARTESIAN_POINT('Ctrl Pts',(-17.734,13.3726806466598,3.76802811897179));
#207388=CARTESIAN_POINT('Ctrl Pts',(-17.734,13.4596595863362,3.87255547327408));
#207389=CARTESIAN_POINT('Ctrl Pts',(-17.734,13.5418047089289,3.98068713564632));
#207390=CARTESIAN_POINT('Ctrl Pts',(-17.734,13.6188521515589,4.09212747512559));
#207391=CARTESIAN_POINT('Ctrl Pts',(-17.734,13.6955050681823,4.20299717772703));
#207392=CARTESIAN_POINT('Ctrl Pts',(-17.734,13.7671127723517,4.31714241929128));
#207393=CARTESIAN_POINT('Ctrl Pts',(-17.734,13.8333700251483,4.43429573902715));
#207394=CARTESIAN_POINT('Ctrl Pts',(-17.734,13.8529952952312,4.46899632566313));
#207395=CARTESIAN_POINT('Ctrl Pts',(-17.734,13.8721508267902,4.50396094344829));
#207396=CARTESIAN_POINT('Ctrl Pts',(-17.734,13.89082783933,4.53918291414616));
#207397=CARTESIAN_POINT('Ctrl Pts',(-17.734,13.9541037547201,4.65851155051141));
#207398=CARTESIAN_POINT('Ctrl Pts',(-17.734,14.0118911506689,4.78079380916991));
#207399=CARTESIAN_POINT('Ctrl Pts',(-17.734,14.0640355569298,4.90562952893941));
#207400=CARTESIAN_POINT('Ctrl Pts',(-17.734,14.1069769502113,5.00843288068092));
#207401=CARTESIAN_POINT('Ctrl Pts',(-17.734,14.1460905703569,5.11296827640031));
#207402=CARTESIAN_POINT('Ctrl Pts',(-17.734,14.181263595494,5.21901089821796));
#207403=CARTESIAN_POINT('Ctrl Pts',(-17.734,14.189228939926,5.24302549474362));
#207404=CARTESIAN_POINT('Ctrl Pts',(-17.734,14.1969936498824,5.26712264831227));
#207405=CARTESIAN_POINT('Ctrl Pts',(-17.734,14.2045469401604,5.29126909440454));
#207406=CARTESIAN_POINT('Ctrl Pts',(-17.734,14.2441345445802,5.41782320802469));
#207407=CARTESIAN_POINT('Ctrl Pts',(-17.734,14.2779661336648,5.54586509835337));
#207408=CARTESIAN_POINT('Ctrl Pts',(-17.734,14.3059575691914,5.67500275481732));
#207409=CARTESIAN_POINT('Ctrl Pts',(-17.734,14.3337111014901,5.80304285180508));
#207410=CARTESIAN_POINT('Ctrl Pts',(-17.734,14.3557233452508,5.93216096675456));
#207411=CARTESIAN_POINT('Ctrl Pts',(-17.734,14.3718618342412,6.06197882819122));
#207412=CARTESIAN_POINT('Ctrl Pts',(-17.734,14.3878809810452,6.19083670214492));
#207413=CARTESIAN_POINT('Ctrl Pts',(-17.734,14.3981129478512,6.32038474523077));
#207414=CARTESIAN_POINT('Ctrl Pts',(-17.734,14.4023779577645,6.45024544035567));
#207415=CARTESIAN_POINT('Ctrl Pts',(-17.734,14.404077015673,6.50197822540308));
#207416=CARTESIAN_POINT('Ctrl Pts',(-17.734,14.4048285550272,6.55376048351597));
#207417=CARTESIAN_POINT('Ctrl Pts',(-17.734,14.4046189505891,6.60556761626202));
#207418=CARTESIAN_POINT('Ctrl Pts',(-17.734,14.4041999753073,6.7091241450779));
#207419=CARTESIAN_POINT('Ctrl Pts',(-17.734,14.3999416905426,6.8127807955209));
#207420=CARTESIAN_POINT('Ctrl Pts',(-17.734,14.3918515993157,6.91632173312881));
#207421=CARTESIAN_POINT('Ctrl Pts',(-23.534,12.9193325810254,3.77664721604209));
#207422=CARTESIAN_POINT('Ctrl Pts',(-23.534,12.8290342749467,3.68176973928167));
#207423=CARTESIAN_POINT('Ctrl Pts',(-23.534,12.7344699653718,3.59136003915295));
#207424=CARTESIAN_POINT('Ctrl Pts',(-23.534,12.6360835972834,3.50554511160901));
#207425=CARTESIAN_POINT('Ctrl Pts',(-23.534,12.5375436323605,3.41959621325707));
#207426=CARTESIAN_POINT('Ctrl Pts',(-23.534,12.4351690929809,3.33825596343349));
#207427=CARTESIAN_POINT('Ctrl Pts',(-23.534,12.3293560803945,3.26167549385161));
#207428=CARTESIAN_POINT('Ctrl Pts',(-23.534,12.2223961810542,3.18426498338892));
#207429=CARTESIAN_POINT('Ctrl Pts',(-23.534,12.111922327755,3.11171743092897));
#207430=CARTESIAN_POINT('Ctrl Pts',(-23.534,11.9983009629277,3.04422091350619));
#207431=CARTESIAN_POINT('Ctrl Pts',(-23.534,11.8876418446549,2.97848411201776));
#207432=CARTESIAN_POINT('Ctrl Pts',(-23.534,11.7739964774377,2.91753808376478));
#207433=CARTESIAN_POINT('Ctrl Pts',(-23.534,11.6576727871419,2.86159294221042));
#207434=CARTESIAN_POINT('Ctrl Pts',(-23.534,11.6332495630019,2.84984674736182));
#207435=CARTESIAN_POINT('Ctrl Pts',(-23.534,11.6087081820176,2.83832114633447));
#207436=CARTESIAN_POINT('Ctrl Pts',(-23.534,11.5840513615887,2.82701831535873));
#207437=CARTESIAN_POINT('Ctrl Pts',(-23.534,11.5622209636691,2.81701113302431));
#207438=CARTESIAN_POINT('Ctrl Pts',(-23.534,11.5402959333441,2.80717685242453));
#207439=CARTESIAN_POINT('Ctrl Pts',(-23.534,11.5183047885456,2.79752845804063));
#207440=CARTESIAN_POINT('Ctrl Pts',(-23.534,11.3911942477278,2.74175998216545));
#207441=CARTESIAN_POINT('Ctrl Pts',(-23.534,11.2617238431345,2.69212530511711));
#207442=CARTESIAN_POINT('Ctrl Pts',(-23.534,11.1303326631264,2.64879502193041));
#207443=CARTESIAN_POINT('Ctrl Pts',(-23.534,11.0033822809627,2.60692922843141));
#207444=CARTESIAN_POINT('Ctrl Pts',(-23.534,10.8746380135545,2.57094816886311));
#207445=CARTESIAN_POINT('Ctrl Pts',(-23.534,10.744524252389,2.54079174717232));
#207446=CARTESIAN_POINT('Ctrl Pts',(-23.534,10.6129949118458,2.51030723713584));
#207447=CARTESIAN_POINT('Ctrl Pts',(-23.534,10.4800654160338,2.48577456351454));
#207448=CARTESIAN_POINT('Ctrl Pts',(-23.534,10.3461486693946,2.46717850659781));
#207449=CARTESIAN_POINT('Ctrl Pts',(-23.534,10.211711690067,2.44851020870358));
#207450=CARTESIAN_POINT('Ctrl Pts',(-23.534,10.0762789980584,2.43582454854997));
#207451=CARTESIAN_POINT('Ctrl Pts',(-23.534,9.94025397646493,2.42915620857004));
#207452=CARTESIAN_POINT('Ctrl Pts',(-23.534,9.9245534826481,2.42838652495304));
#207453=CARTESIAN_POINT('Ctrl Pts',(-23.534,9.9088450894565,2.42769706425901));
#207454=CARTESIAN_POINT('Ctrl Pts',(-23.534,9.89312941238515,2.42708792441797));
#207455=CARTESIAN_POINT('Ctrl Pts',(-23.534,9.86982544152734,2.42618466221429));
#207456=CARTESIAN_POINT('Ctrl Pts',(-23.534,9.84650207816375,2.425458012161));
#207457=CARTESIAN_POINT('Ctrl Pts',(-23.534,9.82318746608169,2.4249087042635));
#207458=CARTESIAN_POINT('Ctrl Pts',(-23.534,9.68481926730006,2.42164865669821));
#207459=CARTESIAN_POINT('Ctrl Pts',(-23.534,9.54658084862216,2.42462233472131));
#207460=CARTESIAN_POINT('Ctrl Pts',(-23.534,9.40891306409928,2.43376529968542));
#207461=CARTESIAN_POINT('Ctrl Pts',(-23.534,9.26969699145749,2.44301109149514));
#207462=CARTESIAN_POINT('Ctrl Pts',(-23.534,9.13106368655266,2.45856549918087));
#207463=CARTESIAN_POINT('Ctrl Pts',(-23.534,8.99345056596637,2.48041133998068));
#207464=CARTESIAN_POINT('Ctrl Pts',(-23.534,8.97031116334576,2.48408467943915));
#207465=CARTESIAN_POINT('Ctrl Pts',(-23.534,8.94720057917996,2.48793601825196));
#207466=CARTESIAN_POINT('Ctrl Pts',(-23.534,8.9241208670849,2.49196541689415));
#207467=CARTESIAN_POINT('Ctrl Pts',(-23.534,8.7873871274078,2.51583723742324));
#207468=CARTESIAN_POINT('Ctrl Pts',(-23.534,8.65173684163142,2.54595438851018));
#207469=CARTESIAN_POINT('Ctrl Pts',(-23.534,8.51752579699816,2.58210352084366));
#207470=CARTESIAN_POINT('Ctrl Pts',(-23.534,8.39200772104798,2.61591124173701));
#207471=CARTESIAN_POINT('Ctrl Pts',(-23.534,8.2677479659076,2.65499549928287));
#207472=CARTESIAN_POINT('Ctrl Pts',(-23.534,8.14504361020047,2.69922256987843));
#207473=CARTESIAN_POINT('Ctrl Pts',(-23.534,8.12749669976606,2.70554710857997));
#207474=CARTESIAN_POINT('Ctrl Pts',(-23.534,8.10998161428438,2.71197687835703));
#207475=CARTESIAN_POINT('Ctrl Pts',(-23.534,8.09249924250724,2.71851155108686));
#207476=CARTESIAN_POINT('Ctrl Pts',(-23.534,8.07453683582073,2.72522565433514));
#207477=CARTESIAN_POINT('Ctrl Pts',(-23.534,8.05661738961167,2.73204736693228));
#207478=CARTESIAN_POINT('Ctrl Pts',(-23.534,8.03874521119562,2.73897465977803));
#207479=CARTESIAN_POINT('Ctrl Pts',(-23.534,7.90644077728778,2.79025612850192));
#207480=CARTESIAN_POINT('Ctrl Pts',(-23.534,7.77666647852651,2.84734176999563));
#207481=CARTESIAN_POINT('Ctrl Pts',(-23.534,7.64978171058127,2.90995636965286));
#207482=CARTESIAN_POINT('Ctrl Pts',(-23.534,7.52165755881585,2.97318257559647));
#207483=CARTESIAN_POINT('Ctrl Pts',(-23.534,7.39647891359876,3.04204645156364));
#207484=CARTESIAN_POINT('Ctrl Pts',(-23.534,7.27461872478453,3.11631789506347));
#207485=CARTESIAN_POINT('Ctrl Pts',(-23.534,7.15263517659778,3.19066452373046));
#207486=CARTESIAN_POINT('Ctrl Pts',(-23.534,7.03397603470935,3.27042992499855));
#207487=CARTESIAN_POINT('Ctrl Pts',(-23.534,6.91902974171529,3.35543308857631));
#207488=CARTESIAN_POINT('Ctrl Pts',(-23.534,6.88443823547605,3.38101362176852));
#207489=CARTESIAN_POINT('Ctrl Pts',(-23.534,6.8501831168222,3.40706882773967));
#207490=CARTESIAN_POINT('Ctrl Pts',(-23.534,6.81627539023442,3.43359460199418));
#207491=CARTESIAN_POINT('Ctrl Pts',(-23.534,6.76396915960913,3.47451339559359));
#207492=CARTESIAN_POINT('Ctrl Pts',(-23.534,6.71248951985117,3.51655187486385));
#207493=CARTESIAN_POINT('Ctrl Pts',(-23.534,6.66185982789806,3.55967699429164));
#207494=CARTESIAN_POINT('Ctrl Pts',(-23.534,6.63093354883434,3.58601923392675));
#207495=CARTESIAN_POINT('Ctrl Pts',(-23.534,6.60032442690432,3.6127669567928));
#207496=CARTESIAN_POINT('Ctrl Pts',(-23.534,6.5700380650519,3.63991298274907));
#207497=CARTESIAN_POINT('Ctrl Pts',(-23.534,6.54970174956393,3.65814066393382));
#207498=CARTESIAN_POINT('Ctrl Pts',(-23.534,6.52950985990992,3.67654895545334));
#207499=CARTESIAN_POINT('Ctrl Pts',(-23.534,6.50946759143304,3.69513255183675));
#207500=CARTESIAN_POINT('Ctrl Pts',(-23.534,6.48629939502987,3.71661457176801));
#207501=CARTESIAN_POINT('Ctrl Pts',(-23.534,6.46334194239172,3.73832084933172));
#207502=CARTESIAN_POINT('Ctrl Pts',(-23.534,6.44060381900491,3.76024083524255));
#207503=CARTESIAN_POINT('Ctrl Pts',(-23.534,6.33630358435424,3.86078825664344));
#207504=CARTESIAN_POINT('Ctrl Pts',(-23.534,6.23656911765673,3.96587231787068));
#207505=CARTESIAN_POINT('Ctrl Pts',(-23.534,6.14160415274189,4.07509691465864));
#207506=CARTESIAN_POINT('Ctrl Pts',(-23.534,6.04554420146357,4.18558091741959));
#207507=CARTESIAN_POINT('Ctrl Pts',(-23.534,5.9543637852261,4.30030196798446));
#207508=CARTESIAN_POINT('Ctrl Pts',(-23.534,5.86830289292554,4.41889447763156));
#207509=CARTESIAN_POINT('Ctrl Pts',(-23.534,5.82757976357167,4.47501123382195));
#207510=CARTESIAN_POINT('Ctrl Pts',(-23.534,5.78800341363274,4.53199543604809));
#207511=CARTESIAN_POINT('Ctrl Pts',(-23.534,5.74960209595384,4.58981127009334));
#207512=CARTESIAN_POINT('Ctrl Pts',(-23.534,5.73602768423563,4.61024848377764));
#207513=CARTESIAN_POINT('Ctrl Pts',(-23.534,5.72260309324962,4.63078521650428));
#207514=CARTESIAN_POINT('Ctrl Pts',(-23.534,5.7093336961382,4.65141296650499));
#207515=CARTESIAN_POINT('Ctrl Pts',(-23.534,5.62878693151662,4.77662577836291));
#207516=CARTESIAN_POINT('Ctrl Pts',(-23.534,5.55390603885587,4.90526364111019));
#207517=CARTESIAN_POINT('Ctrl Pts',(-23.534,5.48492211365496,5.03693496093977));
#207518=CARTESIAN_POINT('Ctrl Pts',(-23.534,5.43386982584413,5.13437972211847));
#207519=CARTESIAN_POINT('Ctrl Pts',(-23.534,5.38604780954608,5.23348685196463));
#207520=CARTESIAN_POINT('Ctrl Pts',(-23.534,5.34156275575684,5.33411058694693));
#207521=CARTESIAN_POINT('Ctrl Pts',(-23.534,5.29184265751413,5.4465758210584));
#207522=CARTESIAN_POINT('Ctrl Pts',(-23.534,5.24629059068216,5.56093558465364));
#207523=CARTESIAN_POINT('Ctrl Pts',(-23.534,5.20492644341908,5.67694766332001));
#207524=CARTESIAN_POINT('Ctrl Pts',(-23.5319822466055,5.20171862064502,
8.32379167009335));
#207525=CARTESIAN_POINT('Ctrl Pts',(-23.4932003649694,5.41676747330397,
9.12430564500732));
#207526=CARTESIAN_POINT('Ctrl Pts',(-23.4156366016973,6.24411030078641,
10.617835827178));
#207527=CARTESIAN_POINT('Ctrl Pts',(-23.2992909567891,8.39090024522478,
12.0161880404286));
#207528=CARTESIAN_POINT('Ctrl Pts',(-23.1829453118809,10.9421734655344,
12.2463212707424));
#207529=CARTESIAN_POINT('Ctrl Pts',(-23.0665996669727,13.304392578115,11.2549883803824));
#207530=CARTESIAN_POINT('Ctrl Pts',(-22.9502540220645,14.927276862139,9.2728561879833));
#207531=CARTESIAN_POINT('Ctrl Pts',(-22.8339083771563,15.4330671204992,
6.7615280730017));
#207532=CARTESIAN_POINT('Ctrl Pts',(-22.7175627322481,14.7039361435109,
4.30571495106923));
#207533=CARTESIAN_POINT('Ctrl Pts',(-22.6012170873399,12.9096846230479,
2.47725497604962));
#207534=CARTESIAN_POINT('Ctrl Pts',(-22.4848714424317,10.4680804717197,
1.70188576751079));
#207535=CARTESIAN_POINT('Ctrl Pts',(-22.3685257975235,7.94764111846411,
2.16015054073166));
#207536=CARTESIAN_POINT('Ctrl Pts',(-22.2521801526153,5.93523494026475,
3.74534471809911));
#207537=CARTESIAN_POINT('Ctrl Pts',(-22.1358345077071,4.89943419990334,
6.08836351785797));
#207538=CARTESIAN_POINT('Ctrl Pts',(-22.0194888627989,5.08142954165806,
8.64365537460478));
#207539=CARTESIAN_POINT('Ctrl Pts',(-21.9031432178907,6.43882069342724,
10.8162233567271));
#207540=CARTESIAN_POINT('Ctrl Pts',(-21.7867975729826,8.65559778633532,
12.1002259870008));
#207541=CARTESIAN_POINT('Ctrl Pts',(-21.6704519280743,11.2154925541789,
12.1966333884833));
#207542=CARTESIAN_POINT('Ctrl Pts',(-21.5541062831661,13.5226699559939,
11.0831186756717));
#207543=CARTESIAN_POINT('Ctrl Pts',(-21.4377606382579,15.0394563872939,
9.01870375488018));
#207544=CARTESIAN_POINT('Ctrl Pts',(-21.3214149933497,15.4136431368683,
6.48460438397758));
#207545=CARTESIAN_POINT('Ctrl Pts',(-21.2050693484416,14.5560831704402,
4.06976232245845));
#207546=CARTESIAN_POINT('Ctrl Pts',(-21.0887237035334,12.6706797211637,
2.33877575209256));
#207547=CARTESIAN_POINT('Ctrl Pts',(-20.9723780586252,10.1876014272064,
1.68985066266665));
#207548=CARTESIAN_POINT('Ctrl Pts',(-20.856032413717,7.70350655415105,2.28420940052766));
#207549=CARTESIAN_POINT('Ctrl Pts',(-20.7009048871727,5.11052082316887,
4.5226382644136));
#207550=CARTESIAN_POINT('Ctrl Pts',(-20.5069954789924,4.53607622899261,
9.14006197037595));
#207551=CARTESIAN_POINT('Ctrl Pts',(-20.274304189176,8.77988224509149,12.8347910532216));
#207552=CARTESIAN_POINT('Ctrl Pts',(-20.0803947809957,13.2742515855875,
11.6301199348782));
#207553=CARTESIAN_POINT('Ctrl Pts',(-19.9252672544514,15.1343801571744,
8.75365326951933));
#207554=CARTESIAN_POINT('Ctrl Pts',(-19.8089216095432,15.3810853499648,
6.21138534590041));
#207555=CARTESIAN_POINT('Ctrl Pts',(-19.692575964635,14.3964856232887,3.84129147353207));
#207556=CARTESIAN_POINT('Ctrl Pts',(-19.5762303197268,12.4224121035996,
2.21215231060185));
#207557=CARTESIAN_POINT('Ctrl Pts',(-19.4598846748187,9.91250172714882,
1.69521790442747));
#207558=CARTESIAN_POINT('Ctrl Pts',(-19.3435390299104,7.45404844673223,
2.4147196856449));
#207559=CARTESIAN_POINT('Ctrl Pts',(-19.2271933850022,5.6181127491502,4.20127787325212));
#207560=CARTESIAN_POINT('Ctrl Pts',(-19.110847740094,4.83283831742701,6.63978697636726));
#207561=CARTESIAN_POINT('Ctrl Pts',(-18.9945020951859,5.28075719645332,
9.16203285797858));
#207562=CARTESIAN_POINT('Ctrl Pts',(-18.8781564502777,6.85772444914764,
11.1809280306217));
#207563=CARTESIAN_POINT('Ctrl Pts',(-18.7618108053695,9.19648123363852,
12.2262887716303));
#207564=CARTESIAN_POINT('Ctrl Pts',(-18.6454651604612,11.7524966959059,
12.054755293186));
#207565=CARTESIAN_POINT('Ctrl Pts',(-18.5291195155531,13.9306022671102,
10.7062463423646));
#207566=CARTESIAN_POINT('Ctrl Pts',(-18.4127738706449,15.2236468447518,
8.49476382462988));
#207567=CARTESIAN_POINT('Ctrl Pts',(-18.2964282257367,15.3305503344285,
5.93523402802474));
#207568=CARTESIAN_POINT('Ctrl Pts',(-18.1800825808285,14.2264204181411,
3.62362736397207));
#207569=CARTESIAN_POINT('Ctrl Pts',(-18.0637369359203,12.1683508661136,
2.09819164983995));
#207570=CARTESIAN_POINT('Ctrl Pts',(-17.9473912910121,9.63554082881353,
1.71410391713887));
#207571=CARTESIAN_POINT('Ctrl Pts',(-17.8310456461039,7.21776027584542,
2.56082103887325));
#207572=CARTESIAN_POINT('Ctrl Pts',(-17.7147000011957,5.47793063941487,
4.44113863536456));
#207573=CARTESIAN_POINT('Ctrl Pts',(-17.5983543562875,4.82125235646171,
6.91734413330858));
#207574=CARTESIAN_POINT('Ctrl Pts',(-17.4820087113793,5.40043672555636,
9.41264007065955));
#207575=CARTESIAN_POINT('Ctrl Pts',(-17.365659185369,7.08108537827514,11.3465361450299));
#207576=CARTESIAN_POINT('Ctrl Pts',(-17.2880915409948,8.67440018888338,
11.9603782381559));
#207577=CARTESIAN_POINT('Ctrl Pts',(-17.2493057782566,9.49698541727643,
12.0631392445802));
#207578=CARTESIAN_POINT('Ctrl Pts',(-23.6945707061519,5.47368749304882,
8.25073036722769));
#207579=CARTESIAN_POINT('Ctrl Pts',(-23.6557888245159,5.67686759799619,
9.00706322566336));
#207580=CARTESIAN_POINT('Ctrl Pts',(-23.5782250612437,6.45854859948439,
10.4181640774162));
#207581=CARTESIAN_POINT('Ctrl Pts',(-23.4618794163355,8.48685519502201,
11.7393399215497));
#207582=CARTESIAN_POINT('Ctrl Pts',(-23.3455337714274,10.8973212553735,
11.9567718832129));
#207583=CARTESIAN_POINT('Ctrl Pts',(-23.2291881265191,13.1291672813738,
11.0201515841008));
#207584=CARTESIAN_POINT('Ctrl Pts',(-23.112842481611,14.6624830608743,9.14741512495814));
#207585=CARTESIAN_POINT('Ctrl Pts',(-22.9964968367027,15.1403582808735,
6.77468956213704));
#207586=CARTESIAN_POINT('Ctrl Pts',(-22.8801511917946,14.4514687258114,
4.45441506787272));
#207587=CARTESIAN_POINT('Ctrl Pts',(-22.7638055468864,12.7562436282479,
2.72686951241825));
#207588=CARTESIAN_POINT('Ctrl Pts',(-22.6474599019782,10.4493938981843,
1.99429365713702));
#207589=CARTESIAN_POINT('Ctrl Pts',(-22.53111425707,8.06805995486816,2.42726636806037));
#207590=CARTESIAN_POINT('Ctrl Pts',(-22.4147686121618,6.1667203595729,3.92497219321195));
#207591=CARTESIAN_POINT('Ctrl Pts',(-22.2984229672536,5.18808643277415,
6.13867758964879));
#207592=CARTESIAN_POINT('Ctrl Pts',(-22.1820773223454,5.36003728106023,
8.55294049412641));
#207593=CARTESIAN_POINT('Ctrl Pts',(-22.0657316774372,6.64251274308225,
10.6056024132903));
#207594=CARTESIAN_POINT('Ctrl Pts',(-21.949386032529,8.73694383077701,11.8187397350944));
#207595=CARTESIAN_POINT('Ctrl Pts',(-21.8330403876208,11.1555556073744,
11.9098263217407));
#207596=CARTESIAN_POINT('Ctrl Pts',(-21.7166947427126,13.3353977262086,
10.857767529461));
#207597=CARTESIAN_POINT('Ctrl Pts',(-21.6003490978044,14.7684712929067,
8.90728960281731));
#207598=CARTESIAN_POINT('Ctrl Pts',(-21.4840034528962,15.1220063251024,
6.51304955102958));
#207599=CARTESIAN_POINT('Ctrl Pts',(-21.367657807988,14.311775896885,4.23148488595831));
#207600=CARTESIAN_POINT('Ctrl Pts',(-21.2513121630798,12.5304296308826,
2.59603308660738));
#207601=CARTESIAN_POINT('Ctrl Pts',(-21.1349665181716,10.184394754989,1.98292278100795));
#207602=CARTESIAN_POINT('Ctrl Pts',(-21.0186208732634,7.83739940595061,
2.54447830312228));
#207603=CARTESIAN_POINT('Ctrl Pts',(-20.8634933467192,5.38752298748152,
4.65936618026363));
#207604=CARTESIAN_POINT('Ctrl Pts',(-20.6695839385389,4.84478252879942,
9.02194994466884));
#207605=CARTESIAN_POINT('Ctrl Pts',(-20.4368926487225,8.85436891378104,
12.5127634669118));
#207606=CARTESIAN_POINT('Ctrl Pts',(-20.2429832405422,13.1006897984706,
11.374579276549));
#207607=CARTESIAN_POINT('Ctrl Pts',(-20.0878557139979,14.8581561309695,
8.65686750213595));
#207608=CARTESIAN_POINT('Ctrl Pts',(-19.9715100690897,15.0912454329697,
6.25490972771149));
#207609=CARTESIAN_POINT('Ctrl Pts',(-19.8551644241815,14.1609866879279,
4.01562355729595));
#207610=CARTESIAN_POINT('Ctrl Pts',(-19.7388187792733,12.2958641357962,
2.47639811151788));
#207611=CARTESIAN_POINT('Ctrl Pts',(-19.6224731343651,9.92447806518769,
1.98799379966607));
#207612=CARTESIAN_POINT('Ctrl Pts',(-19.5061274894569,7.60170912526025,
2.66778560329601));
#207613=CARTESIAN_POINT('Ctrl Pts',(-19.3897818445487,5.86710043937747,
4.35574197025367));
#207614=CARTESIAN_POINT('Ctrl Pts',(-19.2734361996405,5.12516603946211,
6.65966747071569));
#207615=CARTESIAN_POINT('Ctrl Pts',(-19.1570905547323,5.54836385578716,
9.04270823839462));
#207616=CARTESIAN_POINT('Ctrl Pts',(-19.0407449098241,7.0382968079482,10.9501786944492));
#207617=CARTESIAN_POINT('Ctrl Pts',(-18.9243992649159,9.24797541373385,
11.9378449965002));
#207618=CARTESIAN_POINT('Ctrl Pts',(-18.8080536200077,11.6629219872652,
11.775778611484));
#207619=CARTESIAN_POINT('Ctrl Pts',(-18.6917079750996,13.7208158707802,
10.5016951334156));
#207620=CARTESIAN_POINT('Ctrl Pts',(-18.5753623301913,14.9424961064032,
8.41226640832857));
#207621=CARTESIAN_POINT('Ctrl Pts',(-18.4590166852832,15.0434994922998,
5.99399945986498));
#207622=CARTESIAN_POINT('Ctrl Pts',(-18.342671040375,14.0003075408293,3.80997253392679));
#207623=CARTESIAN_POINT('Ctrl Pts',(-18.2263253954668,12.0558247761009,
2.36872704642182));
#207624=CARTESIAN_POINT('Ctrl Pts',(-18.1099797505586,9.66280289838584,
2.00583747563687));
#207625=CARTESIAN_POINT('Ctrl Pts',(-17.9936341056504,7.37846191996246,
2.8058234859206));
#207626=CARTESIAN_POINT('Ctrl Pts',(-17.8772884607422,5.73465511165029,
4.58236459211928));
#207627=CARTESIAN_POINT('Ctrl Pts',(-17.760942815834,5.11421951854028,6.92190598805235));
#207628=CARTESIAN_POINT('Ctrl Pts',(-17.6445971709258,5.66143815952116,
9.27948420415084));
#207629=CARTESIAN_POINT('Ctrl Pts',(-17.5282476449155,7.24933023807416,
11.1066467418232));
#207630=CARTESIAN_POINT('Ctrl Pts',(-17.4506800005413,8.75470851110772,
11.6866103145668));
#207631=CARTESIAN_POINT('Ctrl Pts',(-17.411894237803,9.53189448985888,11.7836998447437));
#207632=CARTESIAN_POINT('Ctrl Pts',(-23.8571591656983,5.74565636545262,
8.17766906436202));
#207633=CARTESIAN_POINT('Ctrl Pts',(-23.8183772840622,5.93696772268841,
8.88982080631942));
#207634=CARTESIAN_POINT('Ctrl Pts',(-23.7408135207901,6.67298689818237,
10.2184923276544));
#207635=CARTESIAN_POINT('Ctrl Pts',(-23.6244678758819,8.58281014481923,
11.4624918026709));
#207636=CARTESIAN_POINT('Ctrl Pts',(-23.5081222309737,10.8524690452125,
11.6672224956832));
#207637=CARTESIAN_POINT('Ctrl Pts',(-23.3917765860655,12.9539419846326,
10.7853147878191));
#207638=CARTESIAN_POINT('Ctrl Pts',(-23.2754309411573,14.3976892596095,
9.021974061933));
#207639=CARTESIAN_POINT('Ctrl Pts',(-23.1590852962491,14.8476494412477,
6.78785105127238));
#207640=CARTESIAN_POINT('Ctrl Pts',(-23.0427396513409,14.1990013081117,
4.6031151846762));
#207641=CARTESIAN_POINT('Ctrl Pts',(-22.9263940064328,12.6028026334481,
2.97648404878689));
#207642=CARTESIAN_POINT('Ctrl Pts',(-22.8100483615245,10.4307073246489,
2.28670154676325));
#207643=CARTESIAN_POINT('Ctrl Pts',(-22.6937027166164,8.18847879127224,
2.69438219538906));
#207644=CARTESIAN_POINT('Ctrl Pts',(-22.5773570717082,6.39820577888104,
4.10459966832482));
#207645=CARTESIAN_POINT('Ctrl Pts',(-22.4610114268,5.47673866564495,6.18899166143961));
#207646=CARTESIAN_POINT('Ctrl Pts',(-22.3446657818918,5.6386450204624,8.46222561364805));
#207647=CARTESIAN_POINT('Ctrl Pts',(-22.2283201369836,6.84620479273727,
10.3949814698534));
#207648=CARTESIAN_POINT('Ctrl Pts',(-22.1119744920754,8.81828987521867,
11.5372534831879));
#207649=CARTESIAN_POINT('Ctrl Pts',(-21.9956288471672,11.0956186605698,
11.6230192549981));
#207650=CARTESIAN_POINT('Ctrl Pts',(-21.879283202259,13.1481254964233,10.6324163832503));
#207651=CARTESIAN_POINT('Ctrl Pts',(-21.7629375573508,14.4974861985194,
8.79587545075443));
#207652=CARTESIAN_POINT('Ctrl Pts',(-21.6465919124426,14.8303695133365,
6.54149471808157));
#207653=CARTESIAN_POINT('Ctrl Pts',(-21.5302462675344,14.0674686233298,
4.39320744945815));
#207654=CARTESIAN_POINT('Ctrl Pts',(-21.4139006226262,12.3901795406013,
2.8532904211222));
#207655=CARTESIAN_POINT('Ctrl Pts',(-21.297554977718,10.1811880827716,2.27599489934924));
#207656=CARTESIAN_POINT('Ctrl Pts',(-21.1812093328098,7.97129225775015,
2.80474720571691));
#207657=CARTESIAN_POINT('Ctrl Pts',(-21.0260818062656,5.66452515179418,
4.79609409611365));
#207658=CARTESIAN_POINT('Ctrl Pts',(-20.8321723980852,5.1534888286062,8.90383791896172));
#207659=CARTESIAN_POINT('Ctrl Pts',(-20.5994811082689,8.92885558247061,
12.1907358806019));
#207660=CARTESIAN_POINT('Ctrl Pts',(-20.4055717000885,12.9271280113536,
11.1190386182196));
#207661=CARTESIAN_POINT('Ctrl Pts',(-20.2504441735443,14.5819321047646,
8.56008173475257));
#207662=CARTESIAN_POINT('Ctrl Pts',(-20.1340985286361,14.8014055159746,
6.29843410952257));
#207663=CARTESIAN_POINT('Ctrl Pts',(-20.0177528837279,13.925487752567,4.18995564105982));
#207664=CARTESIAN_POINT('Ctrl Pts',(-19.9014072388197,12.1693161679927,
2.74064391243392));
#207665=CARTESIAN_POINT('Ctrl Pts',(-19.7850615939115,9.93645440322659,
2.28076969490466));
#207666=CARTESIAN_POINT('Ctrl Pts',(-19.6687159490033,7.74936980378826,
2.92085152094712));
#207667=CARTESIAN_POINT('Ctrl Pts',(-19.5523703040951,6.11608812960472,
4.51020606725524));
#207668=CARTESIAN_POINT('Ctrl Pts',(-19.4360246591869,5.41749376149721,
6.67954796506412));
#207669=CARTESIAN_POINT('Ctrl Pts',(-19.3196790142787,5.81597051512098,
8.92338361881067));
#207670=CARTESIAN_POINT('Ctrl Pts',(-19.2033333693705,7.21886916674878,
10.7194293582766));
#207671=CARTESIAN_POINT('Ctrl Pts',(-19.0869877244623,9.29946959382919,
11.6494012213701));
#207672=CARTESIAN_POINT('Ctrl Pts',(-18.9706420795541,11.5733472786245,
11.4968019297822));
#207673=CARTESIAN_POINT('Ctrl Pts',(-18.8542964346459,13.51102947445,10.2971439244665));
#207674=CARTESIAN_POINT('Ctrl Pts',(-18.7379507897377,14.6613453680545,
8.32976899202724));
#207675=CARTESIAN_POINT('Ctrl Pts',(-18.6216051448295,14.756448650171,6.05276489170521));
#207676=CARTESIAN_POINT('Ctrl Pts',(-18.5052594999214,13.7741946635174,
3.9963177038815));
#207677=CARTESIAN_POINT('Ctrl Pts',(-18.3889138550131,11.9432986860881,
2.6392624430037));
#207678=CARTESIAN_POINT('Ctrl Pts',(-18.272568210105,9.69006496795816,2.29757103413487));
#207679=CARTESIAN_POINT('Ctrl Pts',(-18.1562225651967,7.5391635640795,3.05082593296795));
#207680=CARTESIAN_POINT('Ctrl Pts',(-18.0398769202886,5.9913795838857,4.72359054887402));
#207681=CARTESIAN_POINT('Ctrl Pts',(-17.9235312753804,5.40718668061885,
6.9264678427961));
#207682=CARTESIAN_POINT('Ctrl Pts',(-17.8071856304722,5.92243959348596,
9.14632833764213));
#207683=CARTESIAN_POINT('Ctrl Pts',(-17.6908361044619,7.41757509787318,
10.8667573386166));
#207684=CARTESIAN_POINT('Ctrl Pts',(-17.6132684600876,8.83501683333207,
11.4128423909775));
#207685=CARTESIAN_POINT('Ctrl Pts',(-17.5744826973495,9.56680356244131,
11.5042604449073));
#207686=CARTESIAN_POINT('Ctrl Pts',(-24.0197476252447,6.01762523785643,
8.10460776149636));
#207687=CARTESIAN_POINT('Ctrl Pts',(-23.9809657436086,6.19706784738064,
8.77257838697545));
#207688=CARTESIAN_POINT('Ctrl Pts',(-23.9034019803365,6.88742519688036,
10.0188205778924));
#207689=CARTESIAN_POINT('Ctrl Pts',(-23.7870563354283,8.67876509461647,
11.185643683792));
#207690=CARTESIAN_POINT('Ctrl Pts',(-23.6707106905201,10.8076168350517,
11.3776731081537));
#207691=CARTESIAN_POINT('Ctrl Pts',(-23.5543650456119,12.7787166878914,
10.5504779915376));
#207692=CARTESIAN_POINT('Ctrl Pts',(-23.4380194007037,14.1328954583448,
8.89653299890785));
#207693=CARTESIAN_POINT('Ctrl Pts',(-23.3216737557955,14.5549406016221,
6.80101254040771));
#207694=CARTESIAN_POINT('Ctrl Pts',(-23.2053281108873,13.9465338904122,
4.75181530147969));
#207695=CARTESIAN_POINT('Ctrl Pts',(-23.0889824659791,12.4493616386481,
3.22609858515552));
#207696=CARTESIAN_POINT('Ctrl Pts',(-22.9726368210709,10.4120207511136,
2.57910943638948));
#207697=CARTESIAN_POINT('Ctrl Pts',(-22.8562911761627,8.30889762767629,
2.96149802271777));
#207698=CARTESIAN_POINT('Ctrl Pts',(-22.7399455312545,6.62969119818919,
4.28422714343766));
#207699=CARTESIAN_POINT('Ctrl Pts',(-22.6235998863464,5.76539089851575,
6.23930573323043));
#207700=CARTESIAN_POINT('Ctrl Pts',(-22.5072542414381,5.91725275986458,
8.37151073316967));
#207701=CARTESIAN_POINT('Ctrl Pts',(-22.39090859653,7.04989684239228,10.1843605264167));
#207702=CARTESIAN_POINT('Ctrl Pts',(-22.2745629516218,8.89963591966034,
11.2557672312814));
#207703=CARTESIAN_POINT('Ctrl Pts',(-22.1582173067136,11.0356817137652,
11.3362121882554));
#207704=CARTESIAN_POINT('Ctrl Pts',(-22.0418716618054,12.9608532666381,
10.4070652370397));
#207705=CARTESIAN_POINT('Ctrl Pts',(-21.9255260168972,14.2265011041321,
8.68446129869154));
#207706=CARTESIAN_POINT('Ctrl Pts',(-21.809180371989,14.5387327015706,6.56993988513358));
#207707=CARTESIAN_POINT('Ctrl Pts',(-21.6928347270808,13.8231613497746,
4.554930012958));
#207708=CARTESIAN_POINT('Ctrl Pts',(-21.5764890821726,12.2499294503202,
3.11054775563703));
#207709=CARTESIAN_POINT('Ctrl Pts',(-21.4601434372644,10.1779814105543,
2.56906701769053));
#207710=CARTESIAN_POINT('Ctrl Pts',(-21.3437977923562,8.10518510954971,
3.06501610831153));
#207711=CARTESIAN_POINT('Ctrl Pts',(-21.1886702658119,5.94152731610683,
4.93282201196367));
#207712=CARTESIAN_POINT('Ctrl Pts',(-20.9947608576316,5.462195128413,8.78572589325462));
#207713=CARTESIAN_POINT('Ctrl Pts',(-20.7620695678152,9.00334225116017,
11.868708294292));
#207714=CARTESIAN_POINT('Ctrl Pts',(-20.5681601596349,12.7535662242368,
10.8634979598904));
#207715=CARTESIAN_POINT('Ctrl Pts',(-20.4130326330907,14.3057080785598,
8.46329596736919));
#207716=CARTESIAN_POINT('Ctrl Pts',(-20.2966869881824,14.5115655989794,
6.34195849133365));
#207717=CARTESIAN_POINT('Ctrl Pts',(-20.1803413432743,13.6899888172062,
4.3642877248237));
#207718=CARTESIAN_POINT('Ctrl Pts',(-20.063995698366,12.0427682001893,3.00488971334995));
#207719=CARTESIAN_POINT('Ctrl Pts',(-19.9476500534579,9.94843074126549,
2.57354559014325));
#207720=CARTESIAN_POINT('Ctrl Pts',(-19.8313044085497,7.89703048231626,
3.17391743859823));
#207721=CARTESIAN_POINT('Ctrl Pts',(-19.7149587636415,6.36507581983199,
4.66467016425681));
#207722=CARTESIAN_POINT('Ctrl Pts',(-19.5986131187333,5.7098214835323,6.69942845941255));
#207723=CARTESIAN_POINT('Ctrl Pts',(-19.4822674738251,6.08357717445482,
8.80405899922673));
#207724=CARTESIAN_POINT('Ctrl Pts',(-19.3659218289169,7.39944152554934,
10.4886800221041));
#207725=CARTESIAN_POINT('Ctrl Pts',(-19.2495761840087,9.35096377392451,
11.36095744624));
#207726=CARTESIAN_POINT('Ctrl Pts',(-19.1332305391005,11.4837725699839,
11.2178252480802));
#207727=CARTESIAN_POINT('Ctrl Pts',(-19.0168848941923,13.3012430781199,
10.0925927155175));
#207728=CARTESIAN_POINT('Ctrl Pts',(-18.9005392492841,14.3801946297058,
8.2472715757259));
#207729=CARTESIAN_POINT('Ctrl Pts',(-18.7841936043759,14.4693978080423,
6.11153032354543));
#207730=CARTESIAN_POINT('Ctrl Pts',(-18.6678479594677,13.5480817862055,
4.18266287383621));
#207731=CARTESIAN_POINT('Ctrl Pts',(-18.5515023145595,11.8307725960754,
2.90979783958556));
#207732=CARTESIAN_POINT('Ctrl Pts',(-18.4351566696513,9.71732703753046,
2.58930459263287));
#207733=CARTESIAN_POINT('Ctrl Pts',(-18.3188110247431,7.69986520819653,
3.29582838001529));
#207734=CARTESIAN_POINT('Ctrl Pts',(-18.2024653798349,6.24810405612113,
4.86481650562875));
#207735=CARTESIAN_POINT('Ctrl Pts',(-18.0861197349267,5.70015384269742,
6.93102969753986));
#207736=CARTESIAN_POINT('Ctrl Pts',(-17.9697740900186,6.18344102745076,
9.01317247113341));
#207737=CARTESIAN_POINT('Ctrl Pts',(-17.8534245640082,7.58581995767219,
10.6268679354101));
#207738=CARTESIAN_POINT('Ctrl Pts',(-17.775856919634,8.91532515555641,11.1390744673883));
#207739=CARTESIAN_POINT('Ctrl Pts',(-17.7370711568959,9.60171263502375,
11.2248210450709));
#207740=CARTESIAN_POINT('Ctrl Pts',(-17.734,9.60084442449481,11.2300936493755));
#207741=CARTESIAN_POINT('Ctrl Pts',(-17.734,9.47184184893842,11.2265276083404));
#207742=CARTESIAN_POINT('Ctrl Pts',(-17.734,9.34319367231557,11.2169788959015));
#207743=CARTESIAN_POINT('Ctrl Pts',(-17.734,9.21527281511507,11.2016549822556));
#207744=CARTESIAN_POINT('Ctrl Pts',(-17.734,9.0850114707997,11.1860506966421));
#207745=CARTESIAN_POINT('Ctrl Pts',(-17.734,8.95550358620178,11.1644579949205));
#207746=CARTESIAN_POINT('Ctrl Pts',(-17.7339999999999,8.82713205802554,
11.137043167845));
#207747=CARTESIAN_POINT('Ctrl Pts',(-17.7339999999999,8.77054626711207,
11.1249587929462));
#207748=CARTESIAN_POINT('Ctrl Pts',(-17.734,8.71418119819127,11.1117424824689));
#207749=CARTESIAN_POINT('Ctrl Pts',(-17.7339999999999,8.65806956321802,
11.0974052780753));
#207750=CARTESIAN_POINT('Ctrl Pts',(-17.7339999999999,8.63585998151805,
11.0917304601435));
#207751=CARTESIAN_POINT('Ctrl Pts',(-17.734,8.61369010565667,11.0858800148832));
#207752=CARTESIAN_POINT('Ctrl Pts',(-17.734,8.59156197215374,11.0798545436473));
#207753=CARTESIAN_POINT('Ctrl Pts',(-17.734,8.56803675576561,11.073448647974));
#207754=CARTESIAN_POINT('Ctrl Pts',(-17.734,8.54456657927922,11.0668470333961));
#207755=CARTESIAN_POINT('Ctrl Pts',(-17.734,8.52115967302967,11.0600525704303));
#207756=CARTESIAN_POINT('Ctrl Pts',(-17.734,8.39238352917026,11.0226719473357));
#207757=CARTESIAN_POINT('Ctrl Pts',(-17.7339999999999,8.2654669075248,10.9794433217256));
#207758=CARTESIAN_POINT('Ctrl Pts',(-17.7339999999999,8.14080691439627,
10.9305498903925));
#207759=CARTESIAN_POINT('Ctrl Pts',(-17.7339999999999,8.04196929345981,
10.8917843625668));
#207760=CARTESIAN_POINT('Ctrl Pts',(-17.7339999999999,7.94454991934812,
10.8494567334459));
#207761=CARTESIAN_POINT('Ctrl Pts',(-17.7339999999999,7.84874780521351,
10.8036350740797));
#207762=CARTESIAN_POINT('Ctrl Pts',(-17.7339999999999,7.8007073644388,10.780657577885));
#207763=CARTESIAN_POINT('Ctrl Pts',(-17.734,7.75307363883164,10.7568011656462));
#207764=CARTESIAN_POINT('Ctrl Pts',(-17.734,7.70587215411362,10.7320725309682));
#207765=CARTESIAN_POINT('Ctrl Pts',(-17.734,7.6793174922842,10.7181606691847));
#207766=CARTESIAN_POINT('Ctrl Pts',(-17.734,7.65289964014865,10.7039727286759));
#207767=CARTESIAN_POINT('Ctrl Pts',(-17.734,7.6266232029969,10.6895097288812));
#207768=CARTESIAN_POINT('Ctrl Pts',(-17.734,7.60953423118557,10.6801036669266));
#207769=CARTESIAN_POINT('Ctrl Pts',(-17.734,7.59250626485928,10.6705818595696));
#207770=CARTESIAN_POINT('Ctrl Pts',(-17.734,7.57555065957241,10.660950526036));
#207771=CARTESIAN_POINT('Ctrl Pts',(-17.734,7.57223521227194,10.6590672444767));
#207772=CARTESIAN_POINT('Ctrl Pts',(-17.734,7.56892242572952,10.6571797172604));
#207773=CARTESIAN_POINT('Ctrl Pts',(-17.734,7.56561230852364,10.655287949029));
#207774=CARTESIAN_POINT('Ctrl Pts',(-17.734,7.4452780447926,10.5865155995581));
#207775=CARTESIAN_POINT('Ctrl Pts',(-17.734,7.32847088871135,10.5121436774441));
#207776=CARTESIAN_POINT('Ctrl Pts',(-17.734,7.21544353549545,10.4326038138175));
#207777=CARTESIAN_POINT('Ctrl Pts',(-17.734,7.10471415648963,10.3546810857788));
#207778=CARTESIAN_POINT('Ctrl Pts',(-17.734,6.9976118719238,10.2717977527096));
#207779=CARTESIAN_POINT('Ctrl Pts',(-17.734,6.89438670712407,10.1843052779667));
#207780=CARTESIAN_POINT('Ctrl Pts',(-17.734,6.78794818419838,10.0940891974518));
#207781=CARTESIAN_POINT('Ctrl Pts',(-17.734,6.6856311233395,9.99897228946867));
#207782=CARTESIAN_POINT('Ctrl Pts',(-17.734,6.58773359226503,9.89928785076239));
#207783=CARTESIAN_POINT('Ctrl Pts',(-17.734,6.48983606119057,9.79960341205611));
#207784=CARTESIAN_POINT('Ctrl Pts',(-17.734,6.39635732386311,9.69535089177202));
#207785=CARTESIAN_POINT('Ctrl Pts',(-17.734,6.30763052920929,9.58681889811916));
#207786=CARTESIAN_POINT('Ctrl Pts',(-17.734,6.29613696047738,9.57275978628571));
#207787=CARTESIAN_POINT('Ctrl Pts',(-17.734,6.2847217875374,9.55862705010366));
#207788=CARTESIAN_POINT('Ctrl Pts',(-17.734,6.27339033844863,9.54442698291116));
#207789=CARTESIAN_POINT('Ctrl Pts',(-17.734,6.18608899588886,9.43502482960916));
#207790=CARTESIAN_POINT('Ctrl Pts',(-17.734,6.10395851094937,9.32188720168948));
#207791=CARTESIAN_POINT('Ctrl Pts',(-17.734,6.02725312841166,9.20538411899327));
#207792=CARTESIAN_POINT('Ctrl Pts',(-17.734,6.00879365458167,9.17734716076432));
#207793=CARTESIAN_POINT('Ctrl Pts',(-17.734,5.99064847657934,9.14911508036603));
#207794=CARTESIAN_POINT('Ctrl Pts',(-17.734,5.97282135213961,9.12069264219457));
#207795=CARTESIAN_POINT('Ctrl Pts',(-17.734,5.89932193605749,9.00350982809041));
#207796=CARTESIAN_POINT('Ctrl Pts',(-17.734,5.83122601110488,8.88309435288582));
#207797=CARTESIAN_POINT('Ctrl Pts',(-17.734,5.76858202624982,8.75987299061834));
#207798=CARTESIAN_POINT('Ctrl Pts',(-17.734,5.70371974075208,8.63228820817982));
#207799=CARTESIAN_POINT('Ctrl Pts',(-17.734,5.64470175837658,8.5016947685322));
#207800=CARTESIAN_POINT('Ctrl Pts',(-17.734,5.59162577020732,8.36852853807731));
#207801=CARTESIAN_POINT('Ctrl Pts',(-17.734,5.53854978203807,8.23536230762243));
#207802=CARTESIAN_POINT('Ctrl Pts',(-17.734,5.49141540954945,8.099622483443));
#207803=CARTESIAN_POINT('Ctrl Pts',(-17.734,5.45037050417322,7.96171819969766));
#207804=CARTESIAN_POINT('Ctrl Pts',(-17.734,5.44370883977346,7.93933607823385));
#207805=CARTESIAN_POINT('Ctrl Pts',(-17.734,5.43720810246527,7.91689789292579));
#207806=CARTESIAN_POINT('Ctrl Pts',(-17.734,5.43087453784511,7.89442611014828));
#207807=CARTESIAN_POINT('Ctrl Pts',(-17.734,5.39210005999986,7.75685245365212));
#207808=CARTESIAN_POINT('Ctrl Pts',(-17.734,5.35952760979182,7.61782263160567));
#207809=CARTESIAN_POINT('Ctrl Pts',(-17.734,5.33320157527804,7.47778296865981));
#207810=CARTESIAN_POINT('Ctrl Pts',(-17.734,5.30659247765412,7.33623756953797));
#207811=CARTESIAN_POINT('Ctrl Pts',(-17.734,5.28636445802549,7.19365980491143));
#207812=CARTESIAN_POINT('Ctrl Pts',(-17.734,5.27260711226952,7.05048093602787));
#207813=CARTESIAN_POINT('Ctrl Pts',(-17.734,5.2685667290597,7.00843085543087));
#207814=CARTESIAN_POINT('Ctrl Pts',(-17.734,5.26508476885768,6.96632877290582));
#207815=CARTESIAN_POINT('Ctrl Pts',(-17.734,5.26216428318298,6.92418527139126));
#207816=CARTESIAN_POINT('Ctrl Pts',(-17.734,5.25225669184947,6.78121569821777));
#207817=CARTESIAN_POINT('Ctrl Pts',(-17.734,5.24880693790303,6.63777018725341));
#207818=CARTESIAN_POINT('Ctrl Pts',(-17.734,5.25169843615224,6.49425035729583));
#207819=CARTESIAN_POINT('Ctrl Pts',(-17.734,5.25418827323925,6.37066702279185));
#207820=CARTESIAN_POINT('Ctrl Pts',(-17.734,5.26138083595832,6.24702806280391));
#207821=CARTESIAN_POINT('Ctrl Pts',(-17.734,5.27323254549849,6.12358757186399));
#207822=CARTESIAN_POINT('Ctrl Pts',(-17.734,5.27508188116906,6.10432597063131));
#207823=CARTESIAN_POINT('Ctrl Pts',(-17.734,5.27704501035193,6.08506650230671));
#207824=CARTESIAN_POINT('Ctrl Pts',(-17.734,5.27912085414996,6.06581909013264));
#207825=CARTESIAN_POINT('Ctrl Pts',(-17.734,5.29479715330723,5.92046702099761));
#207826=CARTESIAN_POINT('Ctrl Pts',(-17.734,5.31686509682758,5.77608379440672));
#207827=CARTESIAN_POINT('Ctrl Pts',(-17.734,5.34513749586769,5.63308999580947));
#207828=CARTESIAN_POINT('Ctrl Pts',(-17.734,5.37370011526018,5.48862834474738));
#207829=CARTESIAN_POINT('Ctrl Pts',(-17.734,5.40859521040085,5.34558404093898));
#207830=CARTESIAN_POINT('Ctrl Pts',(-17.734,5.44968220909514,5.20437948161231));
#207831=CARTESIAN_POINT('Ctrl Pts',(-17.734,5.49084209463958,5.06292443050275));
#207832=CARTESIAN_POINT('Ctrl Pts',(-17.734,5.53821592674961,4.9233148595374));
#207833=CARTESIAN_POINT('Ctrl Pts',(-17.734,5.59171431210286,4.78597586977869));
#207834=CARTESIAN_POINT('Ctrl Pts',(-17.734,5.62179155274454,4.70876273863118));
#207835=CARTESIAN_POINT('Ctrl Pts',(-17.734,5.65380556163705,4.63226736340509));
#207836=CARTESIAN_POINT('Ctrl Pts',(-17.734,5.68774754568469,4.55656680513933));
#207837=CARTESIAN_POINT('Ctrl Pts',(-17.734,5.73801817128877,4.44444859728045));
#207838=CARTESIAN_POINT('Ctrl Pts',(-17.734,5.7925169840286,4.3340732964859));
#207839=CARTESIAN_POINT('Ctrl Pts',(-17.734,5.85109760638757,4.22562345682714));
#207840=CARTESIAN_POINT('Ctrl Pts',(-23.534,5.20509380555676,8.32288496556915));
#207841=CARTESIAN_POINT('Ctrl Pts',(-23.534,5.25448034822735,8.46102114255294));
#207842=CARTESIAN_POINT('Ctrl Pts',(-23.534,5.30984160896073,8.59666377487398));
#207843=CARTESIAN_POINT('Ctrl Pts',(-23.534,5.37090550416418,8.72949042856166));
#207844=CARTESIAN_POINT('Ctrl Pts',(-23.534,5.43261983427359,8.86373191325075));
#207845=CARTESIAN_POINT('Ctrl Pts',(-23.534,5.50015936697075,8.99509777454297));
#207846=CARTESIAN_POINT('Ctrl Pts',(-23.534,5.57328932777325,9.12322955612724));
#207847=CARTESIAN_POINT('Ctrl Pts',(-23.534,5.64611803495858,9.25083350804698));
#207848=CARTESIAN_POINT('Ctrl Pts',(-23.534,5.72449172930617,9.37523055725192));
#207849=CARTESIAN_POINT('Ctrl Pts',(-23.534,5.80821663878109,9.49603209760072));
#207850=CARTESIAN_POINT('Ctrl Pts',(-23.534,5.89053472328053,9.61480381641726));
#207851=CARTESIAN_POINT('Ctrl Pts',(-23.534,5.97802623664759,9.73010029344401));
#207852=CARTESIAN_POINT('Ctrl Pts',(-23.534,6.07053600560125,9.84151116234556));
#207853=CARTESIAN_POINT('Ctrl Pts',(-23.534,6.09530240301151,9.8713376972753));
#207854=CARTESIAN_POINT('Ctrl Pts',(-23.534,6.1204286083341,9.90088549066091));
#207855=CARTESIAN_POINT('Ctrl Pts',(-23.534,6.14591193093455,9.93014609427624));
#207856=CARTESIAN_POINT('Ctrl Pts',(-23.534,6.15955451065975,9.94581085369119));
#207857=CARTESIAN_POINT('Ctrl Pts',(-23.534,6.1732994431912,9.9613932992639));
#207858=CARTESIAN_POINT('Ctrl Pts',(-23.534,6.18714632818517,9.97689210391278));
#207859=CARTESIAN_POINT('Ctrl Pts',(-23.534,6.19947043338816,9.99068646265098));
#207860=CARTESIAN_POINT('Ctrl Pts',(-23.534,6.21187374698249,10.0044127646295));
#207861=CARTESIAN_POINT('Ctrl Pts',(-23.534,6.2243484693293,10.0180621311511));
#207862=CARTESIAN_POINT('Ctrl Pts',(-23.534,6.32643586438779,10.1297622743404));
#207863=CARTESIAN_POINT('Ctrl Pts',(-23.534,6.43344023196213,10.2364692341204));
#207864=CARTESIAN_POINT('Ctrl Pts',(-23.534,6.54511720413425,10.3377902027729));
#207865=CARTESIAN_POINT('Ctrl Pts',(-23.5339999999999,6.65173379038045,
10.4345200440534));
#207866=CARTESIAN_POINT('Ctrl Pts',(-23.534,6.76261007331514,10.5263410649745));
#207867=CARTESIAN_POINT('Ctrl Pts',(-23.534,6.87736332873699,10.6130492088599));
#207868=CARTESIAN_POINT('Ctrl Pts',(-23.5339999999999,6.99147784435786,
10.6992747177004));
#207869=CARTESIAN_POINT('Ctrl Pts',(-23.5339999999999,7.10942705472184,
10.7804443794007));
#207870=CARTESIAN_POINT('Ctrl Pts',(-23.5339999999999,7.23085436779322,
10.8563105129933));
#207871=CARTESIAN_POINT('Ctrl Pts',(-23.5339999999999,7.33613170340885,
10.9220863603382));
#207872=CARTESIAN_POINT('Ctrl Pts',(-23.534,7.44402406928014,10.9838750073567));
#207873=CARTESIAN_POINT('Ctrl Pts',(-23.534,7.55430465571587,11.0414837770386));
#207874=CARTESIAN_POINT('Ctrl Pts',(-23.534,7.58853359014114,11.059364411006));
#207875=CARTESIAN_POINT('Ctrl Pts',(-23.5339999999999,7.62299261107083,
11.0768421517888));
#207876=CARTESIAN_POINT('Ctrl Pts',(-23.534,7.65767495108206,11.0939106313755));
#207877=CARTESIAN_POINT('Ctrl Pts',(-23.534,7.68146530654451,11.1056187570799));
#207878=CARTESIAN_POINT('Ctrl Pts',(-23.5339999999999,7.70536587584369,
11.1171366355578));
#207879=CARTESIAN_POINT('Ctrl Pts',(-23.5339999999999,7.72934494066839,
11.1284484864467));
#207880=CARTESIAN_POINT('Ctrl Pts',(-23.534,7.85661864731222,11.1884884088606));
#207881=CARTESIAN_POINT('Ctrl Pts',(-23.5339999999999,7.98623315832197,
11.2427954978079));
#207882=CARTESIAN_POINT('Ctrl Pts',(-23.534,8.11783022540222,11.2911803845138));
#207883=CARTESIAN_POINT('Ctrl Pts',(-23.534,8.2483999926991,11.3391875592788));
#207884=CARTESIAN_POINT('Ctrl Pts',(-23.534,8.38092221481638,11.3813648380392));
#207885=CARTESIAN_POINT('Ctrl Pts',(-23.534,8.51505911917084,11.4174776458748));
#207886=CARTESIAN_POINT('Ctrl Pts',(-23.534,8.54046938028188,11.4243186854901));
#207887=CARTESIAN_POINT('Ctrl Pts',(-23.534,8.56593760257076,11.430941947973));
#207888=CARTESIAN_POINT('Ctrl Pts',(-23.534,8.59146150656054,11.4373456266197));
#207889=CARTESIAN_POINT('Ctrl Pts',(-23.534,8.7269958712635,11.4713497710281));
#207890=CARTESIAN_POINT('Ctrl Pts',(-23.534,8.86410085374641,11.4991663722465));
#207891=CARTESIAN_POINT('Ctrl Pts',(-23.534,9.00234645392465,11.5207487445334));
#207892=CARTESIAN_POINT('Ctrl Pts',(-23.534,9.11948261257159,11.5390355918611));
#207893=CARTESIAN_POINT('Ctrl Pts',(-23.534,9.2374378836336,11.5528458391875));
#207894=CARTESIAN_POINT('Ctrl Pts',(-23.534,9.355943158363,11.5621227489501));
#207895=CARTESIAN_POINT('Ctrl Pts',(-23.534,9.38621145908859,11.5644922324617));
#207896=CARTESIAN_POINT('Ctrl Pts',(-23.5339999999999,9.41651558906432,
11.5665658392786));
#207897=CARTESIAN_POINT('Ctrl Pts',(-23.5339999999999,9.44685094557672,
11.5683423557483));
#207898=CARTESIAN_POINT('Ctrl Pts',(-23.5339999999999,9.46479541432074,
11.5693932299733));
#207899=CARTESIAN_POINT('Ctrl Pts',(-23.534,9.48274095025218,11.5703395658612));
#207900=CARTESIAN_POINT('Ctrl Pts',(-23.534,9.50068594451741,11.5711814160656));
#207901=CARTESIAN_POINT('Ctrl Pts',(-23.534,9.6376789645452,11.5776081443338));
#207902=CARTESIAN_POINT('Ctrl Pts',(-23.534,9.77465402965032,11.5779506548684));
#207903=CARTESIAN_POINT('Ctrl Pts',(-23.534,9.91120575942693,11.572220826072));
#207904=CARTESIAN_POINT('Ctrl Pts',(-23.534,10.0465379651817,11.5665421695593));
#207905=CARTESIAN_POINT('Ctrl Pts',(-23.534,10.1814551280495,11.5548989762848));
#207906=CARTESIAN_POINT('Ctrl Pts',(-23.5339999999999,10.3155540558513,
11.5372529906715));
#207907=CARTESIAN_POINT('Ctrl Pts',(-23.5339999999999,10.4488851811288,
11.5197080396639));
#207908=CARTESIAN_POINT('Ctrl Pts',(-23.534,10.5814081302335,11.4962287057346));
#207909=CARTESIAN_POINT('Ctrl Pts',(-23.5339999999999,10.7127070778146,
11.466730168397));
#207910=CARTESIAN_POINT('Ctrl Pts',(-23.5339999999999,10.7477535156779,
11.4588563912274));
#207911=CARTESIAN_POINT('Ctrl Pts',(-23.534,10.7827126062386,11.4505535095437));
#207912=CARTESIAN_POINT('Ctrl Pts',(-23.534,10.8175761048042,11.4418193551064));
#207913=CARTESIAN_POINT('Ctrl Pts',(-23.534,10.9043442667858,11.4200818199142));
#207914=CARTESIAN_POINT('Ctrl Pts',(-23.534,10.9905208003715,11.3956733994087));
#207915=CARTESIAN_POINT('Ctrl Pts',(-23.534,11.0759855672366,11.3686310737129));
#207916=CARTESIAN_POINT('Ctrl Pts',(-23.534,11.1080452454195,11.3584869138336));
#207917=CARTESIAN_POINT('Ctrl Pts',(-23.5339999999999,11.1400046970052,
11.3479720510328));
#207918=CARTESIAN_POINT('Ctrl Pts',(-23.534,11.1718573159444,11.3370881949364));
#207919=CARTESIAN_POINT('Ctrl Pts',(-23.534,11.1899003611931,11.3309229904864));
#207920=CARTESIAN_POINT('Ctrl Pts',(-23.5339999999999,11.2079056979589,
11.3246405183814));
#207921=CARTESIAN_POINT('Ctrl Pts',(-23.5339999999999,11.2258644852499,
11.3182440453307));
#207922=CARTESIAN_POINT('Ctrl Pts',(-23.5339999999999,11.3524381725536,
11.2731616482488));
#207923=CARTESIAN_POINT('Ctrl Pts',(-23.534,11.4768170268763,11.2223807678744));
#207924=CARTESIAN_POINT('Ctrl Pts',(-23.534,11.5986229667085,11.1660898819114));
#207925=CARTESIAN_POINT('Ctrl Pts',(-23.534,11.7193673208799,11.1102895926916));
#207926=CARTESIAN_POINT('Ctrl Pts',(-23.534,11.8375840317477,11.0490744065508));
#207927=CARTESIAN_POINT('Ctrl Pts',(-23.534,11.9528722695249,10.9825889536062));
#207928=CARTESIAN_POINT('Ctrl Pts',(-23.534,12.0079182811876,10.9508445268654));
#207929=CARTESIAN_POINT('Ctrl Pts',(-23.534,12.0622961454576,10.9178981000385));
#207930=CARTESIAN_POINT('Ctrl Pts',(-23.534,12.115958959572,10.8837627538526));
#207931=CARTESIAN_POINT('Ctrl Pts',(-23.534,12.1331643569177,10.8728182626933));
#207932=CARTESIAN_POINT('Ctrl Pts',(-23.534,12.150294211089,10.8617527782972));
#207933=CARTESIAN_POINT('Ctrl Pts',(-23.534,12.1673397958196,10.8505716388401));
#207934=CARTESIAN_POINT('Ctrl Pts',(-23.5339999999999,12.2766355142431,
10.7788785471058));
#207935=CARTESIAN_POINT('Ctrl Pts',(-23.534,12.3825568873876,10.7023781389818));
#207936=CARTESIAN_POINT('Ctrl Pts',(-23.534,12.4847306195173,10.6212230158632));
#207937=CARTESIAN_POINT('Ctrl Pts',(-23.534,12.5574317395047,10.5634775638721));
#207938=CARTESIAN_POINT('Ctrl Pts',(-23.534,12.6282347834106,10.503374641833));
#207939=CARTESIAN_POINT('Ctrl Pts',(-23.534,12.6969925515033,10.4409593113222));
#207940=CARTESIAN_POINT('Ctrl Pts',(-23.534,12.7737176242397,10.3713116059626));
#207941=CARTESIAN_POINT('Ctrl Pts',(-23.534,12.8478962945781,10.2987843938166));
#207942=CARTESIAN_POINT('Ctrl Pts',(-23.5339999999999,12.9193848394627,
10.2235362295063));
#207943=CARTESIAN_POINT('Ctrl Pts',(23.5309283172883,7.34300535603735,3.78082119416608));
#207944=CARTESIAN_POINT('Ctrl Pts',(23.4921425539738,7.86601024404076,3.32811163657506));
#207945=CARTESIAN_POINT('Ctrl Pts',(23.4145749090232,9.13626656589345,2.68283027075003));
#207946=CARTESIAN_POINT('Ctrl Pts',(23.2982253824366,11.2738498134804,2.72043220540736));
#207947=CARTESIAN_POINT('Ctrl Pts',(23.1818797375284,13.1445654280131,3.75450519529614));
#207948=CARTESIAN_POINT('Ctrl Pts',(23.0655340926202,14.3134104771639,5.54427759941156));
#207949=CARTESIAN_POINT('Ctrl Pts',(22.949188447712,14.5079780693299,7.67300394796904));
#207950=CARTESIAN_POINT('Ctrl Pts',(22.8328428028038,13.6830822571742,9.64502652688917));
#207951=CARTESIAN_POINT('Ctrl Pts',(22.7164971578956,12.0307386115573,11.0011705393577));
#207952=CARTESIAN_POINT('Ctrl Pts',(22.6001515129874,9.93571184213651,11.4256669327143));
#207953=CARTESIAN_POINT('Ctrl Pts',(22.4838058680792,7.88580366311466,10.8196740498626));
#207954=CARTESIAN_POINT('Ctrl Pts',(22.367460223171,6.35832750127234,9.32429364407502));
#207955=CARTESIAN_POINT('Ctrl Pts',(22.2511145782628,5.70894628402538,7.28771595678545));
#207956=CARTESIAN_POINT('Ctrl Pts',(22.1347689333546,6.08886062127945,5.18414506891689));
#207957=CARTESIAN_POINT('Ctrl Pts',(22.0184232884464,7.40962001767397,3.50338546661371));
#207958=CARTESIAN_POINT('Ctrl Pts',(21.9020776435382,9.36367135867349,2.63678951113586));
#207959=CARTESIAN_POINT('Ctrl Pts',(21.78573199863,11.4960733546058,2.78614318046246));
#207960=CARTESIAN_POINT('Ctrl Pts',(21.6693863537218,13.3102097615393,3.91666104806278));
#207961=CARTESIAN_POINT('Ctrl Pts',(21.5530407088136,14.3838786712727,5.76512857483606));
#207962=CARTESIAN_POINT('Ctrl Pts',(21.4366950639055,14.4666465134933,7.90110058902803));
#207963=CARTESIAN_POINT('Ctrl Pts',(21.3203494189972,13.5401544226926,9.82731484321649));
#207964=CARTESIAN_POINT('Ctrl Pts',(21.2040037740891,11.818219849542,11.0950850634552));
#207965=CARTESIAN_POINT('Ctrl Pts',(21.0876581291808,9.70578223018301,11.4095937069531));
#207966=CARTESIAN_POINT('Ctrl Pts',(20.9713124842727,7.68634952883146,10.6968241722325));
#207967=CARTESIAN_POINT('Ctrl Pts',(20.8549668393645,6.24762631375591,9.12439123907643));
#207968=CARTESIAN_POINT('Ctrl Pts',(20.6998393128202,5.50252433774221,6.36487623709474));
#207969=CARTESIAN_POINT('Ctrl Pts',(20.5059299046399,7.26489001546572,2.90530097391561));
#207970=CARTESIAN_POINT('Ctrl Pts',(20.2732386148235,11.9254850147715,2.33663337229139));
#207971=CARTESIAN_POINT('Ctrl Pts',(20.0793292066432,14.4680075562826,5.27094298607233));
#207972=CARTESIAN_POINT('Ctrl Pts',(19.9242016800989,14.4082980438857,8.12865794298295));
#207973=CARTESIAN_POINT('Ctrl Pts',(19.8078560351907,13.3898808093813,10.0009015583641));
#207974=CARTESIAN_POINT('Ctrl Pts',(19.6915103902825,11.6010834707722,11.1783364509586));
#207975=CARTESIAN_POINT('Ctrl Pts',(19.5751647453743,9.47499843604004,11.3809957897657));
#207976=CARTESIAN_POINT('Ctrl Pts',(19.4588191004661,7.49874546760186,10.5644639714789));
#207977=CARTESIAN_POINT('Ctrl Pts',(19.3424734555579,6.1362730321213,8.91754023010204));
#207978=CARTESIAN_POINT('Ctrl Pts',(19.2261278106497,5.70301304802592,6.82433389834715));
#207979=CARTESIAN_POINT('Ctrl Pts',(19.1097821657415,6.3007131588549,4.77193245058443));
#207980=CARTESIAN_POINT('Ctrl Pts',(18.9934365208334,7.78978883331376,3.23836954425806));
#207981=CARTESIAN_POINT('Ctrl Pts',(18.8770908759252,9.82371572424119,2.58065669417856));
#207982=CARTESIAN_POINT('Ctrl Pts',(18.760745231017,11.9288120776716,2.95197129944819));
#207983=CARTESIAN_POINT('Ctrl Pts',(18.6443995861088,13.6149642392687,4.26583929580108));
#207984=CARTESIAN_POINT('Ctrl Pts',(18.5280539412006,14.4895408169203,6.21634210117263));
#207985=CARTESIAN_POINT('Ctrl Pts',(18.4117082962924,14.3489117283966,8.34931376088588));
#207986=CARTESIAN_POINT('Ctrl Pts',(18.2953626513842,13.225818013417,10.1681063522451));
#207987=CARTESIAN_POINT('Ctrl Pts',(18.179017006476,11.3817646217731,11.2492252195552));
#207988=CARTESIAN_POINT('Ctrl Pts',(18.0626713615678,9.24613280585004,11.3409372655453));
#207989=CARTESIAN_POINT('Ctrl Pts',(17.9463257166596,7.31617934650269,10.421891156518));
#207990=CARTESIAN_POINT('Ctrl Pts',(17.8299800717514,6.04130773120048,8.70607399924876));
#207991=CARTESIAN_POINT('Ctrl Pts',(17.7136344268432,5.71830963515471,6.59301823923793));
#207992=CARTESIAN_POINT('Ctrl Pts',(17.597288781935,6.42250688754369,4.57470452794694));
#207993=CARTESIAN_POINT('Ctrl Pts',(17.4809431370268,7.9896921867418,3.1211522939865));
#207994=CARTESIAN_POINT('Ctrl Pts',(17.3645974921186,10.0554503632162,2.57068500932872));
#207995=CARTESIAN_POINT('Ctrl Pts',(17.2870337288465,11.4435279727104,2.89154782505743));
#207996=CARTESIAN_POINT('Ctrl Pts',(17.2482518472104,12.0599972964235,3.20515550067288));
#207997=CARTESIAN_POINT('Ctrl Pts',(23.6935169503155,7.15869994272444,3.56789701660741));
#207998=CARTESIAN_POINT('Ctrl Pts',(23.654731187001,7.71629762359647,3.08524416725256));
#207999=CARTESIAN_POINT('Ctrl Pts',(23.5771635420504,9.07057173350399,2.39728235016981));
#208000=CARTESIAN_POINT('Ctrl Pts',(23.4608140154638,11.3495398442526,2.43737136662486));
#208001=CARTESIAN_POINT('Ctrl Pts',(23.3444683705557,13.3439890590901,3.53984041469738));
#208002=CARTESIAN_POINT('Ctrl Pts',(23.2281227256474,14.5901443124249,5.44799264178905));
#208003=CARTESIAN_POINT('Ctrl Pts',(23.1117770807393,14.7975810700024,7.71751803704522));
#208004=CARTESIAN_POINT('Ctrl Pts',(22.9954314358311,13.9181246779694,9.81997490093976));
#208005=CARTESIAN_POINT('Ctrl Pts',(22.8790857909229,12.1564910758115,11.2658175185254));
#208006=CARTESIAN_POINT('Ctrl Pts',(22.7627401460147,9.92289423037199,11.7183911175558));
#208007=CARTESIAN_POINT('Ctrl Pts',(22.6463945011065,7.73740022669883,11.0723164175793));
#208008=CARTESIAN_POINT('Ctrl Pts',(22.5300488561983,6.10889314202882,9.47802797895342));
#208009=CARTESIAN_POINT('Ctrl Pts',(22.4137032112901,5.41656029955566,7.30674617758523));
#208010=CARTESIAN_POINT('Ctrl Pts',(22.2973575663819,5.82160307877634,5.06404008528999));
#208011=CARTESIAN_POINT('Ctrl Pts',(22.1810119214737,7.22972065723908,3.2721110271785));
#208012=CARTESIAN_POINT('Ctrl Pts',(22.0646662765655,9.3130176225996,2.34819634471306));
#208013=CARTESIAN_POINT('Ctrl Pts',(21.9483206316573,11.5864617813299,2.50742862256836));
#208014=CARTESIAN_POINT('Ctrl Pts',(21.8319749867491,13.5205895045972,3.71272164299274));
#208015=CARTESIAN_POINT('Ctrl Pts',(21.7156293418409,14.6652734412564,5.68345122839067));
#208016=CARTESIAN_POINT('Ctrl Pts',(21.5992836969327,14.7535157463124,7.96070153491793));
#208017=CARTESIAN_POINT('Ctrl Pts',(21.4829380520245,13.7657432550285,10.0143202020366));
#208018=CARTESIAN_POINT('Ctrl Pts',(21.3665924071164,11.9299158151215,11.3659437736297));
#208019=CARTESIAN_POINT('Ctrl Pts',(21.2502467622081,9.67775652453044,11.7012547702403));
#208020=CARTESIAN_POINT('Ctrl Pts',(21.1339011172999,7.52475371943345,10.9413409555267));
#208021=CARTESIAN_POINT('Ctrl Pts',(21.0175554723918,5.99086991348007,9.26490355127649));
#208022=CARTESIAN_POINT('Ctrl Pts',(20.8624279458475,5.19648511255694,6.32286763396294));
#208023=CARTESIAN_POINT('Ctrl Pts',(20.6685185376672,7.07541786689233,2.63446779717522));
#208024=CARTESIAN_POINT('Ctrl Pts',(20.4358272478508,12.0442757546598,2.02818716170503));
#208025=CARTESIAN_POINT('Ctrl Pts',(20.2419178396704,14.7549668117235,5.1565790240658));
#208026=CARTESIAN_POINT('Ctrl Pts',(20.0867903131262,14.6913079695174,8.20331007594904));
#208027=CARTESIAN_POINT('Ctrl Pts',(19.970444668218,13.6055301858954,10.1993883572618));
#208028=CARTESIAN_POINT('Ctrl Pts',(19.8540990233098,11.6984175174723,11.4547016068087));
#208029=CARTESIAN_POINT('Ctrl Pts',(19.7377533784016,9.43170813884858,11.6707653184832));
#208030=CARTESIAN_POINT('Ctrl Pts',(19.6214077334934,7.32474107736591,10.8002261348571));
#208031=CARTESIAN_POINT('Ctrl Pts',(19.5050620885852,5.87215145975016,9.04437092235506));
#208032=CARTESIAN_POINT('Ctrl Pts',(19.388716443677,5.41023462515135,6.81271492267807));
#208033=CARTESIAN_POINT('Ctrl Pts',(19.2723707987688,6.04746804935031,4.62456273951254));
#208034=CARTESIAN_POINT('Ctrl Pts',(19.1560251538606,7.63503474665393,2.98956631853571));
#208035=CARTESIAN_POINT('Ctrl Pts',(19.0396795089524,9.80349042165522,2.28835076912831));
#208036=CARTESIAN_POINT('Ctrl Pts',(18.9233338640442,12.0478228774492,2.68422500954442));
#208037=CARTESIAN_POINT('Ctrl Pts',(18.806988219136,13.8455011716103,4.08499537430166));
#208038=CARTESIAN_POINT('Ctrl Pts',(18.6906425742278,14.7779243336677,6.16450909540956));
#208039=CARTESIAN_POINT('Ctrl Pts',(18.5742969293197,14.6279937012347,8.43856059684434));
#208040=CARTESIAN_POINT('Ctrl Pts',(18.4579512844115,13.4306158846232,10.3776524756999));
#208041=CARTESIAN_POINT('Ctrl Pts',(18.3416056395033,11.4645923957984,11.5302791279295));
#208042=CARTESIAN_POINT('Ctrl Pts',(18.2252599945951,9.18770478906643,11.628057227762));
#208043=CARTESIAN_POINT('Ctrl Pts',(18.1089143496868,7.13009959682579,10.6482232132763));
#208044=CARTESIAN_POINT('Ctrl Pts',(17.9925687047787,5.77090492693302,8.81891780975284));
#208045=CARTESIAN_POINT('Ctrl Pts',(17.8762230598705,5.42654296509983,6.56609949321034));
#208046=CARTESIAN_POINT('Ctrl Pts',(17.7598774149623,6.17731750624712,4.41428969085003));
#208047=CARTESIAN_POINT('Ctrl Pts',(17.6435317700541,7.84816018549169,2.86459603927288));
#208048=CARTESIAN_POINT('Ctrl Pts',(17.5271861251459,10.0505525433181,2.27771953321792));
#208049=CARTESIAN_POINT('Ctrl Pts',(17.4496223618738,11.5304409223333,2.61980498219221));
#208050=CARTESIAN_POINT('Ctrl Pts',(17.4108404802377,12.1876850000003,2.954155418752));
#208051=CARTESIAN_POINT('Ctrl Pts',(23.8561055833427,6.97439452941152,3.35497283904874));
#208052=CARTESIAN_POINT('Ctrl Pts',(23.8173198200282,7.56658500315218,2.84237669793006));
#208053=CARTESIAN_POINT('Ctrl Pts',(23.7397521750777,9.00487690111454,2.11173442958961));
#208054=CARTESIAN_POINT('Ctrl Pts',(23.6234026484911,11.4252298750248,2.15431052784236));
#208055=CARTESIAN_POINT('Ctrl Pts',(23.5070570035829,13.543412690167,3.32517563409861));
#208056=CARTESIAN_POINT('Ctrl Pts',(23.3907113586747,14.8668781476858,5.35170768416653));
#208057=CARTESIAN_POINT('Ctrl Pts',(23.2743657137665,15.0871840706748,7.7620321261214));
#208058=CARTESIAN_POINT('Ctrl Pts',(23.1580200688583,14.1531670987647,9.99492327499034));
#208059=CARTESIAN_POINT('Ctrl Pts',(23.0416744239502,12.2822435400657,11.5304644976931));
#208060=CARTESIAN_POINT('Ctrl Pts',(22.925328779042,9.91007661860751,12.0111153023973));
#208061=CARTESIAN_POINT('Ctrl Pts',(22.8089831341337,7.58899679028301,11.324958785296));
#208062=CARTESIAN_POINT('Ctrl Pts',(22.6926374892256,5.85945878278532,9.63176231383182));
#208063=CARTESIAN_POINT('Ctrl Pts',(22.5762918443174,5.12417431508593,7.32577639838504));
#208064=CARTESIAN_POINT('Ctrl Pts',(22.4599461994092,5.55434553627324,4.94393510166309));
#208065=CARTESIAN_POINT('Ctrl Pts',(22.343600554501,7.04982129680419,3.04083658774328));
#208066=CARTESIAN_POINT('Ctrl Pts',(22.2272549095928,9.26236388652573,2.05960317829026));
#208067=CARTESIAN_POINT('Ctrl Pts',(22.1109092646846,11.6768502080541,2.22871406467427));
#208068=CARTESIAN_POINT('Ctrl Pts',(21.9945636197764,13.730969247655,3.50878223792271));
#208069=CARTESIAN_POINT('Ctrl Pts',(21.8782179748682,14.9466682112401,5.60177388194529));
#208070=CARTESIAN_POINT('Ctrl Pts',(21.76187232996,15.0403849791315,8.02030248080784));
#208071=CARTESIAN_POINT('Ctrl Pts',(21.6455266850518,13.9913320873644,10.2013255608568));
#208072=CARTESIAN_POINT('Ctrl Pts',(21.5291810401436,12.041611780701,11.6368024838041));
#208073=CARTESIAN_POINT('Ctrl Pts',(21.4128353952354,9.64973081887787,11.9929158335273));
#208074=CARTESIAN_POINT('Ctrl Pts',(21.2964897503273,7.36315791003544,11.185857738821));
#208075=CARTESIAN_POINT('Ctrl Pts',(21.180144105419,5.73411351320423,9.40541586347656));
#208076=CARTESIAN_POINT('Ctrl Pts',(21.0250165788748,4.89044588737168,6.28085903083115));
#208077=CARTESIAN_POINT('Ctrl Pts',(20.8311071706945,6.88594571831891,2.36363462043484));
#208078=CARTESIAN_POINT('Ctrl Pts',(20.598415880878,12.1630664945482,1.71974095111867));
#208079=CARTESIAN_POINT('Ctrl Pts',(20.4045064726977,15.0419260671645,5.04221506205927));
#208080=CARTESIAN_POINT('Ctrl Pts',(20.2493789461535,14.9743178951491,8.27796220891513));
#208081=CARTESIAN_POINT('Ctrl Pts',(20.1330333012453,13.8211795624095,10.3978751561594));
#208082=CARTESIAN_POINT('Ctrl Pts',(20.0166876563371,11.7957515641725,11.7310667626589));
#208083=CARTESIAN_POINT('Ctrl Pts',(19.9003420114289,9.3884178416571,11.9605348472007));
#208084=CARTESIAN_POINT('Ctrl Pts',(19.7839963665207,7.15073668712996,11.0359882982353));
#208085=CARTESIAN_POINT('Ctrl Pts',(19.6676507216125,5.60802988737902,9.17120161460807));
#208086=CARTESIAN_POINT('Ctrl Pts',(19.5513050767043,5.11745620227678,6.80109594700901));
#208087=CARTESIAN_POINT('Ctrl Pts',(19.4349594317961,5.79422293984571,4.47719302844065));
#208088=CARTESIAN_POINT('Ctrl Pts',(19.3186137868879,7.4802806599941,2.74076309281336));
#208089=CARTESIAN_POINT('Ctrl Pts',(19.2022681419797,9.78326511906926,1.99604484407805));
#208090=CARTESIAN_POINT('Ctrl Pts',(19.0859224970715,12.1668336772269,2.41647871964064));
#208091=CARTESIAN_POINT('Ctrl Pts',(18.9695768521633,14.0760381039521,3.90415145280225));
#208092=CARTESIAN_POINT('Ctrl Pts',(18.8532312072551,15.0663078504151,6.11267608964647));
#208093=CARTESIAN_POINT('Ctrl Pts',(18.7368855623469,14.9070756740727,8.52780743280282));
#208094=CARTESIAN_POINT('Ctrl Pts',(18.6205399174387,13.6354137558295,10.5871985991546));
#208095=CARTESIAN_POINT('Ctrl Pts',(18.5041942725306,11.5474201698238,11.8113330363039));
#208096=CARTESIAN_POINT('Ctrl Pts',(18.3878486276223,9.12927677228282,11.9151771899788));
#208097=CARTESIAN_POINT('Ctrl Pts',(18.2715029827142,6.94401984714889,10.8745552700345));
#208098=CARTESIAN_POINT('Ctrl Pts',(18.155157337806,5.50050212266556,8.93176162025691));
#208099=CARTESIAN_POINT('Ctrl Pts',(18.0388116928978,5.13477629504494,6.53918074718275));
#208100=CARTESIAN_POINT('Ctrl Pts',(17.9224660479896,5.93212812495056,4.25387485375313));
#208101=CARTESIAN_POINT('Ctrl Pts',(17.8061204030814,7.70662818424157,2.60803978455923));
#208102=CARTESIAN_POINT('Ctrl Pts',(17.6897747581732,10.0456547234199,1.9847540571071));
#208103=CARTESIAN_POINT('Ctrl Pts',(17.612210994901,11.6173538719561,2.34806213932699));
#208104=CARTESIAN_POINT('Ctrl Pts',(17.573429113265,12.3153727035772,2.70315533683113));
#208105=CARTESIAN_POINT('Ctrl Pts',(24.01869421637,6.79008911609861,3.14204866149007));
#208106=CARTESIAN_POINT('Ctrl Pts',(23.9799084530555,7.4168723827079,2.59950922860756));
#208107=CARTESIAN_POINT('Ctrl Pts',(23.902340808105,8.93918206872512,1.8261865090094));
#208108=CARTESIAN_POINT('Ctrl Pts',(23.7859912815184,11.500919905797,1.87124968905985));
#208109=CARTESIAN_POINT('Ctrl Pts',(23.6696456366102,13.7428363212439,3.11051085349985));
#208110=CARTESIAN_POINT('Ctrl Pts',(23.553299991702,15.1436119829468,5.25542272654401));
#208111=CARTESIAN_POINT('Ctrl Pts',(23.4369543467938,15.3767870713474,7.80654621519758));
#208112=CARTESIAN_POINT('Ctrl Pts',(23.3206087018856,14.3882095195599,10.169871649041));
#208113=CARTESIAN_POINT('Ctrl Pts',(23.2042630569774,12.40799600432,11.7951114768609));
#208114=CARTESIAN_POINT('Ctrl Pts',(23.0879174120693,9.89725900684299,12.3038394872388));
#208115=CARTESIAN_POINT('Ctrl Pts',(22.971571767161,7.4405933538672,11.5776011530127));
#208116=CARTESIAN_POINT('Ctrl Pts',(22.8552261222528,5.6100244235418,9.78549664871022));
#208117=CARTESIAN_POINT('Ctrl Pts',(22.7388804773446,4.83178833061622,7.34480661918484));
#208118=CARTESIAN_POINT('Ctrl Pts',(22.6225348324365,5.28708799377012,4.82383011803619));
#208119=CARTESIAN_POINT('Ctrl Pts',(22.5061891875283,6.86992193636931,2.80956214830806));
#208120=CARTESIAN_POINT('Ctrl Pts',(22.38984354262,9.21171015045184,1.77101001186746));
#208121=CARTESIAN_POINT('Ctrl Pts',(22.2734978977119,11.7672386347782,1.94999950678018));
#208122=CARTESIAN_POINT('Ctrl Pts',(22.1571522528037,13.9413489907128,3.30484283285267));
#208123=CARTESIAN_POINT('Ctrl Pts',(22.0408066078955,15.2280629812237,5.52009653549991));
#208124=CARTESIAN_POINT('Ctrl Pts',(21.9244609629873,15.3272542119506,8.07990342669773));
#208125=CARTESIAN_POINT('Ctrl Pts',(21.8081153180791,14.2169209197003,10.3883309196771));
#208126=CARTESIAN_POINT('Ctrl Pts',(21.6917696731709,12.1533077462805,11.9076611939785));
#208127=CARTESIAN_POINT('Ctrl Pts',(21.5754240282627,9.62170511322531,12.2845768968145));
#208128=CARTESIAN_POINT('Ctrl Pts',(21.4590783833545,7.20156210063743,11.4303745221154));
#208129=CARTESIAN_POINT('Ctrl Pts',(21.3427327384463,5.4773571129284,9.54592817567664));
#208130=CARTESIAN_POINT('Ctrl Pts',(21.187605211902,4.58440666218642,6.23885042769937));
#208131=CARTESIAN_POINT('Ctrl Pts',(20.9936958037217,6.69647356974549,2.09280144369445));
#208132=CARTESIAN_POINT('Ctrl Pts',(20.7610045139053,12.2818572344366,1.41129474053231));
#208133=CARTESIAN_POINT('Ctrl Pts',(20.567095105725,15.3288853226055,4.92785110005275));
#208134=CARTESIAN_POINT('Ctrl Pts',(20.4119675791808,15.2573278207807,8.3526143418812));
#208135=CARTESIAN_POINT('Ctrl Pts',(20.2956219342725,14.0368289389236,10.5963619550571));
#208136=CARTESIAN_POINT('Ctrl Pts',(20.1792762893644,11.8930856108726,12.007431918509));
#208137=CARTESIAN_POINT('Ctrl Pts',(20.0629306444561,9.34512754446563,12.2503043759182));
#208138=CARTESIAN_POINT('Ctrl Pts',(19.946584999548,6.97673229689402,11.2717504616136));
#208139=CARTESIAN_POINT('Ctrl Pts',(19.8302393546397,5.34390831500789,9.29803230686109));
#208140=CARTESIAN_POINT('Ctrl Pts',(19.7138937097316,4.82467777940222,6.78947697133994));
#208141=CARTESIAN_POINT('Ctrl Pts',(19.5975480648234,5.54097783034111,4.32982331736877));
#208142=CARTESIAN_POINT('Ctrl Pts',(19.4812024199152,7.32552657333427,2.49195986709101));
#208143=CARTESIAN_POINT('Ctrl Pts',(19.364856775007,9.7630398164833,1.7037389190278));
#208144=CARTESIAN_POINT('Ctrl Pts',(19.2485111300988,12.2858444770046,2.14873242973686));
#208145=CARTESIAN_POINT('Ctrl Pts',(19.1321654851906,14.3065750362938,3.72330753130284));
#208146=CARTESIAN_POINT('Ctrl Pts',(19.0158198402824,15.3546913671625,6.06084308388339));
#208147=CARTESIAN_POINT('Ctrl Pts',(18.8994741953742,15.1861576469106,8.61705426876128));
#208148=CARTESIAN_POINT('Ctrl Pts',(18.783128550466,13.8402116270357,10.7967447226094));
#208149=CARTESIAN_POINT('Ctrl Pts',(18.6667829055578,11.6302479438492,12.0923869446781));
#208150=CARTESIAN_POINT('Ctrl Pts',(18.5504372606496,9.07084875549921,12.2022971521955));
#208151=CARTESIAN_POINT('Ctrl Pts',(18.4340916157414,6.75794009747201,11.1008873267927));
#208152=CARTESIAN_POINT('Ctrl Pts',(18.3177459708332,5.23009931839809,9.04460543076101));
#208153=CARTESIAN_POINT('Ctrl Pts',(18.201400325925,4.84300962499006,6.51226200115517));
#208154=CARTESIAN_POINT('Ctrl Pts',(18.0850546810169,5.686938743654,4.09346001665621));
#208155=CARTESIAN_POINT('Ctrl Pts',(17.9687090361086,7.56509618299146,2.3514835298456));
#208156=CARTESIAN_POINT('Ctrl Pts',(17.8523633912005,10.0407569035218,1.69178858099628));
#208157=CARTESIAN_POINT('Ctrl Pts',(17.7747996279283,11.7042668215791,2.07631929646177));
#208158=CARTESIAN_POINT('Ctrl Pts',(17.7360177462923,12.4430604071541,2.45215525491025));
#208159=CARTESIAN_POINT('Ctrl Pts',(17.734,12.4414757859805,2.45527019889633));
#208160=CARTESIAN_POINT('Ctrl Pts',(17.734,12.3039867051776,2.39880617496762));
#208161=CARTESIAN_POINT('Ctrl Pts',(17.734,12.1641669931159,2.34855999836893));
#208162=CARTESIAN_POINT('Ctrl Pts',(17.734,12.0224504771058,2.30458254792744));
#208163=CARTESIAN_POINT('Ctrl Pts',(17.734,11.8806702981265,2.26058534160181));
#208164=CARTESIAN_POINT('Ctrl Pts',(17.734,11.7369908076955,2.22286244819522));
#208165=CARTESIAN_POINT('Ctrl Pts',(17.734,11.5918412571295,2.19151632686583));
#208166=CARTESIAN_POINT('Ctrl Pts',(17.734,11.5283759214344,2.17781051720157));
#208167=CARTESIAN_POINT('Ctrl Pts',(17.734,11.4646295455477,2.16532448469426));
#208168=CARTESIAN_POINT('Ctrl Pts',(17.734,11.4006382986832,2.15406992347917));
#208169=CARTESIAN_POINT('Ctrl Pts',(17.734,11.3633072808146,2.14750427198133));
#208170=CARTESIAN_POINT('Ctrl Pts',(17.734,11.3258921197711,2.14135763815236));
#208171=CARTESIAN_POINT('Ctrl Pts',(17.734,11.2884026214455,2.13563303349492));
#208172=CARTESIAN_POINT('Ctrl Pts',(17.734,11.2692561047233,2.13270938170716));
#208173=CARTESIAN_POINT('Ctrl Pts',(17.734,11.250091584631,2.12989604625388));
#208174=CARTESIAN_POINT('Ctrl Pts',(17.734,11.2309171197761,2.12719424914615));
#208175=CARTESIAN_POINT('Ctrl Pts',(17.734,11.0859964654593,2.10677405970945));
#208176=CARTESIAN_POINT('Ctrl Pts',(17.734,10.9403799749511,2.09270150463882));
#208177=CARTESIAN_POINT('Ctrl Pts',(17.734,10.7944837770183,2.0850637244268));
#208178=CARTESIAN_POINT('Ctrl Pts',(17.734,10.6507966464814,2.07754159062287));
#208179=CARTESIAN_POINT('Ctrl Pts',(17.734,10.5068375056611,2.07626094200617));
#208180=CARTESIAN_POINT('Ctrl Pts',(17.734,10.3630121887448,2.08135439022792));
#208181=CARTESIAN_POINT('Ctrl Pts',(17.734,10.2786127987142,2.08434332105237));
#208182=CARTESIAN_POINT('Ctrl Pts',(17.734,10.1942597021903,2.08952813543894));
#208183=CARTESIAN_POINT('Ctrl Pts',(17.734,10.1100377343263,2.0969435515888));
#208184=CARTESIAN_POINT('Ctrl Pts',(17.734,10.0914524803675,2.09857991079354));
#208185=CARTESIAN_POINT('Ctrl Pts',(17.734,10.0728758846397,2.10032474830959));
#208186=CARTESIAN_POINT('Ctrl Pts',(17.734,10.054317787698,2.10217740077462));
#208187=CARTESIAN_POINT('Ctrl Pts',(17.734,10.0520311372889,2.10240567679508));
#208188=CARTESIAN_POINT('Ctrl Pts',(17.734,10.0497447287136,2.1026355930538));
#208189=CARTESIAN_POINT('Ctrl Pts',(17.734,10.0474585635589,2.10286714977861));
#208190=CARTESIAN_POINT('Ctrl Pts',(17.734,9.90553857679408,2.11724167003299));
#208191=CARTESIAN_POINT('Ctrl Pts',(17.734,9.76455596495627,2.13793360360503));
#208192=CARTESIAN_POINT('Ctrl Pts',(17.734,9.62489441371198,2.164760150274));
#208193=CARTESIAN_POINT('Ctrl Pts',(17.734,9.4842370437923,2.19177797633183));
#208194=CARTESIAN_POINT('Ctrl Pts',(17.734,9.34491888101862,2.2250185138914));
#208195=CARTESIAN_POINT('Ctrl Pts',(17.734,9.2073470145511,2.26434539672021));
#208196=CARTESIAN_POINT('Ctrl Pts',(17.734,9.0710255779474,2.30331482631383));
#208197=CARTESIAN_POINT('Ctrl Pts',(17.734,8.93641816408468,2.34826086911714));
#208198=CARTESIAN_POINT('Ctrl Pts',(17.734,8.8039462971496,2.39909462227723));
#208199=CARTESIAN_POINT('Ctrl Pts',(17.734,8.67331233993274,2.44922310985069));
#208200=CARTESIAN_POINT('Ctrl Pts',(17.734,8.54475450125128,2.50507746381745));
#208201=CARTESIAN_POINT('Ctrl Pts',(17.734,8.4187110735798,2.56660924088476));
#208202=CARTESIAN_POINT('Ctrl Pts',(17.734,8.39060081781657,2.58033208247104));
#208203=CARTESIAN_POINT('Ctrl Pts',(17.734,8.36261638829719,2.59433712698117));
#208204=CARTESIAN_POINT('Ctrl Pts',(17.734,8.33476077291323,2.60862517471304));
#208205=CARTESIAN_POINT('Ctrl Pts',(17.734,8.31199475765094,2.62030260162493));
#208206=CARTESIAN_POINT('Ctrl Pts',(17.734,8.28931855664526,2.63216728166961));
#208207=CARTESIAN_POINT('Ctrl Pts',(17.734,8.26675493626269,2.64420787360863));
#208208=CARTESIAN_POINT('Ctrl Pts',(17.734,8.14790051002851,2.70763198827501));
#208209=CARTESIAN_POINT('Ctrl Pts',(17.734,8.032030238517,2.77600356619099));
#208210=CARTESIAN_POINT('Ctrl Pts',(17.734,7.91948448293877,2.84921041197833));
#208211=CARTESIAN_POINT('Ctrl Pts',(17.734,7.89990776773299,2.86194434018138));
#208212=CARTESIAN_POINT('Ctrl Pts',(17.734,7.88043170399221,2.87482465916843));
#208213=CARTESIAN_POINT('Ctrl Pts',(17.734,7.86105816656312,2.88785089183458));
#208214=CARTESIAN_POINT('Ctrl Pts',(17.734,7.74528165055074,2.96569583060084));
#208215=CARTESIAN_POINT('Ctrl Pts',(17.734,7.63316351668281,3.04874885969149));
#208216=CARTESIAN_POINT('Ctrl Pts',(17.734,7.52499462458614,3.13669681545407));
#208217=CARTESIAN_POINT('Ctrl Pts',(17.734,7.41763480848604,3.22398694271739));
#208218=CARTESIAN_POINT('Ctrl Pts',(17.734,7.31416494708026,3.31609973205607));
#208219=CARTESIAN_POINT('Ctrl Pts',(17.734,7.2149110901292,3.41275797655135));
#208220=CARTESIAN_POINT('Ctrl Pts',(17.734,7.13012408679148,3.4953276937431));
#208221=CARTESIAN_POINT('Ctrl Pts',(17.734,7.04841415789455,3.5812150691776));
#208222=CARTESIAN_POINT('Ctrl Pts',(17.734,6.97001249572361,3.67025869427777));
#208223=CARTESIAN_POINT('Ctrl Pts',(17.734,6.95431915067657,3.68808219819647));
#208224=CARTESIAN_POINT('Ctrl Pts',(17.734,6.93875844510523,3.70603218668507));
#208225=CARTESIAN_POINT('Ctrl Pts',(17.734,6.92333236973455,3.72410739902025));
#208226=CARTESIAN_POINT('Ctrl Pts',(17.734,6.91090397970631,3.7386701301976));
#208227=CARTESIAN_POINT('Ctrl Pts',(17.734,6.89856246392884,3.75331485694984));
#208228=CARTESIAN_POINT('Ctrl Pts',(17.734,6.88631933290202,3.7680280979283));
#208229=CARTESIAN_POINT('Ctrl Pts',(17.734,6.79919924774975,3.87272507487816));
#208230=CARTESIAN_POINT('Ctrl Pts',(17.734,6.7169286678634,3.98103806042143));
#208231=CARTESIAN_POINT('Ctrl Pts',(17.734,6.63977277908297,4.09267000357134));
#208232=CARTESIAN_POINT('Ctrl Pts',(17.734,6.56326133238926,4.20336954449602));
#208233=CARTESIAN_POINT('Ctrl Pts',(17.734,6.49177912371476,4.3173335019011));
#208234=CARTESIAN_POINT('Ctrl Pts',(17.734,6.42562994044659,4.43429573638148));
#208235=CARTESIAN_POINT('Ctrl Pts',(17.734,6.40600466641507,4.46899632964067));
#208236=CARTESIAN_POINT('Ctrl Pts',(17.734,6.38684913115322,4.50396095400166));
#208237=CARTESIAN_POINT('Ctrl Pts',(17.734,6.36817211518176,4.5391829311905));
#208238=CARTESIAN_POINT('Ctrl Pts',(17.734,6.30473751328733,4.65881082594215));
#208239=CARTESIAN_POINT('Ctrl Pts',(17.734,6.24681897356675,4.78140717330283));
#208240=CARTESIAN_POINT('Ctrl Pts',(17.734,6.19457219597214,4.90656879650476));
#208241=CARTESIAN_POINT('Ctrl Pts',(17.734,6.166564858854,4.97366276739939));
#208242=CARTESIAN_POINT('Ctrl Pts',(17.734,6.14018823211239,5.04149397277739));
#208243=CARTESIAN_POINT('Ctrl Pts',(17.734,6.11547251222998,5.11000011542537));
#208244=CARTESIAN_POINT('Ctrl Pts',(17.734,6.10242953316116,5.14615217528421));
#208245=CARTESIAN_POINT('Ctrl Pts',(17.734,6.08984917084278,5.18249218937426));
#208246=CARTESIAN_POINT('Ctrl Pts',(17.734,6.07773636073121,5.21901091873209));
#208247=CARTESIAN_POINT('Ctrl Pts',(17.734,6.06903436381049,5.24524643860674));
#208248=CARTESIAN_POINT('Ctrl Pts',(17.734,6.06057221985005,5.27157936583366));
#208249=CARTESIAN_POINT('Ctrl Pts',(17.734,6.05236276273648,5.29796985450767));
#208250=CARTESIAN_POINT('Ctrl Pts',(17.734,6.01297460249778,5.42458879925516));
#208251=CARTESIAN_POINT('Ctrl Pts',(17.734,5.97934462684376,5.55268880302192));
#208252=CARTESIAN_POINT('Ctrl Pts',(17.734,5.95155790703941,5.68187791678551));
#208253=CARTESIAN_POINT('Ctrl Pts',(17.734,5.92387819466376,5.81056951968859));
#208254=CARTESIAN_POINT('Ctrl Pts',(17.734,5.90199676487722,5.94034266902156));
#208255=CARTESIAN_POINT('Ctrl Pts',(17.734,5.88604904274555,6.07081358834923));
#208256=CARTESIAN_POINT('Ctrl Pts',(17.734,5.87037715515666,6.1990278602334));
#208257=CARTESIAN_POINT('Ctrl Pts',(17.734,5.8604355485385,6.3279166852093));
#208258=CARTESIAN_POINT('Ctrl Pts',(17.734,5.85640219965237,6.4571081864847));
#208259=CARTESIAN_POINT('Ctrl Pts',(17.734,5.85485839225705,6.50655761441974));
#208260=CARTESIAN_POINT('Ctrl Pts',(17.734,5.85418069613621,6.55605125001335));
#208261=CARTESIAN_POINT('Ctrl Pts',(17.734,5.85438103290403,6.60556760587704));
#208262=CARTESIAN_POINT('Ctrl Pts',(17.734,5.85480000921424,6.70912413372275));
#208263=CARTESIAN_POINT('Ctrl Pts',(17.734,5.85905829450831,6.81278078385137));
#208264=CARTESIAN_POINT('Ctrl Pts',(17.734,5.86714838588205,6.9163217216595));
#208265=CARTESIAN_POINT('Ctrl Pts',(23.534,7.33966741897454,3.77664721604216));
#208266=CARTESIAN_POINT('Ctrl Pts',(23.534,7.4278110653291,3.68403366522654));
#208267=CARTESIAN_POINT('Ctrl Pts',(23.534,7.52001976376112,3.59567730315309));
#208268=CARTESIAN_POINT('Ctrl Pts',(23.534,7.61588000351043,3.51169601948419));
#208269=CARTESIAN_POINT('Ctrl Pts',(23.534,7.71428950781667,3.42548137493008));
#208270=CARTESIAN_POINT('Ctrl Pts',(23.534,7.81654770302536,3.34387704113668));
#208271=CARTESIAN_POINT('Ctrl Pts',(23.534,7.92225677089516,3.2670337517176));
#208272=CARTESIAN_POINT('Ctrl Pts',(23.534,8.02887849234131,3.18952702533591));
#208273=CARTESIAN_POINT('Ctrl Pts',(23.534,8.13901148190336,3.11686336124311));
#208274=CARTESIAN_POINT('Ctrl Pts',(23.534,8.25229019242955,3.04922905262568));
#208275=CARTESIAN_POINT('Ctrl Pts',(23.534,8.36548868719601,2.98164263771595));
#208276=CARTESIAN_POINT('Ctrl Pts',(23.534,8.48182908274332,2.91907793777968));
#208277=CARTESIAN_POINT('Ctrl Pts',(23.534,8.60098002349002,2.86176024173783));
#208278=CARTESIAN_POINT('Ctrl Pts',(23.534,8.62551775114871,2.84995633984092));
#208279=CARTESIAN_POINT('Ctrl Pts',(23.534,8.65017477000968,2.83837511498036));
#208280=CARTESIAN_POINT('Ctrl Pts',(23.534,8.67494832377365,2.82701877421198));
#208281=CARTESIAN_POINT('Ctrl Pts',(23.534,8.69677888932777,2.81701151631264));
#208282=CARTESIAN_POINT('Ctrl Pts',(23.534,8.7187040887079,2.80717716259871));
#208283=CARTESIAN_POINT('Ctrl Pts',(23.534,8.7406954034996,2.7975286977491));
#208284=CARTESIAN_POINT('Ctrl Pts',(23.534,8.86780597067235,2.74176023410807));
#208285=CARTESIAN_POINT('Ctrl Pts',(23.534,8.99727639743939,2.69212556532351));
#208286=CARTESIAN_POINT('Ctrl Pts',(23.534,9.12866759232672,2.6487952833054));
#208287=CARTESIAN_POINT('Ctrl Pts',(23.534,9.25547643309881,2.60697617329764));
#208288=CARTESIAN_POINT('Ctrl Pts',(23.534,9.38407515938091,2.57102868262553));
#208289=CARTESIAN_POINT('Ctrl Pts',(23.534,9.51404078368099,2.54089289360578));
#208290=CARTESIAN_POINT('Ctrl Pts',(23.534,9.64599296324215,2.51029647193376));
#208291=CARTESIAN_POINT('Ctrl Pts',(23.534,9.77935483569613,2.48569051020136));
#208292=CARTESIAN_POINT('Ctrl Pts',(23.534,9.91370948271856,2.46705966806754));
#208293=CARTESIAN_POINT('Ctrl Pts',(23.534,10.031006234944,2.45079422938006));
#208294=CARTESIAN_POINT('Ctrl Pts',(23.534,10.1490603917624,2.43908365615739));
#208295=CARTESIAN_POINT('Ctrl Pts',(23.534,10.2676037380491,2.43194887296395));
#208296=CARTESIAN_POINT('Ctrl Pts',(23.534,10.3041175791339,2.42975120984864));
#208297=CARTESIAN_POINT('Ctrl Pts',(23.534,10.3406773911072,2.42798791270649));
#208298=CARTESIAN_POINT('Ctrl Pts',(23.534,10.3772769926549,2.4266601138214));
#208299=CARTESIAN_POINT('Ctrl Pts',(23.534,10.4011419710093,2.42579431500634));
#208300=CARTESIAN_POINT('Ctrl Pts',(23.534,10.4250202861952,2.42511392850954));
#208301=CARTESIAN_POINT('Ctrl Pts',(23.534,10.4488889852346,2.42461930902579));
#208302=CARTESIAN_POINT('Ctrl Pts',(23.534,10.5881947640817,2.42173254287641));
#208303=CARTESIAN_POINT('Ctrl Pts',(23.534,10.7273545088382,2.4251622122633));
#208304=CARTESIAN_POINT('Ctrl Pts',(23.534,10.8659190930214,2.43484421424554));
#208305=CARTESIAN_POINT('Ctrl Pts',(23.534,10.9998137685222,2.44419991304298));
#208306=CARTESIAN_POINT('Ctrl Pts',(23.534,11.1331535298942,2.45939375404109));
#208307=CARTESIAN_POINT('Ctrl Pts',(23.534,11.2655490821966,2.48041129060109));
#208308=CARTESIAN_POINT('Ctrl Pts',(23.534,11.2886886126467,2.48408464607836));
#208309=CARTESIAN_POINT('Ctrl Pts',(23.534,11.3117993244444,2.48793600302252));
#208310=CARTESIAN_POINT('Ctrl Pts',(23.534,11.3348791639493,2.49196542192025));
#208311=CARTESIAN_POINT('Ctrl Pts',(23.534,11.4716128752646,2.51583722571738));
#208312=CARTESIAN_POINT('Ctrl Pts',(23.534,11.6072631372987,2.54595436303442));
#208313=CARTESIAN_POINT('Ctrl Pts',(23.534,11.741474161821,2.58210348353803));
#208314=CARTESIAN_POINT('Ctrl Pts',(23.534,11.8669921985643,2.61591118787352));
#208315=CARTESIAN_POINT('Ctrl Pts',(23.534,11.9912519180839,2.65499542884546));
#208316=CARTESIAN_POINT('Ctrl Pts',(23.534,12.1139562411199,2.69922248208064));
#208317=CARTESIAN_POINT('Ctrl Pts',(23.534,12.1324792825538,2.70589885271947));
#208318=CARTESIAN_POINT('Ctrl Pts',(23.534,12.1509668598302,2.71269248793648));
#208319=CARTESIAN_POINT('Ctrl Pts',(23.534,12.1694179272643,2.71960300224709));
#208320=CARTESIAN_POINT('Ctrl Pts',(23.534,12.1864042738565,2.725964931801));
#208321=CARTESIAN_POINT('Ctrl Pts',(23.534,12.2033501584913,2.73242235622137));
#208322=CARTESIAN_POINT('Ctrl Pts',(23.534,12.2202547019028,2.73897459134067));
#208323=CARTESIAN_POINT('Ctrl Pts',(23.534,12.3523840941254,2.79018821024405));
#208324=CARTESIAN_POINT('Ctrl Pts',(23.534,12.4819900441372,2.84719066756166));
#208325=CARTESIAN_POINT('Ctrl Pts',(23.534,12.6087145787098,2.90970780354203));
#208326=CARTESIAN_POINT('Ctrl Pts',(23.534,12.7371473048524,2.97306764330525));
#208327=CARTESIAN_POINT('Ctrl Pts',(23.534,12.8626211666514,3.04209197614692));
#208328=CARTESIAN_POINT('Ctrl Pts',(23.534,12.9847605797274,3.11654906625687));
#208329=CARTESIAN_POINT('Ctrl Pts',(23.534,13.1066107532674,3.19082983380514));
#208330=CARTESIAN_POINT('Ctrl Pts',(23.534,13.2251430159627,3.27051793771162));
#208331=CARTESIAN_POINT('Ctrl Pts',(23.534,13.339970121412,3.35543295399967));
#208332=CARTESIAN_POINT('Ctrl Pts',(23.534,13.3745616920472,3.38101353249137));
#208333=CARTESIAN_POINT('Ctrl Pts',(23.534,13.4088168737746,3.40706878536305));
#208334=CARTESIAN_POINT('Ctrl Pts',(23.534,13.442724662023,3.43359460806598));
#208335=CARTESIAN_POINT('Ctrl Pts',(23.534,13.5222654936816,3.49581883757828));
#208336=CARTESIAN_POINT('Ctrl Pts',(23.534,13.5998952497886,3.56063180043892));
#208337=CARTESIAN_POINT('Ctrl Pts',(23.534,13.6755304223662,3.62791906475953));
#208338=CARTESIAN_POINT('Ctrl Pts',(23.534,13.6988785584492,3.64869025031348));
#208339=CARTESIAN_POINT('Ctrl Pts',(23.534,13.7220365683719,3.66969729110703));
#208340=CARTESIAN_POINT('Ctrl Pts',(23.534,13.7450018328666,3.69093701222324));
#208341=CARTESIAN_POINT('Ctrl Pts',(23.534,13.7616807918054,3.70636276255376));
#208342=CARTESIAN_POINT('Ctrl Pts',(23.534,13.778252633284,3.72190625726443));
#208343=CARTESIAN_POINT('Ctrl Pts',(23.534,13.794710755701,3.73756042625356));
#208344=CARTESIAN_POINT('Ctrl Pts',(23.534,13.8994714966307,3.83720376954569));
#208345=CARTESIAN_POINT('Ctrl Pts',(23.5339999999999,13.9997005890967,3.9413957803482));
#208346=CARTESIAN_POINT('Ctrl Pts',(23.5339999999999,14.0951974348199,4.04973935219108));
#208347=CARTESIAN_POINT('Ctrl Pts',(23.5339999999999,14.1919272854646,4.15948179910966));
#208348=CARTESIAN_POINT('Ctrl Pts',(23.5339999999999,14.2838024902719,4.27348416760255));
#208349=CARTESIAN_POINT('Ctrl Pts',(23.534,14.370586183448,4.39137862115632));
#208350=CARTESIAN_POINT('Ctrl Pts',(23.534,14.3939765840093,4.42315415860651));
#208351=CARTESIAN_POINT('Ctrl Pts',(23.534,14.4169969315166,4.45521265895707));
#208352=CARTESIAN_POINT('Ctrl Pts',(23.5339999999999,14.4396421540893,4.48754739858326));
#208353=CARTESIAN_POINT('Ctrl Pts',(23.5339999999999,14.4633057306723,4.52133622909603));
#208354=CARTESIAN_POINT('Ctrl Pts',(23.534,14.486559687685,4.55542670188665));
#208355=CARTESIAN_POINT('Ctrl Pts',(23.534,14.5093979973546,4.58981135573279));
#208356=CARTESIAN_POINT('Ctrl Pts',(23.5339999999999,14.5229724195575,4.6102485866559));
#208357=CARTESIAN_POINT('Ctrl Pts',(23.534,14.5363970207432,4.63078533674386));
#208358=CARTESIAN_POINT('Ctrl Pts',(23.534,14.5496664278029,4.65141310427564));
#208359=CARTESIAN_POINT('Ctrl Pts',(23.534,14.6302131840668,4.77662591568343));
#208360=CARTESIAN_POINT('Ctrl Pts',(23.5339999999999,14.7050940684627,4.90526377791114));
#208361=CARTESIAN_POINT('Ctrl Pts',(23.5339999999999,14.7740779860328,5.03693509762841));
#208362=CARTESIAN_POINT('Ctrl Pts',(23.5339999999999,14.825130242171,5.13437980904875));
#208363=CARTESIAN_POINT('Ctrl Pts',(23.534,14.8729522304357,5.2334868876652));
#208364=CARTESIAN_POINT('Ctrl Pts',(23.534,14.917437260214,5.33411057035729));
#208365=CARTESIAN_POINT('Ctrl Pts',(23.534,14.9671573568045,5.44657580299121));
#208366=CARTESIAN_POINT('Ctrl Pts',(23.5339999999999,15.012709422787,5.56093556570214));
#208367=CARTESIAN_POINT('Ctrl Pts',(23.5339999999999,15.0540735698273,5.67694764394986));
#208368=CARTESIAN_POINT('Ctrl Pts',(23.5319822588655,15.0572813588473,8.3237916645841));
#208369=CARTESIAN_POINT('Ctrl Pts',(23.4932003772294,14.8422325070833,9.12430563616661));
#208370=CARTESIAN_POINT('Ctrl Pts',(23.4156366139573,14.0148887345381,10.6178356099985));
#208371=CARTESIAN_POINT('Ctrl Pts',(23.2992909690491,11.8680999648663,12.0161880919895));
#208372=CARTESIAN_POINT('Ctrl Pts',(23.1829453241409,9.31682637793275,12.2463212706672));
#208373=CARTESIAN_POINT('Ctrl Pts',(23.0665996792327,6.95460748608732,11.2549883962344));
#208374=CARTESIAN_POINT('Ctrl Pts',(22.9502540343245,5.33172308320188,9.27285619592476));
#208375=CARTESIAN_POINT('Ctrl Pts',(22.8339083894163,4.82593288295298,6.76152807094034));
#208376=CARTESIAN_POINT('Ctrl Pts',(22.7175627445081,5.55506383184552,4.30571494350424));
#208377=CARTESIAN_POINT('Ctrl Pts',(22.6012170995999,7.3493153728942,2.47725496135783));
#208378=CARTESIAN_POINT('Ctrl Pts',(22.4848714546917,9.79091952574551,1.70188575047227));
#208379=CARTESIAN_POINT('Ctrl Pts',(22.3685258097835,12.3113588873047,2.16015052666956));
#208380=CARTESIAN_POINT('Ctrl Pts',(22.2521801648753,14.3237650772533,3.74534470495516));
#208381=CARTESIAN_POINT('Ctrl Pts',(22.1358345199671,15.3595658072703,6.08836352082835));
#208382=CARTESIAN_POINT('Ctrl Pts',(22.0194888750589,15.1775704930741,8.64365536817768));
#208383=CARTESIAN_POINT('Ctrl Pts',(21.9031432301507,13.8201792815797,10.8162233916012));
#208384=CARTESIAN_POINT('Ctrl Pts',(21.7867975852425,11.6034022891174,12.100225958688));
#208385=CARTESIAN_POINT('Ctrl Pts',(21.6704519403344,9.0435073068744,12.1966334909658));
#208386=CARTESIAN_POINT('Ctrl Pts',(21.5541062954261,6.73633029032072,11.0831185230676));
#208387=CARTESIAN_POINT('Ctrl Pts',(21.437760650518,5.21954311482696,9.01870407716815));
#208388=CARTESIAN_POINT('Ctrl Pts',(21.3214150056097,4.84535773940766,6.4846037851452));
#208389=CARTESIAN_POINT('Ctrl Pts',(21.2050693607016,5.70291518904701,4.06976343034357));
#208390=CARTESIAN_POINT('Ctrl Pts',(21.0887237157934,7.58832315778984,2.3387736849668));
#208391=CARTESIAN_POINT('Ctrl Pts',(20.9723780708852,10.0713935791024,1.68985436313296));
#208392=CARTESIAN_POINT('Ctrl Pts',(20.856032425977,12.555501431994,2.28420306077143));
#208393=CARTESIAN_POINT('Ctrl Pts',(20.7009048994327,15.1484714499262,4.5226444707105));
#208394=CARTESIAN_POINT('Ctrl Pts',(20.5069954912524,15.7229266692027,9.1400596639883));
#208395=CARTESIAN_POINT('Ctrl Pts',(20.274304201436,11.4791150714787,12.8347936062911));
#208396=CARTESIAN_POINT('Ctrl Pts',(20.0803947932557,6.98475562540071,11.6301131359937));
#208397=CARTESIAN_POINT('Ctrl Pts',(19.9252672667114,5.12461246395865,8.75366030680187));
#208398=CARTESIAN_POINT('Ctrl Pts',(19.8089216218032,4.87791900276309,6.21138090921678));
#208399=CARTESIAN_POINT('Ctrl Pts',(19.692575976895,5.86251193291384,3.84129404048311));
#208400=CARTESIAN_POINT('Ctrl Pts',(19.5762303319868,7.83658921959077,2.21215083823699));
#208401=CARTESIAN_POINT('Ctrl Pts',(19.4598846870786,10.346497559081,1.69521868991591));
#208402=CARTESIAN_POINT('Ctrl Pts',(19.3435390421704,12.8049519410314,2.41471923687709));
#208403=CARTESIAN_POINT('Ctrl Pts',(19.2271933972622,14.6408870657878,4.20127809621151));
#208404=CARTESIAN_POINT('Ctrl Pts',(19.1108477523541,15.4261618032088,6.63978685285258));
#208405=CARTESIAN_POINT('Ctrl Pts',(18.9945021074458,14.9782427651156,9.16203292881471));
#208406=CARTESIAN_POINT('Ctrl Pts',(18.8781564625377,13.4012755888355,11.1809280106677));
#208407=CARTESIAN_POINT('Ctrl Pts',(18.7618108176295,11.062518755214,12.2262888051469));
#208408=CARTESIAN_POINT('Ctrl Pts',(18.6454651727213,8.50650330604877,12.0547553007003));
#208409=CARTESIAN_POINT('Ctrl Pts',(18.5291195278131,6.32839771745935,10.7062463579064));
#208410=CARTESIAN_POINT('Ctrl Pts',(18.4127738829049,5.03535314052584,8.49476382840791));
#208411=CARTESIAN_POINT('Ctrl Pts',(18.2964282379967,4.92844964904422,5.9352340231685));
#208412=CARTESIAN_POINT('Ctrl Pts',(18.1800825930885,6.03257956786553,3.62362735793028));
#208413=CARTESIAN_POINT('Ctrl Pts',(18.0637369481803,8.09064912978604,2.09819162438962));
#208414=CARTESIAN_POINT('Ctrl Pts',(17.9473913032721,10.6234591686693,1.7141039202743));
#208415=CARTESIAN_POINT('Ctrl Pts',(17.8310456583639,13.0412397395454,2.56082098582784));
#208416=CARTESIAN_POINT('Ctrl Pts',(17.7147000134557,14.7810693674473,4.44113870113773));
#208417=CARTESIAN_POINT('Ctrl Pts',(17.5983543685475,15.4377476650143,6.9173439782558));
#208418=CARTESIAN_POINT('Ctrl Pts',(17.4820087236393,14.8585632965897,9.41264028584843));
#208419=CARTESIAN_POINT('Ctrl Pts',(17.3656591966584,13.1779145254008,11.3465351757322));
#208420=CARTESIAN_POINT('Ctrl Pts',(17.2880915513137,11.5845997651963,11.9603782329704));
#208421=CARTESIAN_POINT('Ctrl Pts',(17.2493057876049,10.7620145183404,12.0631392312232));
#208422=CARTESIAN_POINT('Ctrl Pts',(23.694570999514,14.7853120162315,8.25073023540143));
#208423=CARTESIAN_POINT('Ctrl Pts',(23.655789117878,14.5821319326992,9.00706301412011));
#208424=CARTESIAN_POINT('Ctrl Pts',(23.5782253546058,13.8004501174428,10.4181635261759));
#208425=CARTESIAN_POINT('Ctrl Pts',(23.4618797096977,11.7721448371763,11.739339490465));
#208426=CARTESIAN_POINT('Ctrl Pts',(23.3455340647894,9.36167867446536,11.9567713813296));
#208427=CARTESIAN_POINT('Ctrl Pts',(23.2291884198813,7.12983308296455,11.020151192087));
#208428=CARTESIAN_POINT('Ctrl Pts',(23.112842774973,5.59651734639213,9.14741491506193));
#208429=CARTESIAN_POINT('Ctrl Pts',(22.9964971300649,5.11864222967593,6.77468958299936));
#208430=CARTESIAN_POINT('Ctrl Pts',(22.8801514851566,5.80753168845142,4.45441531843442));
#208431=CARTESIAN_POINT('Ctrl Pts',(22.7638058402485,7.50275663384358,2.72686993113926));
#208432=CARTESIAN_POINT('Ctrl Pts',(22.6474601953403,9.80960613180611,1.99429414780511));
#208433=CARTESIAN_POINT('Ctrl Pts',(22.5311145504321,12.1909398418867,2.42726681770743));
#208434=CARTESIAN_POINT('Ctrl Pts',(22.4147689055239,14.0922792557956,3.9249724921022));
#208435=CARTESIAN_POINT('Ctrl Pts',(22.2984232606157,15.0709130737463,6.13867767965353));
#208436=CARTESIAN_POINT('Ctrl Pts',(22.1820776157075,14.8989622689056,8.5529403308379));
#208437=CARTESIAN_POINT('Ctrl Pts',(22.0657319707993,13.6164868802894,10.6056020812167));
#208438=CARTESIAN_POINT('Ctrl Pts',(21.9493863258911,11.5220560995322,11.8187392205059));
#208439=CARTESIAN_POINT('Ctrl Pts',(21.8330406809829,9.10344436522311,11.9098259215075));
#208440=CARTESIAN_POINT('Ctrl Pts',(21.7166950360747,6.92360283106935,10.8577669947277));
#208441=CARTESIAN_POINT('Ctrl Pts',(21.6003493911665,5.49052870633148,8.90728971422824));
#208442=CARTESIAN_POINT('Ctrl Pts',(21.4840037462583,5.13699500824085,6.51304903454513));
#208443=CARTESIAN_POINT('Ctrl Pts',(21.3676581013501,5.94722297654782,4.23148621297622));
#208444=CARTESIAN_POINT('Ctrl Pts',(21.251312456442,7.72857333224318,2.59603157941593));
#208445=CARTESIAN_POINT('Ctrl Pts',(21.1349668115337,10.0746005324842,1.98292678515909));
#208446=CARTESIAN_POINT('Ctrl Pts',(21.0186211666256,12.4216079073839,2.54447276433055));
#208447=CARTESIAN_POINT('Ctrl Pts',(20.8634936400813,14.8714692320025,4.65937228098899));
#208448=CARTESIAN_POINT('Ctrl Pts',(20.669584231901,15.4142196744288,9.02194756087552));
#208449=CARTESIAN_POINT('Ctrl Pts',(20.4368929420846,11.404628421799,12.5127653209751));
#208450=CARTESIAN_POINT('Ctrl Pts',(20.2429835339043,7.15831731533217,11.3745724100295));
#208451=CARTESIAN_POINT('Ctrl Pts',(20.08785600736,5.40083737612914,8.65687398328613));
#208452=CARTESIAN_POINT('Ctrl Pts',(19.9715103624518,5.16775918184238,6.25490561132425));
#208453=CARTESIAN_POINT('Ctrl Pts',(19.8551647175436,6.09801141128885,4.01562628470573));
#208454=CARTESIAN_POINT('Ctrl Pts',(19.7388190726354,7.96313733368371,2.47639717837344));
#208455=CARTESIAN_POINT('Ctrl Pts',(19.6224734277272,10.3345212396799,1.98799504920659));
#208456=CARTESIAN_POINT('Ctrl Pts',(19.506127782819,12.6572909851945,2.6677856178796));
#208457=CARTESIAN_POINT('Ctrl Pts',(19.3897821379108,14.3918989542587,4.35574244860633));
#208458=CARTESIAN_POINT('Ctrl Pts',(19.2734364930026,15.1338335678885,6.65966738847239));
#208459=CARTESIAN_POINT('Ctrl Pts',(19.1570908480944,14.7106356441191,9.04270809852214));
#208460=CARTESIAN_POINT('Ctrl Pts',(19.0407452031862,13.2207029149922,10.9501782756895));
#208461=CARTESIAN_POINT('Ctrl Pts',(18.924399558278,11.0110244864905,11.9378445282709));
#208462=CARTESIAN_POINT('Ctrl Pts',(18.8080539133698,8.59607816982169,11.7757781350949));
#208463=CARTESIAN_POINT('Ctrl Pts',(18.6917082684616,6.53818447821767,10.501694793596));
#208464=CARTESIAN_POINT('Ctrl Pts',(18.5753626235535,5.31650436694375,8.41226626892347));
#208465=CARTESIAN_POINT('Ctrl Pts',(18.4590169786453,5.21550098956712,5.99399955712194));
#208466=CARTESIAN_POINT('Ctrl Pts',(18.342671333737,6.25869283782141,3.80997285116951));
#208467=CARTESIAN_POINT('Ctrl Pts',(18.2263256888289,8.2031754150418,2.36872749123559));
#208468=CARTESIAN_POINT('Ctrl Pts',(18.1099800439207,10.5961970519886,2.00583798419682));
#208469=CARTESIAN_POINT('Ctrl Pts',(17.9936343990125,12.8805378160702,2.80582386041163));
#208470=CARTESIAN_POINT('Ctrl Pts',(17.8772887541043,14.524344449909,4.58236489901824));
#208471=CARTESIAN_POINT('Ctrl Pts',(17.7609431091961,15.1447799940149,6.92190584946314));
#208472=CARTESIAN_POINT('Ctrl Pts',(17.6445974642879,14.5975614090662,9.27948417669346));
#208473=CARTESIAN_POINT('Ctrl Pts',(17.528247937307,13.0096693793363,11.1066454102745));
#208474=CARTESIAN_POINT('Ctrl Pts',(17.4506802919623,11.5042913063256,11.6866098352056));
#208475=CARTESIAN_POINT('Ctrl Pts',(17.4118945282535,10.7271053888111,11.7836993478332));
#208476=CARTESIAN_POINT('Ctrl Pts',(23.8571597401626,14.5133426736158,8.17766880621875));
#208477=CARTESIAN_POINT('Ctrl Pts',(23.8183778585265,14.3220313583152,8.88982039207361));
#208478=CARTESIAN_POINT('Ctrl Pts',(23.7408140952544,13.5860115003476,10.2184914423533));
#208479=CARTESIAN_POINT('Ctrl Pts',(23.6244684503462,11.6761897094863,11.4624908889405));
#208480=CARTESIAN_POINT('Ctrl Pts',(23.508122805438,9.40653097099794,11.667221491992));
#208481=CARTESIAN_POINT('Ctrl Pts',(23.3917771605298,7.30505867984177,10.7853139879396));
#208482=CARTESIAN_POINT('Ctrl Pts',(23.2754315156216,5.86131160958236,9.02197363419911));
#208483=CARTESIAN_POINT('Ctrl Pts',(23.1590858707135,5.4113515763989,6.78785109505837));
#208484=CARTESIAN_POINT('Ctrl Pts',(23.0427402258052,6.0599995450573,4.60311569336461));
#208485=CARTESIAN_POINT('Ctrl Pts',(22.9263945808971,7.65619789479296,2.97648490092068));
#208486=CARTESIAN_POINT('Ctrl Pts',(22.8100489359889,9.8282927378667,2.28670254513794));
#208487=CARTESIAN_POINT('Ctrl Pts',(22.6937032910807,12.0705207964688,2.69438310874529));
#208488=CARTESIAN_POINT('Ctrl Pts',(22.5773576461725,13.8607934343379,4.10460027924924));
#208489=CARTESIAN_POINT('Ctrl Pts',(22.4610120012643,14.7822603402221,6.18899183847872));
#208490=CARTESIAN_POINT('Ctrl Pts',(22.3446663563561,14.620354044737,8.46222529349812));
#208491=CARTESIAN_POINT('Ctrl Pts',(22.2283207114479,13.4127944789992,10.3949807708323));
#208492=CARTESIAN_POINT('Ctrl Pts',(22.1119750665397,11.440709909947,11.5372524823239));
#208493=CARTESIAN_POINT('Ctrl Pts',(21.9956294216315,9.16338142357181,11.6230183520491));
#208494=CARTESIAN_POINT('Ctrl Pts',(21.8792837767233,7.11087537181799,10.6324154663879));
#208495=CARTESIAN_POINT('Ctrl Pts',(21.7629381318151,5.76151429783599,8.79587535128832));
#208496=CARTESIAN_POINT('Ctrl Pts',(21.6465924869069,5.42863227707405,6.54149428394506));
#208497=CARTESIAN_POINT('Ctrl Pts',(21.5302468419987,6.19153076404863,4.39320899560886));
#208498=CARTESIAN_POINT('Ctrl Pts',(21.4139011970905,7.86882350669652,2.85328947386507));
#208499=CARTESIAN_POINT('Ctrl Pts',(21.2975555521823,10.0778074858659,2.27599920718522));
#208500=CARTESIAN_POINT('Ctrl Pts',(21.1812099072741,12.2877143827737,2.80474246788965));
#208501=CARTESIAN_POINT('Ctrl Pts',(21.0260823807299,14.5944670140789,4.79610009126748));
#208502=CARTESIAN_POINT('Ctrl Pts',(20.8321729725495,15.105512679655,8.90383545776275));
#208503=CARTESIAN_POINT('Ctrl Pts',(20.5994816827331,11.3301417721195,12.1907370356592));
#208504=CARTESIAN_POINT('Ctrl Pts',(20.4055722745528,7.33187900526365,11.1190316840652));
#208505=CARTESIAN_POINT('Ctrl Pts',(20.2504447480086,5.6770622882996,8.56008765977039));
#208506=CARTESIAN_POINT('Ctrl Pts',(20.1340991031004,5.45759936092166,6.29843031343171));
#208507=CARTESIAN_POINT('Ctrl Pts',(20.0177534581922,6.33351088966386,4.18995852892835));
#208508=CARTESIAN_POINT('Ctrl Pts',(19.901407813284,8.08968544777665,2.74064351850989));
#208509=CARTESIAN_POINT('Ctrl Pts',(19.7850621683758,10.3225449202788,2.28077140849729));
#208510=CARTESIAN_POINT('Ctrl Pts',(19.6687165234676,12.5096300293577,2.92085199888212));
#208511=CARTESIAN_POINT('Ctrl Pts',(19.5523708785594,14.1429108427297,4.51020680100116));
#208512=CARTESIAN_POINT('Ctrl Pts',(19.4360252336512,14.841505332568,6.67954792409221));
#208513=CARTESIAN_POINT('Ctrl Pts',(19.319679588743,14.4430285231226,8.92338326822958));
#208514=CARTESIAN_POINT('Ctrl Pts',(19.2033339438348,13.040130241149,10.7194285407112));
#208515=CARTESIAN_POINT('Ctrl Pts',(19.0869882989266,10.9595302177668,11.6494002513949));
#208516=CARTESIAN_POINT('Ctrl Pts',(18.9706426540184,8.6856530335946,11.4968009694893));
#208517=CARTESIAN_POINT('Ctrl Pts',(18.8542970091102,6.74797123897598,10.2971432292856));
#208518=CARTESIAN_POINT('Ctrl Pts',(18.737951364202,5.59765559336166,8.329768709439));
#208519=CARTESIAN_POINT('Ctrl Pts',(18.6216057192938,5.50255233009001,6.05276509107539));
#208520=CARTESIAN_POINT('Ctrl Pts',(18.5052600743856,6.4848061077773,3.99631834440874));
#208521=CARTESIAN_POINT('Ctrl Pts',(18.3889144294774,8.31570170029755,2.63926335808154));
#208522=CARTESIAN_POINT('Ctrl Pts',(18.2725687845692,10.5689349353078,2.29757204811932));
#208523=CARTESIAN_POINT('Ctrl Pts',(18.1562231396611,12.7198358925949,3.05082673499542));
#208524=CARTESIAN_POINT('Ctrl Pts',(18.0398774947529,14.267619532371,4.72359109689875));
#208525=CARTESIAN_POINT('Ctrl Pts',(17.9235318498447,14.8518123230155,6.92646772067049));
#208526=CARTESIAN_POINT('Ctrl Pts',(17.8071862049365,14.3365595215429,9.14632806753851));
#208527=CARTESIAN_POINT('Ctrl Pts',(17.6908366779556,12.8414242332716,10.866755644817));
#208528=CARTESIAN_POINT('Ctrl Pts',(17.6132690326108,11.423982847455,11.4128414374409));
#208529=CARTESIAN_POINT('Ctrl Pts',(17.5744832689021,10.6921962592818,11.5042594644432));
#208530=CARTESIAN_POINT('Ctrl Pts',(24.0197484808112,14.241373331,8.10460737703607));
#208531=CARTESIAN_POINT('Ctrl Pts',(23.980966599175,14.0619307839311,8.7725777700271));
#208532=CARTESIAN_POINT('Ctrl Pts',(23.903402835903,13.3715728832524,10.0188193585307));
#208533=CARTESIAN_POINT('Ctrl Pts',(23.7870571909947,11.5802345817964,11.185642287416));
#208534=CARTESIAN_POINT('Ctrl Pts',(23.6707115460865,9.45138326753054,11.3776716026543));
#208535=CARTESIAN_POINT('Ctrl Pts',(23.5543659011784,7.48028427671899,10.5504767837922));
#208536=CARTESIAN_POINT('Ctrl Pts',(23.4380202562701,6.1261058727726,8.89653235333628));
#208537=CARTESIAN_POINT('Ctrl Pts',(23.3216746113619,5.70406092312185,6.80101260711739));
#208538=CARTESIAN_POINT('Ctrl Pts',(23.2053289664538,6.3124674016632,4.7518160682948));
#208539=CARTESIAN_POINT('Ctrl Pts',(23.0889833215455,7.80963915574233,3.2260998707021));
#208540=CARTESIAN_POINT('Ctrl Pts',(22.9726376766373,9.8469793439273,2.57911094247078));
#208541=CARTESIAN_POINT('Ctrl Pts',(22.8562920317291,11.950101751051,2.96149939978317));
#208542=CARTESIAN_POINT('Ctrl Pts',(22.7399463868209,13.6293076128802,4.28422806639629));
#208543=CARTESIAN_POINT('Ctrl Pts',(22.6236007419127,14.493607606698,6.23930599730392));
#208544=CARTESIAN_POINT('Ctrl Pts',(22.5072550970047,14.3417458205685,8.37151025615833));
#208545=CARTESIAN_POINT('Ctrl Pts',(22.3909094520964,13.209102077709,10.1843594604477));
#208546=CARTESIAN_POINT('Ctrl Pts',(22.2745638071882,11.3593637203619,11.2557657441419));
#208547=CARTESIAN_POINT('Ctrl Pts',(22.15821816228,9.22331848192051,11.3362107825909));
#208548=CARTESIAN_POINT('Ctrl Pts',(22.0418725173718,7.29814791256664,10.4070639380481));
#208549=CARTESIAN_POINT('Ctrl Pts',(21.9255268724636,6.0324998893405,8.68446098834841));
#208550=CARTESIAN_POINT('Ctrl Pts',(21.8091812275554,5.72026954590726,6.56993953334496));
#208551=CARTESIAN_POINT('Ctrl Pts',(21.6928355826472,6.43583855154944,4.55493177824152));
#208552=CARTESIAN_POINT('Ctrl Pts',(21.576489937739,8.00907368114986,3.11054736831421));
#208553=CARTESIAN_POINT('Ctrl Pts',(21.4601442928308,10.0810144392476,2.56907162921135));
#208554=CARTESIAN_POINT('Ctrl Pts',(21.3437986479226,12.1538208581636,3.06501217144877));
#208555=CARTESIAN_POINT('Ctrl Pts',(21.1886711213784,14.3174647961552,4.93282790154597));
#208556=CARTESIAN_POINT('Ctrl Pts',(20.9947617131981,14.7968056848811,8.78572335464998));
#208557=CARTESIAN_POINT('Ctrl Pts',(20.7620704233818,11.2556551224398,11.8687087503432));
#208558=CARTESIAN_POINT('Ctrl Pts',(20.5681610152013,7.50544069519511,10.8634909581011));
#208559=CARTESIAN_POINT('Ctrl Pts',(20.4130334886571,5.95328720047008,8.46330133625465));
#208560=CARTESIAN_POINT('Ctrl Pts',(20.2966878437488,5.74743954000095,6.34195501553917));
#208561=CARTESIAN_POINT('Ctrl Pts',(20.1803421988407,6.56901036803888,4.36429077315096));
#208562=CARTESIAN_POINT('Ctrl Pts',(20.0639965539325,8.21623356186958,3.00488985864633));
#208563=CARTESIAN_POINT('Ctrl Pts',(19.9476509090243,10.3105686008776,2.57354776778798));
#208564=CARTESIAN_POINT('Ctrl Pts',(19.8313052641161,12.3619690735209,3.17391837988464));
#208565=CARTESIAN_POINT('Ctrl Pts',(19.7149596192079,13.8939227312006,4.66467115339598));
#208566=CARTESIAN_POINT('Ctrl Pts',(19.5986139742997,14.5491770972477,6.69942845971203));
#208567=CARTESIAN_POINT('Ctrl Pts',(19.4822683293915,14.1754214021261,8.80405843793702));
#208568=CARTESIAN_POINT('Ctrl Pts',(19.3659226844833,12.8595575673058,10.4886788057329));
#208569=CARTESIAN_POINT('Ctrl Pts',(19.2495770395751,10.9080359490432,11.3609559745189));
#208570=CARTESIAN_POINT('Ctrl Pts',(19.1332313946669,8.77522789736752,11.2178238038838));
#208571=CARTESIAN_POINT('Ctrl Pts',(19.0168857497587,6.95775799973429,10.0925916649752));
#208572=CARTESIAN_POINT('Ctrl Pts',(18.9005401048505,5.87880681977957,8.24727114995455));
#208573=CARTESIAN_POINT('Ctrl Pts',(18.7841944599423,5.7896036706129,6.11153062502883));
#208574=CARTESIAN_POINT('Ctrl Pts',(18.6678488150341,6.71091937773318,4.18266383764797));
#208575=CARTESIAN_POINT('Ctrl Pts',(18.5515031701259,8.4282279855533,2.9097992249275));
#208576=CARTESIAN_POINT('Ctrl Pts',(18.4351575252177,10.5416728186271,2.58930611204184));
#208577=CARTESIAN_POINT('Ctrl Pts',(18.3188118803095,12.5591339691196,3.29582960957921));
#208578=CARTESIAN_POINT('Ctrl Pts',(18.2024662354013,14.0108946148327,4.86481729477925));
#208579=CARTESIAN_POINT('Ctrl Pts',(18.0861205904931,14.5588446520163,6.93102959187783));
#208580=CARTESIAN_POINT('Ctrl Pts',(17.969774945585,14.0755576340194,9.01317195838355));
#208581=CARTESIAN_POINT('Ctrl Pts',(17.8534254186041,12.6731790872071,10.6268658793594));
#208582=CARTESIAN_POINT('Ctrl Pts',(17.7758577732593,11.3436743885842,11.1390730396763));
#208583=CARTESIAN_POINT('Ctrl Pts',(17.7370720095507,10.6572871297526,11.2248195810532));
#208584=CARTESIAN_POINT('Ctrl Pts',(17.734,10.6581555755053,11.2300936493755));
#208585=CARTESIAN_POINT('Ctrl Pts',(17.734,10.7871580301293,11.2265276116833));
#208586=CARTESIAN_POINT('Ctrl Pts',(17.734,10.9158060854873,11.2169788999138));
#208587=CARTESIAN_POINT('Ctrl Pts',(17.734,11.0437268225089,11.2016549886171));
#208588=CARTESIAN_POINT('Ctrl Pts',(17.734,11.1739880981934,11.1860506989574));
#208589=CARTESIAN_POINT('Ctrl Pts',(17.7339999999999,11.3034959146602,11.1644579899871));
#208590=CARTESIAN_POINT('Ctrl Pts',(17.734,11.4318673761861,11.1370431572688));
#208591=CARTESIAN_POINT('Ctrl Pts',(17.734,11.4884530910301,11.1249587898537));
#208592=CARTESIAN_POINT('Ctrl Pts',(17.734,11.5448180845333,11.1117424890396));
#208593=CARTESIAN_POINT('Ctrl Pts',(17.734,11.6009296449061,11.0974052968746));
#208594=CARTESIAN_POINT('Ctrl Pts',(17.734,11.6231422455803,11.0917297048534));
#208595=CARTESIAN_POINT('Ctrl Pts',(17.734,11.6453151296432,11.0858784376901));
#208596=CARTESIAN_POINT('Ctrl Pts',(17.734,11.6674462597462,11.0798520970063));
#208597=CARTESIAN_POINT('Ctrl Pts',(17.734,11.6909691969026,11.0734467651264));
#208598=CARTESIAN_POINT('Ctrl Pts',(17.7339999999999,11.7144371000566,11.0668457533736));
#208599=CARTESIAN_POINT('Ctrl Pts',(17.7339999999999,11.7378417469923,11.0600519299264));
#208600=CARTESIAN_POINT('Ctrl Pts',(17.7339999999999,11.8666178352729,11.0226712332466));
#208601=CARTESIAN_POINT('Ctrl Pts',(17.734,11.9935344010332,10.9794425381218));
#208602=CARTESIAN_POINT('Ctrl Pts',(17.734,12.1181943387372,10.9305490461558));
#208603=CARTESIAN_POINT('Ctrl Pts',(17.734,12.2170317257716,10.8917835447612));
#208604=CARTESIAN_POINT('Ctrl Pts',(17.7339999999999,12.3144508717194,10.8494559613376));
#208605=CARTESIAN_POINT('Ctrl Pts',(17.734,12.4102527649422,10.8036343689628));
#208606=CARTESIAN_POINT('Ctrl Pts',(17.734,12.4582931021382,10.7806569029182));
#208607=CARTESIAN_POINT('Ctrl Pts',(17.7339999999999,12.5059267258685,10.7568005259236));
#208608=CARTESIAN_POINT('Ctrl Pts',(17.7339999999999,12.5531281105939,10.7320719318602));
#208609=CARTESIAN_POINT('Ctrl Pts',(17.7339999999999,12.5796828219838,10.7181600374899));
#208610=CARTESIAN_POINT('Ctrl Pts',(17.734,12.6061007231861,10.703972063894));
#208611=CARTESIAN_POINT('Ctrl Pts',(17.734,12.6323772088884,10.6895090305751));
#208612=CARTESIAN_POINT('Ctrl Pts',(17.734,12.6494661520011,10.6801029799934));
#208613=CARTESIAN_POINT('Ctrl Pts',(17.734,12.6664940896698,10.6705811847365));
#208614=CARTESIAN_POINT('Ctrl Pts',(17.734,12.6834496665741,10.6609498639215));
#208615=CARTESIAN_POINT('Ctrl Pts',(17.734,12.6867649951574,10.6590666491319));
#208616=CARTESIAN_POINT('Ctrl Pts',(17.7339999999999,12.6900776631735,10.6571791889994));
#208617=CARTESIAN_POINT('Ctrl Pts',(17.7339999999999,12.6933876620448,10.6552874881657));
#208618=CARTESIAN_POINT('Ctrl Pts',(17.734,12.813721983353,10.5865150973585));
#208619=CARTESIAN_POINT('Ctrl Pts',(17.7339999999999,12.9305291947834,10.5121431425042));
#208620=CARTESIAN_POINT('Ctrl Pts',(17.7339999999999,13.0435566004255,10.4326032510522));
#208621=CARTESIAN_POINT('Ctrl Pts',(17.7339999999999,13.1542860408063,10.3546804887062));
#208622=CARTESIAN_POINT('Ctrl Pts',(17.734,13.2613883832878,10.2717971251543));
#208623=CARTESIAN_POINT('Ctrl Pts',(17.734,13.3646136018082,10.184304620467));
#208624=CARTESIAN_POINT('Ctrl Pts',(17.734,13.4710521658323,10.0940885211913));
#208625=CARTESIAN_POINT('Ctrl Pts',(17.734,13.5733692644384,9.99897159633861));
#208626=CARTESIAN_POINT('Ctrl Pts',(17.734,13.6712668291685,9.89928713892361));
#208627=CARTESIAN_POINT('Ctrl Pts',(17.734,13.7691643938986,9.79960268150861));
#208628=CARTESIAN_POINT('Ctrl Pts',(17.734,13.8626431607924,9.69535014068124));
#208629=CARTESIAN_POINT('Ctrl Pts',(17.734,13.9513699801085,9.58681812087919));
#208630=CARTESIAN_POINT('Ctrl Pts',(17.734,13.9628634835586,9.57275908941993));
#208631=CARTESIAN_POINT('Ctrl Pts',(17.734,13.9742785921472,9.55862643429634));
#208632=CARTESIAN_POINT('Ctrl Pts',(17.734,13.9856099775934,9.54442644912111));
#208633=CARTESIAN_POINT('Ctrl Pts',(17.734,14.0729113490609,9.43502427702995));
#208634=CARTESIAN_POINT('Ctrl Pts',(17.734,14.155041858068,9.32188662452608));
#208635=CARTESIAN_POINT('Ctrl Pts',(17.734,14.2317472591746,9.20538350790436));
#208636=CARTESIAN_POINT('Ctrl Pts',(17.734,14.2502066068323,9.17734673993373));
#208637=CARTESIAN_POINT('Ctrl Pts',(17.734,14.2683516627921,9.14911485201464));
#208638=CARTESIAN_POINT('Ctrl Pts',(17.734,14.2861786693898,9.12069260839312));
#208639=CARTESIAN_POINT('Ctrl Pts',(17.734,14.3596274174382,9.003590603674));
#208640=CARTESIAN_POINT('Ctrl Pts',(17.734,14.4276801174426,8.88326038142579));
#208641=CARTESIAN_POINT('Ctrl Pts',(17.734,14.4902884333847,8.76012784854773));
#208642=CARTESIAN_POINT('Ctrl Pts',(17.734,14.5537529998883,8.63531131732493));
#208643=CARTESIAN_POINT('Ctrl Pts',(17.734,14.6116236543273,8.50761468833234));
#208644=CARTESIAN_POINT('Ctrl Pts',(17.734,14.6638094340128,8.37744644946211));
#208645=CARTESIAN_POINT('Ctrl Pts',(17.734,14.7100740696555,8.26204746184758));
#208646=CARTESIAN_POINT('Ctrl Pts',(17.734,14.7518702709569,8.14470509092437));
#208647=CARTESIAN_POINT('Ctrl Pts',(17.734,14.7891046475072,8.02568745899151));
#208648=CARTESIAN_POINT('Ctrl Pts',(17.734,14.7957588699923,8.0044176036614));
#208649=CARTESIAN_POINT('Ctrl Pts',(17.734,14.802267320164,7.98309421356168));
#208650=CARTESIAN_POINT('Ctrl Pts',(17.734,14.8086293625773,7.9617187827321));
#208651=CARTESIAN_POINT('Ctrl Pts',(17.734,14.8141582507119,7.94314261517331));
#208652=CARTESIAN_POINT('Ctrl Pts',(17.734,14.8195767038318,7.92452645243315));
#208653=CARTESIAN_POINT('Ctrl Pts',(17.734,14.8248800133524,7.90588690657763));
#208654=CARTESIAN_POINT('Ctrl Pts',(17.734,14.8642211214105,7.76761468527757));
#208655=CARTESIAN_POINT('Ctrl Pts',(17.734,14.8972903477015,7.62785672464352));
#208656=CARTESIAN_POINT('Ctrl Pts',(17.734,14.9240435546541,7.48706785777848));
#208657=CARTESIAN_POINT('Ctrl Pts',(17.734,14.9507706801502,7.34641624469049));
#208658=CARTESIAN_POINT('Ctrl Pts',(17.734,14.9711943919531,7.20473499473391));
#208659=CARTESIAN_POINT('Ctrl Pts',(17.734,14.9852278277044,7.06244825044858));
#208660=CARTESIAN_POINT('Ctrl Pts',(17.734,14.9897675457622,7.01641948644058));
#208661=CARTESIAN_POINT('Ctrl Pts',(17.734,14.9936381823968,6.9703271759923));
#208662=CARTESIAN_POINT('Ctrl Pts',(17.734,14.9968357553433,6.92418521713769));
#208663=CARTESIAN_POINT('Ctrl Pts',(17.734,15.0067323514289,6.78137429866483));
#208664=CARTESIAN_POINT('Ctrl Pts',(17.734,15.010185425558,6.63808849971136));
#208665=CARTESIAN_POINT('Ctrl Pts',(17.734,15.0073112040798,6.49472810706366));
#208666=CARTESIAN_POINT('Ctrl Pts',(17.734,15.0056440306924,6.41157284806935));
#208667=CARTESIAN_POINT('Ctrl Pts',(17.734,15.0018470671246,6.32839227527477));
#208668=CARTESIAN_POINT('Ctrl Pts',(17.734,14.9959350165701,6.24526375434569));
#208669=CARTESIAN_POINT('Ctrl Pts',(17.734,14.9930494071184,6.20468960101485));
#208670=CARTESIAN_POINT('Ctrl Pts',(17.734,14.9896598294849,6.16412784684823));
#208671=CARTESIAN_POINT('Ctrl Pts',(17.734,14.9857674896188,6.12358750933691));
#208672=CARTESIAN_POINT('Ctrl Pts',(17.734,14.9839181537182,6.10432590727623));
#208673=CARTESIAN_POINT('Ctrl Pts',(17.734,14.9819550242892,6.08506643814876));
#208674=CARTESIAN_POINT('Ctrl Pts',(17.734,14.9798791802301,6.06581902520355));
#208675=CARTESIAN_POINT('Ctrl Pts',(17.734,14.9642028796882,5.92046695568584));
#208676=CARTESIAN_POINT('Ctrl Pts',(17.734,14.9421349343852,5.77608373015697));
#208677=CARTESIAN_POINT('Ctrl Pts',(17.734,14.9138625332143,5.63308993321275));
#208678=CARTESIAN_POINT('Ctrl Pts',(17.734,14.8852999123965,5.48862828749952));
#208679=CARTESIAN_POINT('Ctrl Pts',(17.734,14.8504048157976,5.34558398957191));
#208680=CARTESIAN_POINT('Ctrl Pts',(17.734,14.8093178156465,5.20437943577393));
#208681=CARTESIAN_POINT('Ctrl Pts',(17.734,14.7681579286769,5.06292439032063));
#208682=CARTESIAN_POINT('Ctrl Pts',(17.734,14.7207840951535,4.9233148246561));
#208683=CARTESIAN_POINT('Ctrl Pts',(17.734,14.667285708432,4.78597583896446));
#208684=CARTESIAN_POINT('Ctrl Pts',(17.734,14.6372084702283,4.70876271833717));
#208685=CARTESIAN_POINT('Ctrl Pts',(17.734,14.6051944642011,4.63226735308866));
#208686=CARTESIAN_POINT('Ctrl Pts',(17.734,14.5712524834494,4.55656680407632));
#208687=CARTESIAN_POINT('Ctrl Pts',(17.734,14.5209818578362,4.44444859901504));
#208688=CARTESIAN_POINT('Ctrl Pts',(17.734,14.4664830452091,4.33407329976893));
#208689=CARTESIAN_POINT('Ctrl Pts',(17.734,14.4079024230562,4.22562346067727));
#208690=CARTESIAN_POINT('Ctrl Pts',(23.534,15.0539061944433,8.32288496556903));
#208691=CARTESIAN_POINT('Ctrl Pts',(23.534,15.0045196831565,8.46102105477102));
#208692=CARTESIAN_POINT('Ctrl Pts',(23.534,14.9491584466399,8.59666359933282));
#208693=CARTESIAN_POINT('Ctrl Pts',(23.534,14.8880945730864,8.72949016701669));
#208694=CARTESIAN_POINT('Ctrl Pts',(23.534,14.8263802252141,8.86373165101867));
#208695=CARTESIAN_POINT('Ctrl Pts',(23.534,14.7588406646471,8.99509750972211));
#208696=CARTESIAN_POINT('Ctrl Pts',(23.534,14.6857106710821,9.1232292879567));
#208697=CARTESIAN_POINT('Ctrl Pts',(23.534,14.6128819085716,9.25083327630936));
#208698=CARTESIAN_POINT('Ctrl Pts',(23.534,14.5345081505848,9.37523035919426));
#208699=CARTESIAN_POINT('Ctrl Pts',(23.534,14.450783174498,9.49603193123717));
#208700=CARTESIAN_POINT('Ctrl Pts',(23.534,14.3684650046542,9.61480370985814));
#208701=CARTESIAN_POINT('Ctrl Pts',(23.534,14.280973400568,9.73010024309469));
#208702=CARTESIAN_POINT('Ctrl Pts',(23.534,14.1884635407845,9.84151116501465));
#208703=CARTESIAN_POINT('Ctrl Pts',(23.534,14.1636970862173,9.87133775368834));
#208704=CARTESIAN_POINT('Ctrl Pts',(23.534,14.1385708227763,9.90088559984961));
#208705=CARTESIAN_POINT('Ctrl Pts',(23.534,14.1130874412093,9.9301462552455));
#208706=CARTESIAN_POINT('Ctrl Pts',(23.534,14.0994446628436,9.94581123421829));
#208707=CARTESIAN_POINT('Ctrl Pts',(23.534,14.0856995289216,9.96139389704753));
#208708=CARTESIAN_POINT('Ctrl Pts',(23.534,14.0718524398192,9.97689291659844));
#208709=CARTESIAN_POINT('Ctrl Pts',(23.534,14.0595282691968,9.99068733649516));
#208710=CARTESIAN_POINT('Ctrl Pts',(23.534,14.0471248899774,10.0044136985475));
#208711=CARTESIAN_POINT('Ctrl Pts',(23.534,14.0346501013912,10.0180631245397));
#208712=CARTESIAN_POINT('Ctrl Pts',(23.534,13.9325629744592,10.129762867921));
#208713=CARTESIAN_POINT('Ctrl Pts',(23.534,13.8255589167938,10.2364694610508));
#208714=CARTESIAN_POINT('Ctrl Pts',(23.534,13.7138822995671,10.3377901011926));
#208715=CARTESIAN_POINT('Ctrl Pts',(23.534,13.6072656917372,10.4345199558688));
#208716=CARTESIAN_POINT('Ctrl Pts',(23.534,13.4963893994936,10.5263409917788));
#208717=CARTESIAN_POINT('Ctrl Pts',(23.534,13.3816361432654,10.6130491512947));
#208718=CARTESIAN_POINT('Ctrl Pts',(23.534,13.2675216549389,10.6992746544493));
#208719=CARTESIAN_POINT('Ctrl Pts',(23.534,13.14957248217,10.7804443135872));
#208720=CARTESIAN_POINT('Ctrl Pts',(23.534,13.0281452130351,10.8563104469715));
#208721=CARTESIAN_POINT('Ctrl Pts',(23.534,12.9228679008957,10.9220863032682));
#208722=CARTESIAN_POINT('Ctrl Pts',(23.534,12.8149755625439,10.9838749599025));
#208723=CARTESIAN_POINT('Ctrl Pts',(23.534,12.7046950051531,11.0414837392859));
#208724=CARTESIAN_POINT('Ctrl Pts',(23.534,12.6704660549416,11.0593643892202));
#208725=CARTESIAN_POINT('Ctrl Pts',(23.534,12.6360070180388,11.0768421453942));
#208726=CARTESIAN_POINT('Ctrl Pts',(23.534,12.6013246618057,11.0939106397649));
#208727=CARTESIAN_POINT('Ctrl Pts',(23.534,12.5775343548302,11.1056187462719));
#208728=CARTESIAN_POINT('Ctrl Pts',(23.534,12.5536338344587,11.1171366062184));
#208729=CARTESIAN_POINT('Ctrl Pts',(23.534,12.5296548188552,11.1284484392924));
#208730=CARTESIAN_POINT('Ctrl Pts',(23.534,12.4026030627483,11.1883836877031));
#208731=CARTESIAN_POINT('Ctrl Pts',(23.534,12.2732186532336,11.2426060623178));
#208732=CARTESIAN_POINT('Ctrl Pts',(23.534,12.1418579788868,11.2909272251374));
#208733=CARTESIAN_POINT('Ctrl Pts',(23.534,12.0110656904147,11.3390393066126));
#208734=CARTESIAN_POINT('Ctrl Pts',(23.534,11.8783134757111,11.381301368659));
#208735=CARTESIAN_POINT('Ctrl Pts',(23.534,11.7439408942886,11.4174776418709));
#208736=CARTESIAN_POINT('Ctrl Pts',(23.534,11.7185306168275,11.4243186888322));
#208737=CARTESIAN_POINT('Ctrl Pts',(23.534,11.6930623778329,11.4309419582457));
#208738=CARTESIAN_POINT('Ctrl Pts',(23.534,11.6675384567621,11.4373456433974));
#208739=CARTESIAN_POINT('Ctrl Pts',(23.534,11.5320041155766,11.4713497936919));
#208740=CARTESIAN_POINT('Ctrl Pts',(23.534,11.394899148674,11.4991663992332));
#208741=CARTESIAN_POINT('Ctrl Pts',(23.534,11.2566535581235,11.5207487746459));
#208742=CARTESIAN_POINT('Ctrl Pts',(23.534,11.1395174117289,11.5390356239828));
#208743=CARTESIAN_POINT('Ctrl Pts',(23.534,11.0215621487013,11.5528458727715));
#208744=CARTESIAN_POINT('Ctrl Pts',(23.534,10.9030568789718,11.5621227836795));
#208745=CARTESIAN_POINT('Ctrl Pts',(23.534,10.8727885717626,11.5644922680911));
#208746=CARTESIAN_POINT('Ctrl Pts',(23.534,10.842484435087,11.5665658756357));
#208747=CARTESIAN_POINT('Ctrl Pts',(23.534,10.8121490716819,11.5683423926637));
#208748=CARTESIAN_POINT('Ctrl Pts',(23.534,10.7942046025595,11.5693932670024));
#208749=CARTESIAN_POINT('Ctrl Pts',(23.5339999999999,10.7762590661863,11.5703396029876));
#208750=CARTESIAN_POINT('Ctrl Pts',(23.534,10.7583140714215,11.5711814532735));
#208751=CARTESIAN_POINT('Ctrl Pts',(23.534,10.621315610092,11.5776084372518));
#208752=CARTESIAN_POINT('Ctrl Pts',(23.534,10.4843351016943,11.5779507199327));
#208753=CARTESIAN_POINT('Ctrl Pts',(23.534,10.3477779769602,11.5722201804618));
#208754=CARTESIAN_POINT('Ctrl Pts',(23.534,10.2117250437028,11.5665107990898));
#208755=CARTESIAN_POINT('Ctrl Pts',(23.5339999999999,10.0760915867093,11.5547732226163));
#208756=CARTESIAN_POINT('Ctrl Pts',(23.534,9.94128731881931,11.5369684475339));
#208757=CARTESIAN_POINT('Ctrl Pts',(23.534,9.80868446687355,11.5194544326505));
#208758=CARTESIAN_POINT('Ctrl Pts',(23.534,9.6768832696469,11.4960695457153));
#208759=CARTESIAN_POINT('Ctrl Pts',(23.534,9.54629292150131,11.4667302088784));
#208760=CARTESIAN_POINT('Ctrl Pts',(23.534,9.51124646542765,11.4588564280494));
#208761=CARTESIAN_POINT('Ctrl Pts',(23.534,9.47628735690692,11.4505535423166));
#208762=CARTESIAN_POINT('Ctrl Pts',(23.534,9.44142384068048,11.4418193834442));
#208763=CARTESIAN_POINT('Ctrl Pts',(23.534,9.35465567581843,11.4200818475038));
#208764=CARTESIAN_POINT('Ctrl Pts',(23.534,9.26847914064439,11.395673426388));
#208765=CARTESIAN_POINT('Ctrl Pts',(23.534,9.18301437324067,11.3686311001959));
#208766=CARTESIAN_POINT('Ctrl Pts',(23.5339999999999,9.15095469784315,11.3584869410757));
#208767=CARTESIAN_POINT('Ctrl Pts',(23.534,9.11899524917183,11.347972079119));
#208768=CARTESIAN_POINT('Ctrl Pts',(23.534,9.08714263326126,11.3370882239502));
#208769=CARTESIAN_POINT('Ctrl Pts',(23.534,9.06138445704345,11.328286803679));
#208770=CARTESIAN_POINT('Ctrl Pts',(23.534,9.03570611685647,11.3192474073759));
#208771=CARTESIAN_POINT('Ctrl Pts',(23.534,9.01012249887741,11.3099758407481));
#208772=CARTESIAN_POINT('Ctrl Pts',(23.534,8.88381687735452,11.2642023701475));
#208773=CARTESIAN_POINT('Ctrl Pts',(23.534,8.75972821578054,11.2127431095304));
#208774=CARTESIAN_POINT('Ctrl Pts',(23.534,8.63823633686677,11.1557838962941));
#208775=CARTESIAN_POINT('Ctrl Pts',(23.534,8.51762502970603,11.099237522786));
#208776=CARTESIAN_POINT('Ctrl Pts',(23.534,8.39957237008985,11.0372701269964));
#208777=CARTESIAN_POINT('Ctrl Pts',(23.534,8.28448331186548,10.9700247931754));
#208778=CARTESIAN_POINT('Ctrl Pts',(23.534,8.26743565831103,10.9600640273839));
#208779=CARTESIAN_POINT('Ctrl Pts',(23.534,8.25045309970698,10.9499873952506));
#208780=CARTESIAN_POINT('Ctrl Pts',(23.534,8.23353702790625,10.939795299223));
#208781=CARTESIAN_POINT('Ctrl Pts',(23.534,8.20315452082413,10.9214895463633));
#208782=CARTESIAN_POINT('Ctrl Pts',(23.534,8.17298647883075,10.902811329405));
#208783=CARTESIAN_POINT('Ctrl Pts',(23.534,8.14304114129207,10.8837628607093));
#208784=CARTESIAN_POINT('Ctrl Pts',(23.534,8.12583577094011,10.8728183870288));
#208785=CARTESIAN_POINT('Ctrl Pts',(23.534,8.1087059434679,10.8617529204478));
#208786=CARTESIAN_POINT('Ctrl Pts',(23.534,8.09166038518003,10.8505717991687));
#208787=CARTESIAN_POINT('Ctrl Pts',(23.534,7.98236466033437,10.778878708561));
#208788=CARTESIAN_POINT('Ctrl Pts',(23.534,7.87644328077357,10.7023783007896));
#208789=CARTESIAN_POINT('Ctrl Pts',(23.534,7.77426954147463,10.6212231772217));
#208790=CARTESIAN_POINT('Ctrl Pts',(23.534,7.70156836402746,10.5634776833234));
#208791=CARTESIAN_POINT('Ctrl Pts',(23.534,7.6307652650132,10.5033747155762));
#208792=CARTESIAN_POINT('Ctrl Pts',(23.534,7.56200744420826,10.4409593356367));
#208793=CARTESIAN_POINT('Ctrl Pts',(23.534,7.4852823732511,10.3713116301304));
#208794=CARTESIAN_POINT('Ctrl Pts',(23.534,7.41110370365363,10.298784417752));
#208795=CARTESIAN_POINT('Ctrl Pts',(23.534,7.33961515870573,10.2235362531339));
#208796=CARTESIAN_POINT('Ctrl Pts',(-17.1175857387455,20.5721719462546,
0.0021420622487661));
#208797=CARTESIAN_POINT('Ctrl Pts',(-16.6641680440313,20.0337688721201,
0.0445526553076218));
#208798=CARTESIAN_POINT('Ctrl Pts',(-16.3459143283547,18.477787514409,0.129355183926955));
#208799=CARTESIAN_POINT('Ctrl Pts',(-18.0613963234494,16.802775720219,0.256549648106768));
#208800=CARTESIAN_POINT('Ctrl Pts',(-20.3933471209293,17.343653714663,0.383725454788201));
#208801=CARTESIAN_POINT('Ctrl Pts',(-21.203092243631,19.5945946034862,0.510901261469636));
#208802=CARTESIAN_POINT('Ctrl Pts',(-19.7475288885744,21.4952120560344,
0.638077068151069));
#208803=CARTESIAN_POINT('Ctrl Pts',(-17.3621513494713,21.2993774656764,
0.765252874832505));
#208804=CARTESIAN_POINT('Ctrl Pts',(-16.2353413405934,19.1880163469751,
0.892428681513937));
#208805=CARTESIAN_POINT('Ctrl Pts',(-17.4009051420832,17.0975180849442,
1.01960448819538));
#208806=CARTESIAN_POINT('Ctrl Pts',(-19.7894957664261,16.9461241370553,
1.14678029487681));
#208807=CARTESIAN_POINT('Ctrl Pts',(-21.2097371145961,18.8725531087288,
1.27395610155824));
#208808=CARTESIAN_POINT('Ctrl Pts',(-20.358641983851,21.1095172903669,1.40113190823968));
#208809=CARTESIAN_POINT('Ctrl Pts',(-18.0170393638345,21.6046935058561,
1.52830771492111));
#208810=CARTESIAN_POINT('Ctrl Pts',(-16.333203267628,19.9038128993918,1.65548352160254));
#208811=CARTESIAN_POINT('Ctrl Pts',(-16.8519493500829,17.5673150993311,
1.78265932828398));
#208812=CARTESIAN_POINT('Ctrl Pts',(-19.0973599935786,16.7387984392048,
1.90983513496541));
#208813=CARTESIAN_POINT('Ctrl Pts',(-21.0094104459781,18.1783720950554,
2.03701094164685));
#208814=CARTESIAN_POINT('Ctrl Pts',(-20.8339130159653,20.5653183707664,
2.16418674832828));
#208815=CARTESIAN_POINT('Ctrl Pts',(-18.7318757426636,21.7097612836464,
2.29136255500972));
#208816=CARTESIAN_POINT('Ctrl Pts',(-16.6317873365857,20.561745973449,2.41853836169115));
#208817=CARTESIAN_POINT('Ctrl Pts',(-16.4603485748086,18.1745049842297,
2.54571416837258));
#208818=CARTESIAN_POINT('Ctrl Pts',(-18.3748438750272,16.7381838840222,
2.67288997505402));
#208819=CARTESIAN_POINT('Ctrl Pts',(-20.6188426291484,17.5705180670209,
2.80006578173545));
#208820=CARTESIAN_POINT('Ctrl Pts',(-21.1336152570428,19.9078926156331,
2.92724158841689));
#208821=CARTESIAN_POINT('Ctrl Pts',(-19.4468898237851,21.6059114372621,
3.05441739509832));
#208822=CARTESIAN_POINT('Ctrl Pts',(-17.1061322239997,21.1067476633747,
3.18159320177976));
#208823=CARTESIAN_POINT('Ctrl Pts',(-16.2588422718968,18.8683530700484,
3.30876900846119));
#208824=CARTESIAN_POINT('Ctrl Pts',(-17.6823559096773,16.9443157687486,
3.43594481514263));
#208825=CARTESIAN_POINT('Ctrl Pts',(-20.0706877279544,17.0998205628843,
3.56312062182406));
#208826=CARTESIAN_POINT('Ctrl Pts',(-21.2326915200203,19.1922014562322,
3.6902964285055));
#208827=CARTESIAN_POINT('Ctrl Pts',(-20.102300928759,21.3018288465973,3.81747223518693));
#208828=CARTESIAN_POINT('Ctrl Pts',(-17.7165791616921,21.4932505417456,
3.94464804186836));
#208829=CARTESIAN_POINT('Ctrl Pts',(-16.264277865515,19.590849017254,4.0718238485498));
#208830=CARTESIAN_POINT('Ctrl Pts',(-17.0777933394838,17.3399595955375,
4.19899965523123));
#208831=CARTESIAN_POINT('Ctrl Pts',(-19.4107756286979,16.8056336150422,
4.32617546191267));
#208832=CARTESIAN_POINT('Ctrl Pts',(-21.1228582840144,18.4780819988752,
4.4533512685941));
#208833=CARTESIAN_POINT('Ctrl Pts',(-20.6433117330145,20.8229371587163,
4.58052707527553));
#208834=CARTESIAN_POINT('Ctrl Pts',(-18.4120901722247,21.6889400235399,
4.70770288195697));
#208835=CARTESIAN_POINT('Ctrl Pts',(-16.4762008984415,20.281586715068,4.8348786886384));
#208836=CARTESIAN_POINT('Ctrl Pts',(-16.6117021655217,17.8920365436271,
4.96205449531983));
#208837=CARTESIAN_POINT('Ctrl Pts',(-18.6942799710763,16.7125534793035,
5.08923030200127));
#208838=CARTESIAN_POINT('Ctrl Pts',(-20.8132984378653,17.8252400266391,
5.21640610868271));
#208839=CARTESIAN_POINT('Ctrl Pts',(-21.0246896437286,20.2092753395693,
5.34358191536413));
#208840=CARTESIAN_POINT('Ctrl Pts',(-19.1345152777048,21.6774549884001,
5.47075772204558));
#208841=CARTESIAN_POINT('Ctrl Pts',(-16.8768930031683,20.8828152708351,
5.59793352872701));
#208842=CARTESIAN_POINT('Ctrl Pts',(-16.3230511331653,18.5543888068372,
5.72510933540844));
#208843=CARTESIAN_POINT('Ctrl Pts',(-17.98110520812,16.8283623586792,5.85228514208988));
#208844=CARTESIAN_POINT('Ctrl Pts',(-20.3298935247037,17.288258063263,5.97946094877131));
#208845=CARTESIAN_POINT('Ctrl Pts',(-21.2145485846948,19.5121501559794,
6.10663675545275));
#208846=CARTESIAN_POINT('Ctrl Pts',(-19.8234542784372,21.4597556720715,
6.23381256213418));
#208847=CARTESIAN_POINT('Ctrl Pts',(-17.4328532908718,21.3442674325558,
6.36098836881561));
#208848=CARTESIAN_POINT('Ctrl Pts',(-16.235973650659,19.2716387291798,6.48816417549706));
#208849=CARTESIAN_POINT('Ctrl Pts',(-17.3308781409654,17.1433777554452,
6.61533998217847));
#208850=CARTESIAN_POINT('Ctrl Pts',(-19.7130598493718,16.9120318599802,
6.74251578885992));
#208851=CARTESIAN_POINT('Ctrl Pts',(-21.1970149132871,18.7898465429281,
6.86969159554135));
#208852=CARTESIAN_POINT('Ctrl Pts',(-20.4213066662076,21.054043383008,6.99686740222279));
#208853=CARTESIAN_POINT('Ctrl Pts',(-18.0975992789452,21.6273623113514,
7.12404320890422));
#208854=CARTESIAN_POINT('Ctrl Pts',(-16.3577500537671,19.9838187953891,
7.25121901558565));
#208855=CARTESIAN_POINT('Ctrl Pts',(-16.7979626675525,17.6312620012014,
7.37839482226709));
#208856=CARTESIAN_POINT('Ctrl Pts',(-19.0143693698296,16.7280167713133,
7.50557062894852));
#208857=CARTESIAN_POINT('Ctrl Pts',(-20.9735545769736,18.1027545424254,
7.63274643562996));
#208858=CARTESIAN_POINT('Ctrl Pts',(-20.8780874621779,20.4942387353917,
7.75992224231139));
#208859=CARTESIAN_POINT('Ctrl Pts',(-18.8155531779101,21.7084310354144,
7.88709804899282));
#208860=CARTESIAN_POINT('Ctrl Pts',(-16.6781989146708,20.6313853684961,
8.01427385567426));
#208861=CARTESIAN_POINT('Ctrl Pts',(-16.4269145498154,18.2512242850411,
8.1414496623557));
#208862=CARTESIAN_POINT('Ctrl Pts',(-18.2922378916319,16.7515978496617,
8.26862546903713));
#208863=CARTESIAN_POINT('Ctrl Pts',(-20.5628505490275,17.5083202395048,
8.39580127571856));
#208864=CARTESIAN_POINT('Ctrl Pts',(-21.155606338957,19.8271456293778,8.5229770824));
#208865=CARTESIAN_POINT('Ctrl Pts',(-19.5266886147337,21.5806956466074,
8.65015288908143));
#208866=CARTESIAN_POINT('Ctrl Pts',(-17.1705282862964,21.160196987974,8.77732869576286));
#208867=CARTESIAN_POINT('Ctrl Pts',(-16.2487562151834,18.9514310736836,
8.9045045024443));
#208868=CARTESIAN_POINT('Ctrl Pts',(-17.607041065014,16.9808035386242,9.03168030912573));
#208869=CARTESIAN_POINT('Ctrl Pts',(-19.9992407907343,17.0562428352734,
9.15885611580717));
#208870=CARTESIAN_POINT('Ctrl Pts',(-21.2306606206557,19.1085380912468,
9.2860319224886));
#208871=CARTESIAN_POINT('Ctrl Pts',(-20.1715492913599,21.2548357889979,
9.41320772917003));
#208872=CARTESIAN_POINT('Ctrl Pts',(-17.7935757116131,21.5260410050991,
9.54038353585147));
#208873=CARTESIAN_POINT('Ctrl Pts',(-16.278383047147,19.6733397866716,9.66755934253291));
#208874=CARTESIAN_POINT('Ctrl Pts',(-17.0160665241465,17.3964705100163,
9.79473514921434));
#208875=CARTESIAN_POINT('Ctrl Pts',(-19.3298473382648,16.7843194180195,
9.92191095589577));
#208876=CARTESIAN_POINT('Ctrl Pts',(-21.0969752019817,18.3984971432064,
10.0490867625772));
#208877=CARTESIAN_POINT('Ctrl Pts',(-20.696219980662,20.7580958098868,10.1762625692586));
#208878=CARTESIAN_POINT('Ctrl Pts',(-18.4952497161921,21.6983300945914,
10.3034383759401));
#208879=CARTESIAN_POINT('Ctrl Pts',(-16.5133180186021,20.356593398625,10.4306141826215));
#208880=CARTESIAN_POINT('Ctrl Pts',(-16.5687242078764,17.9638458629655,
10.5577899893029));
#208881=CARTESIAN_POINT('Ctrl Pts',(-18.6106365442519,16.7152848409195,
10.6849657959844));
#208882=CARTESIAN_POINT('Ctrl Pts',(-20.7657271944765,17.7563875757774,
10.8121416026658));
#208883=CARTESIAN_POINT('Ctrl Pts',(-21.0568342469805,20.1320069264304,
10.9393174093472));
#208884=CARTESIAN_POINT('Ctrl Pts',(-19.2168850492326,21.6626595862203,
11.0664932160287));
#208885=CARTESIAN_POINT('Ctrl Pts',(-16.93391879004,20.9440667428082,11.1936690227101));
#208886=CARTESIAN_POINT('Ctrl Pts',(-16.3024153153455,18.6354927291228,
11.3208448293915));
#208887=CARTESIAN_POINT('Ctrl Pts',(-17.9017398676552,16.8549109164576,
11.448020636073));
#208888=CARTESIAN_POINT('Ctrl Pts',(-20.2646114355015,17.2358946025617,
11.5751964427544));
#208889=CARTESIAN_POINT('Ctrl Pts',(-21.2232420117351,19.428914901949,11.7023722494359));
#208890=CARTESIAN_POINT('Ctrl Pts',(-19.8981475419851,21.4220118041223,
11.8295480561173));
#208891=CARTESIAN_POINT('Ctrl Pts',(-17.5050199576091,21.3866426068827,
11.9567238627987));
#208892=CARTESIAN_POINT('Ctrl Pts',(-16.2394052830226,19.3552563534375,
12.0838996694802));
#208893=CARTESIAN_POINT('Ctrl Pts',(-17.2624264292529,17.1915238492725,
12.2110754761616));
#208894=CARTESIAN_POINT('Ctrl Pts',(-19.635524990487,16.880535370574,12.338251282843));
#208895=CARTESIAN_POINT('Ctrl Pts',(-21.1815303279007,18.707603544426,12.4654270895244));
#208896=CARTESIAN_POINT('Ctrl Pts',(-20.48207850033,20.9965067219594,12.5926028962059));
#208897=CARTESIAN_POINT('Ctrl Pts',(-18.1788731466945,21.6473183031405,
12.7197787028873));
#208898=CARTESIAN_POINT('Ctrl Pts',(-16.3849622259084,20.0629590561579,
12.8469545095688));
#208899=CARTESIAN_POINT('Ctrl Pts',(-16.7461476651242,17.6969802536931,
12.9741303162502));
#208900=CARTESIAN_POINT('Ctrl Pts',(-18.9310642415578,16.7200205978014,
13.1013061229316));
#208901=CARTESIAN_POINT('Ctrl Pts',(-20.9351866075484,18.0283799358088,
13.2284819296131));
#208902=CARTESIAN_POINT('Ctrl Pts',(-20.9198568821621,20.4217197810322,
13.3556577362945));
#208903=CARTESIAN_POINT('Ctrl Pts',(-18.8991391369708,21.7042993729031,
13.4828335429759));
#208904=CARTESIAN_POINT('Ctrl Pts',(-16.7269164832995,20.6994315417472,
13.6100093496574));
#208905=CARTESIAN_POINT('Ctrl Pts',(-16.3960683825486,18.3290201535185,
13.7371851563388));
#208906=CARTESIAN_POINT('Ctrl Pts',(-18.2101274324079,16.7677705325936,
13.8643609630202));
#208907=CARTESIAN_POINT('Ctrl Pts',(-20.5048070478343,17.4480323040911,
13.9915367697017));
#208908=CARTESIAN_POINT('Ctrl Pts',(-21.1748811055536,19.7457075144692,
14.1187125763831));
#208909=CARTESIAN_POINT('Ctrl Pts',(-19.6055982470946,21.5528217680131,
14.2458883830645));
#208910=CARTESIAN_POINT('Ctrl Pts',(-17.2366780944146,21.2114598992563,
14.373064189746));
#208911=CARTESIAN_POINT('Ctrl Pts',(-16.2414578558307,19.0348002354761,
14.5002399964274));
#208912=CARTESIAN_POINT('Ctrl Pts',(-17.5329903299092,17.0197929194559,
14.6274158031088));
#208913=CARTESIAN_POINT('Ctrl Pts',(-19.926374633229,17.0150820981853,14.7545916097903));
#208914=CARTESIAN_POINT('Ctrl Pts',(-21.2258292176773,19.0249896577937,
14.8817674164717));
#208915=CARTESIAN_POINT('Ctrl Pts',(-20.2391851552704,21.2055501612724,
15.0089432231531));
#208916=CARTESIAN_POINT('Ctrl Pts',(-17.8716271352296,21.5562346875283,
15.1361190298346));
#208917=CARTESIAN_POINT('Ctrl Pts',(-16.2952426937192,19.7553119496581,
15.263294836516));
#208918=CARTESIAN_POINT('Ctrl Pts',(-16.956266714372,17.4550167817861,15.3904706431974));
#208919=CARTESIAN_POINT('Ctrl Pts',(-19.2482506860169,16.7657272280153,
15.5176464498789));
#208920=CARTESIAN_POINT('Ctrl Pts',(-21.0684415712385,18.3198236717957,
15.6448222565603));
#208921=CARTESIAN_POINT('Ctrl Pts',(-20.7469272066335,20.6915190840625,
15.7719980632418));
#208922=CARTESIAN_POINT('Ctrl Pts',(-18.5786770662948,21.7049301280798,
15.8991738699232));
#208923=CARTESIAN_POINT('Ctrl Pts',(-16.5529260772022,20.4303150703447,
16.0263496766046));
#208924=CARTESIAN_POINT('Ctrl Pts',(-16.5281750395616,18.0370541147968,
16.153525483286));
#208925=CARTESIAN_POINT('Ctrl Pts',(-18.5271314941859,16.7208156456237,
16.2807012899675));
#208926=CARTESIAN_POINT('Ctrl Pts',(-20.7158769631869,17.689166763319,16.4078770966489));
#208927=CARTESIAN_POINT('Ctrl Pts',(-21.0863733276212,20.0537054200458,
16.5350529033304));
#208928=CARTESIAN_POINT('Ctrl Pts',(-19.2987131687179,21.6451141580778,
16.6622287100118));
#208929=CARTESIAN_POINT('Ctrl Pts',(-16.9929637275681,21.0033742342365,
16.7894045166932));
#208930=CARTESIAN_POINT('Ctrl Pts',(-16.2845070054764,18.7172421977746,
16.9165803233747));
#208931=CARTESIAN_POINT('Ctrl Pts',(-17.8233080731787,16.884102298789,17.0437561300561));
#208932=CARTESIAN_POINT('Ctrl Pts',(-20.1976124598239,17.1857466171053,
17.1709319367376));
#208933=CARTESIAN_POINT('Ctrl Pts',(-21.2291432566148,19.3454352128261,
17.2981077434189));
#208934=CARTESIAN_POINT('Ctrl Pts',(-19.9715349815179,21.3817878447692,
17.4252835501004));
#208935=CARTESIAN_POINT('Ctrl Pts',(-17.5785651709616,21.4265773634257,
17.5524593567818));
#208936=CARTESIAN_POINT('Ctrl Pts',(-16.245635101675,19.4387121653785,17.6796351634633));
#208937=CARTESIAN_POINT('Ctrl Pts',(-17.195625381257,17.2419351890085,17.8068109701447));
#208938=CARTESIAN_POINT('Ctrl Pts',(-19.5569788912398,16.8516529627759,
17.9339867768261));
#208939=CARTESIAN_POINT('Ctrl Pts',(-21.1633003483382,18.6259252056079,
18.0611625835076));
#208940=CARTESIAN_POINT('Ctrl Pts',(-20.5408895152254,20.9369672584502,
18.188338390189));
#208941=CARTESIAN_POINT('Ctrl Pts',(-18.2607697000954,21.6645414772881,
18.3155141968704));
#208942=CARTESIAN_POINT('Ctrl Pts',(-16.4148093131604,20.1411436746453,
18.4426900035519));
#208943=CARTESIAN_POINT('Ctrl Pts',(-16.696562436159,17.7643967817956,18.5698658102333));
#208944=CARTESIAN_POINT('Ctrl Pts',(-18.8475380664095,16.7148185552248,
18.6970416169147));
#208945=CARTESIAN_POINT('Ctrl Pts',(-20.8943495675715,17.9553318739381,
18.8242174235962));
#208946=CARTESIAN_POINT('Ctrl Pts',(-20.9591744271437,20.3478427623818,
18.9513932302776));
#208947=CARTESIAN_POINT('Ctrl Pts',(-18.9825398592484,21.6973709774882,
19.078569036959));
#208948=CARTESIAN_POINT('Ctrl Pts',(-16.77788539751,20.7658081409326,19.2057448436405));
#208949=CARTESIAN_POINT('Ctrl Pts',(-16.3678446716688,18.4078053400529,
19.3329206503219));
#208950=CARTESIAN_POINT('Ctrl Pts',(-18.1286046027284,16.7866837825795,
19.4600964570034));
#208951=CARTESIAN_POINT('Ctrl Pts',(-20.4447772293123,17.3897218945994,
19.5872722636848));
#208952=CARTESIAN_POINT('Ctrl Pts',(-21.1914179431377,19.6636696077008,
19.7144480703662));
#208953=CARTESIAN_POINT('Ctrl Pts',(-19.683530194942,21.5223210888799,19.8416238770476));
#208954=CARTESIAN_POINT('Ctrl Pts',(-17.3045074731465,21.260478855902,19.9687996837291));
#208955=CARTESIAN_POINT('Ctrl Pts',(-16.2369553322288,19.118367116143,20.0959754904105));
#208956=CARTESIAN_POINT('Ctrl Pts',(-17.4602868598788,17.0612400309757,
20.223151297092));
#208957=CARTESIAN_POINT('Ctrl Pts',(-19.8521708105233,16.9763848025611,
20.3503271037734));
#208958=CARTESIAN_POINT('Ctrl Pts',(-21.2182030751438,18.9416493308234,
20.4775029104549));
#208959=CARTESIAN_POINT('Ctrl Pts',(-20.305131989166,21.154028290157,20.6046787171362));
#208960=CARTESIAN_POINT('Ctrl Pts',(-17.9506471621875,21.5837957108187,
20.7318545238177));
#208961=CARTESIAN_POINT('Ctrl Pts',(-16.3148354273652,19.8366774312875,
20.8590303304991));
#208962=CARTESIAN_POINT('Ctrl Pts',(-16.8984657403956,17.5155252757358,
20.9862061371806));
#208963=CARTESIAN_POINT('Ctrl Pts',(-19.1660680401668,16.7498922826988,
21.113381943862));
#208964=CARTESIAN_POINT('Ctrl Pts',(-21.0373070469929,18.2421221167019,
21.2405577505435));
#208965=CARTESIAN_POINT('Ctrl Pts',(-20.7953425225475,20.6233350697589,
21.3677335572248));
#208966=CARTESIAN_POINT('Ctrl Pts',(-18.6623441810672,21.7086297969706,
21.4949093639063));
#208967=CARTESIAN_POINT('Ctrl Pts',(-16.5948543422637,20.502867400276,21.6220851705877));
#208968=CARTESIAN_POINT('Ctrl Pts',(-16.4903436183303,18.1111966683195,
21.7492609772692));
#208969=CARTESIAN_POINT('Ctrl Pts',(-18.4433885098624,16.7298792897364,
21.8764367839506));
#208970=CARTESIAN_POINT('Ctrl Pts',(-20.6647168984764,17.6222041838633,
22.003612590632));
#208971=CARTESIAN_POINT('Ctrl Pts',(-21.1114420608105,19.9774734447106,
22.1307883973135));
#208972=CARTESIAN_POINT('Ctrl Pts',(-19.9599075668543,21.0705044715179,
22.2155722684344));
#208973=CARTESIAN_POINT('Ctrl Pts',(-19.2802415985968,21.2523731445725,
22.2579642039949));
#208974=CARTESIAN_POINT('Ctrl Pts',(-17.0028273852109,20.6688092100886,
-0.0844763361257089));
#208975=CARTESIAN_POINT('Ctrl Pts',(-16.5172190142843,20.092181868941,-0.0420657430668533));
#208976=CARTESIAN_POINT('Ctrl Pts',(-16.1763706746349,18.4257326299315,
0.0427367855524802));
#208977=CARTESIAN_POINT('Ctrl Pts',(-18.01364439973,16.6318023132686,0.169931249732293));
#208978=CARTESIAN_POINT('Ctrl Pts',(-20.5111535200096,17.2110802832593,
0.297107056413727));
#208979=CARTESIAN_POINT('Ctrl Pts',(-21.3783870101994,19.6218281451444,
0.424282863095161));
#208980=CARTESIAN_POINT('Ctrl Pts',(-19.8194850134989,21.6573811366705,
0.551458669776596));
#208981=CARTESIAN_POINT('Ctrl Pts',(-17.2647560862599,21.4476431456228,
0.678634476458029));
#208982=CARTESIAN_POINT('Ctrl Pts',(-16.057947487624,19.1863846079818,0.805810283139464));
#208983=CARTESIAN_POINT('Ctrl Pts',(-17.3062612289062,16.947470098725,0.932986089820897));
#208984=CARTESIAN_POINT('Ctrl Pts',(-19.8644313564053,16.7853278416859,
1.06016189650233));
#208985=CARTESIAN_POINT('Ctrl Pts',(-21.3855036379843,18.848524857474,1.18733770318377));
#208986=CARTESIAN_POINT('Ctrl Pts',(-20.4739844697589,21.2443037270014,
1.3145135098652));
#208987=CARTESIAN_POINT('Ctrl Pts',(-17.9661382896929,21.774635291315,1.44168931654664));
#208988=CARTESIAN_POINT('Ctrl Pts',(-16.1627571841069,19.9529995896776,
1.56886512322807));
#208989=CARTESIAN_POINT('Ctrl Pts',(-16.7183319730092,17.4506206494911,
1.69604092990951));
#208990=CARTESIAN_POINT('Ctrl Pts',(-19.1231569662995,16.5632829246964,
1.82321673659094));
#208991=CARTESIAN_POINT('Ctrl Pts',(-21.1709546507375,18.1050600233756,
1.95039254327237));
#208992=CARTESIAN_POINT('Ctrl Pts',(-20.9829976696055,20.6614690606707,
2.07756834995381));
#208993=CARTESIAN_POINT('Ctrl Pts',(-18.7317249296694,21.8871624224886,
2.20474415663524));
#208994=CARTESIAN_POINT('Ctrl Pts',(-16.4825394180193,20.6576430387449,
2.33191996331668));
#208995=CARTESIAN_POINT('Ctrl Pts',(-16.2989292528432,18.1009183645693,
2.45909576999811));
#208996=CARTESIAN_POINT('Ctrl Pts',(-18.3493453586185,16.5626247387795,
2.58627157667954));
#208997=CARTESIAN_POINT('Ctrl Pts',(-20.7526582245547,17.4540510138992,
2.71344738336098));
#208998=CARTESIAN_POINT('Ctrl Pts',(-21.3039774609752,19.9573689479556,
2.84062319004241));
#208999=CARTESIAN_POINT('Ctrl Pts',(-19.4975018880252,21.7759396905319,
2.96779899672385));
#209000=CARTESIAN_POINT('Ctrl Pts',(-16.9905607209365,21.2413374685879,
3.09497480340528));
#209001=CARTESIAN_POINT('Ctrl Pts',(-16.0831168824194,18.8440266343892,
3.22215061008672));
#209002=CARTESIAN_POINT('Ctrl Pts',(-17.6076937718807,16.7833910871266,
3.34932641676815));
#209003=CARTESIAN_POINT('Ctrl Pts',(-20.1655867192137,16.9499360425438,
3.47650222344959));
#209004=CARTESIAN_POINT('Ctrl Pts',(-21.4100877059499,19.1908668417195,
3.60367803013102));
#209005=CARTESIAN_POINT('Ctrl Pts',(-20.1994443192179,21.4502685638837,
3.73085383681246));
#209006=CARTESIAN_POINT('Ctrl Pts',(-17.6443467253329,21.6552803634332,
3.85802964349388));
#209007=CARTESIAN_POINT('Ctrl Pts',(-16.0889383794468,19.6178166386469,
3.98520545017533));
#209008=CARTESIAN_POINT('Ctrl Pts',(-16.9602098993781,17.2071238978084,
4.11238125685675));
#209009=CARTESIAN_POINT('Ctrl Pts',(-19.4588237428005,16.6348631061435,
4.23955706353819));
#209010=CARTESIAN_POINT('Ctrl Pts',(-21.2924567898383,18.4260480215086,
4.36673287021963));
#209011=CARTESIAN_POINT('Ctrl Pts',(-20.7788645279368,20.9373776575228,
4.49390867690106));
#209012=CARTESIAN_POINT('Ctrl Pts',(-18.3892359802594,21.8648629438428,
4.62108448358249));
#209013=CARTESIAN_POINT('Ctrl Pts',(-16.3159070222257,20.3575936964975,
4.74826029026393));
#209014=CARTESIAN_POINT('Ctrl Pts',(-16.4610282875234,17.7983958982468,
4.87543609694536));
#209015=CARTESIAN_POINT('Ctrl Pts',(-18.6914600224833,16.535174687256,5.0026119036268));
#209016=CARTESIAN_POINT('Ctrl Pts',(-20.9609195464861,17.7268571202586,
5.12978771030823));
#209017=CARTESIAN_POINT('Ctrl Pts',(-21.1873186048029,20.280148529128,5.25696351698966));
#209018=CARTESIAN_POINT('Ctrl Pts',(-19.1629501133386,21.8525625213641,
5.38413932367111));
#209019=CARTESIAN_POINT('Ctrl Pts',(-16.7450465165327,21.0015068541093,
5.51131513035253));
#209020=CARTESIAN_POINT('Ctrl Pts',(-16.1518842924324,18.5077722795978,
5.63849093703398));
#209021=CARTESIAN_POINT('Ctrl Pts',(-17.9276529658501,16.6592054913206,
5.7656667437154));
#209022=CARTESIAN_POINT('Ctrl Pts',(-20.4431949955591,17.1517517825272,
5.89284255039684));
#209023=CARTESIAN_POINT('Ctrl Pts',(-21.390656701448,19.5335305019064,6.02001835707826));
#209024=CARTESIAN_POINT('Ctrl Pts',(-19.9008007744695,21.6194075042871,
6.14719416375971));
#209025=CARTESIAN_POINT('Ctrl Pts',(-17.3404775567387,21.4957201041125,
6.27436997044113));
#209026=CARTESIAN_POINT('Ctrl Pts',(-16.0586246889428,19.2759438141371,
6.40154577712258));
#209027=CARTESIAN_POINT('Ctrl Pts',(-17.2312626165228,16.9965856055586,
6.528721583804));
#209028=CARTESIAN_POINT('Ctrl Pts',(-19.7825688230421,16.7488151618222,
6.65589739048545));
#209029=CARTESIAN_POINT('Ctrl Pts',(-21.3718782159412,18.7599464866879,
6.78307319716687));
#209030=CARTESIAN_POINT('Ctrl Pts',(-20.5410980709011,21.1848914144791,
6.91024900384832));
#209031=CARTESIAN_POINT('Ctrl Pts',(-18.0524176069647,21.7989134830039,
7.03742481052974));
#209032=CARTESIAN_POINT('Ctrl Pts',(-16.189046684864,20.0386855548983,7.16460061721119));
#209033=CARTESIAN_POINT('Ctrl Pts',(-16.6605124717835,17.5191075021328,
7.2917764238926));
#209034=CARTESIAN_POINT('Ctrl Pts',(-19.0342743706913,16.551735805469,7.41895223057406));
#209035=CARTESIAN_POINT('Ctrl Pts',(-21.1325531716193,18.024073954737,7.54612803725548));
#209036=CARTESIAN_POINT('Ctrl Pts',(-21.0303083085858,20.5853430815951,
7.67330384393691));
#209037=CARTESIAN_POINT('Ctrl Pts',(-18.8213430973923,21.8857377324416,
7.80047965061835));
#209038=CARTESIAN_POINT('Ctrl Pts',(-16.5322460154652,20.7322265267193,
7.92765545729978));
#209039=CARTESIAN_POINT('Ctrl Pts',(-16.2631215580847,18.1830844006987,
8.05483126398122));
#209040=CARTESIAN_POINT('Ctrl Pts',(-18.2608747111494,16.5769910373997,
8.18200707066265));
#209041=CARTESIAN_POINT('Ctrl Pts',(-20.6926909512673,17.3874374122526,
8.30918287734408));
#209042=CARTESIAN_POINT('Ctrl Pts',(-21.3275298136684,19.8708892783048,
8.43635868402552));
#209043=CARTESIAN_POINT('Ctrl Pts',(-19.5829660446433,21.7489336888602,
8.56353449070696));
#209044=CARTESIAN_POINT('Ctrl Pts',(-17.0595286224332,21.2985814618163,
8.69071029738838));
#209045=CARTESIAN_POINT('Ctrl Pts',(-16.0723147597259,18.9330028134741,
8.81788610406983));
#209046=CARTESIAN_POINT('Ctrl Pts',(-17.5270319021526,16.8224693293182,
8.94506191075126));
#209047=CARTESIAN_POINT('Ctrl Pts',(-20.0890673614655,16.90326448658,9.07223771743269));
#209048=CARTESIAN_POINT('Ctrl Pts',(-21.4079126215994,19.1012637431849,
9.19941352411413));
#209049=CARTESIAN_POINT('Ctrl Pts',(-20.2736090131502,21.3999392044174,
9.32658933079555));
#209050=CARTESIAN_POINT('Ctrl Pts',(-17.726809694048,21.6903988064862,9.453765137477));
#209051=CARTESIAN_POINT('Ctrl Pts',(-16.1040449673761,19.7061638924493,
9.58094094415843));
#209052=CARTESIAN_POINT('Ctrl Pts',(-16.894100749718,17.2676468404274,9.70811675083986));
#209053=CARTESIAN_POINT('Ctrl Pts',(-19.3721498971671,16.6120356942131,
9.83529255752129));
#209054=CARTESIAN_POINT('Ctrl Pts',(-21.2647361220149,18.3408129886411,
9.96246836420274));
#209055=CARTESIAN_POINT('Ctrl Pts',(-20.8355290301125,20.8679328560937,
10.0896441708842));
#209056=CARTESIAN_POINT('Ctrl Pts',(-18.4782994886839,21.8749196689318,
10.2168199775656));
#209057=CARTESIAN_POINT('Ctrl Pts',(-16.3556592958241,20.4379255270265,
10.3439957842471));
#209058=CARTESIAN_POINT('Ctrl Pts',(-16.4149990825736,17.875303365661,10.4711715909285));
#209059=CARTESIAN_POINT('Ctrl Pts',(-18.6018782776321,16.5380999636187,
10.59834739761));
#209060=CARTESIAN_POINT('Ctrl Pts',(-20.9099709525642,17.65311644607,10.7255232042914));
#209061=CARTESIAN_POINT('Ctrl Pts',(-21.2217453345073,20.1973943960938,
10.8526990109728));
#209062=CARTESIAN_POINT('Ctrl Pts',(-19.2511677789294,21.8367167102424,
10.9798748176543));
#209063=CARTESIAN_POINT('Ctrl Pts',(-16.806120885236,21.0671069131022,11.1070506243357));
#209064=CARTESIAN_POINT('Ctrl Pts',(-16.1297834216659,18.5946342261783,
11.2342264310171));
#209065=CARTESIAN_POINT('Ctrl Pts',(-17.8426530328072,16.6876388807614,
11.3614022376985));
#209066=CARTESIAN_POINT('Ctrl Pts',(-20.3732781631159,17.0956707447917,
11.48857804438));
#209067=CARTESIAN_POINT('Ctrl Pts',(-21.3999673238431,19.4443859083351,
11.6157538510614));
#209068=CARTESIAN_POINT('Ctrl Pts',(-19.9807969335377,21.5789839865442,
11.7429296577429));
#209069=CARTESIAN_POINT('Ctrl Pts',(-17.4177677416566,21.5411037307608,
11.8701054644243));
#209070=CARTESIAN_POINT('Ctrl Pts',(-16.062299952218,19.3654979245523,11.9972812711057));
#209071=CARTESIAN_POINT('Ctrl Pts',(-17.157951132213,17.0481498617898,12.1244570777871));
#209072=CARTESIAN_POINT('Ctrl Pts',(-19.6995293277776,16.7150825592159,
12.2516328844686));
#209073=CARTESIAN_POINT('Ctrl Pts',(-21.3552942926149,18.671864594454,12.37880869115));
#209074=CARTESIAN_POINT('Ctrl Pts',(-20.6061844398505,21.1232699017635,
12.5059844978315));
#209075=CARTESIAN_POINT('Ctrl Pts',(-18.1394615643946,21.8202862630607,
12.6331603045129));
#209076=CARTESIAN_POINT('Ctrl Pts',(-16.2181908023896,20.1234444285697,
12.7603361111943));
#209077=CARTESIAN_POINT('Ctrl Pts',(-16.605018830463,17.5894914635544,12.8875119178758));
#209078=CARTESIAN_POINT('Ctrl Pts',(-18.9450549421127,16.5431719385577,
13.0146877245572));
#209079=CARTESIAN_POINT('Ctrl Pts',(-21.091461243921,17.9444190758505,13.1418635312386));
#209080=CARTESIAN_POINT('Ctrl Pts',(-21.0750431749784,20.5076755981723,
13.2690393379201));
#209081=CARTESIAN_POINT('Ctrl Pts',(-18.9108632945195,21.8813127399352,
13.3962151446015));
#209082=CARTESIAN_POINT('Ctrl Pts',(-16.584422318713,20.8051036811079,13.5233909512829));
#209083=CARTESIAN_POINT('Ctrl Pts',(-16.2300854476496,18.2664034360971,
13.6505667579644));
#209084=CARTESIAN_POINT('Ctrl Pts',(-18.1729347679036,16.5943119101923,
13.7777425646458));
#209085=CARTESIAN_POINT('Ctrl Pts',(-20.6305266149702,17.3228692967068,
13.9049183713272));
#209086=CARTESIAN_POINT('Ctrl Pts',(-21.3481730045189,19.7836694128848,
14.0320941780087));
#209087=CARTESIAN_POINT('Ctrl Pts',(-19.6674779162968,21.7190808866133,
14.1592699846901));
#209088=CARTESIAN_POINT('Ctrl Pts',(-17.1303747780463,21.3534838159302,
14.2864457913715));
#209089=CARTESIAN_POINT('Ctrl Pts',(-16.0644982487317,19.0222908216738,
14.413621598053));
#209090=CARTESIAN_POINT('Ctrl Pts',(-17.447723888241,16.8642267859192,14.5407974047344));
#209091=CARTESIAN_POINT('Ctrl Pts',(-20.0110280249899,16.859181516911,14.6679732114158));
#209092=CARTESIAN_POINT('Ctrl Pts',(-21.4027382101088,19.0117837358195,
14.7951490180973));
#209093=CARTESIAN_POINT('Ctrl Pts',(-20.3460467280269,21.3471545123578,
14.9223248247787));
#209094=CARTESIAN_POINT('Ctrl Pts',(-17.8104024278843,21.7227361085096,
15.0495006314601));
#209095=CARTESIAN_POINT('Ctrl Pts',(-16.1221015752275,19.7939557210286,
15.1766764381416));
#209096=CARTESIAN_POINT('Ctrl Pts',(-16.8300554146003,17.3303496418165,
15.303852244823));
#209097=CARTESIAN_POINT('Ctrl Pts',(-19.284760238949,16.5921235399122,15.4310280515045));
#209098=CARTESIAN_POINT('Ctrl Pts',(-21.2341767280976,18.2565540443337,
15.5582038581859));
#209099=CARTESIAN_POINT('Ctrl Pts',(-20.8898362476853,20.7966294734819,
15.6853796648673));
#209100=CARTESIAN_POINT('Ctrl Pts',(-18.5676498163098,21.8819882759749,
15.8125554715487));
#209101=CARTESIAN_POINT('Ctrl Pts',(-16.3980793536131,20.5168811154897,
15.9397312782302));
#209102=CARTESIAN_POINT('Ctrl Pts',(-16.3715711003901,17.9537090836658,
16.0669070849116));
#209103=CARTESIAN_POINT('Ctrl Pts',(-18.5124447336848,16.5440234313033,
16.1940828915931));
#209104=CARTESIAN_POINT('Ctrl Pts',(-20.8565815725531,17.5811232494858,
16.3212586982745));
#209105=CARTESIAN_POINT('Ctrl Pts',(-21.253381560874,20.1135338247049,16.4484345049559));
#209106=CARTESIAN_POINT('Ctrl Pts',(-19.338805337548,21.8179256333241,16.5756103116374));
#209107=CARTESIAN_POINT('Ctrl Pts',(-16.8693577554744,21.1306249774212,
16.7027861183188));
#209108=CARTESIAN_POINT('Ctrl Pts',(-16.1106037000031,18.6821875500976,
16.8299619250002));
#209109=CARTESIAN_POINT('Ctrl Pts',(-17.7586529234411,16.7189027237572,
16.9571377316817));
#209110=CARTESIAN_POINT('Ctrl Pts',(-20.3015225527551,17.0419624713682,
17.0843135383631));
#209111=CARTESIAN_POINT('Ctrl Pts',(-21.4062875313382,19.354979525847,17.2114893450445));
#209112=CARTESIAN_POINT('Ctrl Pts',(-20.0593945607884,21.5359043017382,
17.338665151726));
#209113=CARTESIAN_POINT('Ctrl Pts',(-17.4965343439791,21.5838736806199,
17.4658409584074));
#209114=CARTESIAN_POINT('Ctrl Pts',(-16.0689720607886,19.4548787346826,
17.5930167650888));
#209115=CARTESIAN_POINT('Ctrl Pts',(-17.0864075015351,17.1021401864965,
17.7201925717703));
#209116=CARTESIAN_POINT('Ctrl Pts',(-19.6154067985012,16.6841496265959,
17.8473683784517));
#209117=CARTESIAN_POINT('Ctrl Pts',(-21.3357700641153,18.584387450276,17.9745441851331));
#209118=CARTESIAN_POINT('Ctrl Pts',(-20.6691707799709,21.0595033963588,
18.1017199918146));
#209119=CARTESIAN_POINT('Ctrl Pts',(-18.2271724154379,21.8387322073577,
18.228895798496));
#209120=CARTESIAN_POINT('Ctrl Pts',(-16.2501569024917,20.207179813531,18.3560716051774));
#209121=CARTESIAN_POINT('Ctrl Pts',(-16.5519132667841,17.6616942707386,
18.4832474118589));
#209122=CARTESIAN_POINT('Ctrl Pts',(-18.8555987732945,16.537600573676,18.6104232185403));
#209123=CARTESIAN_POINT('Ctrl Pts',(-21.0477249524445,17.8661849205939,
18.7375990252217));
#209124=CARTESIAN_POINT('Ctrl Pts',(-21.1171520939507,20.4285536338248,
18.8647748319032));
#209125=CARTESIAN_POINT('Ctrl Pts',(-19.0001851038609,21.8738924587027,
18.9919506385846));
#209126=CARTESIAN_POINT('Ctrl Pts',(-16.639009803247,20.8761927289634,19.119126445266));
#209127=CARTESIAN_POINT('Ctrl Pts',(-16.1998579765528,18.3507820268139,
19.2463022519475));
#209128=CARTESIAN_POINT('Ctrl Pts',(-18.0856241733337,16.6145679183314,
19.3734780586289));
#209129=CARTESIAN_POINT('Ctrl Pts',(-20.5662349414884,17.2604191027876,
19.5006538653103));
#209130=CARTESIAN_POINT('Ctrl Pts',(-21.3658838853536,19.695807173002,19.6278296719918));
#209131=CARTESIAN_POINT('Ctrl Pts',(-19.7509426921062,21.6864147924606,
19.7550054786732));
#209132=CARTESIAN_POINT('Ctrl Pts',(-17.2030197464517,21.4059829044279,
19.8821812853547));
#209133=CARTESIAN_POINT('Ctrl Pts',(-16.059676065617,19.1117905859247,20.0093570920361));
#209134=CARTESIAN_POINT('Ctrl Pts',(-17.3698587893405,16.908616461354,20.1365328987175));
#209135=CARTESIAN_POINT('Ctrl Pts',(-19.9315560549264,16.8177368822917,
20.2637087053989));
#209136=CARTESIAN_POINT('Ctrl Pts',(-21.3945706447594,18.9225266095884,
20.3908845120804));
#209137=CARTESIAN_POINT('Ctrl Pts',(-20.4166754991338,21.2919748133934,
20.5180603187618));
#209138=CARTESIAN_POINT('Ctrl Pts',(-17.8950325316693,21.7522538440923,
20.6452361254433));
#209139=CARTESIAN_POINT('Ctrl Pts',(-16.1430853073993,19.881097796524,20.7724119321247));
#209140=CARTESIAN_POINT('Ctrl Pts',(-16.7681508238931,17.395153974591,20.8995877388061));
#209141=CARTESIAN_POINT('Ctrl Pts',(-19.1967429841419,16.5751643826307,
21.0267635454876));
#209142=CARTESIAN_POINT('Ctrl Pts',(-21.2008317885977,18.1733360181572,
21.153939352169));
#209143=CARTESIAN_POINT('Ctrl Pts',(-20.9416888395956,20.7236046919281,
21.2811151588505));
#209144=CARTESIAN_POINT('Ctrl Pts',(-18.6572569308498,21.8859506052002,
21.4082909655318));
#209145=CARTESIAN_POINT('Ctrl Pts',(-16.4429843423898,20.5945843440041,
21.5354667722133));
#209146=CARTESIAN_POINT('Ctrl Pts',(-16.3310538134642,18.033115434702,21.6626425788947));
#209147=CARTESIAN_POINT('Ctrl Pts',(-18.4227563631869,16.5537305545665,
21.7898183855762));
#209148=CARTESIAN_POINT('Ctrl Pts',(-20.8017893666684,17.50940661932,21.9169941922576));
#209149=CARTESIAN_POINT('Ctrl Pts',(-21.2802300646426,20.0318897120323,
22.0441699989391));
#209150=CARTESIAN_POINT('Ctrl Pts',(-20.0469416504615,21.2025211683863,
22.12895387006));
#209151=CARTESIAN_POINT('Ctrl Pts',(-19.3190223666151,21.3973017229923,
22.1713458056205));
#209152=CARTESIAN_POINT('Ctrl Pts',(-16.8880690316762,20.7654464739225,
-0.171094734500184));
#209153=CARTESIAN_POINT('Ctrl Pts',(-16.3702699845374,20.1505948657621,
-0.128684141441329));
#209154=CARTESIAN_POINT('Ctrl Pts',(-16.006827020915,18.3736777454539,-0.0438816128219947));
#209155=CARTESIAN_POINT('Ctrl Pts',(-17.9658924760107,16.4608289063181,
0.0833128513578173));
#209156=CARTESIAN_POINT('Ctrl Pts',(-20.6289599190898,17.0785068518555,
0.210488658039252));
#209157=CARTESIAN_POINT('Ctrl Pts',(-21.5536817767679,19.6490616868026,
0.337664464720685));
#209158=CARTESIAN_POINT('Ctrl Pts',(-19.8914411384235,21.8195502173065,
0.46484027140212));
#209159=CARTESIAN_POINT('Ctrl Pts',(-17.1673608230486,21.5959088255693,
0.592016078083554));
#209160=CARTESIAN_POINT('Ctrl Pts',(-15.8805536346544,19.1847528689885,
0.719191884764988));
#209161=CARTESIAN_POINT('Ctrl Pts',(-17.2116173157294,16.7974221125058,
0.846367691446423));
#209162=CARTESIAN_POINT('Ctrl Pts',(-19.9393669463845,16.6245315463164,
0.973543498127856));
#209163=CARTESIAN_POINT('Ctrl Pts',(-21.5612701613726,18.8244966062191,
1.10071930480929));
#209164=CARTESIAN_POINT('Ctrl Pts',(-20.5893269556668,21.3790901636359,
1.22789511149073));
#209165=CARTESIAN_POINT('Ctrl Pts',(-17.9152372155514,21.9445770767739,
1.35507091817216));
#209166=CARTESIAN_POINT('Ctrl Pts',(-15.9923111005858,20.0021862799634,
1.4822467248536));
#209167=CARTESIAN_POINT('Ctrl Pts',(-16.5847145959355,17.3339261996511,
1.60942253153503));
#209168=CARTESIAN_POINT('Ctrl Pts',(-19.1489539390206,16.3877674101879,
1.73659833821646));
#209169=CARTESIAN_POINT('Ctrl Pts',(-21.332498855497,18.0317479516957,1.8637741448979));
#209170=CARTESIAN_POINT('Ctrl Pts',(-21.1320823232458,20.7576197505752,
1.99094995157933));
#209171=CARTESIAN_POINT('Ctrl Pts',(-18.7315741166753,22.064563561331,2.11812575826077));
#209172=CARTESIAN_POINT('Ctrl Pts',(-16.3332914994529,20.7535401040407,
2.2453015649422));
#209173=CARTESIAN_POINT('Ctrl Pts',(-16.1375099308779,18.0273317449088,
2.37247737162363));
#209174=CARTESIAN_POINT('Ctrl Pts',(-18.3238468422098,16.387065593537,2.49965317830507));
#209175=CARTESIAN_POINT('Ctrl Pts',(-20.8864738199611,17.3375839607775,
2.62682898498651));
#209176=CARTESIAN_POINT('Ctrl Pts',(-21.4743396649076,20.006845280278,2.75400479166794));
#209177=CARTESIAN_POINT('Ctrl Pts',(-19.5481139522653,21.9459679438018,
2.88118059834937));
#209178=CARTESIAN_POINT('Ctrl Pts',(-16.8749892178732,21.3759272738012,
3.00835640503081));
#209179=CARTESIAN_POINT('Ctrl Pts',(-15.9073914929419,18.8197001987301,
3.13553221171224));
#209180=CARTESIAN_POINT('Ctrl Pts',(-17.5330316340844,16.6224664055047,
3.26270801839368));
#209181=CARTESIAN_POINT('Ctrl Pts',(-20.2604857104729,16.8000515222033,
3.38988382507511));
#209182=CARTESIAN_POINT('Ctrl Pts',(-21.5874838918795,19.1895322272068,
3.51705963175655));
#209183=CARTESIAN_POINT('Ctrl Pts',(-20.2965877096769,21.5987082811702,
3.64423543843798));
#209184=CARTESIAN_POINT('Ctrl Pts',(-17.5721142889738,21.8173101851209,
3.77141124511941));
#209185=CARTESIAN_POINT('Ctrl Pts',(-15.9135988933785,19.64478426004,3.89858705180085));
#209186=CARTESIAN_POINT('Ctrl Pts',(-16.8426264592725,17.0742882000792,
4.02576285848228));
#209187=CARTESIAN_POINT('Ctrl Pts',(-19.5068718569032,16.4640925972449,
4.15293866516372));
#209188=CARTESIAN_POINT('Ctrl Pts',(-21.4620552956622,18.3740140441421,
4.28011447184515));
#209189=CARTESIAN_POINT('Ctrl Pts',(-20.914417322859,21.0518181563291,4.40729027852659));
#209190=CARTESIAN_POINT('Ctrl Pts',(-18.3663817882941,22.0407858641459,
4.53446608520802));
#209191=CARTESIAN_POINT('Ctrl Pts',(-16.15561314601,20.4336006779268,4.66164189188945));
#209192=CARTESIAN_POINT('Ctrl Pts',(-16.3103544095251,17.7047552528665,
4.78881769857089));
#209193=CARTESIAN_POINT('Ctrl Pts',(-18.6886400738904,16.3577958952085,
4.91599350525232));
#209194=CARTESIAN_POINT('Ctrl Pts',(-21.1085406551067,17.628474213878,5.04316931193375));
#209195=CARTESIAN_POINT('Ctrl Pts',(-21.3499475658771,20.3510217186868,
5.1703451186152));
#209196=CARTESIAN_POINT('Ctrl Pts',(-19.1913849489723,22.0276700543283,
5.29752092529662));
#209197=CARTESIAN_POINT('Ctrl Pts',(-16.613200029897,21.1201984373834,5.42469673197806));
#209198=CARTESIAN_POINT('Ctrl Pts',(-15.9807174516997,18.4611557523585,
5.5518725386595));
#209199=CARTESIAN_POINT('Ctrl Pts',(-17.8742007235803,16.4900486239617,
5.67904834534092));
#209200=CARTESIAN_POINT('Ctrl Pts',(-20.5564964664144,17.0152455017915,
5.80622415202237));
#209201=CARTESIAN_POINT('Ctrl Pts',(-21.5667648182011,19.5549108478334,
5.93339995870379));
#209202=CARTESIAN_POINT('Ctrl Pts',(-19.9781472705018,21.7790593365027,
6.06057576538524));
#209203=CARTESIAN_POINT('Ctrl Pts',(-17.2481018226055,21.6471727756692,
6.18775157206665));
#209204=CARTESIAN_POINT('Ctrl Pts',(-15.8812757272267,19.2802488990946,
6.31492737874811));
#209205=CARTESIAN_POINT('Ctrl Pts',(-17.1316470920802,16.849793455672,6.44210318542952));
#209206=CARTESIAN_POINT('Ctrl Pts',(-19.8520777967125,16.5855984636642,
6.56927899211098));
#209207=CARTESIAN_POINT('Ctrl Pts',(-21.5467415185955,18.7300464304477,
6.6964547987924));
#209208=CARTESIAN_POINT('Ctrl Pts',(-20.6608894755945,21.3157394459503,
6.82363060547384));
#209209=CARTESIAN_POINT('Ctrl Pts',(-18.0072359349844,21.9704646546564,
6.95080641215527));
#209210=CARTESIAN_POINT('Ctrl Pts',(-16.020343315961,20.0935523144076,7.07798221883671));
#209211=CARTESIAN_POINT('Ctrl Pts',(-16.5230622760143,17.4069530030642,
7.20515802551813));
#209212=CARTESIAN_POINT('Ctrl Pts',(-19.0541793715532,16.3754548396247,
7.33233383219958));
#209213=CARTESIAN_POINT('Ctrl Pts',(-21.291551766265,17.9453933670485,7.459509638881));
#209214=CARTESIAN_POINT('Ctrl Pts',(-21.1825291549937,20.6764474277986,
7.58668544556244));
#209215=CARTESIAN_POINT('Ctrl Pts',(-18.8271330168744,22.0630444294688,
7.71386125224388));
#209216=CARTESIAN_POINT('Ctrl Pts',(-16.3862931162597,20.8330676849425,
7.84103705892531));
#209217=CARTESIAN_POINT('Ctrl Pts',(-16.099328566354,18.1149445163563,7.96821286560675));
#209218=CARTESIAN_POINT('Ctrl Pts',(-18.2295115306668,16.4023842251376,
8.09538867228817));
#209219=CARTESIAN_POINT('Ctrl Pts',(-20.8225313535071,17.2665545850003,
8.22256447896962));
#209220=CARTESIAN_POINT('Ctrl Pts',(-21.4994532883798,19.9146329272319,
8.34974028565105));
#209221=CARTESIAN_POINT('Ctrl Pts',(-19.6392434745528,21.917171731113,8.47691609233248));
#209222=CARTESIAN_POINT('Ctrl Pts',(-16.9485289585702,21.4369659356584,
8.60409189901392));
#209223=CARTESIAN_POINT('Ctrl Pts',(-15.8958733042685,18.9145745532646,
8.73126770569535));
#209224=CARTESIAN_POINT('Ctrl Pts',(-17.4470227392911,16.6641351200123,
8.85844351237678));
#209225=CARTESIAN_POINT('Ctrl Pts',(-20.1788939321968,16.7502861378866,
8.98561931905823));
#209226=CARTESIAN_POINT('Ctrl Pts',(-21.5851646225432,19.093989395123,9.11279512573965));
#209227=CARTESIAN_POINT('Ctrl Pts',(-20.3756687349404,21.5450426198368,
9.23997093242109));
#209228=CARTESIAN_POINT('Ctrl Pts',(-17.6600436764829,21.8547566078734,
9.36714673910252));
#209229=CARTESIAN_POINT('Ctrl Pts',(-15.9297068876053,19.738987998227,9.49432254578396));
#209230=CARTESIAN_POINT('Ctrl Pts',(-16.7721349752896,17.1388231708385,
9.62149835246539));
#209231=CARTESIAN_POINT('Ctrl Pts',(-19.4144524560694,16.4397519704066,
9.74867415914682));
#209232=CARTESIAN_POINT('Ctrl Pts',(-21.432497042048,18.2831288340757,9.87584996582827));
#209233=CARTESIAN_POINT('Ctrl Pts',(-20.974838079563,20.9777699023008,10.0030257725097));
#209234=CARTESIAN_POINT('Ctrl Pts',(-18.4613492611758,22.0515092432722,
10.1302015791911));
#209235=CARTESIAN_POINT('Ctrl Pts',(-16.1980005730462,20.5192576554282,
10.2573773858725));
#209236=CARTESIAN_POINT('Ctrl Pts',(-16.2612739572708,17.7867608683564,
10.384553192554));
#209237=CARTESIAN_POINT('Ctrl Pts',(-18.5931200110123,16.3609150863178,
10.5117289992354));
#209238=CARTESIAN_POINT('Ctrl Pts',(-21.0542147106519,17.5498453163626,
10.6389048059168));
#209239=CARTESIAN_POINT('Ctrl Pts',(-21.3866564220343,20.2627818657572,
10.7660806125983));
#209240=CARTESIAN_POINT('Ctrl Pts',(-19.2854505086261,22.0107738342645,
10.8932564192797));
#209241=CARTESIAN_POINT('Ctrl Pts',(-16.6783229804319,21.1901470833962,
11.0204322259611));
#209242=CARTESIAN_POINT('Ctrl Pts',(-15.9571515279862,18.5537757232337,
11.1476080326426));
#209243=CARTESIAN_POINT('Ctrl Pts',(-17.7835661979594,16.5203668450652,
11.274783839324));
#209244=CARTESIAN_POINT('Ctrl Pts',(-20.4819448907301,16.9554468870216,
11.4019596460055));
#209245=CARTESIAN_POINT('Ctrl Pts',(-21.5766926359512,19.4598569147211,
11.5291354526869));
#209246=CARTESIAN_POINT('Ctrl Pts',(-20.0634463250904,21.735956168966,11.6563112593683));
#209247=CARTESIAN_POINT('Ctrl Pts',(-17.330515525704,21.6955648546388,11.7834870660497));
#209248=CARTESIAN_POINT('Ctrl Pts',(-15.8851946214135,19.3757394956669,
11.9106628727312));
#209249=CARTESIAN_POINT('Ctrl Pts',(-17.053475835173,16.9047758743069,12.0378386794126));
#209250=CARTESIAN_POINT('Ctrl Pts',(-19.7635336650682,16.5496297478578,
12.165014486094));
#209251=CARTESIAN_POINT('Ctrl Pts',(-21.5290582573291,18.6361256444822,
12.2921902927755));
#209252=CARTESIAN_POINT('Ctrl Pts',(-20.7302903793709,21.2500330815674,
12.4193660994569));
#209253=CARTESIAN_POINT('Ctrl Pts',(-18.1000499820946,21.9932542229807,
12.5465419061383));
#209254=CARTESIAN_POINT('Ctrl Pts',(-16.0514193788707,20.1839298009815,
12.6737177128198));
#209255=CARTESIAN_POINT('Ctrl Pts',(-16.4638899958019,17.4820026734157,
12.8008935195012));
#209256=CARTESIAN_POINT('Ctrl Pts',(-18.9590456426674,16.3663232793141,
12.9280693261827));
#209257=CARTESIAN_POINT('Ctrl Pts',(-21.2477358802935,17.8604582158923,
13.0552451328641));
#209258=CARTESIAN_POINT('Ctrl Pts',(-21.2302294677946,20.5936314153126,
13.1824209395455));
#209259=CARTESIAN_POINT('Ctrl Pts',(-18.9225874520683,22.0583261069674,
13.309596746227));
#209260=CARTESIAN_POINT('Ctrl Pts',(-16.4419281541264,20.9107758204687,
13.4367725529084));
#209261=CARTESIAN_POINT('Ctrl Pts',(-16.0641025127507,18.2037867186756,
13.5639483595899));
#209262=CARTESIAN_POINT('Ctrl Pts',(-18.1357421033992,16.4208532877909,
13.6911241662712));
#209263=CARTESIAN_POINT('Ctrl Pts',(-20.756246182106,17.1977062893226,13.8182999729527));
#209264=CARTESIAN_POINT('Ctrl Pts',(-21.5214649034841,19.8216313113002,
13.9454757796341));
#209265=CARTESIAN_POINT('Ctrl Pts',(-19.7293575854992,21.8853400052135,
14.0726515863156));
#209266=CARTESIAN_POINT('Ctrl Pts',(-17.0240714616778,21.495507732604,14.199827392997));
#209267=CARTESIAN_POINT('Ctrl Pts',(-15.8875386416327,19.0097814078715,
14.3270031996784));
#209268=CARTESIAN_POINT('Ctrl Pts',(-17.3624574465728,16.7086606523826,
14.4541790063599));
#209269=CARTESIAN_POINT('Ctrl Pts',(-20.0956814167509,16.7032809356367,
14.5813548130413));
#209270=CARTESIAN_POINT('Ctrl Pts',(-21.5796472025402,18.9985778138453,
14.7085306197227));
#209271=CARTESIAN_POINT('Ctrl Pts',(-20.4529083007835,21.4887588634431,
14.8357064264042));
#209272=CARTESIAN_POINT('Ctrl Pts',(-17.749177720539,21.8892375294908,14.9628822330856));
#209273=CARTESIAN_POINT('Ctrl Pts',(-15.9489604567358,19.8325994923992,
15.090058039767));
#209274=CARTESIAN_POINT('Ctrl Pts',(-16.7038441148284,17.2056825018467,
15.2172338464485));
#209275=CARTESIAN_POINT('Ctrl Pts',(-19.321269791881,16.4185198518091,15.3444096531299));
#209276=CARTESIAN_POINT('Ctrl Pts',(-21.3999118849568,18.1932844168717,
15.4715854598113));
#209277=CARTESIAN_POINT('Ctrl Pts',(-21.0327452887372,20.9017398629015,
15.5987612664928));
#209278=CARTESIAN_POINT('Ctrl Pts',(-18.5566225663247,22.05904642387,15.7259370731742));
#209279=CARTESIAN_POINT('Ctrl Pts',(-16.2432326300242,20.6034471606347,
15.8531128798556));
#209280=CARTESIAN_POINT('Ctrl Pts',(-16.2149671612184,17.8703640525348,
15.9802886865371));
#209281=CARTESIAN_POINT('Ctrl Pts',(-18.4977579731839,16.367231216983,16.1074644932185));
#209282=CARTESIAN_POINT('Ctrl Pts',(-20.9972861819192,17.4730797356526,
16.2346402999));
#209283=CARTESIAN_POINT('Ctrl Pts',(-21.4203897941269,20.1733622293642,
16.3618161065814));
#209284=CARTESIAN_POINT('Ctrl Pts',(-19.378897506378,21.9907371085704,16.4889919132628));
#209285=CARTESIAN_POINT('Ctrl Pts',(-16.7457517833806,21.2578757206061,
16.6161677199442));
#209286=CARTESIAN_POINT('Ctrl Pts',(-15.9367003945299,18.6471329024206,
16.7433435266257));
#209287=CARTESIAN_POINT('Ctrl Pts',(-17.6939977737036,16.5537031487253,
16.8705193333071));
#209288=CARTESIAN_POINT('Ctrl Pts',(-20.4054326456862,16.8981783256312,
16.9976951399886));
#209289=CARTESIAN_POINT('Ctrl Pts',(-21.5834318060615,19.364523838868,17.12487094667));
#209290=CARTESIAN_POINT('Ctrl Pts',(-20.1472541400588,21.6900207587073,
17.2520467533514));
#209291=CARTESIAN_POINT('Ctrl Pts',(-17.4145035169965,21.7411699978141,
17.3792225600329));
#209292=CARTESIAN_POINT('Ctrl Pts',(-15.8923090199021,19.4710453039866,
17.5063983667143));
#209293=CARTESIAN_POINT('Ctrl Pts',(-16.9771896218132,16.9623451839844,
17.6335741733957));
#209294=CARTESIAN_POINT('Ctrl Pts',(-19.6738347057625,16.5166462904161,
17.7607499800772));
#209295=CARTESIAN_POINT('Ctrl Pts',(-21.5082397798925,18.542849694944,17.8879257867586));
#209296=CARTESIAN_POINT('Ctrl Pts',(-20.7974520447164,21.1820395342675,
18.01510159344));
#209297=CARTESIAN_POINT('Ctrl Pts',(-18.1935751307804,22.0129229374272,
18.1422774001214));
#209298=CARTESIAN_POINT('Ctrl Pts',(-16.085504491823,20.2732159524167,18.2694532068029));
#209299=CARTESIAN_POINT('Ctrl Pts',(-16.4072640974092,17.5589917596816,
18.3966290134843));
#209300=CARTESIAN_POINT('Ctrl Pts',(-18.8636594801795,16.3603825921271,
18.5238048201658));
#209301=CARTESIAN_POINT('Ctrl Pts',(-21.2011003373174,17.7770379672497,
18.6509806268472));
#209302=CARTESIAN_POINT('Ctrl Pts',(-21.2751297607576,20.5092645052679,
18.7781564335287));
#209303=CARTESIAN_POINT('Ctrl Pts',(-19.0178303484736,22.0504139399173,
18.90533224021));
#209304=CARTESIAN_POINT('Ctrl Pts',(-16.5001342089838,20.9865773169943,
19.0325080468915));
#209305=CARTESIAN_POINT('Ctrl Pts',(-16.0318712814367,18.2937587135751,
19.1596838535729));
#209306=CARTESIAN_POINT('Ctrl Pts',(-18.042643743939,16.4424520540833,19.2868596602544));
#209307=CARTESIAN_POINT('Ctrl Pts',(-20.6876926536642,17.1311163109758,
19.4140354669358));
#209308=CARTESIAN_POINT('Ctrl Pts',(-21.5403498275698,19.7279447383034,
19.5412112736172));
#209309=CARTESIAN_POINT('Ctrl Pts',(-19.8183551892704,21.8505084960413,
19.6683870802987));
#209310=CARTESIAN_POINT('Ctrl Pts',(-17.1015320197568,21.5514869529538,
19.7955628869801));
#209311=CARTESIAN_POINT('Ctrl Pts',(-15.8823967990051,19.1052140557062,
19.9227386936616));
#209312=CARTESIAN_POINT('Ctrl Pts',(-17.2794307188022,16.7559928917323,
20.049914500343));
#209313=CARTESIAN_POINT('Ctrl Pts',(-20.0109412993294,16.6590889620223,
20.1770903070244));
#209314=CARTESIAN_POINT('Ctrl Pts',(-21.5709382143749,18.9034038883535,
20.3042661137059));
#209315=CARTESIAN_POINT('Ctrl Pts',(-20.5282190091016,21.4299213366298,
20.4314419203873));
#209316=CARTESIAN_POINT('Ctrl Pts',(-17.839417901151,21.920711977366,20.5586177270687));
#209317=CARTESIAN_POINT('Ctrl Pts',(-15.9713351874333,19.9255181617605,
20.6857935337502));
#209318=CARTESIAN_POINT('Ctrl Pts',(-16.6378359073908,17.2747826734461,
20.8129693404316));
#209319=CARTESIAN_POINT('Ctrl Pts',(-19.227417928117,16.4004364825627,20.940145147113));
#209320=CARTESIAN_POINT('Ctrl Pts',(-21.3643565302024,18.1045499196127,
21.0673209537945));
#209321=CARTESIAN_POINT('Ctrl Pts',(-21.0880351566437,20.8238743140973,
21.1944967604759));
#209322=CARTESIAN_POINT('Ctrl Pts',(-18.6521696806324,22.0632714134299,
21.3216725671574));
#209323=CARTESIAN_POINT('Ctrl Pts',(-16.2911143425161,20.6863012877323,
21.4488483738387));
#209324=CARTESIAN_POINT('Ctrl Pts',(-16.1717640085979,17.9550342010845,
21.5760241805202));
#209325=CARTESIAN_POINT('Ctrl Pts',(-18.4021242165115,16.3775818193965,
21.7031999872016));
#209326=CARTESIAN_POINT('Ctrl Pts',(-20.9388618348603,17.3966090547766,
21.8303757938831));
#209327=CARTESIAN_POINT('Ctrl Pts',(-21.4490180684747,20.086305979354,21.9575516005645));
#209328=CARTESIAN_POINT('Ctrl Pts',(-20.1339757340687,21.3345378652548,
22.0423354716855));
#209329=CARTESIAN_POINT('Ctrl Pts',(-19.3578031346334,21.5422303014122,
22.0847274072459));
#209330=CARTESIAN_POINT('Ctrl Pts',(-16.7733106781414,20.8620837377565,
-0.257713132874658));
#209331=CARTESIAN_POINT('Ctrl Pts',(-16.2233209547904,20.2090078625832,
-0.215302539815803));
#209332=CARTESIAN_POINT('Ctrl Pts',(-15.8372833671953,18.3216228609763,
-0.130500011196469));
#209333=CARTESIAN_POINT('Ctrl Pts',(-17.9181405522913,16.2898554993676,
-0.00330554701665755));
#209334=CARTESIAN_POINT('Ctrl Pts',(-20.7467663181702,16.9459334204518,
0.123870259664777));
#209335=CARTESIAN_POINT('Ctrl Pts',(-21.7289765433362,19.6762952284609,
0.251046066346211));
#209336=CARTESIAN_POINT('Ctrl Pts',(-19.9633972633481,21.9817192979426,
0.378221873027645));
#209337=CARTESIAN_POINT('Ctrl Pts',(-17.0699655598372,21.7441745055157,
0.50539767970908));
#209338=CARTESIAN_POINT('Ctrl Pts',(-15.703159781685,19.1831211299953,0.632573486390514));
#209339=CARTESIAN_POINT('Ctrl Pts',(-17.1169734025524,16.6473741262867,
0.759749293071947));
#209340=CARTESIAN_POINT('Ctrl Pts',(-20.0143025363638,16.4637352509469,
0.886925099753383));
#209341=CARTESIAN_POINT('Ctrl Pts',(-21.7370366847608,18.8004683549644,
1.01410090643482));
#209342=CARTESIAN_POINT('Ctrl Pts',(-20.7046694415748,21.5138766002705,
1.14127671311625));
#209343=CARTESIAN_POINT('Ctrl Pts',(-17.8643361414099,22.1145188622328,
1.26845251979769));
#209344=CARTESIAN_POINT('Ctrl Pts',(-15.8218650170646,20.0513729702491,
1.39562832647912));
#209345=CARTESIAN_POINT('Ctrl Pts',(-16.4510972188617,17.217231749811,1.52280413316055));
#209346=CARTESIAN_POINT('Ctrl Pts',(-19.1747509117416,16.2122518956796,
1.64997993984199));
#209347=CARTESIAN_POINT('Ctrl Pts',(-21.4940430602564,17.9584358800158,
1.77715574652343));
#209348=CARTESIAN_POINT('Ctrl Pts',(-21.281166976886,20.8537704404796,1.90433155320486));
#209349=CARTESIAN_POINT('Ctrl Pts',(-18.7314233036813,22.2419647001733,
2.03150735988629));
#209350=CARTESIAN_POINT('Ctrl Pts',(-16.1840435808866,20.8494371693366,
2.15868316656773));
#209351=CARTESIAN_POINT('Ctrl Pts',(-15.9760906089126,17.9537451252482,
2.28585897324916));
#209352=CARTESIAN_POINT('Ctrl Pts',(-18.2983483258012,16.2115064482945,
2.4130347799306));
#209353=CARTESIAN_POINT('Ctrl Pts',(-21.0202894153674,17.2211169076559,
2.54021058661203));
#209354=CARTESIAN_POINT('Ctrl Pts',(-21.64470186884,20.0563216126004,2.66738639329346));
#209355=CARTESIAN_POINT('Ctrl Pts',(-19.5987260165054,22.1159961970718,
2.7945621999749));
#209356=CARTESIAN_POINT('Ctrl Pts',(-16.75941771481,21.5105170790144,2.92173800665633));
#209357=CARTESIAN_POINT('Ctrl Pts',(-15.7316661034645,18.7953737630709,
3.04891381333777));
#209358=CARTESIAN_POINT('Ctrl Pts',(-17.4583694962879,16.4615417238828,
3.1760896200192));
#209359=CARTESIAN_POINT('Ctrl Pts',(-20.3553847017321,16.6501670018626,
3.30326542670064));
#209360=CARTESIAN_POINT('Ctrl Pts',(-21.7648800778091,19.1881976126941,
3.43044123338207));
#209361=CARTESIAN_POINT('Ctrl Pts',(-20.3937311001358,21.7471479984566,
3.5576170400635));
#209362=CARTESIAN_POINT('Ctrl Pts',(-17.4998818526145,21.9793400068086,
3.68479284674494));
#209363=CARTESIAN_POINT('Ctrl Pts',(-15.7382594073102,19.671751881433,3.81196865342637));
#209364=CARTESIAN_POINT('Ctrl Pts',(-16.7250430191669,16.9414525023501,
3.93914446010781));
#209365=CARTESIAN_POINT('Ctrl Pts',(-19.5549199710057,16.2933220883461,
4.06632026678924));
#209366=CARTESIAN_POINT('Ctrl Pts',(-21.6316538014862,18.3219800667756,
4.19349607347067));
#209367=CARTESIAN_POINT('Ctrl Pts',(-21.0499701177813,21.1662586551355,
4.32067188015211));
#209368=CARTESIAN_POINT('Ctrl Pts',(-18.3435275963289,22.2167087844487,
4.44784768683354));
#209369=CARTESIAN_POINT('Ctrl Pts',(-15.995319269794,20.5096076593562,4.57502349351498));
#209370=CARTESIAN_POINT('Ctrl Pts',(-16.1596805315267,17.6111146074862,
4.70219930019641));
#209371=CARTESIAN_POINT('Ctrl Pts',(-18.6858201252975,16.180417103161,4.82937510687785));
#209372=CARTESIAN_POINT('Ctrl Pts',(-21.2561617637275,17.5300913074975,
4.95655091355928));
#209373=CARTESIAN_POINT('Ctrl Pts',(-21.5125765269512,20.4218949082454,
5.08372672024072));
#209374=CARTESIAN_POINT('Ctrl Pts',(-19.2198197846062,22.2027775872924,
5.21090252692215));
#209375=CARTESIAN_POINT('Ctrl Pts',(-16.4813535432613,21.2388900206576,
5.33807833360358));
#209376=CARTESIAN_POINT('Ctrl Pts',(-15.8095506109669,18.4145392251191,
5.46525414028503));
#209377=CARTESIAN_POINT('Ctrl Pts',(-17.8207484813105,16.3208917566031,
5.59242994696645));
#209378=CARTESIAN_POINT('Ctrl Pts',(-20.6697979372697,16.8787392210558,
5.71960575364789));
#209379=CARTESIAN_POINT('Ctrl Pts',(-21.7428729349543,19.5762911937604,
5.84678156032932));
#209380=CARTESIAN_POINT('Ctrl Pts',(-20.0554937665342,21.9387111687183,
5.97395736701076));
#209381=CARTESIAN_POINT('Ctrl Pts',(-17.1557260884723,21.7986254472259,
6.10113317369219));
#209382=CARTESIAN_POINT('Ctrl Pts',(-15.7039267655104,19.284553984052,6.22830898037363));
#209383=CARTESIAN_POINT('Ctrl Pts',(-17.0320315676376,16.7030013057854,
6.35548478705506));
#209384=CARTESIAN_POINT('Ctrl Pts',(-19.9215867703828,16.4223817655062,
6.48266059373649));
#209385=CARTESIAN_POINT('Ctrl Pts',(-21.7216048212496,18.7001463742074,
6.60983640041793));
#209386=CARTESIAN_POINT('Ctrl Pts',(-20.7806808802879,21.4465874774214,
6.73701220709936));
#209387=CARTESIAN_POINT('Ctrl Pts',(-17.9620542630039,22.1420158263089,
6.8641880137808));
#209388=CARTESIAN_POINT('Ctrl Pts',(-15.8516399470578,20.1484190739168,
6.99136382046223));
#209389=CARTESIAN_POINT('Ctrl Pts',(-16.3856120802451,17.2947985039956,
7.11853962714367));
#209390=CARTESIAN_POINT('Ctrl Pts',(-19.0740843724149,16.1991738737805,
7.2457154338251));
#209391=CARTESIAN_POINT('Ctrl Pts',(-21.4505503609105,17.86671277936,7.37289124050654));
#209392=CARTESIAN_POINT('Ctrl Pts',(-21.3347500014016,20.7675517740021,
7.50006704718796));
#209393=CARTESIAN_POINT('Ctrl Pts',(-18.8329229363566,22.2403511264959,
7.62724285386941));
#209394=CARTESIAN_POINT('Ctrl Pts',(-16.2403402170543,20.9339088431657,
7.75441866055083));
#209395=CARTESIAN_POINT('Ctrl Pts',(-15.9355355746231,18.0468046320139,
7.88159446723227));
#209396=CARTESIAN_POINT('Ctrl Pts',(-18.1981483501842,16.2277774128756,
8.0087702739137));
#209397=CARTESIAN_POINT('Ctrl Pts',(-20.952371755747,17.145671757748,8.13594608059513));
#209398=CARTESIAN_POINT('Ctrl Pts',(-21.6713767630913,19.958376576159,8.26312188727658));
#209399=CARTESIAN_POINT('Ctrl Pts',(-19.6955209044624,22.0854097733659,
8.390297693958));
#209400=CARTESIAN_POINT('Ctrl Pts',(-16.8375292947071,21.5753504095007,
8.51747350063944));
#209401=CARTESIAN_POINT('Ctrl Pts',(-15.719431848811,18.896146293055,8.64464930732087));
#209402=CARTESIAN_POINT('Ctrl Pts',(-17.3670135764298,16.5058009107065,
8.77182511400231));
#209403=CARTESIAN_POINT('Ctrl Pts',(-20.268720502928,16.5973077891932,8.89900092068374));
#209404=CARTESIAN_POINT('Ctrl Pts',(-21.7624166234869,19.0867150470611,
9.02617672736517));
#209405=CARTESIAN_POINT('Ctrl Pts',(-20.4777284567308,21.6901460352563,
9.15335253404662));
#209406=CARTESIAN_POINT('Ctrl Pts',(-17.5932776589179,22.0191144092604,
9.28052834072804));
#209407=CARTESIAN_POINT('Ctrl Pts',(-15.7553688078344,19.7718121040047,
9.40770414740949));
#209408=CARTESIAN_POINT('Ctrl Pts',(-16.6501692008611,17.0099995012495,
9.53487995409091));
#209409=CARTESIAN_POINT('Ctrl Pts',(-19.4567550149717,16.2674682466002,
9.66205576077236));
#209410=CARTESIAN_POINT('Ctrl Pts',(-21.6002579620812,18.2254446795103,
9.78923156745378));
#209411=CARTESIAN_POINT('Ctrl Pts',(-21.1141471290137,21.0876069485077,
9.91640737413522));
#209412=CARTESIAN_POINT('Ctrl Pts',(-18.4443990336675,22.2280988176125,
10.0435831808167));
#209413=CARTESIAN_POINT('Ctrl Pts',(-16.0403418502683,20.6005897838297,
10.1707589874981));
#209414=CARTESIAN_POINT('Ctrl Pts',(-16.1075488319678,17.698218371052,10.2979347941796));
#209415=CARTESIAN_POINT('Ctrl Pts',(-18.5843617443927,16.183730209017,10.425110600861));
#209416=CARTESIAN_POINT('Ctrl Pts',(-21.1984584687395,17.4465741866552,
10.5522864075424));
#209417=CARTESIAN_POINT('Ctrl Pts',(-21.5515675095613,20.3281693354206,
10.6794622142238));
#209418=CARTESIAN_POINT('Ctrl Pts',(-19.3197332383227,22.1848309582866,
10.8066380209053));
#209419=CARTESIAN_POINT('Ctrl Pts',(-16.5505250756278,21.3131872536903,
10.9338138275867));
#209420=CARTESIAN_POINT('Ctrl Pts',(-15.7845196343066,18.5129172202892,
11.0609896342681));
#209421=CARTESIAN_POINT('Ctrl Pts',(-17.7244793631115,16.3530948093689,
11.1881654409496));
#209422=CARTESIAN_POINT('Ctrl Pts',(-20.5906116183444,16.8152230292517,
11.315341247631));
#209423=CARTESIAN_POINT('Ctrl Pts',(-21.7534179480593,19.4753279211071,
11.4425170543125));
#209424=CARTESIAN_POINT('Ctrl Pts',(-20.1460957166431,21.8929283513879,
11.5696928609939));
#209425=CARTESIAN_POINT('Ctrl Pts',(-17.2432633097514,21.8500259785168,
11.6968686676753));
#209426=CARTESIAN_POINT('Ctrl Pts',(-15.7080892906089,19.3859810667816,
11.8240444743568));
#209427=CARTESIAN_POINT('Ctrl Pts',(-16.9490005381331,16.7614018868241,
11.9512202810382));
#209428=CARTESIAN_POINT('Ctrl Pts',(-19.8275380023589,16.3841769364998,
12.0783960877196));
#209429=CARTESIAN_POINT('Ctrl Pts',(-21.7028222220433,18.6003866945102,
12.205571894401));
#209430=CARTESIAN_POINT('Ctrl Pts',(-20.8543963188915,21.3767962613715,
12.3327477010825));
#209431=CARTESIAN_POINT('Ctrl Pts',(-18.0606383997947,22.1662221829007,
12.4599235077639));
#209432=CARTESIAN_POINT('Ctrl Pts',(-15.8846479553519,20.2444151733933,
12.5870993144454));
#209433=CARTESIAN_POINT('Ctrl Pts',(-16.3227611611408,17.3745138832769,
12.7142751211268));
#209434=CARTESIAN_POINT('Ctrl Pts',(-18.9730363432223,16.1894746200704,
12.8414509278082));
#209435=CARTESIAN_POINT('Ctrl Pts',(-21.4040105166661,17.776497355934,12.9686267344897));
#209436=CARTESIAN_POINT('Ctrl Pts',(-21.385415760611,20.6795872324527,13.0958025411711));
#209437=CARTESIAN_POINT('Ctrl Pts',(-18.934311609617,22.2353394739996,13.2229783478525));
#209438=CARTESIAN_POINT('Ctrl Pts',(-16.2994339895399,21.0164479598295,
13.350154154534));
#209439=CARTESIAN_POINT('Ctrl Pts',(-15.8981195778518,18.1411700012542,
13.4773299612154));
#209440=CARTESIAN_POINT('Ctrl Pts',(-18.0985494388948,16.2473946653896,
13.6045057678968));
#209441=CARTESIAN_POINT('Ctrl Pts',(-20.881965749242,17.0725432819383,13.7316815745783));
#209442=CARTESIAN_POINT('Ctrl Pts',(-21.6947568024494,19.8595932097158,
13.8588573812597));
#209443=CARTESIAN_POINT('Ctrl Pts',(-19.7912372547015,22.0515991238136,
13.9860331879411));
#209444=CARTESIAN_POINT('Ctrl Pts',(-16.9177681453095,21.6375316492779,
14.1132089946226));
#209445=CARTESIAN_POINT('Ctrl Pts',(-15.7105790345338,18.9972719940692,
14.240384801304));
#209446=CARTESIAN_POINT('Ctrl Pts',(-17.2771910049047,16.5530945188459,
14.3675606079854));
#209447=CARTESIAN_POINT('Ctrl Pts',(-20.1803348085118,16.5473803543624,
14.4947364146669));
#209448=CARTESIAN_POINT('Ctrl Pts',(-21.7565561949717,18.9853718918711,
14.6219122213483));
#209449=CARTESIAN_POINT('Ctrl Pts',(-20.5597698735399,21.6303632145285,
14.7490880280298));
#209450=CARTESIAN_POINT('Ctrl Pts',(-17.6879530131938,22.0557389504721,
14.8762638347112));
#209451=CARTESIAN_POINT('Ctrl Pts',(-15.7758193382441,19.8712432637697,
15.0034396413926));
#209452=CARTESIAN_POINT('Ctrl Pts',(-16.5776328150568,17.081015361877,15.130615448074));
#209453=CARTESIAN_POINT('Ctrl Pts',(-19.3577793448131,16.244916163706,15.2577912547555));
#209454=CARTESIAN_POINT('Ctrl Pts',(-21.5656470418159,18.1300147894097,
15.3849670614369));
#209455=CARTESIAN_POINT('Ctrl Pts',(-21.1756543297891,21.006850252321,15.5121428681183));
#209456=CARTESIAN_POINT('Ctrl Pts',(-18.5455953163398,22.2361045717652,
15.6393186747998));
#209457=CARTESIAN_POINT('Ctrl Pts',(-16.0883859064352,20.6900132057797,
15.7664944814812));
#209458=CARTESIAN_POINT('Ctrl Pts',(-16.0583632220467,17.7870190214039,
15.8936702881626));
#209459=CARTESIAN_POINT('Ctrl Pts',(-18.4830712126828,16.1904390026627,
16.0208460948441));
#209460=CARTESIAN_POINT('Ctrl Pts',(-21.1379907912854,17.3650362218196,
16.1480219015255));
#209461=CARTESIAN_POINT('Ctrl Pts',(-21.5873980273796,20.2331906340233,
16.2751977082069));
#209462=CARTESIAN_POINT('Ctrl Pts',(-19.418989675208,22.1635485838168,16.4023735148884));
#209463=CARTESIAN_POINT('Ctrl Pts',(-16.6221458112869,21.3851264637907,
16.5295493215698));
#209464=CARTESIAN_POINT('Ctrl Pts',(-15.7627970890565,18.6120782547437,
16.6567251282513));
#209465=CARTESIAN_POINT('Ctrl Pts',(-17.629342623966,16.3885035736934,16.7839009349327));
#209466=CARTESIAN_POINT('Ctrl Pts',(-20.5093427386175,16.7543941798941,
16.9110767416142));
#209467=CARTESIAN_POINT('Ctrl Pts',(-21.7605760807848,19.374068151889,17.0382525482955));
#209468=CARTESIAN_POINT('Ctrl Pts',(-20.2351137193294,21.8441372156765,
17.165428354977));
#209469=CARTESIAN_POINT('Ctrl Pts',(-17.3324726900139,21.8984663150084,
17.2926041616584));
#209470=CARTESIAN_POINT('Ctrl Pts',(-15.7156459790158,19.4872118732907,
17.4197799683399));
#209471=CARTESIAN_POINT('Ctrl Pts',(-16.8679717420912,16.8225501814725,
17.5469557750213));
#209472=CARTESIAN_POINT('Ctrl Pts',(-19.7322626130239,16.3491429542363,
17.6741315817028));
#209473=CARTESIAN_POINT('Ctrl Pts',(-21.6807094956696,18.501311939612,17.8013073883841));
#209474=CARTESIAN_POINT('Ctrl Pts',(-20.925733309462,21.3045756721761,17.9284831950656));
#209475=CARTESIAN_POINT('Ctrl Pts',(-18.1599778461229,22.1871136674968,
18.055659001747));
#209476=CARTESIAN_POINT('Ctrl Pts',(-15.9208520811544,20.3392520913025,
18.1828348084285));
#209477=CARTESIAN_POINT('Ctrl Pts',(-16.2626149280343,17.4562892486245,
18.3100106151099));
#209478=CARTESIAN_POINT('Ctrl Pts',(-18.8717201870645,16.1831646105782,
18.4371864217913));
#209479=CARTESIAN_POINT('Ctrl Pts',(-21.3544757221902,17.6878910139056,
18.5643622284728));
#209480=CARTESIAN_POINT('Ctrl Pts',(-21.4331074275647,20.5899753767109,
18.6915380351542));
#209481=CARTESIAN_POINT('Ctrl Pts',(-19.0354755930861,22.226935421132,18.8187138418356));
#209482=CARTESIAN_POINT('Ctrl Pts',(-16.3612586147209,21.0969619050252,
18.9458896485171));
#209483=CARTESIAN_POINT('Ctrl Pts',(-15.8638845863206,18.2367354003361,
19.0730654551985));
#209484=CARTESIAN_POINT('Ctrl Pts',(-17.9996633145444,16.2703361898353,
19.20024126188));
#209485=CARTESIAN_POINT('Ctrl Pts',(-20.8091503658403,17.0018135191641,
19.3274170685614));
#209486=CARTESIAN_POINT('Ctrl Pts',(-21.7148157697857,19.7600823036045,
19.4545928752428));
#209487=CARTESIAN_POINT('Ctrl Pts',(-19.8857676864347,22.0146021996221,
19.5817686819242));
#209488=CARTESIAN_POINT('Ctrl Pts',(-17.000044293062,21.6969910014797,19.7089444886057));
#209489=CARTESIAN_POINT('Ctrl Pts',(-15.7051175323933,19.0986375254879,
19.8361202952871));
#209490=CARTESIAN_POINT('Ctrl Pts',(-17.1890026482639,16.6033693221106,
19.9632961019685));
#209491=CARTESIAN_POINT('Ctrl Pts',(-20.0903265437325,16.500441041753,20.09047190865));
#209492=CARTESIAN_POINT('Ctrl Pts',(-21.7473057839905,18.8842811671185,
20.2176477153314));
#209493=CARTESIAN_POINT('Ctrl Pts',(-20.6397625190695,21.5678678598662,
20.3448235220129));
#209494=CARTESIAN_POINT('Ctrl Pts',(-17.7838032706328,22.0891701106396,
20.4719993286943));
#209495=CARTESIAN_POINT('Ctrl Pts',(-15.7995850674674,19.9699385269971,
20.5991751353757));
#209496=CARTESIAN_POINT('Ctrl Pts',(-16.5075209908883,17.1544113723013,
20.7263509420572));
#209497=CARTESIAN_POINT('Ctrl Pts',(-19.2580928720921,16.2257085824946,
20.8535267487386));
#209498=CARTESIAN_POINT('Ctrl Pts',(-21.5278812718071,18.035763821068,20.98070255542));
#209499=CARTESIAN_POINT('Ctrl Pts',(-21.2343814736918,20.9241439362665,
21.1078783621014));
#209500=CARTESIAN_POINT('Ctrl Pts',(-18.6470824304151,22.2405922216597,
21.2350541687829));
#209501=CARTESIAN_POINT('Ctrl Pts',(-16.1392443426422,20.7780182314604,
21.3622299754643));
#209502=CARTESIAN_POINT('Ctrl Pts',(-16.0124742037318,17.876952967467,21.4894057821458));
#209503=CARTESIAN_POINT('Ctrl Pts',(-18.381492069836,16.2014330842265,21.6165815888272));
#209504=CARTESIAN_POINT('Ctrl Pts',(-21.0759343030523,17.2838114902333,
21.7437573955087));
#209505=CARTESIAN_POINT('Ctrl Pts',(-21.6178060723067,20.1407222466758,
21.87093320219));
#209506=CARTESIAN_POINT('Ctrl Pts',(-20.221009817676,21.4665545621232,21.955717073311));
#209507=CARTESIAN_POINT('Ctrl Pts',(-19.3965839026516,21.687158879832,21.9981090088715));
#209508=CARTESIAN_POINT('Ctrl Pts',(-17.1140743056112,20.5739122292573,
-2.78423117894278E-16));
#209509=CARTESIAN_POINT('Ctrl Pts',(-17.0603911325521,20.522111673172,-4.4535200385995E-15));
#209510=CARTESIAN_POINT('Ctrl Pts',(-17.0098645202578,20.4674385257497,
1.04642875463197E-14));
#209511=CARTESIAN_POINT('Ctrl Pts',(-16.9624881995608,20.410264093257,-4.6525283625698E-15));
#209512=CARTESIAN_POINT('Ctrl Pts',(-16.9134245654311,20.3510533863865,
-2.03077315114503E-14));
#209513=CARTESIAN_POINT('Ctrl Pts',(-16.8677391100142,20.2891596196025,
-4.05979361674585E-15));
#209514=CARTESIAN_POINT('Ctrl Pts',(-16.8254532095209,20.2249455930866,
-3.18148285494146E-15));
#209515=CARTESIAN_POINT('Ctrl Pts',(-16.7853187213456,20.1639986330401,
-2.34785858603208E-15));
#209516=CARTESIAN_POINT('Ctrl Pts',(-16.7482466106958,20.1009605704111,
-1.98929216896175E-14));
#209517=CARTESIAN_POINT('Ctrl Pts',(-16.7142836213594,20.0361088469223,
-1.85407245112401E-14));
#209518=CARTESIAN_POINT('Ctrl Pts',(-16.6991853089609,20.0072788881953,
-1.79558883097759E-14));
#209519=CARTESIAN_POINT('Ctrl Pts',(-16.6847018341336,19.9780901364722,
8.22240768298966E-15));
#209520=CARTESIAN_POINT('Ctrl Pts',(-16.6708392964776,19.9485654278612,
-1.03736463863413E-14));
#209521=CARTESIAN_POINT('Ctrl Pts',(-16.6640109607001,19.9340223024153,
-1.91889155439778E-14));
#209522=CARTESIAN_POINT('Ctrl Pts',(-16.657333302533,19.9193976511972,-3.21445356456926E-15));
#209523=CARTESIAN_POINT('Ctrl Pts',(-16.6508071688394,19.9046941363876,
4.60048665829049E-15));
#209524=CARTESIAN_POINT('Ctrl Pts',(-16.6447949816305,19.8911485536865,
1.18973701611653E-14));
#209525=CARTESIAN_POINT('Ctrl Pts',(-16.6389109256811,19.8775346474983,
-3.87472281196432E-15));
#209526=CARTESIAN_POINT('Ctrl Pts',(-16.6331636045017,19.8638740397009,
-6.0507154842071E-15));
#209527=CARTESIAN_POINT('Ctrl Pts',(-16.6020948019513,19.790027683611,-1.85629496859678E-14));
#209528=CARTESIAN_POINT('Ctrl Pts',(-16.5749612060018,19.7146929635301,
-9.23216762033033E-15));
#209529=CARTESIAN_POINT('Ctrl Pts',(-16.5517844460822,19.6382510185693,
-1.35724764760425E-14));
#209530=CARTESIAN_POINT('Ctrl Pts',(-16.5281813102643,19.5604027940831,
-1.7992632691482E-14));
#209531=CARTESIAN_POINT('Ctrl Pts',(-16.5086814210927,19.4814054223281,
-2.58768124863866E-14));
#209532=CARTESIAN_POINT('Ctrl Pts',(-16.4933485190228,19.4016259047523,
-6.64746035994312E-15));
#209533=CARTESIAN_POINT('Ctrl Pts',(-16.4794162838084,19.329134278635,1.08252826095013E-14));
#209534=CARTESIAN_POINT('Ctrl Pts',(-16.4689247639322,19.2559959244267,
-1.01990454609122E-14));
#209535=CARTESIAN_POINT('Ctrl Pts',(-16.4619555680579,19.1824703462648,
-1.64729341278758E-14));
#209536=CARTESIAN_POINT('Ctrl Pts',(-16.4592976470201,19.1544290650995,
-1.9145684836839E-14));
#209537=CARTESIAN_POINT('Ctrl Pts',(-16.4571524088489,19.1263313551069,
-2.39160590086535E-14));
#209538=CARTESIAN_POINT('Ctrl Pts',(-16.4555257409501,19.0981913259617,
4.73232564246473E-15));
#209539=CARTESIAN_POINT('Ctrl Pts',(-16.4546322610198,19.0827348512285,
2.03445886243926E-14));
#209540=CARTESIAN_POINT('Ctrl Pts',(-16.453895246137,19.0672656072016,8.61144224714149E-16));
#209541=CARTESIAN_POINT('Ctrl Pts',(-16.4533157740873,19.051785924702,-1.2712053631958E-14));
#209542=CARTESIAN_POINT('Ctrl Pts',(-16.4528680721876,19.0398262740765,
-2.31702952227711E-14));
#209543=CARTESIAN_POINT('Ctrl Pts',(-16.452514580052,19.0278636904617,-5.25880506684687E-15));
#209544=CARTESIAN_POINT('Ctrl Pts',(-16.4522557186358,19.0159077924821,
-5.49560397189452E-15));
#209545=CARTESIAN_POINT('Ctrl Pts',(-16.4504488747984,18.9324560332097,
-7.08812930653476E-15));
#209546=CARTESIAN_POINT('Ctrl Pts',(-16.4532438607103,18.8492105138102,
-8.50757505162779E-16));
#209547=CARTESIAN_POINT('Ctrl Pts',(-16.4606969184041,18.7665518702536,
-4.28823643261467E-15));
#209548=CARTESIAN_POINT('Ctrl Pts',(-16.4681357553308,18.6840509430821,
-6.93785445528216E-15));
#209549=CARTESIAN_POINT('Ctrl Pts',(-16.4802145308229,18.6021336503298,
-7.5002128928925E-15));
#209550=CARTESIAN_POINT('Ctrl Pts',(-16.4970385284052,18.5211628277987,
-4.57966997657877E-15));
#209551=CARTESIAN_POINT('Ctrl Pts',(-16.5134762563069,18.4420510505752,
-2.05411160106774E-15));
#209552=CARTESIAN_POINT('Ctrl Pts',(-16.5344435942651,18.3638418295306,
1.67537111895845E-14));
#209553=CARTESIAN_POINT('Ctrl Pts',(-16.5596748813382,18.2867616450374,
2.91433543964104E-15));
#209554=CARTESIAN_POINT('Ctrl Pts',(-16.5700722924092,18.2549981301094,
-2.73628106559942E-15));
#209555=CARTESIAN_POINT('Ctrl Pts',(-16.581194395652,18.2234264109971,-1.52990285076908E-14));
#209556=CARTESIAN_POINT('Ctrl Pts',(-16.5930250854222,18.1920628114276,
-1.0991207943789E-14));
#209557=CARTESIAN_POINT('Ctrl Pts',(-16.5995763500233,18.1746951647716,
-8.76724025831231E-15));
#209558=CARTESIAN_POINT('Ctrl Pts',(-16.6063471420461,18.1573861965041,
-1.48891845053629E-14));
#209559=CARTESIAN_POINT('Ctrl Pts',(-16.6133223339605,18.1401687566554,
-1.25177646026486E-14));
#209560=CARTESIAN_POINT('Ctrl Pts',(-16.6442815008621,18.0637496988806,
-1.82337894072226E-15));
#209561=CARTESIAN_POINT('Ctrl Pts',(-16.6792965711232,17.9890373934243,
-5.44156629526273E-17));
#209562=CARTESIAN_POINT('Ctrl Pts',(-16.7180395276146,17.9162554524269,
-4.19109191795997E-15));
#209563=CARTESIAN_POINT('Ctrl Pts',(-16.7588464280445,17.8395962170884,
-8.5481403039391E-15));
#209564=CARTESIAN_POINT('Ctrl Pts',(-16.8037890252177,17.7650776476886,
8.20107877868703E-15));
#209565=CARTESIAN_POINT('Ctrl Pts',(-16.8525445311818,17.692966664072,1.08801856413265E-14));
#209566=CARTESIAN_POINT('Ctrl Pts',(-16.9013000371459,17.6208556804554,
1.3559292503966E-14));
#209567=CARTESIAN_POINT('Ctrl Pts',(-16.9538690505405,17.5511513968607,
-1.85766771511439E-14));
#209568=CARTESIAN_POINT('Ctrl Pts',(-17.0099820350415,17.4841394296583,
2.60902410786912E-15));
#209569=CARTESIAN_POINT('Ctrl Pts',(-17.0318957421493,17.4579693616242,
1.08023314394969E-14));
#209570=CARTESIAN_POINT('Ctrl Pts',(-17.0543504737559,17.4322101781547,
3.45386508731371E-17));
#209571=CARTESIAN_POINT('Ctrl Pts',(-17.0773320757735,17.4068801208169,
-6.93889390390723E-16));
#209572=CARTESIAN_POINT('Ctrl Pts',(-17.0864638250902,17.3968152117818,
-1.01658935222294E-15));
#209573=CARTESIAN_POINT('Ctrl Pts',(-17.0956795264284,17.3868172601505,
-1.08346130998296E-14));
#209574=CARTESIAN_POINT('Ctrl Pts',(-17.1049759845535,17.376889953632,-9.29811783123569E-15));
#209575=CARTESIAN_POINT('Ctrl Pts',(-17.1654855522993,17.3122742668584,
1.31805477752442E-15));
#209576=CARTESIAN_POINT('Ctrl Pts',(-17.2292149096655,17.2508596682763,
6.852693416406E-15));
#209577=CARTESIAN_POINT('Ctrl Pts',(-17.2958559710253,17.1929205201455,
8.77076189453874E-15));
#209578=CARTESIAN_POINT('Ctrl Pts',(-17.3510488277484,17.1449346832427,
1.03593272105537E-14));
#209579=CARTESIAN_POINT('Ctrl Pts',(-17.4082400420401,17.099332805993,4.61397673449403E-15));
#209580=CARTESIAN_POINT('Ctrl Pts',(-17.467277750751,17.0562847197858,-6.63358257213531E-15));
#209581=CARTESIAN_POINT('Ctrl Pts',(-17.4867746862249,17.042068284606,-1.02232182230849E-14));
#209582=CARTESIAN_POINT('Ctrl Pts',(-17.5064731567169,17.0281304980274,
-1.79912501438622E-14));
#209583=CARTESIAN_POINT('Ctrl Pts',(-17.5263681208433,17.0144778848535,
-3.10862446895044E-15));
#209584=CARTESIAN_POINT('Ctrl Pts',(-17.5422931383847,17.0035495864712,
8.76560179579256E-15));
#209585=CARTESIAN_POINT('Ctrl Pts',(-17.5583454202066,16.9928032530657,
-3.50265831023961E-15));
#209586=CARTESIAN_POINT('Ctrl Pts',(-17.5745064361378,16.9822524120729,
-5.07927033766009E-15));
#209587=CARTESIAN_POINT('Ctrl Pts',(-17.6490341987622,16.9335964008203,
-1.25342314173774E-14));
#209588=CARTESIAN_POINT('Ctrl Pts',(-17.7259441000136,16.8890440749741,
-4.70463702209119E-15));
#209589=CARTESIAN_POINT('Ctrl Pts',(-17.8049552753632,16.8488860377447,
-7.60502771868232E-15));
#209590=CARTESIAN_POINT('Ctrl Pts',(-17.8827964927912,16.8093226406223,
-1.17346642570966E-14));
#209591=CARTESIAN_POINT('Ctrl Pts',(-17.9626778959222,16.774023635519,-1.23541329108695E-14));
#209592=CARTESIAN_POINT('Ctrl Pts',(-18.0443633532837,16.7433042678249,
2.18158824338843E-14));
#209593=CARTESIAN_POINT('Ctrl Pts',(-18.0530581203136,16.7400344355435,
2.54036404748463E-14));
#209594=CARTESIAN_POINT('Ctrl Pts',(-18.0617733522417,16.7368165315127,
-1.30026374349307E-14));
#209595=CARTESIAN_POINT('Ctrl Pts',(-18.0705086335888,16.7336504254972,
1.08246744900953E-14));
#209596=CARTESIAN_POINT('Ctrl Pts',(-19.3965839091052,16.7348410960496,
0.00189100554319172));
#209597=CARTESIAN_POINT('Ctrl Pts',(-20.2210098321597,16.9554454159071,
0.0442829411036698));
#209598=CARTESIAN_POINT('Ctrl Pts',(-21.6178061486211,18.2812774518108,
0.129066812224626));
#209599=CARTESIAN_POINT('Ctrl Pts',(-21.0759342831862,21.1381886893359,
0.25624261890606));
#209600=CARTESIAN_POINT('Ctrl Pts',(-18.3814920744256,22.2205668231227,
0.383418425587494));
#209601=CARTESIAN_POINT('Ctrl Pts',(-16.012474196746,20.5450470987711,0.51059423226893));
#209602=CARTESIAN_POINT('Ctrl Pts',(-16.139244329641,17.6439817266502,0.637770038950362));
#209603=CARTESIAN_POINT('Ctrl Pts',(-18.647082433769,16.1814077892925,0.764945845631799));
#209604=CARTESIAN_POINT('Ctrl Pts',(-21.2343814795738,17.4978560455519,
0.89212165231323));
#209605=CARTESIAN_POINT('Ctrl Pts',(-21.5278812831845,20.386236189992,1.01929745899466));
#209606=CARTESIAN_POINT('Ctrl Pts',(-19.2580928727389,22.1962914237501,
1.1464732656761));
#209607=CARTESIAN_POINT('Ctrl Pts',(-16.5075209839662,21.2675886369871,
1.27364907235753));
#209608=CARTESIAN_POINT('Ctrl Pts',(-15.7995850569884,18.4520614691495,
1.40082487903897));
#209609=CARTESIAN_POINT('Ctrl Pts',(-17.7838032676266,16.3328298801955,
1.5280006857204));
#209610=CARTESIAN_POINT('Ctrl Pts',(-20.6397625254543,16.8541321316718,
1.65517649240184));
#209611=CARTESIAN_POINT('Ctrl Pts',(-21.747305794399,19.5377188342137,1.78235229908327));
#209612=CARTESIAN_POINT('Ctrl Pts',(-20.0903265483327,21.9215589674176,
1.90952810576471));
#209613=CARTESIAN_POINT('Ctrl Pts',(-17.1890026429968,21.8186306868887,
2.03670391244613));
#209614=CARTESIAN_POINT('Ctrl Pts',(-15.7051175219999,19.3233624748623,
2.16387971912757));
#209615=CARTESIAN_POINT('Ctrl Pts',(-17.0000442871287,16.7250089900212,
2.291055525809));
#209616=CARTESIAN_POINT('Ctrl Pts',(-19.8857676903764,16.4073977907608,
2.41823133249044));
#209617=CARTESIAN_POINT('Ctrl Pts',(-21.714815780002,18.6619176945194,2.54540713917187));
#209618=CARTESIAN_POINT('Ctrl Pts',(-20.8091503729495,21.4201864884025,
2.67258294585331));
#209619=CARTESIAN_POINT('Ctrl Pts',(-17.9996633120291,22.1516638202427,
2.79975875253474));
#209620=CARTESIAN_POINT('Ctrl Pts',(-15.8638845764858,20.1852646030015,
2.92693455921618));
#209621=CARTESIAN_POINT('Ctrl Pts',(-16.3612586065907,17.3250380885132,
3.05411036589761));
#209622=CARTESIAN_POINT('Ctrl Pts',(-19.0354755941188,16.1950645685336,
3.18128617257904));
#209623=CARTESIAN_POINT('Ctrl Pts',(-21.4331074368131,17.832024618564,3.30846197926048));
#209624=CARTESIAN_POINT('Ctrl Pts',(-21.3544757311695,20.7341089913131,
3.43563778594192));
#209625=CARTESIAN_POINT('Ctrl Pts',(-18.8717201875366,22.2388353997967,
3.56281359262335));
#209626=CARTESIAN_POINT('Ctrl Pts',(-16.2626149195662,20.9657107573881,
3.68998939930478));
#209627=CARTESIAN_POINT('Ctrl Pts',(-15.9208520715149,18.0827479048318,
3.81716520598622));
#209628=CARTESIAN_POINT('Ctrl Pts',(-18.1599778441559,16.2348863223055,
3.94434101266766));
#209629=CARTESIAN_POINT('Ctrl Pts',(-20.9257333169718,17.11742432065,4.07151681934909));
#209630=CARTESIAN_POINT('Ctrl Pts',(-21.6807095057666,19.9206880628195,
4.19869262603052));
#209631=CARTESIAN_POINT('Ctrl Pts',(-19.7322626164446,22.0728570555698,
4.32586843271195));
#209632=CARTESIAN_POINT('Ctrl Pts',(-16.8679717356974,21.5994498267117,
4.45304423939339));
#209633=CARTESIAN_POINT('Ctrl Pts',(-15.7156459686732,18.934788125763,4.58022004607482));
#209634=CARTESIAN_POINT('Ctrl Pts',(-17.3324726852114,16.5235336757831,
4.70739585275626));
#209635=CARTESIAN_POINT('Ctrl Pts',(-20.2351137244727,16.5778627753009,
4.8345716594377));
#209636=CARTESIAN_POINT('Ctrl Pts',(-21.7605760911555,19.0479318475521,
4.96174746611912));
#209637=CARTESIAN_POINT('Ctrl Pts',(-20.5093427447009,21.6676058285233,
5.08892327280057));
#209638=CARTESIAN_POINT('Ctrl Pts',(-17.6293426201811,22.033496435978,5.216099079482));
#209639=CARTESIAN_POINT('Ctrl Pts',(-15.7627970788757,19.8099217473088,
5.34327488616343));
#209640=CARTESIAN_POINT('Ctrl Pts',(-16.6221458040505,17.0368735287597,
5.47045069284487));
#209641=CARTESIAN_POINT('Ctrl Pts',(-19.4189896775549,16.2584514060663,
5.5976264995263));
#209642=CARTESIAN_POINT('Ctrl Pts',(-21.5873980371568,18.1888093624738,
5.72480230620774));
#209643=CARTESIAN_POINT('Ctrl Pts',(-21.1379907995229,21.0569637845056,
5.85197811288916));
#209644=CARTESIAN_POINT('Ctrl Pts',(-18.4830712118232,22.2315610076874,
5.97915391957061));
#209645=CARTESIAN_POINT('Ctrl Pts',(-16.0583632128787,20.6349809834757,
6.10632972625205));
#209646=CARTESIAN_POINT('Ctrl Pts',(-16.0883858973698,17.7319867891525,
6.23350553293348));
#209647=CARTESIAN_POINT('Ctrl Pts',(-18.545595315694,16.1858954178693,6.36068133961491));
#209648=CARTESIAN_POINT('Ctrl Pts',(-21.1756543381554,17.4151497415253,
6.48785714629635));
#209649=CARTESIAN_POINT('Ctrl Pts',(-21.5656470515186,20.2919852142942,
6.61503295297778));
#209650=CARTESIAN_POINT('Ctrl Pts',(-19.3577793469507,22.1770838464573,
6.74220875965921));
#209651=CARTESIAN_POINT('Ctrl Pts',(-16.577632807668,21.3409846454216,6.86938456634065));
#209652=CARTESIAN_POINT('Ctrl Pts',(-15.7758193281077,18.5507567339681,
6.99656037302208));
#209653=CARTESIAN_POINT('Ctrl Pts',(-17.6879530096092,16.3662610397804,
7.12373617970353));
#209654=CARTESIAN_POINT('Ctrl Pts',(-20.5597698797958,16.7916367771814,
7.25091198638494));
#209655=CARTESIAN_POINT('Ctrl Pts',(-21.7565562053286,19.4366281089017,
7.3780877930664));
#209656=CARTESIAN_POINT('Ctrl Pts',(-20.1803348134679,21.8746196547645,
7.50526359974782));
#209657=CARTESIAN_POINT('Ctrl Pts',(-17.277190999913,21.8689054902615,7.63243940642925));
#209658=CARTESIAN_POINT('Ctrl Pts',(-15.710579024174,19.4247280066634,7.75961521311069));
#209659=CARTESIAN_POINT('Ctrl Pts',(-16.917768139086,16.7844683424076,7.88679101979213));
#209660=CARTESIAN_POINT('Ctrl Pts',(-19.7912372583239,16.3704008664529,
8.01396682647355));
#209661=CARTESIAN_POINT('Ctrl Pts',(-21.6947568125944,18.5624067880616,
8.141142633155));
#209662=CARTESIAN_POINT('Ctrl Pts',(-20.8819657566022,21.3494567253891,
8.26831843983642));
#209663=CARTESIAN_POINT('Ctrl Pts',(-18.0985494367176,22.1746053447652,
8.39549424651787));
#209664=CARTESIAN_POINT('Ctrl Pts',(-15.8981195681347,20.2808300024119,
8.52267005319929));
#209665=CARTESIAN_POINT('Ctrl Pts',(-16.2994339811977,17.4055520339842,
8.64984585988074));
#209666=CARTESIAN_POINT('Ctrl Pts',(-18.9343116103032,16.1866605156374,
8.77702166656217));
#209667=CARTESIAN_POINT('Ctrl Pts',(-21.385415769696,17.7424127625149,8.9041974732436));
#209668=CARTESIAN_POINT('Ctrl Pts',(-21.404010525815,20.6455026489812,9.03137327992503));
#209669=CARTESIAN_POINT('Ctrl Pts',(-18.9730363440416,22.2325253902829,
9.15854908660646));
#209670=CARTESIAN_POINT('Ctrl Pts',(-16.3227611528787,21.0474861230161,
9.28572489328791));
#209671=CARTESIAN_POINT('Ctrl Pts',(-15.8846479455884,18.1775848230658,
9.41290069996933));
#209672=CARTESIAN_POINT('Ctrl Pts',(-18.0606383974872,16.2557778069732,
9.54007650665076));
#209673=CARTESIAN_POINT('Ctrl Pts',(-20.8543963261569,17.0452037312071,
9.66725231333221));
#209674=CARTESIAN_POINT('Ctrl Pts',(-21.7028222322161,19.8216133075819,
9.79442812001364));
#209675=CARTESIAN_POINT('Ctrl Pts',(-19.8275380061061,22.0378230731863,
9.92160392669508));
#209676=CARTESIAN_POINT('Ctrl Pts',(-16.9490005320169,21.6605981215696,
10.0487797333765));
#209677=CARTESIAN_POINT('Ctrl Pts',(-15.7080892802405,19.0360189326189,
10.175955540058));
#209678=CARTESIAN_POINT('Ctrl Pts',(-17.2432633046432,16.5719740124406,
10.3031313467394));
#209679=CARTESIAN_POINT('Ctrl Pts',(-20.1460957214815,16.5290716394223,
10.4303071534208));
#209680=CARTESIAN_POINT('Ctrl Pts',(-21.7534179584054,18.9466720779869,
10.5574829601022));
#209681=CARTESIAN_POINT('Ctrl Pts',(-20.5906116247063,21.6067769789573,
10.6846587667837));
#209682=CARTESIAN_POINT('Ctrl Pts',(-17.7244793596526,22.0689052004239,
10.8118345734651));
#209683=CARTESIAN_POINT('Ctrl Pts',(-15.7845196242002,19.9090827821031,
10.9390103801465));
#209684=CARTESIAN_POINT('Ctrl Pts',(-16.5505250681459,17.1088127391066,
11.066186186828));
#209685=CARTESIAN_POINT('Ctrl Pts',(-19.3197332403295,16.2371690315234,
11.1933619935094));
#209686=CARTESIAN_POINT('Ctrl Pts',(-21.5515675192157,18.0938306607512,
11.3205378001909));
#209687=CARTESIAN_POINT('Ctrl Pts',(-21.1984584771842,20.9754258193904,
11.4477136068723));
#209688=CARTESIAN_POINT('Ctrl Pts',(-18.5843617438802,22.2382698013562,
11.5748894135537));
#209689=CARTESIAN_POINT('Ctrl Pts',(-16.1075488229684,20.7237816341318,
11.7020652202351));
#209690=CARTESIAN_POINT('Ctrl Pts',(-16.0403418410383,17.821410211409,11.8292410269166));
#209691=CARTESIAN_POINT('Ctrl Pts',(-18.4443990326749,16.1939011720493,
11.956416833598));
#209692=CARTESIAN_POINT('Ctrl Pts',(-21.1141471371691,17.3343930450618,
12.0835926402795));
#209693=CARTESIAN_POINT('Ctrl Pts',(-21.6002579719026,20.1965553238665,
12.2107684469609));
#209694=CARTESIAN_POINT('Ctrl Pts',(-19.4567550174485,22.1545317634859,
12.3379442536423));
#209695=CARTESIAN_POINT('Ctrl Pts',(-16.650169193721,21.4120005062925,12.4651200603238));
#209696=CARTESIAN_POINT('Ctrl Pts',(-15.7553687976281,18.6501878940739,
12.5922958670052));
#209697=CARTESIAN_POINT('Ctrl Pts',(-17.593277655009,16.4028855811176,12.7194716736866));
#209698=CARTESIAN_POINT('Ctrl Pts',(-20.4777284627055,16.7318539562487,
12.8466474803681));
#209699=CARTESIAN_POINT('Ctrl Pts',(-21.7624166338639,19.3352849533645,
12.9738232870495));
#209700=CARTESIAN_POINT('Ctrl Pts',(-20.268720508187,21.8246922197625,13.1009990937309));
#209701=CARTESIAN_POINT('Ctrl Pts',(-17.3670135717459,21.9161990985631,
13.2281749004124));
#209702=CARTESIAN_POINT('Ctrl Pts',(-15.7194318384815,19.5258537080241,
13.3553507070938));
#209703=CARTESIAN_POINT('Ctrl Pts',(-16.8375292882087,16.8466495823981,
13.4825265137753));
#209704=CARTESIAN_POINT('Ctrl Pts',(-19.6955209077569,16.3365902167848,
13.6097023204567));
#209705=CARTESIAN_POINT('Ctrl Pts',(-21.6713767731562,18.4636234212799,
13.7368781271381));
#209706=CARTESIAN_POINT('Ctrl Pts',(-20.9523717633484,21.2763282493288,
13.8640539338195));
#209707=CARTESIAN_POINT('Ctrl Pts',(-18.1981483483483,22.1942225973466,
13.991229740501));
#209708=CARTESIAN_POINT('Ctrl Pts',(-15.9355355650343,20.3751953719755,
14.1184055471824));
#209709=CARTESIAN_POINT('Ctrl Pts',(-16.2403402085095,17.4880911509308,
14.2455813538639));
#209710=CARTESIAN_POINT('Ctrl Pts',(-18.8329229366954,16.181648863124,14.3727571605453));
#209711=CARTESIAN_POINT('Ctrl Pts',(-21.334750010313,17.6544482206642,14.4999329672267));
#209712=CARTESIAN_POINT('Ctrl Pts',(-21.450550370219,20.555287225246,14.6271087739081));
#209713=CARTESIAN_POINT('Ctrl Pts',(-19.0740843735804,22.2228261365397,
14.7542845805896));
#209714=CARTESIAN_POINT('Ctrl Pts',(-16.3856120721985,21.1272015025705,
14.881460387271));
#209715=CARTESIAN_POINT('Ctrl Pts',(-15.8516399371812,18.2735809228713,
15.0086361939525));
#209716=CARTESIAN_POINT('Ctrl Pts',(-17.9620542603586,16.2799841636479,
15.1358120006339));
#209717=CARTESIAN_POINT('Ctrl Pts',(-20.7806808873008,16.9754125149182,
15.2629878073153));
#209718=CARTESIAN_POINT('Ctrl Pts',(-21.7216048314868,19.7218536275428,
15.3901636139968));
#209719=CARTESIAN_POINT('Ctrl Pts',(-19.9215867744523,21.9996182440491,
15.5173394206782));
#209720=CARTESIAN_POINT('Ctrl Pts',(-17.0320315618059,21.7189987028083,
15.6445152273596));
#209721=CARTESIAN_POINT('Ctrl Pts',(-15.7039267551279,19.1374460156962,
15.771691034041));
#209722=CARTESIAN_POINT('Ctrl Pts',(-17.1557260830642,16.6233745439076,
15.8988668407225));
#209723=CARTESIAN_POINT('Ctrl Pts',(-20.0554937710623,16.483288821935,16.0260426474039));
#209724=CARTESIAN_POINT('Ctrl Pts',(-21.7428729452643,18.8457088049877,
16.1532184540854));
#209725=CARTESIAN_POINT('Ctrl Pts',(-20.669797943903,21.5432607869357,16.2803942607668));
#209726=CARTESIAN_POINT('Ctrl Pts',(-17.8207484781814,22.1011082533001,
16.4075700674482));
#209727=CARTESIAN_POINT('Ctrl Pts',(-15.8095506009463,20.0074607776102,
16.5347458741296));
#209728=CARTESIAN_POINT('Ctrl Pts',(-16.4813535355424,17.1831099723939,
16.6619216808111));
#209729=CARTESIAN_POINT('Ctrl Pts',(-19.2198197862706,16.2192224024562,
16.7890974874925));
#209730=CARTESIAN_POINT('Ctrl Pts',(-21.5125765364721,18.0001050876052,
16.916273294174));
#209731=CARTESIAN_POINT('Ctrl Pts',(-21.2561617723699,20.8919086982621,
17.0434491008554));
#209732=CARTESIAN_POINT('Ctrl Pts',(-18.6858201251326,22.2415829072234,
17.1706249075368));
#209733=CARTESIAN_POINT('Ctrl Pts',(-16.1596805227059,20.8108853979961,
17.2978007142183));
#209734=CARTESIAN_POINT('Ctrl Pts',(-15.9953192604098,17.9123923361942,
17.4249765208997));
#209735=CARTESIAN_POINT('Ctrl Pts',(-18.3435275949907,16.2052912052522,
17.5521523275811));
#209736=CARTESIAN_POINT('Ctrl Pts',(-21.0499701257169,17.2557413381646,
17.6793281342626));
#209737=CARTESIAN_POINT('Ctrl Pts',(-21.6316538114152,20.1000199362705,
17.806503940944));
#209738=CARTESIAN_POINT('Ctrl Pts',(-19.5549199738189,22.1286779216513,
17.9336797476255));
#209739=CARTESIAN_POINT('Ctrl Pts',(-16.7250430122834,21.4805475054267,
18.0608555543069));
#209740=CARTESIAN_POINT('Ctrl Pts',(-15.7382593970452,18.7502481169883,
18.1880313609883));
#209741=CARTESIAN_POINT('Ctrl Pts',(-17.4998818483857,16.4426599837058,
18.3152071676697));
#209742=CARTESIAN_POINT('Ctrl Pts',(-20.3937311058227,16.6748519928532,
18.4423829743512));
#209743=CARTESIAN_POINT('Ctrl Pts',(-21.7648800881944,19.2338023873838,
18.5695587810326));
#209744=CARTESIAN_POINT('Ctrl Pts',(-20.355384707288,21.7718330069121,18.6967345877141));
#209745=CARTESIAN_POINT('Ctrl Pts',(-17.458369491917,21.9604582855383,18.8239103943955));
#209746=CARTESIAN_POINT('Ctrl Pts',(-15.7316660931769,19.6266262383536,
18.9510862010769));
#209747=CARTESIAN_POINT('Ctrl Pts',(-16.7594177080439,16.911482913106,19.0782620077583));
#209748=CARTESIAN_POINT('Ctrl Pts',(-19.5987260194682,16.3060037929748,
19.2054378144398));
#209749=CARTESIAN_POINT('Ctrl Pts',(-21.6447018788134,18.3656783845019,
19.3326136211212));
#209750=CARTESIAN_POINT('Ctrl Pts',(-21.0202894232019,21.2008830991642,
19.4597894278026));
#209751=CARTESIAN_POINT('Ctrl Pts',(-18.298348324308,22.2104935619801,19.5869652344841));
#209752=CARTESIAN_POINT('Ctrl Pts',(-15.9760905994637,20.468254879066,19.7141410411655));
#209753=CARTESIAN_POINT('Ctrl Pts',(-16.1840435721468,17.5725628250384,
19.841316847847));
#209754=CARTESIAN_POINT('Ctrl Pts',(-18.7314233036763,16.1800352894614,
19.9684926545284));
#209755=CARTESIAN_POINT('Ctrl Pts',(-21.2811669856061,17.5682295538539,
20.0956684612098));
#209756=CARTESIAN_POINT('Ctrl Pts',(-21.4940430697286,20.4635641243438,
20.2228442678912));
#209757=CARTESIAN_POINT('Ctrl Pts',(-19.1747509132239,22.2097481144726,
20.3500200745727));
#209758=CARTESIAN_POINT('Ctrl Pts',(-16.4510972110931,21.2047682572431,
20.4771958812541));
#209759=CARTESIAN_POINT('Ctrl Pts',(-15.821865006984,18.370627026472,20.6043716879356));
#209760=CARTESIAN_POINT('Ctrl Pts',(-17.8643361386242,16.3074811285329,
20.731547494617));
#209761=CARTESIAN_POINT('Ctrl Pts',(-20.7046694479571,16.9081233905683,
20.8587233012984));
#209762=CARTESIAN_POINT('Ctrl Pts',(-21.7370366957551,19.6215316486842,
20.9858991079799));
#209763=CARTESIAN_POINT('Ctrl Pts',(-20.0143025394107,21.9582647545422,
21.1130749146613));
#209764=CARTESIAN_POINT('Ctrl Pts',(-17.1169733995615,21.7746258892963,
21.2402507213427));
#209765=CARTESIAN_POINT('Ctrl Pts',(-15.7031597664495,19.2388788584707,
21.3674265280241));
#209766=CARTESIAN_POINT('Ctrl Pts',(-17.0699655633607,16.677825505383,21.4946023347056));
#209767=CARTESIAN_POINT('Ctrl Pts',(-19.9633972500118,16.4402806602734,
21.621778141387));
#209768=CARTESIAN_POINT('Ctrl Pts',(-21.7289765870023,18.7457048218335,
21.7489539480685));
#209769=CARTESIAN_POINT('Ctrl Pts',(-20.7467662613402,21.4760665062299,
21.8761297547499));
#209770=CARTESIAN_POINT('Ctrl Pts',(-17.9181406714293,22.1321446364483,
22.0033055614313));
#209771=CARTESIAN_POINT('Ctrl Pts',(-15.8372831342433,20.1003769378317,
22.1305000254672));
#209772=CARTESIAN_POINT('Ctrl Pts',(-16.2233209291159,18.2129921341989,
22.2153025539425));
#209773=CARTESIAN_POINT('Ctrl Pts',(-16.7733106534419,17.5599162528134,
22.2577131468574));
#209774=CARTESIAN_POINT('Ctrl Pts',(-19.3578031414673,16.879769673048,-0.0847273919817696));
#209775=CARTESIAN_POINT('Ctrl Pts',(-20.133975749406,17.0874621114807,-0.0423354564212915));
#209776=CARTESIAN_POINT('Ctrl Pts',(-21.4490181436218,18.3356937357163,
0.0424484146996647));
#209777=CARTESIAN_POINT('Ctrl Pts',(-20.9388618188364,21.0253911164874,
0.169624221381099));
#209778=CARTESIAN_POINT('Ctrl Pts',(-18.402124220429,22.0444180968188,0.296800028062534));
#209779=CARTESIAN_POINT('Ctrl Pts',(-16.1717639989072,20.466965862803,0.423975834743968));
#209780=CARTESIAN_POINT('Ctrl Pts',(-16.291114327307,17.7356986710373,0.551151641425402));
#209781=CARTESIAN_POINT('Ctrl Pts',(-18.6521696836906,16.3587285934148,
0.678327448106838));
#209782=CARTESIAN_POINT('Ctrl Pts',(-21.0880351650422,17.5981256668252,
0.805503254788269));
#209783=CARTESIAN_POINT('Ctrl Pts',(-21.3643565441105,20.3174500921447,
0.932679061469706));
#209784=CARTESIAN_POINT('Ctrl Pts',(-19.2274179293257,22.0215635267321,
1.05985486815114));
#209785=CARTESIAN_POINT('Ctrl Pts',(-16.6378358983264,21.1472173376516,
1.18703067483258));
#209786=CARTESIAN_POINT('Ctrl Pts',(-15.9713351742103,18.4964818337432,
1.31420648151401));
#209787=CARTESIAN_POINT('Ctrl Pts',(-17.8394178972337,16.5012880107125,
1.44138228819545));
#209788=CARTESIAN_POINT('Ctrl Pts',(-20.5282190172933,16.9920786527069,
1.56855809487688));
#209789=CARTESIAN_POINT('Ctrl Pts',(-21.5709382276219,19.5185961132746,
1.69573390155831));
#209790=CARTESIAN_POINT('Ctrl Pts',(-20.0109413052122,21.7629110497128,
1.82290970823975));
#209791=CARTESIAN_POINT('Ctrl Pts',(-17.2794307120758,21.6660071197238,
1.95008551492118));
#209792=CARTESIAN_POINT('Ctrl Pts',(-15.8823967857546,19.316785944752,2.07726132160262));
#209793=CARTESIAN_POINT('Ctrl Pts',(-17.101532012187,16.8705130362003,2.20443712828405));
#209794=CARTESIAN_POINT('Ctrl Pts',(-19.8183551942992,16.5714914916967,
2.33161293496548));
#209795=CARTESIAN_POINT('Ctrl Pts',(-21.5403498405985,18.6940552593023,
2.45878874164692));
#209796=CARTESIAN_POINT('Ctrl Pts',(-20.6876926627317,21.2908836986755,
2.58596454832835));
#209797=CARTESIAN_POINT('Ctrl Pts',(-18.0426437407308,21.9795479587692,
2.71314035500979));
#209798=CARTESIAN_POINT('Ctrl Pts',(-16.0318712688937,20.128241290682,2.84031616169122));
#209799=CARTESIAN_POINT('Ctrl Pts',(-16.5001341986149,17.4354226747645,
2.96749196837266));
#209800=CARTESIAN_POINT('Ctrl Pts',(-19.0178303497907,16.3715860469025,
3.09466777505409));
#209801=CARTESIAN_POINT('Ctrl Pts',(-21.275129772553,17.9127354887059,3.22184358173553));
#209802=CARTESIAN_POINT('Ctrl Pts',(-21.2011003487691,20.6449620394061,
3.34901938841696));
#209803=CARTESIAN_POINT('Ctrl Pts',(-18.8636594807816,22.0616174211049,
3.4761951950984));
#209804=CARTESIAN_POINT('Ctrl Pts',(-16.4072640866091,20.8630082479868,
3.60337100177983));
#209805=CARTESIAN_POINT('Ctrl Pts',(-16.0855044795293,18.1487840426529,
3.73054680846126));
#209806=CARTESIAN_POINT('Ctrl Pts',(-18.1935751282717,16.4090770495669,
3.8577226151427));
#209807=CARTESIAN_POINT('Ctrl Pts',(-20.7974520542944,17.2399604565832,
3.98489842182413));
#209808=CARTESIAN_POINT('Ctrl Pts',(-21.50823979277,19.8791503081571,4.11207422850556));
#209809=CARTESIAN_POINT('Ctrl Pts',(-19.6738347101252,21.9053537220903,
4.239250035187));
#209810=CARTESIAN_POINT('Ctrl Pts',(-16.9771896136586,21.4596548264534,
4.36642584186844));
#209811=CARTESIAN_POINT('Ctrl Pts',(-15.8923090067117,18.9509546948064,
4.49360164854987));
#209812=CARTESIAN_POINT('Ctrl Pts',(-17.4145035108715,16.6808299904415,
4.62077745523131));
#209813=CARTESIAN_POINT('Ctrl Pts',(-20.1472541466187,16.7319792297855,
4.74795326191273));
#209814=CARTESIAN_POINT('Ctrl Pts',(-21.5834318192879,19.0574761604191,
4.87512906859417));
#209815=CARTESIAN_POINT('Ctrl Pts',(-20.4054326534448,21.5238216851043,
5.00230487527561));
#209816=CARTESIAN_POINT('Ctrl Pts',(-17.6939977688763,21.8682968636094,
5.12948068195703));
#209817=CARTESIAN_POINT('Ctrl Pts',(-15.9367003815454,19.7748671001969,
5.25665648863848));
#209818=CARTESIAN_POINT('Ctrl Pts',(-16.7457517741515,17.164124269893,5.38383229531991));
#209819=CARTESIAN_POINT('Ctrl Pts',(-19.3788975093713,16.4312628785266,
5.51100810200134));
#209820=CARTESIAN_POINT('Ctrl Pts',(-21.4203898065964,18.2486377661686,
5.63818390868278));
#209821=CARTESIAN_POINT('Ctrl Pts',(-20.9972861924251,20.9489202724142,
5.76535971536421));
#209822=CARTESIAN_POINT('Ctrl Pts',(-18.4977579720875,22.0547687962171,
5.89253552204564));
#209823=CARTESIAN_POINT('Ctrl Pts',(-16.2149671495256,20.5516359536883,
6.01971132872709));
#209824=CARTESIAN_POINT('Ctrl Pts',(-16.2432326184625,17.8185528329019,
6.14688713540851));
#209825=CARTESIAN_POINT('Ctrl Pts',(-18.5566225655012,16.36295356291,6.27406294208995));
#209826=CARTESIAN_POINT('Ctrl Pts',(-21.0327452994073,17.5202601292503,
6.40123874877139));
#209827=CARTESIAN_POINT('Ctrl Pts',(-21.3999118973314,20.2287155878522,
6.52841455545281));
#209828=CARTESIAN_POINT('Ctrl Pts',(-19.3212697946072,22.0034801611529,
6.65559036213426));
#209829=CARTESIAN_POINT('Ctrl Pts',(-16.703844105405,21.2163175074616,6.78276616881569));
#209830=CARTESIAN_POINT('Ctrl Pts',(-15.9489604438082,18.5894005047157,
6.90994197549712));
#209831=CARTESIAN_POINT('Ctrl Pts',(-17.7491777159676,16.5327624580774,
7.03711778217856));
#209832=CARTESIAN_POINT('Ctrl Pts',(-20.4529083087621,16.9332411259839,
7.16429358885998));
#209833=CARTESIAN_POINT('Ctrl Pts',(-21.5796472157492,19.4234221871405,
7.29146939554142));
#209834=CARTESIAN_POINT('Ctrl Pts',(-20.0956814230716,21.7187190760035,
7.41864520222286));
#209835=CARTESIAN_POINT('Ctrl Pts',(-17.3624574402067,21.7133393592328,
7.54582100890429));
#209836=CARTESIAN_POINT('Ctrl Pts',(-15.8875386284201,19.4122185930627,
7.67299681558573));
#209837=CARTESIAN_POINT('Ctrl Pts',(-17.0240714537406,16.9264922567919,
7.80017262226716));
#209838=CARTESIAN_POINT('Ctrl Pts',(-19.7293575901193,16.5366599823728,
7.9273484289486));
#209839=CARTESIAN_POINT('Ctrl Pts',(-21.5214649164229,18.6003686858652,
8.05452423563003));
#209840=CARTESIAN_POINT('Ctrl Pts',(-20.756246191493,21.2242937200225,8.18170004231146));
#209841=CARTESIAN_POINT('Ctrl Pts',(-18.1357421006224,22.0011467251603,
8.3088758489929));
#209842=CARTESIAN_POINT('Ctrl Pts',(-16.0641025003577,20.2182132859998,
8.43605165567432));
#209843=CARTESIAN_POINT('Ctrl Pts',(-16.4419281434871,17.5112241716414,
8.56322746235577));
#209844=CARTESIAN_POINT('Ctrl Pts',(-18.9225874529435,16.3636738798159,
8.6904032690372));
#209845=CARTESIAN_POINT('Ctrl Pts',(-21.2302294793815,17.8283685782694,
8.81757907571863));
#209846=CARTESIAN_POINT('Ctrl Pts',(-21.2477358919618,20.5615417903765,
8.94475488240009));
#209847=CARTESIAN_POINT('Ctrl Pts',(-18.9590456437123,22.0556767338902,
9.07193068908149));
#209848=CARTESIAN_POINT('Ctrl Pts',(-16.4638899852646,20.9399973346102,
9.19910649576295));
#209849=CARTESIAN_POINT('Ctrl Pts',(-16.0514193664187,18.2380701945025,
9.32628230244436));
#209850=CARTESIAN_POINT('Ctrl Pts',(-18.1000499791517,16.4287457641048,
9.45345810912581));
#209851=CARTESIAN_POINT('Ctrl Pts',(-20.7302903886372,17.1719669089676,
9.58063391580724));
#209852=CARTESIAN_POINT('Ctrl Pts',(-21.5290582703031,19.7858743581861,
9.70780972248867));
#209853=CARTESIAN_POINT('Ctrl Pts',(-19.7635336698473,21.8723702644956,
9.83498552917011));
#209854=CARTESIAN_POINT('Ctrl Pts',(-17.0534758273726,21.5172241363981,
9.96216133585154));
#209855=CARTESIAN_POINT('Ctrl Pts',(-15.88519460819,19.0462605035686,10.089337142533));
#209856=CARTESIAN_POINT('Ctrl Pts',(-17.3305155191891,16.7264351338286,
10.2165129492144));
#209857=CARTESIAN_POINT('Ctrl Pts',(-20.0634463312613,16.6860438193137,
10.3436887558959));
#209858=CARTESIAN_POINT('Ctrl Pts',(-21.5766926491464,18.9621430841235,
10.4708645625773));
#209859=CARTESIAN_POINT('Ctrl Pts',(-20.4819448988438,21.466553123448,10.5980403692588));
#209860=CARTESIAN_POINT('Ctrl Pts',(-17.7835661935479,21.9016331674242,
10.7252161759402));
#209861=CARTESIAN_POINT('Ctrl Pts',(-15.9571515150968,19.8682242798172,
10.8523919826216));
#209862=CARTESIAN_POINT('Ctrl Pts',(-16.6783229708898,17.2318529074172,
10.9795677893031));
#209863=CARTESIAN_POINT('Ctrl Pts',(-19.2854505111856,16.4112261527396,
11.1067435959845));
#209864=CARTESIAN_POINT('Ctrl Pts',(-21.3866564343474,18.1592181293605,
11.2339194026659));
#209865=CARTESIAN_POINT('Ctrl Pts',(-21.0542147214219,20.8721546913479,
11.3610952093473));
#209866=CARTESIAN_POINT('Ctrl Pts',(-18.5931200103587,22.0610849269117,
11.4882710160288));
#209867=CARTESIAN_POINT('Ctrl Pts',(-16.261273945793,20.6352391382547,11.6154468227102));
#209868=CARTESIAN_POINT('Ctrl Pts',(-16.1980005612746,17.9027423384994,
11.7426226293916));
#209869=CARTESIAN_POINT('Ctrl Pts',(-18.4613492599099,16.3704907435428,
11.8697984360731));
#209870=CARTESIAN_POINT('Ctrl Pts',(-20.9748380899644,17.4442300894981,
11.9969742427545));
#209871=CARTESIAN_POINT('Ctrl Pts',(-21.4324970545739,20.138871170231,12.124150049436));
#209872=CARTESIAN_POINT('Ctrl Pts',(-19.4144524592281,21.9822480424568,
12.2513258561174));
#209873=CARTESIAN_POINT('Ctrl Pts',(-16.7721349661832,21.2831768387803,
12.3785016627988));
#209874=CARTESIAN_POINT('Ctrl Pts',(-15.9297068745883,18.6830119993224,
12.5056774694802));
#209875=CARTESIAN_POINT('Ctrl Pts',(-17.6600436714977,16.5672433798551,
12.6328532761617));
#209876=CARTESIAN_POINT('Ctrl Pts',(-20.3756687425606,16.876957369329,12.7600290828431));
#209877=CARTESIAN_POINT('Ctrl Pts',(-21.5851646357777,19.3280106054199,
12.8872048895246));
#209878=CARTESIAN_POINT('Ctrl Pts',(-20.1788939389038,21.6717138735354,
13.014380696206));
#209879=CARTESIAN_POINT('Ctrl Pts',(-17.4470227333175,21.7578648918097,
13.1415565028874));
#209880=CARTESIAN_POINT('Ctrl Pts',(-15.8958732910946,19.5074254481115,
13.2687323095689));
#209881=CARTESIAN_POINT('Ctrl Pts',(-16.9485289502823,16.9850340540092,
13.3959081162503));
#209882=CARTESIAN_POINT('Ctrl Pts',(-19.6392434787545,16.5048282563255,
13.5230839229317));
#209883=CARTESIAN_POINT('Ctrl Pts',(-21.4994533012164,18.5073670695018,
13.6502597296132));
#209884=CARTESIAN_POINT('Ctrl Pts',(-20.8225313632018,21.1554454240253,
13.7774355362946));
#209885=CARTESIAN_POINT('Ctrl Pts',(-18.2295115283253,22.0196157878994,
13.904611342976));
#209886=CARTESIAN_POINT('Ctrl Pts',(-16.0993285541244,20.3070554887315,
14.0317871496575));
#209887=CARTESIAN_POINT('Ctrl Pts',(-16.3862931053621,17.5889323075283,
14.1589629563389));
#209888=CARTESIAN_POINT('Ctrl Pts',(-18.8271330173065,16.3589555572926,
14.2861387630203));
#209889=CARTESIAN_POINT('Ctrl Pts',(-21.1825291663591,17.745552565399,14.4133145697018));
#209890=CARTESIAN_POINT('Ctrl Pts',(-21.2915517781366,20.476606638826,14.5404903763832));
#209891=CARTESIAN_POINT('Ctrl Pts',(-19.0541793730395,22.0465451735372,
14.6676661830647));
#209892=CARTESIAN_POINT('Ctrl Pts',(-16.5230622657518,21.0150470053099,
14.7948419897461));
#209893=CARTESIAN_POINT('Ctrl Pts',(-16.0203433033647,18.328447681496,14.9220177964275));
#209894=CARTESIAN_POINT('Ctrl Pts',(-18.0072359316107,16.4515353325348,
15.0491936031089));
#209895=CARTESIAN_POINT('Ctrl Pts',(-20.6608894845385,17.1062605442799,
15.1763694097904));
#209896=CARTESIAN_POINT('Ctrl Pts',(-21.5467415316516,19.6919535717847,
15.3035452164718));
#209897=CARTESIAN_POINT('Ctrl Pts',(-19.8520778019025,21.8364015485223,
15.4307210231533));
#209898=CARTESIAN_POINT('Ctrl Pts',(-17.1316470846427,21.5722065552882,
15.5578968298347));
#209899=CARTESIAN_POINT('Ctrl Pts',(-15.8812757139849,19.1417511005842,
15.6850726365161));
#209900=CARTESIAN_POINT('Ctrl Pts',(-17.2481018157082,16.7748272130226,
15.8122484431975));
#209901=CARTESIAN_POINT('Ctrl Pts',(-19.9781472762768,16.6429406515769,
15.939424249879));
#209902=CARTESIAN_POINT('Ctrl Pts',(-21.5667648313502,18.8670891505701,
16.0666000565604));
#209903=CARTESIAN_POINT('Ctrl Pts',(-20.5564964748742,21.4067545084005,
16.1937758632419));
#209904=CARTESIAN_POINT('Ctrl Pts',(-17.8742007195895,21.9319513886684,
16.3209516699233));
#209905=CARTESIAN_POINT('Ctrl Pts',(-15.9807174389196,19.9608442511223,
16.4481274766047));
#209906=CARTESIAN_POINT('Ctrl Pts',(-16.6132000200527,17.3018015537547,
16.5753032832862));
#209907=CARTESIAN_POINT('Ctrl Pts',(-19.1913849510953,16.3943299325974,
16.7024790899676));
#209908=CARTESIAN_POINT('Ctrl Pts',(-21.3499475780197,18.0709782760214,
16.829654896649));
#209909=CARTESIAN_POINT('Ctrl Pts',(-21.1085406661289,20.7935257934676,
16.9568307033305));
#209910=CARTESIAN_POINT('Ctrl Pts',(-18.6886400736801,22.0642041180355,
17.0840065100119));
#209911=CARTESIAN_POINT('Ctrl Pts',(-16.3103543982751,20.7172447541254,
17.2111823166934));
#209912=CARTESIAN_POINT('Ctrl Pts',(-16.1556131340415,17.9883993163983,
17.3383581233747));
#209913=CARTESIAN_POINT('Ctrl Pts',(-18.3663817865876,16.381214122719,17.4655339300562));
#209914=CARTESIAN_POINT('Ctrl Pts',(-20.9144173329798,17.3701818351261,
17.5927097367376));
#209915=CARTESIAN_POINT('Ctrl Pts',(-21.4620553083253,20.0479859597428,
17.7198855434191));
#209916=CARTESIAN_POINT('Ctrl Pts',(-19.5068718604908,21.9579074155056,
17.8470613501005));
#209917=CARTESIAN_POINT('Ctrl Pts',(-16.8426264504933,21.347711809839,17.9742371567819));
#209918=CARTESIAN_POINT('Ctrl Pts',(-15.9135988802868,18.7772157379466,
18.1014129634634));
#209919=CARTESIAN_POINT('Ctrl Pts',(-17.5721142835804,16.6046898027813,
18.2285887701448));
#209920=CARTESIAN_POINT('Ctrl Pts',(-20.2965877169299,16.8232917077465,
18.3557645768262));
#209921=CARTESIAN_POINT('Ctrl Pts',(-21.5874839051248,19.2324677728927,
18.4829403835077));
#209922=CARTESIAN_POINT('Ctrl Pts',(-20.2604857175586,21.6219484889878,
18.6101161901891));
#209923=CARTESIAN_POINT('Ctrl Pts',(-17.5330316285098,21.7995336065107,
18.7372919968706));
#209924=CARTESIAN_POINT('Ctrl Pts',(-15.9073914798215,19.6022998030865,
18.864467803552));
#209925=CARTESIAN_POINT('Ctrl Pts',(-16.874989209244,17.0460727161496,18.9916436102334));
#209926=CARTESIAN_POINT('Ctrl Pts',(-19.5481139560441,16.4760320435035,
19.1188194169148));
#209927=CARTESIAN_POINT('Ctrl Pts',(-21.4743396776274,18.4151547160267,
19.2459952235963));
#209928=CARTESIAN_POINT('Ctrl Pts',(-20.8864738299528,21.08441604792,19.3731710302777));
#209929=CARTESIAN_POINT('Ctrl Pts',(-18.3238468403057,22.0349344195679,
19.5003468369591));
#209930=CARTESIAN_POINT('Ctrl Pts',(-16.1375099188267,20.3946682605915,
19.6275226436406));
#209931=CARTESIAN_POINT('Ctrl Pts',(-16.3332914883073,17.6684598887888,
19.754698450322));
#209932=CARTESIAN_POINT('Ctrl Pts',(-18.7315741166677,16.3574364254427,
19.8818742570035));
#209933=CARTESIAN_POINT('Ctrl Pts',(-21.1320823343698,17.6643802422104,
20.0090500636849));
#209934=CARTESIAN_POINT('Ctrl Pts',(-21.3324988675726,20.390252053842,20.1362258703664));
#209935=CARTESIAN_POINT('Ctrl Pts',(-19.1489539409205,22.0342326028009,
20.2634016770477));
#209936=CARTESIAN_POINT('Ctrl Pts',(-16.5847145860095,21.0880738092713,
20.3905774837292));
#209937=CARTESIAN_POINT('Ctrl Pts',(-15.9923110877633,18.4198137159881,
20.5177532904106));
#209938=CARTESIAN_POINT('Ctrl Pts',(-17.9152372119337,16.4774229112103,
20.6449290970921));
#209939=CARTESIAN_POINT('Ctrl Pts',(-20.5893269639303,17.0429098251043,
20.7721049037735));
#209940=CARTESIAN_POINT('Ctrl Pts',(-21.5612701751591,19.5975033976856,
20.8992807104549));
#209941=CARTESIAN_POINT('Ctrl Pts',(-19.9393669507179,21.7974684619948,
21.0264565171363));
#209942=CARTESIAN_POINT('Ctrl Pts',(-17.2116173110634,21.6245779050981,
21.1536323238178));
#209943=CARTESIAN_POINT('Ctrl Pts',(-15.8805536168431,19.2372471201844,
21.2808081304992));
#209944=CARTESIAN_POINT('Ctrl Pts',(-17.1673608244619,16.8260911817933,
21.4079839371807));
#209945=CARTESIAN_POINT('Ctrl Pts',(-19.8914411272743,16.6024497401849,
21.535159743862));
#209946=CARTESIAN_POINT('Ctrl Pts',(-21.5536818213048,18.7729383600156,
21.6623355505436));
#209947=CARTESIAN_POINT('Ctrl Pts',(-20.628959867889,21.3434930817089,21.7895113572249));
#209948=CARTESIAN_POINT('Ctrl Pts',(-17.9658925872421,21.9611712248908,
21.9166871639064));
#209949=CARTESIAN_POINT('Ctrl Pts',(-16.0068267982834,20.0483220661474,
22.0438816279422));
#209950=CARTESIAN_POINT('Ctrl Pts',(-16.370269957493,18.2714051300663,22.1286841564175));
#209951=CARTESIAN_POINT('Ctrl Pts',(-16.888069006179,17.6565535153103,22.1710947493324));
#209952=CARTESIAN_POINT('Ctrl Pts',(-19.3190223738293,17.0246982500464,
-0.171345789506731));
#209953=CARTESIAN_POINT('Ctrl Pts',(-20.0469416666524,17.2194788070544,
-0.128953853946253));
#209954=CARTESIAN_POINT('Ctrl Pts',(-21.2802301386225,18.3901100196218,
-0.0441699828252965));
#209955=CARTESIAN_POINT('Ctrl Pts',(-20.8017893544867,20.9125935436388,
0.0830058238561378));
#209956=CARTESIAN_POINT('Ctrl Pts',(-18.4227563664326,21.868269370515,0.210181630537572));
#209957=CARTESIAN_POINT('Ctrl Pts',(-16.3310538010686,20.388884626835,0.337357437219006));
#209958=CARTESIAN_POINT('Ctrl Pts',(-16.4429843249731,17.8274156154244,
0.46453324390044));
#209959=CARTESIAN_POINT('Ctrl Pts',(-18.6572569336122,16.5360493975372,
0.591709050581876));
#209960=CARTESIAN_POINT('Ctrl Pts',(-20.9416888505105,17.6983952880986,
0.718884857263308));
#209961=CARTESIAN_POINT('Ctrl Pts',(-21.2008318050364,20.2486639942973,
0.846060663944744));
#209962=CARTESIAN_POINT('Ctrl Pts',(-19.1967429859123,21.846835629714,0.973236470626179));
#209963=CARTESIAN_POINT('Ctrl Pts',(-16.7681508126867,21.0268460383161,
1.10041227730761));
#209964=CARTESIAN_POINT('Ctrl Pts',(-16.1430852914322,18.540902198337,1.22758808398905));
#209965=CARTESIAN_POINT('Ctrl Pts',(-17.8950325268407,16.6697461412296,
1.35476389067048));
#209966=CARTESIAN_POINT('Ctrl Pts',(-20.4166755091321,17.130025173742,1.48193969735192));
#209967=CARTESIAN_POINT('Ctrl Pts',(-21.3945706608446,19.4994733923354,
1.60911550403335));
#209968=CARTESIAN_POINT('Ctrl Pts',(-19.9315560620918,21.6042631320078,
1.73629131071478));
#209969=CARTESIAN_POINT('Ctrl Pts',(-17.3698587811547,21.5133835525588,
1.86346711739622));
#209970=CARTESIAN_POINT('Ctrl Pts',(-16.0596760495093,19.3102094146417,
1.99064292407765));
#209971=CARTESIAN_POINT('Ctrl Pts',(-17.2030197372453,17.0160170823794,
2.11781873075909));
#209972=CARTESIAN_POINT('Ctrl Pts',(-19.750942698222,16.7355851926327,2.24499453744052));
#209973=CARTESIAN_POINT('Ctrl Pts',(-21.365883901195,18.7261928240851,2.37217034412196));
#209974=CARTESIAN_POINT('Ctrl Pts',(-20.5662349525139,21.1615809089484,
2.49934615080339));
#209975=CARTESIAN_POINT('Ctrl Pts',(-18.0856241694325,21.8074320972958,
2.62652195748482));
#209976=CARTESIAN_POINT('Ctrl Pts',(-16.1998579613017,20.0712179783623,
2.75369776416626));
#209977=CARTESIAN_POINT('Ctrl Pts',(-16.6390097906391,17.5458072610157,
2.8808735708477));
#209978=CARTESIAN_POINT('Ctrl Pts',(-19.0001851054626,16.5481075252713,
3.00804937752912));
#209979=CARTESIAN_POINT('Ctrl Pts',(-21.1171521082928,17.9934463588478,
3.13522518421057));
#209980=CARTESIAN_POINT('Ctrl Pts',(-21.0477249663689,20.5558150874991,
3.26240099089199));
#209981=CARTESIAN_POINT('Ctrl Pts',(-18.8555987740266,21.8843994424129,
3.38957679757343));
#209982=CARTESIAN_POINT('Ctrl Pts',(-16.5519132536521,20.7603057385855,
3.51675260425486));
#209983=CARTESIAN_POINT('Ctrl Pts',(-16.2501568875435,18.214820180474,3.64392841093631));
#209984=CARTESIAN_POINT('Ctrl Pts',(-18.2271724123875,16.5832677768283,
3.77110421761772));
#209985=CARTESIAN_POINT('Ctrl Pts',(-20.6691707916169,17.3624965925164,
3.89828002429917));
#209986=CARTESIAN_POINT('Ctrl Pts',(-21.3357700797732,19.8376125534949,
4.0254558309806));
#209987=CARTESIAN_POINT('Ctrl Pts',(-19.6154068038058,21.7378503886108,
4.15263163766203));
#209988=CARTESIAN_POINT('Ctrl Pts',(-17.0864074916199,21.3198598261951,
4.27980744434348));
#209989=CARTESIAN_POINT('Ctrl Pts',(-16.06897204475,18.9671212638499,4.4069832510249));
#209990=CARTESIAN_POINT('Ctrl Pts',(-17.4965343365317,16.8381263050999,
4.53415905770634));
#209991=CARTESIAN_POINT('Ctrl Pts',(-20.0593945687647,16.8860956842701,
4.66133486438777));
#209992=CARTESIAN_POINT('Ctrl Pts',(-21.4062875474204,19.0670204732863,
4.7885106710692));
#209993=CARTESIAN_POINT('Ctrl Pts',(-20.3015225621888,21.3800375416853,
4.91568647775065));
#209994=CARTESIAN_POINT('Ctrl Pts',(-17.7586529175715,21.7030972912407,
5.04286228443207));
#209995=CARTESIAN_POINT('Ctrl Pts',(-16.1106036842152,19.7398124530851,
5.17003809111352));
#209996=CARTESIAN_POINT('Ctrl Pts',(-16.8693577442526,17.2913750110263,
5.29721389779494));
#209997=CARTESIAN_POINT('Ctrl Pts',(-19.3388053411876,16.604074350987,5.42438970447638));
#209998=CARTESIAN_POINT('Ctrl Pts',(-21.253381576036,18.3084661698633,5.55156551115781));
#209999=CARTESIAN_POINT('Ctrl Pts',(-20.8565815853272,20.8408767603229,
5.67874131783925));
#210000=CARTESIAN_POINT('Ctrl Pts',(-18.5124447323517,21.877976584747,5.80591712452068));
#210001=CARTESIAN_POINT('Ctrl Pts',(-16.3715710861727,20.468290923901,5.93309293120211));
#210002=CARTESIAN_POINT('Ctrl Pts',(-16.3980793395551,17.9051188766514,
6.06026873788356));
#210003=CARTESIAN_POINT('Ctrl Pts',(-18.5676498153085,16.5400117079507,
6.18744454456498));
#210004=CARTESIAN_POINT('Ctrl Pts',(-20.8898362606593,17.6253705169753,
6.31462035124643));
#210005=CARTESIAN_POINT('Ctrl Pts',(-21.2341767431441,20.1654459614101,
6.44179615792784));
#210006=CARTESIAN_POINT('Ctrl Pts',(-19.2847602422637,21.8298764758485,
6.56897196460929));
#210007=CARTESIAN_POINT('Ctrl Pts',(-16.8300554031422,21.0916503695018,
6.69614777129072));
#210008=CARTESIAN_POINT('Ctrl Pts',(-16.1221015595086,18.6280442754634,
6.82332357797216));
#210009=CARTESIAN_POINT('Ctrl Pts',(-17.8104024223259,16.6992638763745,
6.95049938465359));
#210010=CARTESIAN_POINT('Ctrl Pts',(-20.3460467377283,17.0748454747864,
7.07767519133502));
#210011=CARTESIAN_POINT('Ctrl Pts',(-21.4027382261697,19.4102162653792,
7.20485099801646));
#210012=CARTESIAN_POINT('Ctrl Pts',(-20.0110280326754,21.5628184972425,
7.33202680469789));
#210013=CARTESIAN_POINT('Ctrl Pts',(-17.4477238805002,21.5577732282041,
7.45920261137933));
#210014=CARTESIAN_POINT('Ctrl Pts',(-16.0644982326662,19.3997091794621,
7.58637841806076));
#210015=CARTESIAN_POINT('Ctrl Pts',(-17.1303747683952,17.0685161711762,
7.7135542247422));
#210016=CARTESIAN_POINT('Ctrl Pts',(-19.6674779219145,16.7029190982927,
7.84073003142363));
#210017=CARTESIAN_POINT('Ctrl Pts',(-21.3481730202512,18.6383305836686,
7.96790583810506));
#210018=CARTESIAN_POINT('Ctrl Pts',(-20.6305266263839,21.0991307146561,
8.0950816447865));
#210019=CARTESIAN_POINT('Ctrl Pts',(-18.1729347645271,21.8276881055553,
8.22225745146793));
#210020=CARTESIAN_POINT('Ctrl Pts',(-16.2300854325808,20.1555965695878,
8.34943325814937));
#210021=CARTESIAN_POINT('Ctrl Pts',(-16.5844223057765,17.6168963092987,
8.4766090648308));
#210022=CARTESIAN_POINT('Ctrl Pts',(-18.9108632955837,16.5406872439944,
8.60378487151224));
#210023=CARTESIAN_POINT('Ctrl Pts',(-21.075043189067,17.9143243940239,8.73096067819366));
#210024=CARTESIAN_POINT('Ctrl Pts',(-21.0914612581086,20.4775809317718,
8.85813648487511));
#210025=CARTESIAN_POINT('Ctrl Pts',(-18.945054943383,21.8788280774976,8.98531229155654));
#210026=CARTESIAN_POINT('Ctrl Pts',(-16.6050188176507,20.8325085462043,
9.11248809823798));
#210027=CARTESIAN_POINT('Ctrl Pts',(-16.218190787249,18.2985555659393,9.23966390491941));
#210028=CARTESIAN_POINT('Ctrl Pts',(-18.1394615608164,16.6017137212363,
9.36683971160084));
#210029=CARTESIAN_POINT('Ctrl Pts',(-20.6061844511175,17.2987300867281,
9.49401551828229));
#210030=CARTESIAN_POINT('Ctrl Pts',(-21.3552943083903,19.7501354087903,
9.62119132496371));
#210031=CARTESIAN_POINT('Ctrl Pts',(-19.6995293335885,21.7069174558048,
9.74836713164515));
#210032=CARTESIAN_POINT('Ctrl Pts',(-17.1579511227282,21.3738501512268,
9.87554293832658));
#210033=CARTESIAN_POINT('Ctrl Pts',(-16.0622999361394,19.0565020745182,
10.002718745008));
#210034=CARTESIAN_POINT('Ctrl Pts',(-17.4177677337352,16.8808962552165,
10.1298945516894));
#210035=CARTESIAN_POINT('Ctrl Pts',(-19.980796941041,16.8430159992049,10.2570703583709));
#210036=CARTESIAN_POINT('Ctrl Pts',(-21.3999673398873,18.9776140902601,
10.3842461650523));
#210037=CARTESIAN_POINT('Ctrl Pts',(-20.3732781729815,21.3263292679386,
10.5114219717337));
#210038=CARTESIAN_POINT('Ctrl Pts',(-17.8426530274432,21.7343611344247,
10.6385977784151));
#210039=CARTESIAN_POINT('Ctrl Pts',(-16.1297834059934,19.8273657775314,
10.7657735850966));
#210040=CARTESIAN_POINT('Ctrl Pts',(-16.8061208736337,17.3548930757276,
10.892949391778));
#210041=CARTESIAN_POINT('Ctrl Pts',(-19.2511677820415,16.5852832739556,
11.0201251984594));
#210042=CARTESIAN_POINT('Ctrl Pts',(-21.2217453494789,18.2246055979698,
11.1473010051409));
#210043=CARTESIAN_POINT('Ctrl Pts',(-20.9099709656597,20.7688835633054,
11.2744768118223));
#210044=CARTESIAN_POINT('Ctrl Pts',(-18.6018782768372,21.8839000524673,
11.4016526185037));
#210045=CARTESIAN_POINT('Ctrl Pts',(-16.4149990686176,20.5466966423776,
11.5288284251852));
#210046=CARTESIAN_POINT('Ctrl Pts',(-16.3556592815108,17.9840744655897,
11.6560042318666));
#210047=CARTESIAN_POINT('Ctrl Pts',(-18.4782994871448,16.5470803150364,
11.783180038548));
#210048=CARTESIAN_POINT('Ctrl Pts',(-20.8355290427597,17.5540671339344,
11.9103558452295));
#210049=CARTESIAN_POINT('Ctrl Pts',(-21.2647361372453,20.0811870165956,
12.0375316519109));
#210050=CARTESIAN_POINT('Ctrl Pts',(-19.3721499010078,21.8099643214279,
12.1647074585924));
#210051=CARTESIAN_POINT('Ctrl Pts',(-16.8941007386454,21.1543531712681,
12.2918832652738));
#210052=CARTESIAN_POINT('Ctrl Pts',(-16.1040449515487,18.7158361045709,
12.4190590719552));
#210053=CARTESIAN_POINT('Ctrl Pts',(-17.7268096879865,16.7316011785925,
12.5462348786367));
#210054=CARTESIAN_POINT('Ctrl Pts',(-20.2736090224157,17.0220607824092,
12.6734106853181));
#210055=CARTESIAN_POINT('Ctrl Pts',(-21.4079126376915,19.3207362574753,
12.8005864919995));
#210056=CARTESIAN_POINT('Ctrl Pts',(-20.0890673696206,21.5187355273081,
12.9277622986809));
#210057=CARTESIAN_POINT('Ctrl Pts',(-17.5270318948891,21.5995306850564,
13.0549381053624));
#210058=CARTESIAN_POINT('Ctrl Pts',(-16.0723147437075,19.4889971881991,
13.1821139120438));
#210059=CARTESIAN_POINT('Ctrl Pts',(-17.0595286123559,17.1234185256205,
13.3092897187253));
#210060=CARTESIAN_POINT('Ctrl Pts',(-19.5829660497523,16.6730662958661,
13.4364655254067));
#210061=CARTESIAN_POINT('Ctrl Pts',(-21.3275298292767,18.5511107177236,
13.5636413320881));
#210062=CARTESIAN_POINT('Ctrl Pts',(-20.6926909630551,21.0345625987219,
13.6908171387696));
#210063=CARTESIAN_POINT('Ctrl Pts',(-18.2608747083023,21.8450089784522,
13.817992945451));
#210064=CARTESIAN_POINT('Ctrl Pts',(-16.2631215432146,20.2389156054877,
13.9451687521324));
#210065=CARTESIAN_POINT('Ctrl Pts',(-16.5322460022147,17.6897734641258,
14.0723445588139));
#210066=CARTESIAN_POINT('Ctrl Pts',(-18.8213430979177,16.5362622514614,
14.1995203654953));
#210067=CARTESIAN_POINT('Ctrl Pts',(-21.0303083224052,17.8366569101336,
14.3266961721767));
#210068=CARTESIAN_POINT('Ctrl Pts',(-21.1325531860542,20.3979260524059,
14.4538719788582));
#210069=CARTESIAN_POINT('Ctrl Pts',(-19.0342743724987,21.8702642105349,
14.5810477855396));
#210070=CARTESIAN_POINT('Ctrl Pts',(-16.6605124593049,20.9028925080494,
14.708223592221));
#210071=CARTESIAN_POINT('Ctrl Pts',(-16.1890466695481,18.3833144401207,
14.8353993989025));
#210072=CARTESIAN_POINT('Ctrl Pts',(-18.0524176028627,16.6230865014217,
14.9625752055839));
#210073=CARTESIAN_POINT('Ctrl Pts',(-20.5410980817764,17.2371085736416,
15.0897510122653));
#210074=CARTESIAN_POINT('Ctrl Pts',(-21.3718782318164,19.6620535160264,
15.2169268189468));
#210075=CARTESIAN_POINT('Ctrl Pts',(-19.7825688293528,21.6731848529956,
15.3441026256282));
#210076=CARTESIAN_POINT('Ctrl Pts',(-17.2312626074793,21.4254144077681,
15.4712784323096));
#210077=CARTESIAN_POINT('Ctrl Pts',(-16.0586246728421,19.1460561854722,
15.5984542389911));
#210078=CARTESIAN_POINT('Ctrl Pts',(-17.3404775483521,16.9262798821378,
15.7256300456725));
#210079=CARTESIAN_POINT('Ctrl Pts',(-19.9008007814914,16.8025924812187,
15.852805852354));
#210080=CARTESIAN_POINT('Ctrl Pts',(-21.3906567174362,18.8884694961524,
15.9799816590354));
#210081=CARTESIAN_POINT('Ctrl Pts',(-20.4431950058454,21.2702482298655,
16.1071574657168));
#210082=CARTESIAN_POINT('Ctrl Pts',(-17.9276529609976,21.7627945240366,
16.2343332723983));
#210083=CARTESIAN_POINT('Ctrl Pts',(-16.1518842768929,19.9142277246345,
16.3615090790797));
#210084=CARTESIAN_POINT('Ctrl Pts',(-16.7450465045628,17.4204931351153,
16.4886848857611));
#210085=CARTESIAN_POINT('Ctrl Pts',(-19.1629501159199,16.5694374627385,
16.6158606924426));
#210086=CARTESIAN_POINT('Ctrl Pts',(-21.1873186195673,18.1418514644375,
16.743036499124));
#210087=CARTESIAN_POINT('Ctrl Pts',(-20.960919559888,20.6951428886731,16.8702123058054));
#210088=CARTESIAN_POINT('Ctrl Pts',(-18.6914600222275,21.8868253288476,
16.9973881124868));
#210089=CARTESIAN_POINT('Ctrl Pts',(-16.4610282738444,20.6236041102547,
17.1245639191683));
#210090=CARTESIAN_POINT('Ctrl Pts',(-16.3159070076732,18.0644062966023,
17.2517397258497));
#210091=CARTESIAN_POINT('Ctrl Pts',(-18.3892359781844,16.5571370401859,
17.3789155325312));
#210092=CARTESIAN_POINT('Ctrl Pts',(-20.7788645402429,17.4846223320876,
17.5060913392126));
#210093=CARTESIAN_POINT('Ctrl Pts',(-21.2924568052356,19.9959519832151,
17.633267145894));
#210094=CARTESIAN_POINT('Ctrl Pts',(-19.4588237471628,21.78713690936,17.7604429525755));
#210095=CARTESIAN_POINT('Ctrl Pts',(-16.9602098887033,21.2148761142513,
17.8876187592569));
#210096=CARTESIAN_POINT('Ctrl Pts',(-16.0889383635284,18.8041833589049,
18.0147945659384));
#210097=CARTESIAN_POINT('Ctrl Pts',(-17.6443467187751,16.7667196218568,
18.1419703726198));
#210098=CARTESIAN_POINT('Ctrl Pts',(-20.199444328037,16.97173142264,18.2691461793012));
#210099=CARTESIAN_POINT('Ctrl Pts',(-21.410087722055,19.2311331584014,18.3963219859826));
#210100=CARTESIAN_POINT('Ctrl Pts',(-20.1655867278293,21.4720639710636,
18.5234977926641));
#210101=CARTESIAN_POINT('Ctrl Pts',(-17.6076937651026,21.638608927483,18.6506735993455));
#210102=CARTESIAN_POINT('Ctrl Pts',(-16.083116866466,19.5779733678196,18.777849406027));
#210103=CARTESIAN_POINT('Ctrl Pts',(-16.9905607104441,17.1806625191931,
18.9050252127084));
#210104=CARTESIAN_POINT('Ctrl Pts',(-19.4975018926199,16.6460602940324,
19.0322010193898));
#210105=CARTESIAN_POINT('Ctrl Pts',(-21.3039774764415,18.4646310475516,
19.1593768260712));
#210106=CARTESIAN_POINT('Ctrl Pts',(-20.7526582367037,20.9679489966759,
19.2865526327527));
#210107=CARTESIAN_POINT('Ctrl Pts',(-18.3493453563032,21.8593752771558,
19.4137284394341));
#210108=CARTESIAN_POINT('Ctrl Pts',(-16.2989292381897,20.3210816421169,
19.5409042461156));
#210109=CARTESIAN_POINT('Ctrl Pts',(-16.4825394044677,17.7643569525393,
19.668080052797));
#210110=CARTESIAN_POINT('Ctrl Pts',(-18.7317249296591,16.5348375614239,
19.7952558594784));
#210111=CARTESIAN_POINT('Ctrl Pts',(-20.9829976831335,17.760530930567,19.9224316661598));
#210112=CARTESIAN_POINT('Ctrl Pts',(-21.1709546654166,20.31693998334,20.0496074728413));
#210113=CARTESIAN_POINT('Ctrl Pts',(-19.1231569686169,21.8587170911293,
20.1767832795227));
#210114=CARTESIAN_POINT('Ctrl Pts',(-16.7183319609261,20.9713793612995,
20.3039590862042));
#210115=CARTESIAN_POINT('Ctrl Pts',(-16.1627571685425,18.4690004055044,
20.4311348928856));
#210116=CARTESIAN_POINT('Ctrl Pts',(-17.9661382852434,16.6473646938877,
20.558310699567));
#210117=CARTESIAN_POINT('Ctrl Pts',(-20.4739844799035,17.1776962596402,
20.6854865062485));
#210118=CARTESIAN_POINT('Ctrl Pts',(-21.3855036545633,19.573475146687,20.8126623129299));
#210119=CARTESIAN_POINT('Ctrl Pts',(-19.8644313620253,21.6366721694472,
20.9398381196113));
#210120=CARTESIAN_POINT('Ctrl Pts',(-17.3062612225653,21.4745299209001,
21.0670139262928));
#210121=CARTESIAN_POINT('Ctrl Pts',(-16.0579474672366,19.2356153818981,
21.1941897329742));
#210122=CARTESIAN_POINT('Ctrl Pts',(-17.2647560855632,16.9743568582036,
21.3213655396557));
#210123=CARTESIAN_POINT('Ctrl Pts',(-19.8194850045369,16.7646188200965,
21.448541346337));
#210124=CARTESIAN_POINT('Ctrl Pts',(-21.3783870556072,18.8001718981978,
21.5757171530185));
#210125=CARTESIAN_POINT('Ctrl Pts',(-20.5111534744378,21.210919657188,21.7028929596999));
#210126=CARTESIAN_POINT('Ctrl Pts',(-18.013644503055,21.7901978133332,21.8300687663814));
#210127=CARTESIAN_POINT('Ctrl Pts',(-16.1763704623236,19.996267194463,21.9572632304172));
#210128=CARTESIAN_POINT('Ctrl Pts',(-16.5172189858702,18.3298181259339,
22.0420657588926));
#210129=CARTESIAN_POINT('Ctrl Pts',(-17.0028273589161,17.7531907778071,
22.0844763518074));
#210130=CARTESIAN_POINT('Ctrl Pts',(-19.2802416061914,17.1696268270448,
-0.257964187031692));
#210131=CARTESIAN_POINT('Ctrl Pts',(-19.9599075838988,17.3514955026281,
-0.215572251471214));
#210132=CARTESIAN_POINT('Ctrl Pts',(-21.1114421336233,18.4445263035272,
-0.130788380350257));
#210133=CARTESIAN_POINT('Ctrl Pts',(-20.664716890137,20.7997959707902,-0.00361257366882362));
#210134=CARTESIAN_POINT('Ctrl Pts',(-18.4433885124361,21.6921206442111,
0.123563233012611));
#210135=CARTESIAN_POINT('Ctrl Pts',(-16.4903436032298,20.310803390867,0.250739039694045));
#210136=CARTESIAN_POINT('Ctrl Pts',(-16.5948543226392,17.9191325598114,
0.37791484637548));
#210137=CARTESIAN_POINT('Ctrl Pts',(-18.6623441835338,16.7133702016597,
0.505090653056915));
#210138=CARTESIAN_POINT('Ctrl Pts',(-20.7953425359789,17.7986649093718,
0.632266459738347));
#210139=CARTESIAN_POINT('Ctrl Pts',(-21.0373070659623,20.1798778964501,
0.759442266419783));
#210140=CARTESIAN_POINT('Ctrl Pts',(-19.1660680424989,21.6721077326961,
0.886618073101216));
#210141=CARTESIAN_POINT('Ctrl Pts',(-16.8984657270469,20.9064747389806,
1.01379387978265));
#210142=CARTESIAN_POINT('Ctrl Pts',(-16.3148354086541,18.5853225629306,
1.14096968646408));
#210143=CARTESIAN_POINT('Ctrl Pts',(-17.9506471564477,16.8382042717466,
1.26814549314552));
#210144=CARTESIAN_POINT('Ctrl Pts',(-20.305132000971,17.2679716947772,1.39532129982695));
#210145=CARTESIAN_POINT('Ctrl Pts',(-21.2182030940675,19.4803506713964,
1.52249710650838));
#210146=CARTESIAN_POINT('Ctrl Pts',(-19.8521708189713,21.445615214303,1.64967291318982));
#210147=CARTESIAN_POINT('Ctrl Pts',(-17.4602868502336,21.3607599853939,
1.77684871987125));
#210148=CARTESIAN_POINT('Ctrl Pts',(-16.236955313264,19.3036328845313,1.90402452655269));
#210149=CARTESIAN_POINT('Ctrl Pts',(-17.3045074623036,17.1615211285584,
2.03120033323412));
#210150=CARTESIAN_POINT('Ctrl Pts',(-19.6835302021449,16.8996788935686,
2.15837613991555));
#210151=CARTESIAN_POINT('Ctrl Pts',(-21.1914179617914,18.758330388868,2.28555194659699));
#210152=CARTESIAN_POINT('Ctrl Pts',(-20.444777242296,21.0322781192214,2.41272775327842));
#210153=CARTESIAN_POINT('Ctrl Pts',(-18.1286045981342,21.6353162358223,
2.53990355995986));
#210154=CARTESIAN_POINT('Ctrl Pts',(-16.3678446537097,20.0141946660428,
2.66707936664131));
#210155=CARTESIAN_POINT('Ctrl Pts',(-16.7778853826632,17.6561918472671,
2.79425517332272));
#210156=CARTESIAN_POINT('Ctrl Pts',(-18.9825398611346,16.7246290036402,
2.92143098000418));
#210157=CARTESIAN_POINT('Ctrl Pts',(-20.9591744440326,18.0741572289896,
3.04860678668559));
#210158=CARTESIAN_POINT('Ctrl Pts',(-20.8943495839686,20.4666681355921,
3.17578259336703));
#210159=CARTESIAN_POINT('Ctrl Pts',(-18.8475380672715,21.7071814637211,
3.30295840004846));
#210160=CARTESIAN_POINT('Ctrl Pts',(-16.696562420695,20.6576032291843,3.4301342067299));
#210161=CARTESIAN_POINT('Ctrl Pts',(-16.4148092955578,18.2808563182951,
3.55731001341133));
#210162=CARTESIAN_POINT('Ctrl Pts',(-18.2607696965035,16.7574585040896,
3.68448582009278));
#210163=CARTESIAN_POINT('Ctrl Pts',(-20.5408895289395,17.4850327284497,
3.8116616267742));
#210164=CARTESIAN_POINT('Ctrl Pts',(-21.1633003667766,19.7960747988325,
3.93883743345564));
#210165=CARTESIAN_POINT('Ctrl Pts',(-19.5569788974863,21.5703470551314,
4.06601324013707));
#210166=CARTESIAN_POINT('Ctrl Pts',(-17.1956253695811,21.1800648259367,
4.19318904681852));
#210167=CARTESIAN_POINT('Ctrl Pts',(-16.2456350827884,18.9832878328934,
4.32036485349995));
#210168=CARTESIAN_POINT('Ctrl Pts',(-17.5785651621917,16.9954226197583,
4.44754066018137));
#210169=CARTESIAN_POINT('Ctrl Pts',(-19.9715349909106,17.0402121387546,
4.57471646686281));
#210170=CARTESIAN_POINT('Ctrl Pts',(-21.2291432755529,19.0765647861535,
4.70189227354424));
#210171=CARTESIAN_POINT('Ctrl Pts',(-20.1976124709327,21.2362533982663,
4.82906808022569));
#210172=CARTESIAN_POINT('Ctrl Pts',(-17.8233080662669,21.5378977188721,
4.95624388690712));
#210173=CARTESIAN_POINT('Ctrl Pts',(-16.2845069868849,19.7047578059733,
5.08341969358855));
#210174=CARTESIAN_POINT('Ctrl Pts',(-16.9929637143536,17.4186257521595,
5.21059550026999));
#210175=CARTESIAN_POINT('Ctrl Pts',(-19.298713173004,16.7768858234474,5.33777130695141));
#210176=CARTESIAN_POINT('Ctrl Pts',(-21.0863733454756,18.368294573558,5.46494711363286));
#210177=CARTESIAN_POINT('Ctrl Pts',(-20.7158769782294,20.7328332482315,
5.59212292031427));
#210178=CARTESIAN_POINT('Ctrl Pts',(-18.5271314926159,21.7011843732767,
5.71929872699574));
#210179=CARTESIAN_POINT('Ctrl Pts',(-16.5281750228197,20.3849458941136,
5.84647453367714));
#210180=CARTESIAN_POINT('Ctrl Pts',(-16.5529260606478,17.9916849204009,
5.9736503403586));
#210181=CARTESIAN_POINT('Ctrl Pts',(-18.5786770651157,16.7170698529915,
6.10082614704002));
#210182=CARTESIAN_POINT('Ctrl Pts',(-20.7469272219113,17.7304809047003,
6.22800195372147));
#210183=CARTESIAN_POINT('Ctrl Pts',(-21.0684415889569,20.1021763349681,
6.35517776040288));
#210184=CARTESIAN_POINT('Ctrl Pts',(-19.2482506899202,21.6562727905442,
6.48235356708434));
#210185=CARTESIAN_POINT('Ctrl Pts',(-16.9562667008792,20.9669832315418,
6.60952937376576));
#210186=CARTESIAN_POINT('Ctrl Pts',(-16.2952426752091,18.6666880462109,
6.7367051804472));
#210187=CARTESIAN_POINT('Ctrl Pts',(-17.8716271286841,16.8657652946716,
6.86388098712864));
#210188=CARTESIAN_POINT('Ctrl Pts',(-20.2391851666945,17.2164498235889,
6.99105679381006));
#210189=CARTESIAN_POINT('Ctrl Pts',(-21.2258292365902,19.397010343618,7.11823260049151));
#210190=CARTESIAN_POINT('Ctrl Pts',(-19.9263746422792,21.4069179184816,
7.24540840717293));
#210191=CARTESIAN_POINT('Ctrl Pts',(-17.5329903207938,21.4022070971754,
7.37258421385437));
#210192=CARTESIAN_POINT('Ctrl Pts',(-16.2414578369124,19.3871997658614,
7.49976002053581));
#210193=CARTESIAN_POINT('Ctrl Pts',(-17.2366780830498,17.2105400855604,
7.62693582721722));
#210194=CARTESIAN_POINT('Ctrl Pts',(-19.6055982537098,16.8691782142126,
7.75411163389868));
#210195=CARTESIAN_POINT('Ctrl Pts',(-21.1748811240797,18.6762924814722,
7.88128744058011));
#210196=CARTESIAN_POINT('Ctrl Pts',(-20.5048070612748,20.9739677092896,
8.00846324726155));
#210197=CARTESIAN_POINT('Ctrl Pts',(-18.2101274284319,21.6542294859505,
8.13563905394297));
#210198=CARTESIAN_POINT('Ctrl Pts',(-16.3960683648039,20.0929798531758,
8.26281486062441));
#210199=CARTESIAN_POINT('Ctrl Pts',(-16.7269164680658,17.7225684469559,
8.38999066730585));
#210200=CARTESIAN_POINT('Ctrl Pts',(-18.899139138224,16.717700608173,8.51716647398728));
#210201=CARTESIAN_POINT('Ctrl Pts',(-20.9198568987526,18.0002802097783,
8.64434228066872));
#210202=CARTESIAN_POINT('Ctrl Pts',(-20.9351866242553,20.3936200731671,
8.77151808735015));
#210203=CARTESIAN_POINT('Ctrl Pts',(-18.9310642430538,21.7019794211049,
8.89869389403158));
#210204=CARTESIAN_POINT('Ctrl Pts',(-16.7461476500366,20.7250197577984,
9.02586970071301));
#210205=CARTESIAN_POINT('Ctrl Pts',(-16.3849622080794,18.3590409373758,
9.15304550739446));
#210206=CARTESIAN_POINT('Ctrl Pts',(-18.1788731424809,16.774681678368,9.28022131407588));
#210207=CARTESIAN_POINT('Ctrl Pts',(-20.4820785135977,17.4254932644886,
9.40739712075733));
#210208=CARTESIAN_POINT('Ctrl Pts',(-21.1815303464774,19.7143964593946,
9.53457292743875));
#210209=CARTESIAN_POINT('Ctrl Pts',(-19.6355249973296,21.5414646471141,
9.66174873412019));
#210210=CARTESIAN_POINT('Ctrl Pts',(-17.2624264180838,21.2304761660553,
9.78892454080163));
#210211=CARTESIAN_POINT('Ctrl Pts',(-16.2394052640888,19.0667436454676,
9.91610034748306));
#210212=CARTESIAN_POINT('Ctrl Pts',(-17.5050199482811,17.0353573766044,
10.0432761541645));
#210213=CARTESIAN_POINT('Ctrl Pts',(-19.8981475508207,16.9999881790961,
10.1704519608459));
#210214=CARTESIAN_POINT('Ctrl Pts',(-21.2232420306283,18.9930850963969,
10.2976277675273));
#210215=CARTESIAN_POINT('Ctrl Pts',(-20.264611447119,21.1861054124292,10.4248035742088));
#210216=CARTESIAN_POINT('Ctrl Pts',(-17.9017398613385,21.5670891014251,
10.5519793808902));
#210217=CARTESIAN_POINT('Ctrl Pts',(-16.30241529689,19.7865072752454,10.6791551875716));
#210218=CARTESIAN_POINT('Ctrl Pts',(-16.9339187763774,17.477933244038,10.8063309942531));
#210219=CARTESIAN_POINT('Ctrl Pts',(-19.2168850528976,16.7593403951717,
10.9335068009345));
#210220=CARTESIAN_POINT('Ctrl Pts',(-21.0568342646105,18.289993066579,11.0606826076159));
#210221=CARTESIAN_POINT('Ctrl Pts',(-20.7657272098974,20.6656124352628,
11.1878584142974));
#210222=CARTESIAN_POINT('Ctrl Pts',(-18.6106365433157,21.7067151780229,
11.3150342209788));
#210223=CARTESIAN_POINT('Ctrl Pts',(-16.5687241914422,20.4581541465005,
11.4422100276602));
#210224=CARTESIAN_POINT('Ctrl Pts',(-16.5133180017472,18.0654065926801,
11.5693858343417));
#210225=CARTESIAN_POINT('Ctrl Pts',(-18.4952497143798,16.7236698865299,
11.6965616410231));
#210226=CARTESIAN_POINT('Ctrl Pts',(-20.696219995555,17.6639041783707,11.8237374477046));
#210227=CARTESIAN_POINT('Ctrl Pts',(-21.0969752199166,20.0235028629602,
11.950913254386));
#210228=CARTESIAN_POINT('Ctrl Pts',(-19.3298473427874,21.6376806003988,
12.0780890610674));
#210229=CARTESIAN_POINT('Ctrl Pts',(-17.0160665111076,21.0255295037559,
12.2052648677489));
#210230=CARTESIAN_POINT('Ctrl Pts',(-16.278383028509,18.7486602098194,12.3324406744303));
#210231=CARTESIAN_POINT('Ctrl Pts',(-17.7935757044751,16.8959589773299,
12.4596164811117));
#210232=CARTESIAN_POINT('Ctrl Pts',(-20.1715493022707,17.1671641954894,
12.5867922877931));
#210233=CARTESIAN_POINT('Ctrl Pts',(-21.2306606396052,19.3134619095308,
12.7139680944746));
#210234=CARTESIAN_POINT('Ctrl Pts',(-19.9992408003375,21.365757181081,12.841143901156));
#210235=CARTESIAN_POINT('Ctrl Pts',(-17.6070410564606,21.4411964783031,
12.9683197078375));
#210236=CARTESIAN_POINT('Ctrl Pts',(-16.2487561963206,19.4705689282866,
13.0954955145189));
#210237=CARTESIAN_POINT('Ctrl Pts',(-17.1705282744295,17.2618029972318,
13.2226713212003));
#210238=CARTESIAN_POINT('Ctrl Pts',(-19.52668862075,16.8413043354067,13.3498471278818));
#210239=CARTESIAN_POINT('Ctrl Pts',(-21.1556063573368,18.5948543659455,
13.4770229345632));
#210240=CARTESIAN_POINT('Ctrl Pts',(-20.5628505629085,20.9136797734184,
13.6041987412446));
#210241=CARTESIAN_POINT('Ctrl Pts',(-18.2922378882792,21.670402169005,13.7313745479261));
#210242=CARTESIAN_POINT('Ctrl Pts',(-16.4269145323048,20.1707757222437,
13.8585503546075));
#210243=CARTESIAN_POINT('Ctrl Pts',(-16.6781988990673,17.7906146207234,
13.9857261612889));
#210244=CARTESIAN_POINT('Ctrl Pts',(-18.8155531785289,16.7135689456302,
14.1129019679704));
#210245=CARTESIAN_POINT('Ctrl Pts',(-20.8780874784513,17.9277612548684,
14.2400777746518));
#210246=CARTESIAN_POINT('Ctrl Pts',(-20.9735545939718,20.3192454659859,
14.3672535813332));
#210247=CARTESIAN_POINT('Ctrl Pts',(-19.0143693719578,21.6939832475324,
14.4944293880147));
#210248=CARTESIAN_POINT('Ctrl Pts',(-16.7979626528582,20.7907380107889,
14.6216051946961));
#210249=CARTESIAN_POINT('Ctrl Pts',(-16.3577500357315,18.4381811987453,
14.7487810013775));
#210250=CARTESIAN_POINT('Ctrl Pts',(-18.0975992741149,16.7946376703086,
14.875956808059));
#210251=CARTESIAN_POINT('Ctrl Pts',(-20.4213066790141,17.3679566030033,
15.0031326147404));
#210252=CARTESIAN_POINT('Ctrl Pts',(-21.1970149319813,19.6321534602683,
15.1303084214219));
#210253=CARTESIAN_POINT('Ctrl Pts',(-19.713059856803,21.5099681574688,15.2574842281033));
#210254=CARTESIAN_POINT('Ctrl Pts',(-17.3308781303159,21.2786222602481,
15.3846600347847));
#210255=CARTESIAN_POINT('Ctrl Pts',(-16.2359736316991,19.1503612703603,
15.5118358414661));
#210256=CARTESIAN_POINT('Ctrl Pts',(-17.432853280996,17.0777325512529,15.6390116481476));
#210257=CARTESIAN_POINT('Ctrl Pts',(-19.8234542867059,16.9622443108606,
15.766187454829));
#210258=CARTESIAN_POINT('Ctrl Pts',(-21.2145486035221,18.9098498417347,
15.8933632615105));
#210259=CARTESIAN_POINT('Ctrl Pts',(-20.3298935368166,21.1337419513304,
16.0205390681919));
#210260=CARTESIAN_POINT('Ctrl Pts',(-17.9811052024058,21.5936376594049,
16.1477148748733));
#210261=CARTESIAN_POINT('Ctrl Pts',(-16.3230511148663,19.8676111981466,
16.2748906815548));
#210262=CARTESIAN_POINT('Ctrl Pts',(-16.8768929890729,17.5391847164761,
16.4020664882362));
#210263=CARTESIAN_POINT('Ctrl Pts',(-19.1345152807445,16.7445449928796,
16.5292422949176));
#210264=CARTESIAN_POINT('Ctrl Pts',(-21.0246896611148,18.2127246528537,
16.656418101599));
#210265=CARTESIAN_POINT('Ctrl Pts',(-20.8132984536472,20.5967599838785,
16.7835939082805));
#210266=CARTESIAN_POINT('Ctrl Pts',(-18.6942799707749,21.7094465396596,
16.9107697149619));
#210267=CARTESIAN_POINT('Ctrl Pts',(-16.6117021494137,20.5299634663839,
17.0379455216434));
#210268=CARTESIAN_POINT('Ctrl Pts',(-16.4762008813049,18.1404132768064,
17.1651213283248));
#210269=CARTESIAN_POINT('Ctrl Pts',(-18.4120901697813,16.7330599576527,
17.2922971350062));
#210270=CARTESIAN_POINT('Ctrl Pts',(-20.6433117475059,17.5990628290491,
17.4194729416877));
#210271=CARTESIAN_POINT('Ctrl Pts',(-21.1228583021457,19.9439180066875,
17.5466487483691));
#210272=CARTESIAN_POINT('Ctrl Pts',(-19.4107756338348,21.6163664032144,
17.6738245550505));
#210273=CARTESIAN_POINT('Ctrl Pts',(-17.0777933269134,21.0820404186637,
17.801000361732));
#210274=CARTESIAN_POINT('Ctrl Pts',(-16.2642778467699,18.8311509798632,
17.9281761684134));
#210275=CARTESIAN_POINT('Ctrl Pts',(-17.7165791539697,16.9287494409323,
18.0553519750948));
#210276=CARTESIAN_POINT('Ctrl Pts',(-20.1023009391443,17.1201711375333,
18.1825277817763));
#210277=CARTESIAN_POINT('Ctrl Pts',(-21.2326915389853,19.2297985439103,
18.3097035884577));
#210278=CARTESIAN_POINT('Ctrl Pts',(-20.0706877380999,21.3221794531393,
18.4368793951392));
#210279=CARTESIAN_POINT('Ctrl Pts',(-17.6823559016955,21.4776842484555,
18.5640552018205));
#210280=CARTESIAN_POINT('Ctrl Pts',(-16.2588422531106,19.5536469325526,
18.691231008502));
#210281=CARTESIAN_POINT('Ctrl Pts',(-17.1061322116441,17.3152523222366,
18.8184068151834));
#210282=CARTESIAN_POINT('Ctrl Pts',(-19.4468898291958,16.8160885445611,
18.9455826218649));
#210283=CARTESIAN_POINT('Ctrl Pts',(-21.1336152752557,18.5141073790766,
19.0727584285463));
#210284=CARTESIAN_POINT('Ctrl Pts',(-20.6188426434545,20.8514819454316,
19.1999342352277));
#210285=CARTESIAN_POINT('Ctrl Pts',(-18.3748438723008,21.6838161347437,
19.3271100419092));
#210286=CARTESIAN_POINT('Ctrl Pts',(-16.4603485575527,20.2474950236424,
19.4542858485906));
#210287=CARTESIAN_POINT('Ctrl Pts',(-16.6317873206282,17.8602540162898,
19.5814616552721));
#210288=CARTESIAN_POINT('Ctrl Pts',(-18.7318757426506,16.712238697405,19.7086374619535));
#210289=CARTESIAN_POINT('Ctrl Pts',(-20.833913031897,17.8566816189236,19.8358132686349));
#210290=CARTESIAN_POINT('Ctrl Pts',(-21.0094104632606,20.243627912838,19.9629890753163));
#210291=CARTESIAN_POINT('Ctrl Pts',(-19.0973599963134,21.6832015794576,
20.0901648819978));
#210292=CARTESIAN_POINT('Ctrl Pts',(-16.8519493358426,20.8546849133278,
20.2173406886792));
#210293=CARTESIAN_POINT('Ctrl Pts',(-16.3332032493219,18.5181870950206,
20.3445164953606));
#210294=CARTESIAN_POINT('Ctrl Pts',(-18.0170393585529,16.817306476565,20.4716923020421));
#210295=CARTESIAN_POINT('Ctrl Pts',(-20.3586419958767,17.3124826941761,
20.5988681087235));
#210296=CARTESIAN_POINT('Ctrl Pts',(-21.2097371339674,19.5494468956883,
20.726043915405));
#210297=CARTESIAN_POINT('Ctrl Pts',(-19.7894957733326,21.4758758768998,
20.8532197220864));
#210298=CARTESIAN_POINT('Ctrl Pts',(-17.4009051340672,21.3244819367018,
20.9803955287679));
#210299=CARTESIAN_POINT('Ctrl Pts',(-16.2353413176302,19.2339836436119,
21.1075713354492));
#210300=CARTESIAN_POINT('Ctrl Pts',(-17.3621513466646,17.1226225346138,
21.2347471421307));
#210301=CARTESIAN_POINT('Ctrl Pts',(-19.7475288817995,16.9267879000082,
21.3619229488121));
#210302=CARTESIAN_POINT('Ctrl Pts',(-21.2030922899096,18.82740543638,21.4890987554935));
#210303=CARTESIAN_POINT('Ctrl Pts',(-20.3933470809866,21.078346232667,21.616274562175));
#210304=CARTESIAN_POINT('Ctrl Pts',(-18.0613964188678,21.6192244017756,
21.7434503688564));
#210305=CARTESIAN_POINT('Ctrl Pts',(-16.3459141263638,19.9442123227787,
21.8706448328923));
#210306=CARTESIAN_POINT('Ctrl Pts',(-16.6641680142473,18.3882311218014,
21.9554473613676));
#210307=CARTESIAN_POINT('Ctrl Pts',(-17.1175857116532,17.849828040304,21.9978579542825));
#210308=CARTESIAN_POINT('Ctrl Pts',(-19.3957372685685,16.7380050975816,
-1.23165366794353E-15));
#210309=CARTESIAN_POINT('Ctrl Pts',(-19.4773890628972,16.7675693190178,
4.67785589882032E-15));
#210310=CARTESIAN_POINT('Ctrl Pts',(-19.5571491449816,16.8015339789003,
1.41562167189676E-14));
#210311=CARTESIAN_POINT('Ctrl Pts',(-19.6348154881074,16.8395812463466,
1.43895312332276E-14));
#210312=CARTESIAN_POINT('Ctrl Pts',(-19.7143271339378,16.8785324925655,
1.46283891513207E-14));
#210313=CARTESIAN_POINT('Ctrl Pts',(-19.7916450873999,16.9217633018164,
1.59364397924074E-15));
#210314=CARTESIAN_POINT('Ctrl Pts',(-19.8665231354208,16.9689790854395,
1.51961776495568E-15));
#210315=CARTESIAN_POINT('Ctrl Pts',(-19.93658856029,17.0131601775957,1.45034942406773E-15));
#210316=CARTESIAN_POINT('Ctrl Pts',(-20.0045177778054,17.0608314259457,
4.40057979472968E-15));
#210317=CARTESIAN_POINT('Ctrl Pts',(-20.0700782293505,17.1117789745462,
6.48786580015326E-15));
#210318=CARTESIAN_POINT('Ctrl Pts',(-20.0997466327889,17.1348345269478,
7.70028889287582E-15));
#210319=CARTESIAN_POINT('Ctrl Pts',(-20.1289294943527,17.1585613303937,
2.175758139592E-14));
#210320=CARTESIAN_POINT('Ctrl Pts',(-20.1576028725502,17.1829408480985,
1.05748743095546E-14));
#210321=CARTESIAN_POINT('Ctrl Pts',(-20.1753080913464,17.197994696729,3.78565993772445E-15));
#210322=CARTESIAN_POINT('Ctrl Pts',(-20.192819023282,17.213297426603,-2.39744414414718E-14));
#210323=CARTESIAN_POINT('Ctrl Pts',(-20.2101297182957,17.228844786453,-1.88668525247238E-14));
#210324=CARTESIAN_POINT('Ctrl Pts',(-20.2222917522923,17.2397679480536,
-1.53146598863056E-14));
#210325=CARTESIAN_POINT('Ctrl Pts',(-20.2343567224894,17.2508136607941,
-1.04410141243044E-14));
#210326=CARTESIAN_POINT('Ctrl Pts',(-20.2463056670645,17.2619643610397,
-1.12895803816571E-14));
#210327=CARTESIAN_POINT('Ctrl Pts',(-20.3097374450941,17.3211586052181,
-1.46324699270345E-14));
#210328=CARTESIAN_POINT('Ctrl Pts',(-20.3700068842138,17.3834001964164,
-1.31327203746279E-14));
#210329=CARTESIAN_POINT('Ctrl Pts',(-20.4268834249918,17.4484109388489,
-3.60822483003176E-16));
#210330=CARTESIAN_POINT('Ctrl Pts',(-20.4830375676461,17.5125959693496,
1.22488574722256E-14));
#210331=CARTESIAN_POINT('Ctrl Pts',(-20.5358849034917,17.5794810921972,
-4.53135006405206E-15));
#210332=CARTESIAN_POINT('Ctrl Pts',(-20.5851610289898,17.6488247163834,
-5.20417042793042E-15));
#210333=CARTESIAN_POINT('Ctrl Pts',(-20.630598257404,17.712766068496,-5.82457416800118E-15));
#210334=CARTESIAN_POINT('Ctrl Pts',(-20.6729989034477,17.7787984983208,
-1.74365969497394E-14));
#210335=CARTESIAN_POINT('Ctrl Pts',(-20.7121179763249,17.8467438133767,
5.55111512312578E-16));
#210336=CARTESIAN_POINT('Ctrl Pts',(-20.7284900279032,17.8751801775537,
7.98301933950798E-15));
#210337=CARTESIAN_POINT('Ctrl Pts',(-20.7442868194365,17.9039516828061,
-1.01106350429347E-15));
#210338=CARTESIAN_POINT('Ctrl Pts',(-20.7594882783128,17.9330455001009,
-1.22402088464924E-14));
#210339=CARTESIAN_POINT('Ctrl Pts',(-20.7693449710067,17.9519100590029,
-1.96477426282344E-14));
#210340=CARTESIAN_POINT('Ctrl Pts',(-20.7789513429732,17.970910128766,-2.31450257561518E-14));
#210341=CARTESIAN_POINT('Ctrl Pts',(-20.7883016221878,17.9900422154472,
-2.25652829755063E-14));
#210342=CARTESIAN_POINT('Ctrl Pts',(-20.7942275728048,18.0021676074567,
-2.21856505814976E-14));
#210343=CARTESIAN_POINT('Ctrl Pts',(-20.8000468301417,18.0143382523374,
8.10549747755472E-16));
#210344=CARTESIAN_POINT('Ctrl Pts',(-20.8057567255896,18.0265495880407,
7.07767178198537E-16));
#210345=CARTESIAN_POINT('Ctrl Pts',(-20.8408822594586,18.1016699978184,
4.51885638151754E-16));
#210346=CARTESIAN_POINT('Ctrl Pts',(-20.8718943559605,18.1783721483409,
2.2231995317661E-14));
#210347=CARTESIAN_POINT('Ctrl Pts',(-20.8985462175416,18.2564274689474,
7.60502771868232E-15));
#210348=CARTESIAN_POINT('Ctrl Pts',(-20.9251980791227,18.3344827895539,
-7.47990687795419E-15));
#210349=CARTESIAN_POINT('Ctrl Pts',(-20.9474901778909,18.4138920100306,
-4.35017343927013E-16));
#210350=CARTESIAN_POINT('Ctrl Pts',(-20.9651214076632,18.4944358221201,
7.68829444552921E-15));
#210351=CARTESIAN_POINT('Ctrl Pts',(-20.9829513884047,18.5758875777238,
1.55637816228134E-14));
#210352=CARTESIAN_POINT('Ctrl Pts',(-20.9960140913518,18.658500875996,-1.23111829755394E-14));
#210353=CARTESIAN_POINT('Ctrl Pts',(-21.0043852377911,18.7418839028421,
-4.82947015711943E-15));
#210354=CARTESIAN_POINT('Ctrl Pts',(-21.0073021823584,18.7709389037228,
-2.22245071022286E-15));
#210355=CARTESIAN_POINT('Ctrl Pts',(-21.0096490356195,18.8000872405028,
-2.55476121086874E-15));
#210356=CARTESIAN_POINT('Ctrl Pts',(-21.0114276099518,18.8293118127823,
-6.0507154842071E-15));
#210357=CARTESIAN_POINT('Ctrl Pts',(-21.0124180861882,18.8455867830405,
-7.99758920671491E-15));
#210358=CARTESIAN_POINT('Ctrl Pts',(-21.0132324466491,18.8618898462714,
-1.03347261259021E-14));
#210359=CARTESIAN_POINT('Ctrl Pts',(-21.013870300486,18.8781994765334,-6.80011602582908E-15));
#210360=CARTESIAN_POINT('Ctrl Pts',(-21.0156561553971,18.9238629680941,
3.09603955107904E-15));
#210361=CARTESIAN_POINT('Ctrl Pts',(-21.0160589030046,18.9695495767969,
5.33176806238529E-15));
#210362=CARTESIAN_POINT('Ctrl Pts',(-21.0151046780771,19.0152032718637,
6.38378239159465E-16));
#210363=CARTESIAN_POINT('Ctrl Pts',(-21.0142961185617,19.0538877879554,
-3.3385509858536E-15));
#210364=CARTESIAN_POINT('Ctrl Pts',(-21.0125130883268,19.0925470962694,
-8.9035032026131E-15));
#210365=CARTESIAN_POINT('Ctrl Pts',(-21.0097683504117,19.1311426359222,
-5.19029264012261E-15));
#210366=CARTESIAN_POINT('Ctrl Pts',(-21.0039587339496,19.2128354202505,
2.59522987051867E-15));
#210367=CARTESIAN_POINT('Ctrl Pts',(-20.9938436162584,19.2942438410436,
1.41268828373383E-14));
#210368=CARTESIAN_POINT('Ctrl Pts',(-20.9795069236666,19.3749917573276,
-1.80411241501588E-15));
#210369=CARTESIAN_POINT('Ctrl Pts',(-20.9654095554307,19.4543917376819,
-1.746916940066E-14));
#210370=CARTESIAN_POINT('Ctrl Pts',(-20.9472298872572,19.5331539565604,
6.03445153792289E-16));
#210371=CARTESIAN_POINT('Ctrl Pts',(-20.9250049246707,19.6108953906273,
1.41553435639707E-15));
#210372=CARTESIAN_POINT('Ctrl Pts',(-20.9157258007255,19.6433531461612,
1.75458898185226E-15));
#210373=CARTESIAN_POINT('Ctrl Pts',(-20.9057410484994,19.6756325821161,
2.59523708429575E-15));
#210374=CARTESIAN_POINT('Ctrl Pts',(-20.8950514018658,19.7077039335531,
-4.55191440096314E-15));
#210375=CARTESIAN_POINT('Ctrl Pts',(-20.8895107318069,19.72432719368,-8.07758464467123E-15));
#210376=CARTESIAN_POINT('Ctrl Pts',(-20.8837798046829,19.7408965824585,
8.50160659820308E-15));
#210377=CARTESIAN_POINT('Ctrl Pts',(-20.8778666060763,19.757386588617,5.02375918642883E-15));
#210378=CARTESIAN_POINT('Ctrl Pts',(-20.8511334429462,19.83193676932,-1.06923181167905E-14));
#210379=CARTESIAN_POINT('Ctrl Pts',(-20.8206474027028,19.9049627949995,
-1.73353012963057E-14));
#210380=CARTESIAN_POINT('Ctrl Pts',(-20.7864673380873,19.9761054066943,
-1.81799020282369E-14));
#210381=CARTESIAN_POINT('Ctrl Pts',(-20.7601551358713,20.0308717977514,
-1.8830085271024E-14));
#210382=CARTESIAN_POINT('Ctrl Pts',(-20.7316529099465,20.0845216847886,
-2.44471155034467E-16));
#210383=CARTESIAN_POINT('Ctrl Pts',(-20.7009723060731,20.1368764894501,
6.55031584528842E-15));
#210384=CARTESIAN_POINT('Ctrl Pts',(-20.6917380360057,20.1526342759514,
8.31297483703845E-15));
#210385=CARTESIAN_POINT('Ctrl Pts',(-20.6823063437492,20.1682746386422,
7.82297213918542E-15));
#210386=CARTESIAN_POINT('Ctrl Pts',(-20.6726773354748,20.1837924272005,
-6.38378239159465E-15));
#210387=CARTESIAN_POINT('Ctrl Pts',(-20.6644524181989,20.1970474295393,
-1.86960947630402E-14));
#210388=CARTESIAN_POINT('Ctrl Pts',(-20.6560858012134,20.2102092325172,
1.07604636562338E-14));
#210389=CARTESIAN_POINT('Ctrl Pts',(-20.64758209464,20.2232683236723,1.09634523681734E-14));
#210390=CARTESIAN_POINT('Ctrl Pts',(-20.6064305700017,20.286464473114,1.11814633947155E-14));
#210391=CARTESIAN_POINT('Ctrl Pts',(-20.5620419244788,20.3473056726972,
5.47217430806986E-15));
#210392=CARTESIAN_POINT('Ctrl Pts',(-20.5144495335262,20.4054521925719,
8.52096171399808E-15));
#210393=CARTESIAN_POINT('Ctrl Pts',(-20.4703173116583,20.4593712133354,
1.21050310956189E-14));
#210394=CARTESIAN_POINT('Ctrl Pts',(-20.4234297145935,20.5109732585207,
-9.13198254776251E-15));
#210395=CARTESIAN_POINT('Ctrl Pts',(-20.3737907847676,20.5599542646918,
-6.32827124036339E-15));
#210396=CARTESIAN_POINT('Ctrl Pts',(-20.3682022242118,20.5654687534213,
-6.1941711563184E-15));
#210397=CARTESIAN_POINT('Ctrl Pts',(-20.3625787693224,20.5709499818026,
-2.24943731332233E-15));
#210398=CARTESIAN_POINT('Ctrl Pts',(-20.3569207886222,20.5763978007994,
2.27595720048157E-15));
#210399=CARTESIAN_POINT('Ctrl Pts',(20.3504145334569,20.5721720813046,0.00214189615582165));
#210400=CARTESIAN_POINT('Ctrl Pts',(20.8038322552136,20.0337689331937,0.0445524877679971));
#210401=CARTESIAN_POINT('Ctrl Pts',(21.1220877011301,18.4777891502142,0.12935501494065));
#210402=CARTESIAN_POINT('Ctrl Pts',(19.4066027174179,16.8027744939582,0.256549477673783));
#210403=CARTESIAN_POINT('Ctrl Pts',(17.0746532806956,17.3436542441791,0.383725284355217));
#210404=CARTESIAN_POINT('Ctrl Pts',(16.2649072910693,19.5945942026566,0.510901091036652));
#210405=CARTESIAN_POINT('Ctrl Pts',(17.7204711796095,21.4952124979738,0.638076897718085));
#210406=CARTESIAN_POINT('Ctrl Pts',(20.1058486786829,21.2993774626889,0.765252704399521));
#210407=CARTESIAN_POINT('Ctrl Pts',(21.2326588902647,19.1880164416469,0.892428511080953));
#210408=CARTESIAN_POINT('Ctrl Pts',(20.06709493847,17.0975178673283,1.01960431776238));
#210409=CARTESIAN_POINT('Ctrl Pts',(17.6785041641668,16.9461239968056,1.14678012444382));
#210410=CARTESIAN_POINT('Ctrl Pts',(16.2582626906796,18.8725530643131,1.27395593112525));
#210411=CARTESIAN_POINT('Ctrl Pts',(17.1093578952725,21.1095174457449,1.40113173780669));
#210412=CARTESIAN_POINT('Ctrl Pts',(19.4509606892502,21.6046936825495,1.52830754448812));
#210413=CARTESIAN_POINT('Ctrl Pts',(21.1347969163821,19.9038129555627,1.65548335116956));
#210414=CARTESIAN_POINT('Ctrl Pts',(20.6160507930577,17.5673149720866,1.78265915785099));
#210415=CARTESIAN_POINT('Ctrl Pts',(18.3706399789337,16.7387982516159,1.90983496453243));
#210416=CARTESIAN_POINT('Ctrl Pts',(16.4585893803026,18.1783720157104,2.03701077121386));
#210417=CARTESIAN_POINT('Ctrl Pts',(16.6340868238919,20.5653184744001,2.16418657789529));
#210418=CARTESIAN_POINT('Ctrl Pts',(18.7361242574646,21.709761474113,2.29136238457673));
#210419=CARTESIAN_POINT('Ctrl Pts',(20.8362128238147,20.5617460765933,2.41853819125816));
#210420=CARTESIAN_POINT('Ctrl Pts',(21.0076515986441,18.1745049051026,2.54571399793959));
#210421=CARTESIAN_POINT('Ctrl Pts',(19.0931561523786,16.7381836953926,2.67288980462103));
#210422=CARTESIAN_POINT('Ctrl Pts',(16.84915722705,17.5705179418497,2.80006561130246));
#210423=CARTESIAN_POINT('Ctrl Pts',(16.3343845598861,19.9078926688087,2.9272414179839));
#210424=CARTESIAN_POINT('Ctrl Pts',(18.021110121826,21.605911619971,3.05441722466534));
#210425=CARTESIAN_POINT('Ctrl Pts',(20.3618679001945,21.1067478080081,3.18159303134677));
#210426=CARTESIAN_POINT('Ctrl Pts',(21.2091579169385,18.8683530439058,3.3087688380282));
#210427=CARTESIAN_POINT('Ctrl Pts',(19.7856441705552,16.9443155958186,3.43594464470964));
#210428=CARTESIAN_POINT('Ctrl Pts',(17.3973121700664,17.0998204018171,3.56312045139108));
#210429=CARTESIAN_POINT('Ctrl Pts',(16.2353082893486,19.1922014547983,3.69029625807252));
#210430=CARTESIAN_POINT('Ctrl Pts',(17.36569896685,21.3018290061115,3.81747206475393));
#210431=CARTESIAN_POINT('Ctrl Pts',(19.7514209159292,21.4932507158639,3.94464787143538));
#210432=CARTESIAN_POINT('Ctrl Pts',(21.2037223229058,19.5908490462335,4.0718236781168));
#210433=CARTESIAN_POINT('Ctrl Pts',(20.390206786872,17.3399594527915,4.19899948479825));
#210434=CARTESIAN_POINT('Ctrl Pts',(18.0572243196692,16.8056334315311,4.32617529147968));
#210435=CARTESIAN_POINT('Ctrl Pts',(16.345141533734,18.4780819429591,4.45335109816112));
#210436=CARTESIAN_POINT('Ctrl Pts',(16.8246881213196,20.8229372816948,4.58052690484254));
#210437=CARTESIAN_POINT('Ctrl Pts',(19.0559098523345,21.6889402125877,4.70770271152398));
#210438=CARTESIAN_POINT('Ctrl Pts',(20.9917992738112,20.2815867967456,4.83487851820543));
#210439=CARTESIAN_POINT('Ctrl Pts',(20.8562979963933,17.8920364430003,4.96205432488685));
#210440=CARTESIAN_POINT('Ctrl Pts',(18.7737200319539,16.7125532886911,5.0892301315683));
#210441=CARTESIAN_POINT('Ctrl Pts',(16.6547014035,17.8252399209163,5.21640593824972));
#210442=CARTESIAN_POINT('Ctrl Pts',(16.4433101815092,20.2092754157301,5.34358174493117));
#210443=CARTESIAN_POINT('Ctrl Pts',(18.3334846917389,21.6774551765717,5.47075755161258));
#210444=CARTESIAN_POINT('Ctrl Pts',(20.5911071385146,20.8828153983818,5.59793335829403));
#210445=CARTESIAN_POINT('Ctrl Pts',(21.1449490507717,18.5543887567427,5.72510916497546));
#210446=CARTESIAN_POINT('Ctrl Pts',(19.48689484932,16.8283621769022,5.8522849716569));
#210447=CARTESIAN_POINT('Ctrl Pts',(17.1381063535418,17.2882579165725,5.97946077833833));
#210448=CARTESIAN_POINT('Ctrl Pts',(16.2534512260582,19.5121501789549,6.10663658501977));
#210449=CARTESIAN_POINT('Ctrl Pts',(17.6445456384458,21.4597558436343,6.2338123917012));
#210450=CARTESIAN_POINT('Ctrl Pts',(20.0351468083957,21.3442675953079,6.36098819838264));
#210451=CARTESIAN_POINT('Ctrl Pts',(21.2320265399213,19.271638733806,6.48816400506407));
#210452=CARTESIAN_POINT('Ctrl Pts',(20.137121966082,17.1433775977014,6.6153398117455));
#210453=CARTESIAN_POINT('Ctrl Pts',(17.7549400759333,16.9120316845865,6.74251561842694));
#210454=CARTESIAN_POINT('Ctrl Pts',(16.2709848988036,18.7898465107973,6.86969142510837));
#210455=CARTESIAN_POINT('Ctrl Pts',(17.0466932050637,21.0540435236181,6.99686723178981));
#210456=CARTESIAN_POINT('Ctrl Pts',(19.3704007696072,21.6273624957014,7.12404303847125));
#210457=CARTESIAN_POINT('Ctrl Pts',(21.1102501275226,19.9838188543493,7.25121884515266));
#210458=CARTESIAN_POINT('Ctrl Pts',(20.6700374801522,17.6312618806795,7.37839465183412));
#210459=CARTESIAN_POINT('Ctrl Pts',(18.4536306087803,16.7280165818807,7.50557045851553));
#210460=CARTESIAN_POINT('Ctrl Pts',(16.4944452521654,18.1027544578749,7.63274626519699));
#210461=CARTESIAN_POINT('Ctrl Pts',(16.5899123742445,20.494238833293,7.7599220718784));
#210462=CARTESIAN_POINT('Ctrl Pts',(18.6524468158679,21.7084312259493,7.88709787855985));
#210463=CARTESIAN_POINT('Ctrl Pts',(20.7898012421711,20.6313854768606,8.01427368524127));
#210464=CARTESIAN_POINT('Ctrl Pts',(21.0410856261976,18.2512242118175,8.14144949192272));
#210465=CARTESIAN_POINT('Ctrl Pts',(19.175762142071,16.7515976620282,8.26862529860414));
#210466=CARTESIAN_POINT('Ctrl Pts',(16.9051493114451,17.5083201096033,8.39580110528559));
#210467=CARTESIAN_POINT('Ctrl Pts',(16.3123934762929,19.827145676385,8.52297691196702));
#210468=CARTESIAN_POINT('Ctrl Pts',(17.9413113247901,21.580695827397,8.65015271864845));
#210469=CARTESIAN_POINT('Ctrl Pts',(20.2974718329846,21.1601971366828,8.77732852532987));
#210470=CARTESIAN_POINT('Ctrl Pts',(21.2192439744216,18.9514310538806,8.90450433201132));
#210471=CARTESIAN_POINT('Ctrl Pts',(19.8609590209642,16.9808033684772,9.03168013869275));
#210472=CARTESIAN_POINT('Ctrl Pts',(17.4687591127375,17.0562426708819,9.1588559453742));
#210473=CARTESIAN_POINT('Ctrl Pts',(16.2373391888682,19.1085380834297,9.28603175205562));
#210474=CARTESIAN_POINT('Ctrl Pts',(17.296450598966,21.2548359449271,9.41320755873706));
#210475=CARTESIAN_POINT('Ctrl Pts',(19.6744243601341,21.526041181719,9.54038336541849));
#210476=CARTESIAN_POINT('Ctrl Pts',(21.1896171401977,19.6733398219446,9.66755917209993));
#210477=CARTESIAN_POINT('Ctrl Pts',(20.4519336069186,17.3964703715816,9.79473497878135));
#210478=CARTESIAN_POINT('Ctrl Pts',(18.1381526162766,16.7843192328824,9.9219107854628));
#210479=CARTESIAN_POINT('Ctrl Pts',(16.3710246177412,18.3984970812188,10.0490865921442));
#210480=CARTESIAN_POINT('Ctrl Pts',(16.7717798696356,20.7580959279184,10.1762623988257));
#210481=CARTESIAN_POINT('Ctrl Pts',(18.9727503020227,21.6983302843557,10.3034382055071));
#210482=CARTESIAN_POINT('Ctrl Pts',(20.9546821508189,20.356593486025,10.4306140121885));
#210483=CARTESIAN_POINT('Ctrl Pts',(20.8992759573175,17.9638457678171,10.5577898188699));
#210484=CARTESIAN_POINT('Ctrl Pts',(18.8573634651597,16.7152846505156,10.6849656255514));
#210485=CARTESIAN_POINT('Ctrl Pts',(16.7022726505182,17.7563874648017,10.8121414322328));
#210486=CARTESIAN_POINT('Ctrl Pts',(16.411165575805,20.1320069966963,10.9393172389142));
#210487=CARTESIAN_POINT('Ctrl Pts',(18.2511149139269,21.6626597732632,11.0664930455957));
#210488=CARTESIAN_POINT('Ctrl Pts',(20.5340813472922,20.9440668750279,11.1936688522771));
#210489=CARTESIAN_POINT('Ctrl Pts',(21.1655848701657,18.635492685216,11.3208446589586));
#210490=CARTESIAN_POINT('Ctrl Pts',(19.5662601958398,16.854910736706,11.44802046564));
#210491=CARTESIAN_POINT('Ctrl Pts',(17.2033884477244,17.2358944518762,11.5751962723214));
#210492=CARTESIAN_POINT('Ctrl Pts',(16.2447577983548,19.4289149185742,11.7023720790029));
#210493=CARTESIAN_POINT('Ctrl Pts',(17.5698523691992,21.4220119728056,11.8295478856843));
#210494=CARTESIAN_POINT('Ctrl Pts',(19.9629801361526,21.3866427728676,11.9567236923657));
#210495=CARTESIAN_POINT('Ctrl Pts',(21.2285949072958,19.3552563644432,12.0838994990471));
#210496=CARTESIAN_POINT('Ctrl Pts',(20.2055736830169,17.191523695202,12.2110753057286));
#210497=CARTESIAN_POINT('Ctrl Pts',(17.8324749407335,16.8805351927773,12.33825111241));
#210498=CARTESIAN_POINT('Ctrl Pts',(16.2864694853713,18.7076035060207,12.4654269190915));
#210499=CARTESIAN_POINT('Ctrl Pts',(16.985921366305,20.9965068581799,12.5926027257729));
#210500=CARTESIAN_POINT('Ctrl Pts',(19.2891268956574,21.647318489013,12.7197785324543));
#210501=CARTESIAN_POINT('Ctrl Pts',(21.0830379533052,20.0629591211559,12.8469543391357));
#210502=CARTESIAN_POINT('Ctrl Pts',(20.7218524865336,17.6969801381849,12.9741301458172));
#210503=CARTESIAN_POINT('Ctrl Pts',(18.5369357434076,16.7200204077588,13.1013059524986));
#210504=CARTESIAN_POINT('Ctrl Pts',(16.5328132245178,18.0283798455839,13.2284817591801));
#210505=CARTESIAN_POINT('Ctrl Pts',(16.5481429510737,20.4217198734009,13.3556575658615));
#210506=CARTESIAN_POINT('Ctrl Pts',(18.5688608504302,21.7042995631227,13.4828333725429));
#210507=CARTESIAN_POINT('Ctrl Pts',(20.7410836698255,20.6994316553031,13.6100091792244));
#210508=CARTESIAN_POINT('Ctrl Pts',(21.0719317958176,18.3290200862303,13.7371849859058));
#210509=CARTESIAN_POINT('Ctrl Pts',(19.2578726075595,16.7677703461939,13.8643607925872));
#210510=CARTESIAN_POINT('Ctrl Pts',(16.9631928170665,17.4480321695901,13.9915365992687));
#210511=CARTESIAN_POINT('Ctrl Pts',(16.2931187082259,19.7457075552633,14.1187124059501));
#210512=CARTESIAN_POINT('Ctrl Pts',(17.862401686409,21.5528219466762,14.2458882126315));
#210513=CARTESIAN_POINT('Ctrl Pts',(20.2313220198197,21.211460051876,14.373064019313));
#210514=CARTESIAN_POINT('Ctrl Pts',(21.2265423343311,19.0348002220335,14.5002398259944));
#210515=CARTESIAN_POINT('Ctrl Pts',(19.9350097617186,17.0197927522835,14.6274156326758));
#210516=CARTESIAN_POINT('Ctrl Pts',(17.5416252758018,17.0150819306536,14.7545914393573));
#210517=CARTESIAN_POINT('Ctrl Pts',(16.2421705922151,19.0249896436024,14.8817672460387));
#210518=CARTESIAN_POINT('Ctrl Pts',(17.2288147298954,21.2055503134414,15.0089430527202));
#210519=CARTESIAN_POINT('Ctrl Pts',(19.5963729305628,21.5562348664518,15.1361188594016));
#210520=CARTESIAN_POINT('Ctrl Pts',(21.1727574923393,19.7553119911849,15.263294666083));
#210521=CARTESIAN_POINT('Ctrl Pts',(20.5117334212554,17.455016647818,15.3904704727644));
#210522=CARTESIAN_POINT('Ctrl Pts',(18.2197492747497,16.7657270414598,15.5176462794459));
#210523=CARTESIAN_POINT('Ctrl Pts',(16.3995582506614,18.3198236038058,15.6448220861273));
#210524=CARTESIAN_POINT('Ctrl Pts',(16.7210726397956,20.6915191970148,15.7719978928088));
#210525=CARTESIAN_POINT('Ctrl Pts',(18.8893229455551,21.7049303183475,15.8991736994902));
#210526=CARTESIAN_POINT('Ctrl Pts',(20.915074089197,20.4303151633691,16.0263495061716));
#210527=CARTESIAN_POINT('Ctrl Pts',(20.9398251287259,18.0370540252336,16.153525312853));
#210528=CARTESIAN_POINT('Ctrl Pts',(18.9408685215966,16.7208154556417,16.2807011195345));
#210529=CARTESIAN_POINT('Ctrl Pts',(16.7521228856109,17.6891666472147,16.4078769262159));
#210530=CARTESIAN_POINT('Ctrl Pts',(16.3816264929107,20.0537054843378,16.5350527328974));
#210531=CARTESIAN_POINT('Ctrl Pts',(18.1692867881987,21.6451143437821,16.6622285395788));
#210532=CARTESIAN_POINT('Ctrl Pts',(20.4750364052595,21.003374370981,16.7894043462602));
#210533=CARTESIAN_POINT('Ctrl Pts',(21.1834931814011,18.7172421601046,16.9165801529417));
#210534=CARTESIAN_POINT('Ctrl Pts',(19.6446919963,16.8841021212645,17.0437559596231));
#210535=CARTESIAN_POINT('Ctrl Pts',(17.2703874285137,17.1857464625939,17.1709317663045));
#210536=CARTESIAN_POINT('Ctrl Pts',(16.2388565530248,19.3454352230824,17.298107572986));
#210537=CARTESIAN_POINT('Ctrl Pts',(17.4964649240676,21.3817880103836,17.4252833796674));
#210538=CARTESIAN_POINT('Ctrl Pts',(19.8894349171892,21.4265775324573,17.5524591863489));
#210539=CARTESIAN_POINT('Ctrl Pts',(21.2223650881682,19.4387121827512,17.6796349930303));
#210540=CARTESIAN_POINT('Ctrl Pts',(20.272374736109,17.2419350387839,17.8068107997117));
#210541=CARTESIAN_POINT('Ctrl Pts',(17.9110210459732,16.8516527827758,17.9339866063932));
#210542=CARTESIAN_POINT('Ctrl Pts',(16.3046994663247,18.6259251609712,18.0611624130746));
#210543=CARTESIAN_POINT('Ctrl Pts',(16.9271103469226,20.9369673901283,18.188338219756));
#210544=CARTESIAN_POINT('Ctrl Pts',(19.2072303360084,21.6645416644746,18.3155140264374));
#210545=CARTESIAN_POINT('Ctrl Pts',(21.053190863776,20.1411437456081,18.4426898331189));
#210546=CARTESIAN_POINT('Ctrl Pts',(20.7714377192819,17.764396671431,18.5698656398003));
#210547=CARTESIAN_POINT('Ctrl Pts',(18.6204619249281,16.714818364785,18.6970414464817));
#210548=CARTESIAN_POINT('Ctrl Pts',(16.5736502676105,17.9553317781408,18.8242172531632));
#210549=CARTESIAN_POINT('Ctrl Pts',(16.5088254030919,20.347842849113,18.9513930598446));
#210550=CARTESIAN_POINT('Ctrl Pts',(18.4854601217909,21.6973711671813,19.078568866526));
#210551=CARTESIAN_POINT('Ctrl Pts',(20.6901147517246,20.7658082595486,19.2057446732075));
#210552=CARTESIAN_POINT('Ctrl Pts',(21.100155508854,18.4078052787827,19.3329204798889));
#210553=CARTESIAN_POINT('Ctrl Pts',(19.3393954434522,16.786683597609,19.4600962865703));
#210554=CARTESIAN_POINT('Ctrl Pts',(17.02322264018,17.3897217556752,19.5872720932518));
#210555=CARTESIAN_POINT('Ctrl Pts',(16.2765818693588,19.6636696421892,19.7144478999332));
#210556=CARTESIAN_POINT('Ctrl Pts',(17.7844697326546,21.5223212653023,19.8416237066147));
#210557=CARTESIAN_POINT('Ctrl Pts',(20.1634926358433,21.2604790121031,19.9687995132961));
#210558=CARTESIAN_POINT('Ctrl Pts',(21.231044858401,19.1183671093666,20.0959753199775));
#210559=CARTESIAN_POINT('Ctrl Pts',(20.0077132370737,17.0612398664333,20.2231511266589));
#210560=CARTESIAN_POINT('Ctrl Pts',(17.6158291045619,16.976384633048,20.3503269333404));
#210561=CARTESIAN_POINT('Ctrl Pts',(16.2497967346393,18.9416493085074,20.4775027400218));
#210562=CARTESIAN_POINT('Ctrl Pts',(17.1628678921721,21.1540284415978,20.6046785467032));
#210563=CARTESIAN_POINT('Ctrl Pts',(19.5173528955041,21.5837958860619,20.7318543533847));
#210564=CARTESIAN_POINT('Ctrl Pts',(21.1531647607153,19.8366774894172,20.8590301600661));
#210565=CARTESIAN_POINT('Ctrl Pts',(20.5695343937816,17.5155251277943,20.9862059667476));
#210566=CARTESIAN_POINT('Ctrl Pts',(18.301931936395,16.7498921279798,21.113381773429));
#210567=CARTESIAN_POINT('Ctrl Pts',(16.430692762331,18.2421219844588,21.2405575801104));
#210568=CARTESIAN_POINT('Ctrl Pts',(16.6726573424412,20.6233352795928,21.3677333867919));
#210569=CARTESIAN_POINT('Ctrl Pts',(18.8056557941431,21.7086298106478,21.4949091934733));
#210570=CARTESIAN_POINT('Ctrl Pts',(20.8731458549779,20.5028678015929,21.6220850001547));
#210571=CARTESIAN_POINT('Ctrl Pts',(20.9776565334948,18.111196073242,21.7492608068362));
#210572=CARTESIAN_POINT('Ctrl Pts',(19.0246114642159,16.7298799538284,21.8764366135176));
#210573=CARTESIAN_POINT('Ctrl Pts',(16.8032831853607,17.6222026293144,22.0036124201991));
#210574=CARTESIAN_POINT('Ctrl Pts',(16.3565572075883,19.9774759742341,22.1307882268804));
#210575=CARTESIAN_POINT('Ctrl Pts',(17.5080922618947,21.070504731278,22.2155720980014));
#210576=CARTESIAN_POINT('Ctrl Pts',(18.1877583250969,21.2523734297384,22.2579640335619));
#210577=CARTESIAN_POINT('Ctrl Pts',(20.4651728790455,20.6688093317616,-0.0844764937345476));
#210578=CARTESIAN_POINT('Ctrl Pts',(20.9507812712845,20.0921819204693,-0.042065902122372));
#210579=CARTESIAN_POINT('Ctrl Pts',(21.2916314586439,18.4257343942419,0.0427366250502814));
#210580=CARTESIAN_POINT('Ctrl Pts',(19.4543545616952,16.6318010405789,0.169931087783413));
#210581=CARTESIAN_POINT('Ctrl Pts',(16.9568469381246,17.2110808818736,0.297106894464847));
#210582=CARTESIAN_POINT('Ctrl Pts',(16.0896125331239,19.6218277093859,0.424282701146282));
#210583=CARTESIAN_POINT('Ctrl Pts',(17.6485150766254,21.6573815714476,0.551458507827716));
#210584=CARTESIAN_POINT('Ctrl Pts',(20.203243920748,21.4476431071891,0.67863431450915));
#210585=CARTESIAN_POINT('Ctrl Pts',(21.4100527174681,19.1863847097626,0.805810121190585));
#210586=CARTESIAN_POINT('Ctrl Pts',(20.1617388348746,16.9474699013169,0.932985927872018));
#210587=CARTESIAN_POINT('Ctrl Pts',(17.6035685870678,16.7853277296908,1.06016173455346));
#210588=CARTESIAN_POINT('Ctrl Pts',(16.0824961952363,18.8485248156151,1.18733754123489));
#210589=CARTESIAN_POINT('Ctrl Pts',(16.994015428193,21.2443038613797,1.31451334791632));
#210590=CARTESIAN_POINT('Ctrl Pts',(19.5018617550643,21.7746354401676,1.44168915459776));
#210591=CARTESIAN_POINT('Ctrl Pts',(21.3052429724622,19.9529996381475,1.56886496127919));
#210592=CARTESIAN_POINT('Ctrl Pts',(20.7496681485409,17.4506205409442,1.69604076796063));
#210593=CARTESIAN_POINT('Ctrl Pts',(18.3448430103915,16.5632827654992,1.82321657464206));
#210594=CARTESIAN_POINT('Ctrl Pts',(16.2970452015994,18.1050599558195,1.9503923813235));
#210595=CARTESIAN_POINT('Ctrl Pts',(16.4850021943108,20.6614691488127,2.07756818800493));
#210596=CARTESIAN_POINT('Ctrl Pts',(18.736275070432,21.8871625843198,2.20474399468636));
#210597=CARTESIAN_POINT('Ctrl Pts',(20.9854607183013,20.6576431264228,2.3319198013678));
#210598=CARTESIAN_POINT('Ctrl Pts',(21.169070894564,18.1009182973116,2.45909560804923));
#210599=CARTESIAN_POINT('Ctrl Pts',(19.1186546646734,16.5626245784783,2.58627141473067));
#210600=CARTESIAN_POINT('Ctrl Pts',(16.7153416532344,17.4540509075189,2.7134472214121));
#210601=CARTESIAN_POINT('Ctrl Pts',(16.1640223834416,19.9573689931488,2.84062302809354));
#210602=CARTESIAN_POINT('Ctrl Pts',(17.9704980657522,21.7759398458068,2.96779883477497));
#210603=CARTESIAN_POINT('Ctrl Pts',(20.4774393846103,21.2413375915055,3.0949746414564));
#210604=CARTESIAN_POINT('Ctrl Pts',(21.384883278063,18.8440266121716,3.22215044813784));
#210605=CARTESIAN_POINT('Ctrl Pts',(19.8603062963049,16.7833909401617,3.34932625481927));
#210606=CARTESIAN_POINT('Ctrl Pts',(17.3024131941191,16.9499359056603,3.4765020615007));
#210607=CARTESIAN_POINT('Ctrl Pts',(16.0579121320417,19.1908668405009,3.60367786818214));
#210608=CARTESIAN_POINT('Ctrl Pts',(17.268555592065,21.4502686994473,3.73085367486357));
#210609=CARTESIAN_POINT('Ctrl Pts',(19.8236533406339,21.6552805114082,3.85802948154501));
#210610=CARTESIAN_POINT('Ctrl Pts',(21.3790617806833,19.6178166632753,3.98520528822644));
#210611=CARTESIAN_POINT('Ctrl Pts',(20.5077902080058,17.2071237764952,4.11238109490788));
#210612=CARTESIAN_POINT('Ctrl Pts',(18.0091762133191,16.634862950186,4.23955690158931));
#210613=CARTESIAN_POINT('Ctrl Pts',(16.1755430552745,18.4260479739882,4.36673270827075));
#210614=CARTESIAN_POINT('Ctrl Pts',(16.6891353482686,20.9373777620364,4.49390851495218));
#210615=CARTESIAN_POINT('Ctrl Pts',(19.0787640406122,21.8648631045058,4.62108432163361));
#210616=CARTESIAN_POINT('Ctrl Pts',(21.1520931241638,20.3575937659115,4.74826012831505));
#210617=CARTESIAN_POINT('Ctrl Pts',(21.0069718500806,17.7983958127287,4.87543593499648));
#210618=CARTESIAN_POINT('Ctrl Pts',(18.7765399800919,16.5351745252634,5.00261174167792));
#210619=CARTESIAN_POINT('Ctrl Pts',(16.5070803186978,17.7268570304097,5.12978754835935));
#210620=CARTESIAN_POINT('Ctrl Pts',(16.280681246675,20.2801485938535,5.25696335504078));
#210621=CARTESIAN_POINT('Ctrl Pts',(18.305049860693,21.8525626812824,5.38413916172222));
#210622=CARTESIAN_POINT('Ctrl Pts',(20.722953603877,21.0015069625052,5.51131496840365));
#210623=CARTESIAN_POINT('Ctrl Pts',(21.3161158638869,18.5077722370249,5.63849077508509));
#210624=CARTESIAN_POINT('Ctrl Pts',(19.5403470829654,16.6592053368368,5.76566658176652));
#210625=CARTESIAN_POINT('Ctrl Pts',(17.0248049009675,17.1517516578618,5.89284238844796));
#210626=CARTESIAN_POINT('Ctrl Pts',(16.0773431377199,19.5335305214322,6.02001819512939));
#210627=CARTESIAN_POINT('Ctrl Pts',(17.5671991548932,21.6194076500902,6.14719400181082));
#210628=CARTESIAN_POINT('Ctrl Pts',(20.127522527624,21.4957202424278,6.27436980849226));
#210629=CARTESIAN_POINT('Ctrl Pts',(21.4093754730223,19.2759438180688,6.40154561517369));
#210630=CARTESIAN_POINT('Ctrl Pts',(20.2367374744517,16.9965854714996,6.52872142185513));
#210631=CARTESIAN_POINT('Ctrl Pts',(17.6854311134782,16.7488150127633,6.65589722853656));
#210632=CARTESIAN_POINT('Ctrl Pts',(16.0961216243634,18.7599464593815,6.78307303521799));
#210633=CARTESIAN_POINT('Ctrl Pts',(16.9269018196985,21.1848915339771,6.91024884189944));
#210634=CARTESIAN_POINT('Ctrl Pts',(19.4155824342976,21.7989136396742,7.03742464858086));
#210635=CARTESIAN_POINT('Ctrl Pts',(21.2789534692056,20.0386856050059,7.1646004552623));
#210636=CARTESIAN_POINT('Ctrl Pts',(20.8074876537439,17.5191073997068,7.29177626194374));
#210637=CARTESIAN_POINT('Ctrl Pts',(18.4337256111302,16.551735644479,7.41895206862516));
#210638=CARTESIAN_POINT('Ctrl Pts',(16.335446683174,18.0240738828814,7.54612787530661));
#210639=CARTESIAN_POINT('Ctrl Pts',(16.4376915523973,20.5853431647969,7.67330368198803));
#210640=CARTESIAN_POINT('Ctrl Pts',(18.64665689732,21.8857378943683,7.80047948866947));
#210641=CARTESIAN_POINT('Ctrl Pts',(20.9357541178272,20.7322266188132,7.92765529535091));
#210642=CARTESIAN_POINT('Ctrl Pts',(21.2048785915005,18.1830843384694,8.05483110203234));
#210643=CARTESIAN_POINT('Ctrl Pts',(19.2071253174932,16.5769908779387,8.18200690871378));
#210644=CARTESIAN_POINT('Ctrl Pts',(16.7753089301549,17.3874373018554,8.3091827153952));
#210645=CARTESIAN_POINT('Ctrl Pts',(16.1404700293211,19.8708893182541,8.43635852207665));
#210646=CARTESIAN_POINT('Ctrl Pts',(17.8850339039608,21.7489338425049,8.56353432875807));
#210647=CARTESIAN_POINT('Ctrl Pts',(20.4084714789379,21.2985815881968,8.69071013543951));
#210648=CARTESIAN_POINT('Ctrl Pts',(21.3956854014105,18.9330027966444,8.81788594212095));
#210649=CARTESIAN_POINT('Ctrl Pts',(19.9409681709163,16.8224691847183,8.94506174880238));
#210650=CARTESIAN_POINT('Ctrl Pts',(17.3789325564997,16.9032643468714,9.07223755548381));
#210651=CARTESIAN_POINT('Ctrl Pts',(16.0600872165237,19.1012637365415,9.19941336216525));
#210652=CARTESIAN_POINT('Ctrl Pts',(17.1943908936429,21.3999393369342,9.32658916884668));
#210653=CARTESIAN_POINT('Ctrl Pts',(19.7411903669265,21.6903989565872,9.45376497552812));
#210654=CARTESIAN_POINT('Ctrl Pts',(21.3639551918393,19.7061639224262,9.58094078220955));
#210655=CARTESIAN_POINT('Ctrl Pts',(20.5738993616681,17.2676467227782,9.70811658889098));
#210656=CARTESIAN_POINT('Ctrl Pts',(18.0958500641997,16.6120355368737,9.83529239557241));
#210657=CARTESIAN_POINT('Ctrl Pts',(16.2032637247762,18.3408129359606,9.96246820225386));
#210658=CARTESIAN_POINT('Ctrl Pts',(16.6324708426624,20.8679329564033,10.0896440089353));
#210659=CARTESIAN_POINT('Ctrl Pts',(18.989700526796,21.8749198302035,10.2168198156167));
#210660=CARTESIAN_POINT('Ctrl Pts',(21.1123408481587,20.4379256013037,10.3439956222982));
#210661=CARTESIAN_POINT('Ctrl Pts',(21.0530010578169,17.8753032847989,10.4711714289796));
#210662=CARTESIAN_POINT('Ctrl Pts',(18.8661217303663,16.5380998018032,10.5983472356611));
#210663=CARTESIAN_POINT('Ctrl Pts',(16.5580289157041,17.6531163517569,10.7255230423425));
#210664=CARTESIAN_POINT('Ctrl Pts',(16.2462545148863,20.1973944558094,10.8526988490239));
#210665=CARTESIAN_POINT('Ctrl Pts',(18.2168321897617,21.8367168692014,10.9798746557054));
#210666=CARTESIAN_POINT('Ctrl Pts',(20.6618792314763,21.0671070254696,11.1070504623868));
#210667=CARTESIAN_POINT('Ctrl Pts',(21.3382167359914,18.5946341888639,11.2342262690682));
#210668=CARTESIAN_POINT('Ctrl Pts',(19.6253470211541,16.6876387279989,11.3614020757497));
#210669=CARTESIAN_POINT('Ctrl Pts',(17.0947217376433,17.0956706167312,11.4885778824311));
#210670=CARTESIAN_POINT('Ctrl Pts',(16.0680325147611,19.4443859224641,11.6157536891125));
#210671=CARTESIAN_POINT('Ctrl Pts',(17.487202990982,21.5789841299002,11.742929495794));
#210672=CARTESIAN_POINT('Ctrl Pts',(20.0502323380272,21.5411038718235,11.8701053024754));
#210673=CARTESIAN_POINT('Ctrl Pts',(21.4057002095246,19.3654979339054,11.9972811091568));
#210674=CARTESIAN_POINT('Ctrl Pts',(20.3100489631998,17.0481497308524,12.1244569158383));
#210675=CARTESIAN_POINT('Ctrl Pts',(17.7684706137698,16.715082408115,12.2516327225197));
#210676=CARTESIAN_POINT('Ctrl Pts',(16.1127055486938,18.6718645618152,12.3788085292011));
#210677=CARTESIAN_POINT('Ctrl Pts',(16.8618154468087,21.1232700175309,12.5059843358826));
#210678=CARTESIAN_POINT('Ctrl Pts',(19.3285384715983,21.8202864210249,12.633160142564));
#210679=CARTESIAN_POINT('Ctrl Pts',(21.2498093499156,20.1234444838084,12.7603359492454));
#210680=CARTESIAN_POINT('Ctrl Pts',(20.8629812984238,17.5894913653894,12.8875117559269));
#210681=CARTESIAN_POINT('Ctrl Pts',(18.5229450451101,16.5431717770494,13.0146875626083));
#210682=CARTESIAN_POINT('Ctrl Pts',(16.37653861336,17.9444189991726,13.1418633692897));
#210683=CARTESIAN_POINT('Ctrl Pts',(16.3929566832965,20.5076756766722,13.2690391759712));
#210684=CARTESIAN_POINT('Ctrl Pts',(18.5571366947732,21.881312901594,13.3962149826526));
#210685=CARTESIAN_POINT('Ctrl Pts',(20.8835778114207,20.8051037776138,13.523390789334));
#210686=CARTESIAN_POINT('Ctrl Pts',(21.2379147039354,18.2664033789119,13.6505665960155));
#210687=CARTESIAN_POINT('Ctrl Pts',(19.2950652660628,16.5943117517799,13.7777424026969));
#210688=CARTESIAN_POINT('Ctrl Pts',(16.8374732702154,17.3228691824008,13.9049182093783));
#210689=CARTESIAN_POINT('Ctrl Pts',(16.119826837221,19.7836694475537,14.0320940160598));
#210690=CARTESIAN_POINT('Ctrl Pts',(17.800522027191,21.7190810384507,14.1592698227412));
#210691=CARTESIAN_POINT('Ctrl Pts',(20.337625319036,21.3534839456345,14.2864456294226));
#210692=CARTESIAN_POINT('Ctrl Pts',(21.4035019128779,19.0222908102495,14.4136214361041));
#210693=CARTESIAN_POINT('Ctrl Pts',(20.0202761896291,16.8642266438473,14.5407972427855));
#210694=CARTESIAN_POINT('Ctrl Pts',(17.4569718976996,16.8591813745337,14.667973049467));
#210695=CARTESIAN_POINT('Ctrl Pts',(16.0652616283277,19.011783723759,14.7951488561484));
#210696=CARTESIAN_POINT('Ctrl Pts',(17.1219531743809,21.347154641679,14.9223246628298));
#210697=CARTESIAN_POINT('Ctrl Pts',(19.6575976280295,21.7227362605683,15.0495004695112));
#210698=CARTESIAN_POINT('Ctrl Pts',(21.3458985828949,19.7939557563202,15.1766762761927));
#210699=CARTESIAN_POINT('Ctrl Pts',(20.6379447006631,17.3303495279633,15.3038520828741));
#210700=CARTESIAN_POINT('Ctrl Pts',(18.1832397277084,16.5921233813674,15.4310278895556));
#210701=CARTESIAN_POINT('Ctrl Pts',(16.2338231205434,18.2565539865522,15.558203696237));
#210702=CARTESIAN_POINT('Ctrl Pts',(16.5781636218018,20.7966295694748,15.6853795029184));
#210703=CARTESIAN_POINT('Ctrl Pts',(18.9003501937609,21.8819884376745,15.8125553095998));
#210704=CARTESIAN_POINT('Ctrl Pts',(21.0699207878016,20.5168811945468,15.9397311162813));
#210705=CARTESIAN_POINT('Ctrl Pts',(21.0964290426296,17.9537090075503,16.0669069229627));
#210706=CARTESIAN_POINT('Ctrl Pts',(18.9555552797279,16.5440232698465,16.1940827296442));
#210707=CARTESIAN_POINT('Ctrl Pts',(16.6114182989473,17.5811231508143,16.3212585363256));
#210708=CARTESIAN_POINT('Ctrl Pts',(16.2146182866043,20.1135338793437,16.448434343007));
#210709=CARTESIAN_POINT('Ctrl Pts',(18.1291946258374,21.8179257911455,16.5756101496885));
#210710=CARTESIAN_POINT('Ctrl Pts',(20.5986423574096,21.1306250936339,16.7027859563699));
#210711=CARTESIAN_POINT('Ctrl Pts',(21.3573964588153,18.6821875180837,16.8299617630513));
#210712=CARTESIAN_POINT('Ctrl Pts',(19.7093471356056,16.7189025728874,16.9571375697328));
#210713=CARTESIAN_POINT('Ctrl Pts',(17.1664773523482,17.0419623400562,17.0843133764142));
#210714=CARTESIAN_POINT('Ctrl Pts',(16.0617123068835,19.3549795345634,17.2114891830956));
#210715=CARTESIAN_POINT('Ctrl Pts',(17.4086053589731,21.5359044424863,17.3386649897771));
#210716=CARTESIAN_POINT('Ctrl Pts',(19.9714657309362,21.5838738242719,17.4658407964585));
#210717=CARTESIAN_POINT('Ctrl Pts',(21.3990281005501,19.4548787494468,17.5930166031399));
#210718=CARTESIAN_POINT('Ctrl Pts',(20.3815925982089,17.1021400588277,17.7201924098214));
#210719=CARTESIAN_POINT('Ctrl Pts',(17.8525931481391,16.6841494736224,17.8473682165028));
#210720=CARTESIAN_POINT('Ctrl Pts',(16.1322297783753,18.5843874123414,17.9745440231842));
#210721=CARTESIAN_POINT('Ctrl Pts',(16.7988291028752,21.0595035082659,18.1017198298657));
#210722=CARTESIAN_POINT('Ctrl Pts',(19.240827615245,21.8387323664387,18.2288956365471));
#210723=CARTESIAN_POINT('Ctrl Pts',(21.2178432478782,20.2071798738389,18.3560714432285));
#210724=CARTESIAN_POINT('Ctrl Pts',(20.9160868653179,17.661694176945,18.48324724991));
#210725=CARTESIAN_POINT('Ctrl Pts',(18.6124012193438,16.53760041183,18.6104230565914));
#210726=CARTESIAN_POINT('Ctrl Pts',(16.4202749074846,17.8661848391805,18.7375988632728));
#210727=CARTESIAN_POINT('Ctrl Pts',(16.3508477617745,20.4285537075334,18.8647746699543));
#210728=CARTESIAN_POINT('Ctrl Pts',(18.4678148800254,21.8738926199146,18.9919504766357));
#210729=CARTESIAN_POINT('Ctrl Pts',(20.8289903235801,20.8761928297688,19.1191262833172));
#210730=CARTESIAN_POINT('Ctrl Pts',(21.2681421768659,18.3507819747449,19.2463020899985));
#210731=CARTESIAN_POINT('Ctrl Pts',(19.3823758659115,16.6145677611307,19.37347789668));
#210732=CARTESIAN_POINT('Ctrl Pts',(16.901764947602,17.260418984728,19.5006537033614));
#210733=CARTESIAN_POINT('Ctrl Pts',(16.1021159552911,19.6958072023018,19.6278295100429));
#210734=CARTESIAN_POINT('Ctrl Pts',(17.71705724637,21.6864149424128,19.7550053167243));
#210735=CARTESIAN_POINT('Ctrl Pts',(20.2649803461583,21.4059830371408,19.8821811234057));
#210736=CARTESIAN_POINT('Ctrl Pts',(21.4083240964178,19.11179058023,20.0093569300872));
#210737=CARTESIAN_POINT('Ctrl Pts',(20.0981412930058,16.9086163213995,20.1365327367686));
#210738=CARTESIAN_POINT('Ctrl Pts',(17.5364438729955,16.8177367384453,20.2637085434501));
#210739=CARTESIAN_POINT('Ctrl Pts',(16.0734291934315,18.9225265902324,20.3908843501315));
#210740=CARTESIAN_POINT('Ctrl Pts',(17.051324400287,21.2919749428039,20.5180601568129));
#210741=CARTESIAN_POINT('Ctrl Pts',(19.5729675169019,21.7522539917445,20.6452359634943));
#210742=CARTESIAN_POINT('Ctrl Pts',(21.3249148532192,19.8810978482246,20.7724117701758));
#210743=CARTESIAN_POINT('Ctrl Pts',(20.6998492888418,17.3951538447513,20.8995875768572));
#210744=CARTESIAN_POINT('Ctrl Pts',(18.2712569980454,16.5751642584499,21.0267633835387));
#210745=CARTESIAN_POINT('Ctrl Pts',(16.2671680460494,18.173335892872,21.1539391902201));
#210746=CARTESIAN_POINT('Ctrl Pts',(16.5263110505858,20.7236048928311,21.2811149969015));
#210747=CARTESIAN_POINT('Ctrl Pts',(18.8107430413917,21.8859505777098,21.408290803583));
#210748=CARTESIAN_POINT('Ctrl Pts',(21.0250158327644,20.594584752017,21.5354666102644));
#210749=CARTESIAN_POINT('Ctrl Pts',(21.1369463112861,18.033114815932,21.6626424169459));
#210750=CARTESIAN_POINT('Ctrl Pts',(19.045243604148,16.5537313076661,21.7898182236272));
#210751=CARTESIAN_POINT('Ctrl Pts',(16.6662107556949,17.5094049812102,21.9169940303087));
#210752=CARTESIAN_POINT('Ctrl Pts',(16.1877691919268,20.0318924082093,22.0441698369901));
#210753=CARTESIAN_POINT('Ctrl Pts',(17.4210581868123,21.2025214152156,22.1289537081111));
#210754=CARTESIAN_POINT('Ctrl Pts',(18.1489775608771,21.3973019939627,22.1713456436716));
#210755=CARTESIAN_POINT('Ctrl Pts',(20.579931224634,20.7654465822185,-0.171094883624917));
#210756=CARTESIAN_POINT('Ctrl Pts',(21.0977302873553,20.150594907745,-0.128684292012742));
#210757=CARTESIAN_POINT('Ctrl Pts',(21.4611752161576,18.3736796382696,-0.0438817648400879));
#210758=CARTESIAN_POINT('Ctrl Pts',(19.5021064059726,16.4608275871995,0.0833126978930438));
#210759=CARTESIAN_POINT('Ctrl Pts',(16.8390405955535,17.0785075195682,0.210488504574479));
#210760=CARTESIAN_POINT('Ctrl Pts',(15.9143177751785,19.6490612161152,0.337664311255912));
#210761=CARTESIAN_POINT('Ctrl Pts',(17.5765589736414,21.8195506449214,0.464840117937347));
#210762=CARTESIAN_POINT('Ctrl Pts',(20.300639162813,21.5959087516894,0.592015924618781));
#210763=CARTESIAN_POINT('Ctrl Pts',(21.5874465446713,19.1847529778785,0.719191731300216));
#210764=CARTESIAN_POINT('Ctrl Pts',(20.2563827312793,16.7974219353056,0.84636753798165));
#210765=CARTESIAN_POINT('Ctrl Pts',(17.5286330099687,16.6245314625761,0.973543344663085));
#210766=CARTESIAN_POINT('Ctrl Pts',(15.9067296997928,18.8244965669171,1.10071915134451));
#210767=CARTESIAN_POINT('Ctrl Pts',(16.8786729611136,21.3790902770145,1.22789495802595));
#210768=CARTESIAN_POINT('Ctrl Pts',(19.5527628208785,21.9445771977858,1.35507076470738));
#210769=CARTESIAN_POINT('Ctrl Pts',(21.4756890285423,20.0021863207324,1.48224657138882));
#210770=CARTESIAN_POINT('Ctrl Pts',(20.8832855040238,17.3339261098018,1.60942237807025));
#210771=CARTESIAN_POINT('Ctrl Pts',(18.3190460418495,16.3877672793826,1.73659818475169));
#210772=CARTESIAN_POINT('Ctrl Pts',(16.1355010228962,18.0317478959283,1.86377399143312));
#210773=CARTESIAN_POINT('Ctrl Pts',(16.3359175647298,20.7576198232253,1.99094979811455));
#210774=CARTESIAN_POINT('Ctrl Pts',(18.7364258833992,22.0645636945266,2.11812560479599));
#210775=CARTESIAN_POINT('Ctrl Pts',(21.1347086127881,20.7535401762524,2.24530141147742));
#210776=CARTESIAN_POINT('Ctrl Pts',(21.3304901904839,18.0273316895207,2.37247721815886));
#210777=CARTESIAN_POINT('Ctrl Pts',(19.1441531769682,16.387065461564,2.49965302484029));
#210778=CARTESIAN_POINT('Ctrl Pts',(16.5815260794188,17.337583873188,2.62682883152173));
#210779=CARTESIAN_POINT('Ctrl Pts',(15.9936602069971,20.0068453174889,2.75400463820316));
#210780=CARTESIAN_POINT('Ctrl Pts',(17.9198860096782,21.9459680716425,2.88118044488459));
#210781=CARTESIAN_POINT('Ctrl Pts',(20.5930108690263,21.3759273750031,3.00835625156603));
#210782=CARTESIAN_POINT('Ctrl Pts',(21.5606086391872,18.8197001804373,3.13553205824747));
#210783=CARTESIAN_POINT('Ctrl Pts',(19.9349684220548,16.6224662845049,3.2627078649289));
#210784=CARTESIAN_POINT('Ctrl Pts',(17.2075142181716,16.8000514095034,3.38988367161033));
#210785=CARTESIAN_POINT('Ctrl Pts',(15.8805159747347,19.1895322262035,3.51705947829177));
#210786=CARTESIAN_POINT('Ctrl Pts',(17.1714122172801,21.5987083927831,3.6442352849732));
#210787=CARTESIAN_POINT('Ctrl Pts',(19.8958857653384,21.8173103069526,3.77141109165464));
#210788=CARTESIAN_POINT('Ctrl Pts',(21.5544012384607,19.6447842803171,3.89858689833607));
#210789=CARTESIAN_POINT('Ctrl Pts',(20.6253736291394,17.0742881001989,4.02576270501751));
#210790=CARTESIAN_POINT('Ctrl Pts',(17.961128106969,16.464092468841,4.15293851169893));
#210791=CARTESIAN_POINT('Ctrl Pts',(16.0059445768151,18.3740140050173,4.28011431838038));
#210792=CARTESIAN_POINT('Ctrl Pts',(16.5535825752176,21.0518182423779,4.4072901250618));
#210793=CARTESIAN_POINT('Ctrl Pts',(19.10161822889,22.0407859964237,4.53446593174324));
#210794=CARTESIAN_POINT('Ctrl Pts',(21.3123869745163,20.4336007350771,4.66164173842467));
#210795=CARTESIAN_POINT('Ctrl Pts',(21.1576457037679,17.7047551824572,4.78881754510611));
#210796=CARTESIAN_POINT('Ctrl Pts',(18.7793599282299,16.3577957618358,4.91599335178754));
#210797=CARTESIAN_POINT('Ctrl Pts',(16.3594592338956,17.6284741399031,5.04316915846899));
#210798=CARTESIAN_POINT('Ctrl Pts',(16.1180523118408,20.3510217719769,5.17034496515041));
#210799=CARTESIAN_POINT('Ctrl Pts',(18.2766150296472,22.0276701859931,5.29752077183185));
#210800=CARTESIAN_POINT('Ctrl Pts',(20.8548000692393,21.1201985266286,5.42469657851329));
#210801=CARTESIAN_POINT('Ctrl Pts',(21.4872826770021,18.4611557173071,5.55187238519472));
#210802=CARTESIAN_POINT('Ctrl Pts',(19.5937993166108,16.4900484967713,5.67904819187615));
#210803=CARTESIAN_POINT('Ctrl Pts',(16.9115034483931,17.0152453991512,5.80622399855758));
#210804=CARTESIAN_POINT('Ctrl Pts',(15.9012350493816,19.5549108639094,5.93339980523902));
#210805=CARTESIAN_POINT('Ctrl Pts',(17.4898526713405,21.7790594565463,6.06057561192046));
#210806=CARTESIAN_POINT('Ctrl Pts',(20.2198982468525,21.6471728895478,6.18775141860188));
#210807=CARTESIAN_POINT('Ctrl Pts',(21.5867244061235,19.2802489023316,6.31492722528333));
#210808=CARTESIAN_POINT('Ctrl Pts',(20.3363529828215,16.8497933452978,6.44210303196475));
#210809=CARTESIAN_POINT('Ctrl Pts',(17.615922151023,16.5855983409401,6.56927883864619));
#210810=CARTESIAN_POINT('Ctrl Pts',(15.9212583499232,18.7300464079656,6.69645464532762));
#210811=CARTESIAN_POINT('Ctrl Pts',(16.8071104343333,21.315739544336,6.82363045200906));
#210812=CARTESIAN_POINT('Ctrl Pts',(19.4607640989881,21.9704647836472,6.95080625869048));
#210813=CARTESIAN_POINT('Ctrl Pts',(21.4476568108885,20.0935523556623,7.07798206537194));
#210814=CARTESIAN_POINT('Ctrl Pts',(20.9449378273356,17.4069529187342,7.20515787205335));
#210815=CARTESIAN_POINT('Ctrl Pts',(18.4138206134801,16.3754547070776,7.3323336787348));
#210816=CARTESIAN_POINT('Ctrl Pts',(16.1764481141826,17.9453933078879,7.45950948541623));
#210817=CARTESIAN_POINT('Ctrl Pts',(16.2854707305501,20.6764474963007,7.58668529209767));
#210818=CARTESIAN_POINT('Ctrl Pts',(18.640866978772,22.0630445627872,7.7138610987791));
#210819=CARTESIAN_POINT('Ctrl Pts',(21.0817069934834,20.8330677607659,7.84103690546054));
#210820=CARTESIAN_POINT('Ctrl Pts',(21.3686715568034,18.1149444651214,7.96821271214196));
#210821=CARTESIAN_POINT('Ctrl Pts',(19.2384884929154,16.4023840938492,8.0953885188234));
#210822=CARTESIAN_POINT('Ctrl Pts',(16.6454685488647,17.2665544941074,8.22256432550484));
#210823=CARTESIAN_POINT('Ctrl Pts',(15.9685465823494,19.9146329601232,8.34974013218628));
#210824=CARTESIAN_POINT('Ctrl Pts',(17.8287564831316,21.9171718576127,8.47691593886771));
#210825=CARTESIAN_POINT('Ctrl Pts',(20.5194711248913,21.4369660397109,8.60409174554914));
#210826=CARTESIAN_POINT('Ctrl Pts',(21.5721268283993,18.9145745394082,8.73126755223057));
#210827=CARTESIAN_POINT('Ctrl Pts',(20.0209773208683,16.6641350009595,8.858443358912));
#210828=CARTESIAN_POINT('Ctrl Pts',(17.2891060002617,16.7502860228609,8.98561916559344));
#210829=CARTESIAN_POINT('Ctrl Pts',(15.8828352441794,19.0939893896534,9.11279497227487));
#210830=CARTESIAN_POINT('Ctrl Pts',(17.0923311883199,21.5450427289413,9.23997077895631));
#210831=CARTESIAN_POINT('Ctrl Pts',(19.8079563737189,21.8547567314554,9.36714658563774));
#210832=CARTESIAN_POINT('Ctrl Pts',(21.5382932434809,19.7389880229077,9.49432239231918));
#210833=CARTESIAN_POINT('Ctrl Pts',(20.6958651164175,17.1388230739748,9.62149819900061));
#210834=CARTESIAN_POINT('Ctrl Pts',(18.0535475121228,16.439751840865,9.74867400568204));
#210835=CARTESIAN_POINT('Ctrl Pts',(16.035502831811,18.2831287907025,9.87584981236349));
#210836=CARTESIAN_POINT('Ctrl Pts',(16.4931618156892,20.9777699848882,10.0030256190449));
#210837=CARTESIAN_POINT('Ctrl Pts',(19.0066507515693,22.0515093760514,10.1302014257263));
#210838=CARTESIAN_POINT('Ctrl Pts',(21.2699995454986,20.5192577165824,10.2573772324077));
#210839=CARTESIAN_POINT('Ctrl Pts',(21.2067261583164,17.7867608017806,10.3845530390892));
#210840=CARTESIAN_POINT('Ctrl Pts',(18.874879995573,16.3609149530909,10.5117288457706));
#210841=CARTESIAN_POINT('Ctrl Pts',(16.4137851808899,17.5498452387121,10.6389046524521));
#210842=CARTESIAN_POINT('Ctrl Pts',(16.0813434539675,20.2627819149227,10.7660804591335));
#210843=CARTESIAN_POINT('Ctrl Pts',(18.1825494655964,22.0107739651396,10.8932562658149));
#210844=CARTESIAN_POINT('Ctrl Pts',(20.7896771156604,21.1901471759111,11.0204320724963));
#210845=CARTESIAN_POINT('Ctrl Pts',(21.5108486018171,18.5537756925119,11.1476078791778));
#210846=CARTESIAN_POINT('Ctrl Pts',(19.6844338464684,16.5203667192919,11.2747836858592));
#210847=CARTESIAN_POINT('Ctrl Pts',(16.9860550275624,16.9554467815862,11.4019594925407));
#210848=CARTESIAN_POINT('Ctrl Pts',(15.8913072311674,19.4598569263539,11.5291352992221));
#210849=CARTESIAN_POINT('Ctrl Pts',(17.4045536127647,21.7359562869947,11.6563111059035));
#210850=CARTESIAN_POINT('Ctrl Pts',(20.1374845399016,21.6955649707794,11.783486912585));
#210851=CARTESIAN_POINT('Ctrl Pts',(21.5828055117534,19.3757395033677,11.9106627192664));
#210852=CARTESIAN_POINT('Ctrl Pts',(20.4145242433828,16.9047757665027,12.0378385259478));
#210853=CARTESIAN_POINT('Ctrl Pts',(17.7044662868062,16.5496296234525,12.1650143326293));
#210854=CARTESIAN_POINT('Ctrl Pts',(15.9389416120162,18.6361256176097,12.2921901393107));
#210855=CARTESIAN_POINT('Ctrl Pts',(16.7377095273126,21.2500331768819,12.4193659459921));
#210856=CARTESIAN_POINT('Ctrl Pts',(19.3679500475393,21.9932543530368,12.5465417526735));
#210857=CARTESIAN_POINT('Ctrl Pts',(21.416580746526,20.183929846461,12.673717559355));
#210858=CARTESIAN_POINT('Ctrl Pts',(21.004110110314,17.4820025925939,12.8008933660364));
#210859=CARTESIAN_POINT('Ctrl Pts',(18.5089543468127,16.3663231463401,12.9280691727179));
#210860=CARTESIAN_POINT('Ctrl Pts',(16.2202640022022,17.8604581527614,13.0552449793993));
#210861=CARTESIAN_POINT('Ctrl Pts',(16.2377704155193,20.5936314799435,13.1824207860807));
#210862=CARTESIAN_POINT('Ctrl Pts',(18.5454125391162,22.0583262400653,13.3095965927622));
#210863=CARTESIAN_POINT('Ctrl Pts',(21.0260719530159,20.9107758999245,13.4367723994436));
#210864=CARTESIAN_POINT('Ctrl Pts',(21.4038976120531,18.2037866715935,13.563948206125));
#210865=CARTESIAN_POINT('Ctrl Pts',(19.3322579245662,16.4208531573659,13.6911240128065));
#210866=CARTESIAN_POINT('Ctrl Pts',(16.7117537233642,17.1977061952114,13.8182998194879));
#210867=CARTESIAN_POINT('Ctrl Pts',(15.9465349662162,19.8216313398441,13.9454756261693));
#210868=CARTESIAN_POINT('Ctrl Pts',(17.7386423679729,21.8853401302251,14.0726514328508));
#210869=CARTESIAN_POINT('Ctrl Pts',(20.4439286182524,21.495507839393,14.1998272395322));
#210870=CARTESIAN_POINT('Ctrl Pts',(21.5804614914246,19.0097813984656,14.3270030462136));
#210871=CARTESIAN_POINT('Ctrl Pts',(20.1055426175397,16.708660535411,14.4541788528951));
#210872=CARTESIAN_POINT('Ctrl Pts',(17.3723185195974,16.7032808184137,14.5813546595765));
#210873=CARTESIAN_POINT('Ctrl Pts',(15.8883526644403,18.9985778039157,14.708530466258));
#210874=CARTESIAN_POINT('Ctrl Pts',(17.0150916188663,21.4887589699166,14.8357062729394));
#210875=CARTESIAN_POINT('Ctrl Pts',(19.7188223254962,21.8892376546847,14.9628820796208));
#210876=CARTESIAN_POINT('Ctrl Pts',(21.5190396734505,19.8325995214557,15.0900578863023));
#210877=CARTESIAN_POINT('Ctrl Pts',(20.7641559800708,17.2056824081085,15.2172336929837));
#210878=CARTESIAN_POINT('Ctrl Pts',(18.1467301806671,16.4185197212751,15.3444094996651));
#210879=CARTESIAN_POINT('Ctrl Pts',(16.0680879904256,18.1932843692987,15.4715853063465));
#210880=CARTESIAN_POINT('Ctrl Pts',(16.4352546038082,20.9017399419349,15.598761113028));
#210881=CARTESIAN_POINT('Ctrl Pts',(18.9113774419666,22.0590465570016,15.7259369197094));
#210882=CARTESIAN_POINT('Ctrl Pts',(21.2247674864064,20.6034472257245,15.8531127263909));
#210883=CARTESIAN_POINT('Ctrl Pts',(21.2530329565334,17.870363989867,15.9802885330723));
#210884=CARTESIAN_POINT('Ctrl Pts',(18.9702420378592,16.3672310840514,16.1074643397537));
#210885=CARTESIAN_POINT('Ctrl Pts',(16.4707137122836,17.4730796544138,16.2346401464351));
#210886=CARTESIAN_POINT('Ctrl Pts',(16.0476100802981,20.1733622743496,16.3618159531166));
#210887=CARTESIAN_POINT('Ctrl Pts',(18.0891024634763,21.9907372385088,16.488991759798));
#210888=CARTESIAN_POINT('Ctrl Pts',(20.7222483095596,21.2578758162869,16.6161675664795));
#210889=CARTESIAN_POINT('Ctrl Pts',(21.5312997362295,18.6471328760627,16.7433433731609));
#210890=CARTESIAN_POINT('Ctrl Pts',(19.7740022749111,16.5537030245103,16.8705191798423));
#210891=CARTESIAN_POINT('Ctrl Pts',(17.0625672761828,16.8981782175187,16.9976949865238));
#210892=CARTESIAN_POINT('Ctrl Pts',(15.8845680607422,19.3645238460445,17.1248707932052));
#210893=CARTESIAN_POINT('Ctrl Pts',(17.3207457938787,21.6900208745888,17.2520465998866));
#210894=CARTESIAN_POINT('Ctrl Pts',(20.053496544683,21.7411701160866,17.3792224065681));
#210895=CARTESIAN_POINT('Ctrl Pts',(21.5756911129322,19.4710453161425,17.5063982132495));
#210896=CARTESIAN_POINT('Ctrl Pts',(20.4908104603086,16.9623450788714,17.6335740199309));
#210897=CARTESIAN_POINT('Ctrl Pts',(17.794165250305,16.516646164469,17.7607498266124));
#210898=CARTESIAN_POINT('Ctrl Pts',(15.959760090426,18.5428496637114,17.8879256332938));
#210899=CARTESIAN_POINT('Ctrl Pts',(16.6705478588277,21.1820396264035,18.0151014399752));
#210900=CARTESIAN_POINT('Ctrl Pts',(19.2744248944815,22.0129230684028,18.1422772466567));
#210901=CARTESIAN_POINT('Ctrl Pts',(21.3824956319804,20.2732160020698,18.2694530533381));
#210902=CARTESIAN_POINT('Ctrl Pts',(21.0607360113538,17.5589916824588,18.3966288600195));
#210903=CARTESIAN_POINT('Ctrl Pts',(18.6043405137593,16.360382458875,18.523804666701));
#210904=CARTESIAN_POINT('Ctrl Pts',(16.2668995473587,17.7770379002201,18.6509804733824));
#210905=CARTESIAN_POINT('Ctrl Pts',(16.1928701204568,20.5092645659538,18.7781562800638));
#210906=CARTESIAN_POINT('Ctrl Pts',(18.45016963826,22.0504140726478,18.9053320867453));
#210907=CARTESIAN_POINT('Ctrl Pts',(20.9678658954356,20.9865773999889,19.0325078934267));
#210908=CARTESIAN_POINT('Ctrl Pts',(21.4361288448778,18.2937586707072,19.1596837001081));
#210909=CARTESIAN_POINT('Ctrl Pts',(19.4253562883709,16.4424519246523,19.2868595067896));
#210910=CARTESIAN_POINT('Ctrl Pts',(16.780307255024,17.1311162137809,19.414035313471));
#210911=CARTESIAN_POINT('Ctrl Pts',(15.9276500412235,19.7279447624144,19.5412111201524));
#210912=CARTESIAN_POINT('Ctrl Pts',(17.6496447600855,21.8505086195232,19.6683869268339));
#210913=CARTESIAN_POINT('Ctrl Pts',(20.3664680564733,21.5514870621786,19.7955627335153));
#210914=CARTESIAN_POINT('Ctrl Pts',(21.5856033344346,19.1052140510933,19.9227385401968));
#210915=CARTESIAN_POINT('Ctrl Pts',(20.1885693489379,16.7559927763657,20.0499143468782));
#210916=CARTESIAN_POINT('Ctrl Pts',(17.457058641429,16.6590888438425,20.1770901535596));
#210917=CARTESIAN_POINT('Ctrl Pts',(15.8970616522235,18.9034038719576,20.3042659602411));
#210918=CARTESIAN_POINT('Ctrl Pts',(16.9397809084021,21.4299214440102,20.4314417669225));
#210919=CARTESIAN_POINT('Ctrl Pts',(19.6285821382997,21.9207120974271,20.5586175736039));
#210920=CARTESIAN_POINT('Ctrl Pts',(21.4966649457231,19.9255182070319,20.6857933802854));
#210921=CARTESIAN_POINT('Ctrl Pts',(20.8301641839021,17.2747825617085,20.8129691869668));
#210922=CARTESIAN_POINT('Ctrl Pts',(18.240582059696,16.40043638892,20.9401449936482));
#210923=CARTESIAN_POINT('Ctrl Pts',(16.1036433297677,18.104549801285,21.0673208003297));
#210924=CARTESIAN_POINT('Ctrl Pts',(16.3799647587305,20.8238745060694,21.1944966070111));
#210925=CARTESIAN_POINT('Ctrl Pts',(18.8158302886401,22.0632713447716,21.3216724136925));
#210926=CARTESIAN_POINT('Ctrl Pts',(21.176885810551,20.6863017024412,21.4488482203739));
#210927=CARTESIAN_POINT('Ctrl Pts',(21.2962360890773,17.9550335586219,21.5760240270554));
#210928=CARTESIAN_POINT('Ctrl Pts',(19.06587574408,16.377582661504,21.7031998337368));
#210929=CARTESIAN_POINT('Ctrl Pts',(16.529138326029,17.396607333106,21.8303756404183));
#210930=CARTESIAN_POINT('Ctrl Pts',(16.0189811762652,20.0863088421845,21.9575514470997));
#210931=CARTESIAN_POINT('Ctrl Pts',(17.3340241117299,21.3345380991533,22.0423353182207));
#210932=CARTESIAN_POINT('Ctrl Pts',(18.1101967966574,21.5422305581871,22.0847272537811));
#210933=CARTESIAN_POINT('Ctrl Pts',(20.6946895702226,20.8620838326754,-0.257713273515286));
#210934=CARTESIAN_POINT('Ctrl Pts',(21.2446793034262,20.2090078950206,-0.21530268190311));
#210935=CARTESIAN_POINT('Ctrl Pts',(21.6307189736713,18.3216248822974,-0.130500154730457));
#210936=CARTESIAN_POINT('Ctrl Pts',(19.54985825025,16.2898541338203,-0.00330569199732536));
#210937=CARTESIAN_POINT('Ctrl Pts',(16.7212342529824,16.9459341572626,0.123870114684109));
#210938=CARTESIAN_POINT('Ctrl Pts',(15.7390230172331,19.6762947228445,0.251045921365543));
#210939=CARTESIAN_POINT('Ctrl Pts',(17.5046028706573,21.9817197183951,0.378221728046977));
#210940=CARTESIAN_POINT('Ctrl Pts',(20.3980344048781,21.7441743961897,0.505397534728411));
#210941=CARTESIAN_POINT('Ctrl Pts',(21.7648403718746,19.1831212459942,0.632573341409846));
#210942=CARTESIAN_POINT('Ctrl Pts',(20.3510266276838,16.6473739692942,0.75974914809128));
#210943=CARTESIAN_POINT('Ctrl Pts',(17.4536974328697,16.4637351954612,0.886924954772715));
#210944=CARTESIAN_POINT('Ctrl Pts',(15.7309632043494,18.8004683182191,1.01410076145415));
#210945=CARTESIAN_POINT('Ctrl Pts',(16.7633304940341,21.5138766926494,1.14127656813558));
#210946=CARTESIAN_POINT('Ctrl Pts',(19.6036638866926,22.1145189554039,1.26845237481702));
#210947=CARTESIAN_POINT('Ctrl Pts',(21.6461350846223,20.0513730033173,1.39562818149845));
#210948=CARTESIAN_POINT('Ctrl Pts',(21.016902859507,17.2172316786593,1.52280398817988));
#210949=CARTESIAN_POINT('Ctrl Pts',(18.2932490733073,16.2122517932659,1.64997979486132));
#210950=CARTESIAN_POINT('Ctrl Pts',(15.9739568441929,17.9584358360373,1.77715560154276));
#210951=CARTESIAN_POINT('Ctrl Pts',(16.1868329351487,20.853770497638,1.90433140822419));
#210952=CARTESIAN_POINT('Ctrl Pts',(18.7365766963666,22.2419648047335,2.03150721490562));
#210953=CARTESIAN_POINT('Ctrl Pts',(21.2839565072747,20.8494372260819,2.15868302158706));
#210954=CARTESIAN_POINT('Ctrl Pts',(21.4919094864037,17.9537450817297,2.28585882826849));
#210955=CARTESIAN_POINT('Ctrl Pts',(19.169651689263,16.2115063446496,2.41303463494992));
#210956=CARTESIAN_POINT('Ctrl Pts',(16.4477105056032,17.2211168388571,2.54021044163136));
#210957=CARTESIAN_POINT('Ctrl Pts',(15.8232980305525,20.0563216418289,2.66738624831279));
#210958=CARTESIAN_POINT('Ctrl Pts',(17.8692739536042,22.1159962974782,2.79456205499423));
#210959=CARTESIAN_POINT('Ctrl Pts',(20.7085823534422,21.5105171585006,2.92173786167567));
#210960=CARTESIAN_POINT('Ctrl Pts',(21.7363340003116,18.7953737487032,3.04891366835709));
#210961=CARTESIAN_POINT('Ctrl Pts',(20.0096305478046,16.4615416288479,3.17608947503854));
#210962=CARTESIAN_POINT('Ctrl Pts',(17.1126152422242,16.6501669133465,3.30326528171996));
#210963=CARTESIAN_POINT('Ctrl Pts',(15.7031198174278,19.1881976119062,3.4304410884014));
#210964=CARTESIAN_POINT('Ctrl Pts',(17.0742688424951,21.7471480861189,3.55761689508284));
#210965=CARTESIAN_POINT('Ctrl Pts',(19.9681181900429,21.9793401024969,3.68479270176427));
#210966=CARTESIAN_POINT('Ctrl Pts',(21.7297406962381,19.671751897359,3.8119685084457));
#210967=CARTESIAN_POINT('Ctrl Pts',(20.742957050273,16.9414524239027,3.93914431512714));
#210968=CARTESIAN_POINT('Ctrl Pts',(17.9130800006189,16.2933219874959,4.06632012180857));
#210969=CARTESIAN_POINT('Ctrl Pts',(15.8363460983557,18.3219800360464,4.19349592849001));
#210970=CARTESIAN_POINT('Ctrl Pts',(16.4180298021666,21.1662587227194,4.32067173517144));
#210971=CARTESIAN_POINT('Ctrl Pts',(19.1244724171678,22.2167088883417,4.44784754185288));
#210972=CARTESIAN_POINT('Ctrl Pts',(21.4726808248689,20.5096077042429,4.57502334853431));
#210973=CARTESIAN_POINT('Ctrl Pts',(21.3083195574551,17.6111145521858,4.70219915521574));
#210974=CARTESIAN_POINT('Ctrl Pts',(18.7821798763678,16.1804169984081,4.82937496189718));
#210975=CARTESIAN_POINT('Ctrl Pts',(16.2118381490933,17.5300912493964,4.95655076857861));
#210976=CARTESIAN_POINT('Ctrl Pts',(15.9554233770066,20.4218949501003,5.08372657526004));
#210977=CARTESIAN_POINT('Ctrl Pts',(18.2481801986013,22.2027776907038,5.21090238194148));
#210978=CARTESIAN_POINT('Ctrl Pts',(20.9866465346018,21.238890090752,5.33807818862291));
#210979=CARTESIAN_POINT('Ctrl Pts',(21.6584494901173,18.4145391975892,5.46525399530435));
#210980=CARTESIAN_POINT('Ctrl Pts',(19.6472515502562,16.3208916567058,5.59242980198579));
#210981=CARTESIAN_POINT('Ctrl Pts',(16.7982019958189,16.8787391404406,5.71960560866721));
#210982=CARTESIAN_POINT('Ctrl Pts',(15.7251269610433,19.5762912063867,5.84678141534867));
#210983=CARTESIAN_POINT('Ctrl Pts',(17.4125061877879,21.9387112630022,5.97395722203007));
#210984=CARTESIAN_POINT('Ctrl Pts',(20.3122739660809,21.7986255366678,6.10113302871153));
#210985=CARTESIAN_POINT('Ctrl Pts',(21.7640733392246,19.2845539865944,6.22830883539295));
#210986=CARTESIAN_POINT('Ctrl Pts',(20.4359684911912,16.703001219096,6.35548464207439));
#210987=CARTESIAN_POINT('Ctrl Pts',(17.5464131885678,16.422381669117,6.48266044875582));
#210988=CARTESIAN_POINT('Ctrl Pts',(15.7463950754831,18.7001463565497,6.60983625543726));
#210989=CARTESIAN_POINT('Ctrl Pts',(16.6873190489681,21.4465875546951,6.7370120621187));
#210990=CARTESIAN_POINT('Ctrl Pts',(19.5059457636785,22.1420159276201,6.86418786880012));
#210991=CARTESIAN_POINT('Ctrl Pts',(21.6163601525715,20.1484191063189,6.99136367548156));
#210992=CARTESIAN_POINT('Ctrl Pts',(21.0823880009273,17.2947984377616,7.118539482163));
#210993=CARTESIAN_POINT('Ctrl Pts',(18.3939156158299,16.1991737696759,7.24571528884443));
#210994=CARTESIAN_POINT('Ctrl Pts',(16.0174495451912,17.8667127328943,7.37289109552587));
#210995=CARTESIAN_POINT('Ctrl Pts',(16.1332499087027,20.7675518278046,7.50006690220729));
#210996=CARTESIAN_POINT('Ctrl Pts',(18.6350770602241,22.2403512312061,7.62724270888874));
#210997=CARTESIAN_POINT('Ctrl Pts',(21.2276598691396,20.9339089027185,7.75441851557016));
#210998=CARTESIAN_POINT('Ctrl Pts',(21.5324645221063,18.0468045917732,7.8815943222516));
#210999=CARTESIAN_POINT('Ctrl Pts',(19.2698516683375,16.2277773097598,8.00877012893304));
#211000=CARTESIAN_POINT('Ctrl Pts',(16.5156281675744,17.1456716863595,8.13594593561446));
#211001=CARTESIAN_POINT('Ctrl Pts',(15.7966231353776,19.9583766019922,8.26312174229592));
#211002=CARTESIAN_POINT('Ctrl Pts',(17.7724790623024,22.0854098727205,8.39029754897732));
#211003=CARTESIAN_POINT('Ctrl Pts',(20.6304707708447,21.5753504912249,8.51747335565878));
#211004=CARTESIAN_POINT('Ctrl Pts',(21.7485682553881,18.8961462821721,8.64464916234021));
#211005=CARTESIAN_POINT('Ctrl Pts',(20.1009864708203,16.5058008172007,8.77182496902164));
#211006=CARTESIAN_POINT('Ctrl Pts',(17.199279444024,16.5973076988504,8.89900077570308));
#211007=CARTESIAN_POINT('Ctrl Pts',(15.705583271835,19.0867150427652,9.0261765823845));
#211008=CARTESIAN_POINT('Ctrl Pts',(16.9902714829968,21.6901461209486,9.15335238906595));
#211009=CARTESIAN_POINT('Ctrl Pts',(19.8747223805114,22.0191145063235,9.28052819574737));
#211010=CARTESIAN_POINT('Ctrl Pts',(21.7126312951226,19.7718121233893,9.40770400242882));
#211011=CARTESIAN_POINT('Ctrl Pts',(20.8178308711669,17.0099994251714,9.53487980911025));
#211012=CARTESIAN_POINT('Ctrl Pts',(18.011244960046,16.2674681448564,9.66205561579168));
#211013=CARTESIAN_POINT('Ctrl Pts',(15.8677419388458,18.2254446454444,9.78923142247312));
#211014=CARTESIAN_POINT('Ctrl Pts',(16.353852788716,21.0876070133732,9.91640722915455));
#211015=CARTESIAN_POINT('Ctrl Pts',(19.0236009763425,22.2280989218993,10.043583035836));
#211016=CARTESIAN_POINT('Ctrl Pts',(21.4276582428386,20.6005898318611,10.1707588425174));
#211017=CARTESIAN_POINT('Ctrl Pts',(21.3604512588158,17.6982183187623,10.2979346491988));
#211018=CARTESIAN_POINT('Ctrl Pts',(18.8836382607796,16.1837301043787,10.4251104558803));
#211019=CARTESIAN_POINT('Ctrl Pts',(16.2695414460758,17.4465741256675,10.5522862625617));
#211020=CARTESIAN_POINT('Ctrl Pts',(15.9164323930488,20.3281693740358,10.6794620692432));
#211021=CARTESIAN_POINT('Ctrl Pts',(18.1482667414313,22.1848310610778,10.8066378759246));
#211022=CARTESIAN_POINT('Ctrl Pts',(20.9174749998444,21.3131873263528,10.933813682606));
#211023=CARTESIAN_POINT('Ctrl Pts',(21.6834804676428,18.5129171961597,11.0609894892874));
#211024=CARTESIAN_POINT('Ctrl Pts',(19.7435206717827,16.3530947105848,11.1881652959689));
#211025=CARTESIAN_POINT('Ctrl Pts',(16.8773883174812,16.8152229464412,11.3153411026503));
#211026=CARTESIAN_POINT('Ctrl Pts',(15.7145819475737,19.4753279302436,11.4425169093318));
#211027=CARTESIAN_POINT('Ctrl Pts',(17.3219042345475,21.8929284440893,11.5696927160132));
#211028=CARTESIAN_POINT('Ctrl Pts',(20.2247367417761,21.8500260697353,11.6968685226946));
#211029=CARTESIAN_POINT('Ctrl Pts',(21.7599108139823,19.3859810728298,11.824044329376));
#211030=CARTESIAN_POINT('Ctrl Pts',(20.5189995235657,16.7614018021532,11.9512201360575));
#211031=CARTESIAN_POINT('Ctrl Pts',(17.6404619598426,16.38417683879,12.0783959427389));
#211032=CARTESIAN_POINT('Ctrl Pts',(15.7651776753385,18.6003866734043,12.2055717494204));
#211033=CARTESIAN_POINT('Ctrl Pts',(16.6136036078165,21.3767963362328,12.3327475561018));
#211034=CARTESIAN_POINT('Ctrl Pts',(19.4073616234801,22.1662222850487,12.4599233627832));
#211035=CARTESIAN_POINT('Ctrl Pts',(21.5833521431366,20.2444152091134,12.5870991694647));
#211036=CARTESIAN_POINT('Ctrl Pts',(21.1452389222041,17.3745138197983,12.7142749761461));
#211037=CARTESIAN_POINT('Ctrl Pts',(18.4949636485153,16.1894745156307,12.8414507828275));
#211038=CARTESIAN_POINT('Ctrl Pts',(16.0639893910444,17.7764973063501,12.968626589509));
#211039=CARTESIAN_POINT('Ctrl Pts',(16.0825841477421,20.6795872832148,13.0958023961904));
#211040=CARTESIAN_POINT('Ctrl Pts',(18.5336883834592,22.2353395785366,13.2229782028718));
#211041=CARTESIAN_POINT('Ctrl Pts',(21.1685660946113,21.0164480222352,13.3501540095533));
#211042=CARTESIAN_POINT('Ctrl Pts',(21.5698805201709,18.1411699642751,13.4773298162347));
#211043=CARTESIAN_POINT('Ctrl Pts',(19.3694505830695,16.247394562952,13.6045056229161));
#211044=CARTESIAN_POINT('Ctrl Pts',(16.5860341765131,17.072543208022,13.7316814295976));
#211045=CARTESIAN_POINT('Ctrl Pts',(15.7732430952114,19.8595932321345,13.858857236279));
#211046=CARTESIAN_POINT('Ctrl Pts',(17.6767627087548,22.0515992219996,13.9860330429604));
#211047=CARTESIAN_POINT('Ctrl Pts',(20.5502319174689,21.6375317331515,14.1132088496419));
#211048=CARTESIAN_POINT('Ctrl Pts',(21.7574210699713,18.9972719866817,14.2403846563233));
#211049=CARTESIAN_POINT('Ctrl Pts',(20.1908090454502,16.5530944269748,14.3675604630048));
#211050=CARTESIAN_POINT('Ctrl Pts',(17.2876651414952,16.5473802622938,14.4947362696862));
#211051=CARTESIAN_POINT('Ctrl Pts',(15.7114437005529,18.9853718840723,14.6219120763676));
#211052=CARTESIAN_POINT('Ctrl Pts',(16.9082300633519,21.6303632981543,14.749087883049));
#211053=CARTESIAN_POINT('Ctrl Pts',(19.7800470229629,22.0557390488012,14.8762636897305));
#211054=CARTESIAN_POINT('Ctrl Pts',(21.692180764006,19.8712432865912,15.0034394964119));
#211055=CARTESIAN_POINT('Ctrl Pts',(20.8903672594785,17.0810152882537,15.1306153030934));
#211056=CARTESIAN_POINT('Ctrl Pts',(18.1102206336258,16.2449160611827,15.2577911097748));
#211057=CARTESIAN_POINT('Ctrl Pts',(15.9023528603076,18.1300147520451,15.3849669164562));
#211058=CARTESIAN_POINT('Ctrl Pts',(16.2923455858144,21.0068503143949,15.5121427231376));
#211059=CARTESIAN_POINT('Ctrl Pts',(18.9224046901724,22.2361046763285,15.6393185298191));
#211060=CARTESIAN_POINT('Ctrl Pts',(21.379614185011,20.6900132569022,15.7664943365005));
#211061=CARTESIAN_POINT('Ctrl Pts',(21.4096368704371,17.7870189721836,15.8936701431819));
#211062=CARTESIAN_POINT('Ctrl Pts',(18.9849287959905,16.1904388982563,16.0208459498634));
#211063=CARTESIAN_POINT('Ctrl Pts',(16.33000912562,17.3650361580133,16.1480217565448));
#211064=CARTESIAN_POINT('Ctrl Pts',(15.8806018739919,20.2331906693557,16.2751975632263));
#211065=CARTESIAN_POINT('Ctrl Pts',(18.0490103011151,22.1635486858722,16.4023733699077));
#211066=CARTESIAN_POINT('Ctrl Pts',(20.8458542617096,21.3851265389399,16.5295491765891));
#211067=CARTESIAN_POINT('Ctrl Pts',(21.7052030136437,18.6120782340418,16.6567249832706));
#211068=CARTESIAN_POINT('Ctrl Pts',(19.8386574142166,16.3885034761332,16.783900789952));
#211069=CARTESIAN_POINT('Ctrl Pts',(16.9586572000173,16.754394094981,16.9110765966334));
#211070=CARTESIAN_POINT('Ctrl Pts',(15.7074238146008,19.3740681575255,17.0382524033149));
#211071=CARTESIAN_POINT('Ctrl Pts',(17.2328862287842,21.8441373066915,17.1654282099963));
#211072=CARTESIAN_POINT('Ctrl Pts',(20.1355273584301,21.8984664079011,17.2926040166777));
#211073=CARTESIAN_POINT('Ctrl Pts',(21.7523541253142,19.487211882838,17.4197798233592));
#211074=CARTESIAN_POINT('Ctrl Pts',(20.6000283224083,16.8225500989152,17.5469556300406));
#211075=CARTESIAN_POINT('Ctrl Pts',(17.7357373524709,16.3491428553155,17.674131436722));
#211076=CARTESIAN_POINT('Ctrl Pts',(15.7872904024767,18.5013119150815,17.8013072434035));
#211077=CARTESIAN_POINT('Ctrl Pts',(16.5422666147802,21.304575744541,17.9284830500849));
#211078=CARTESIAN_POINT('Ctrl Pts',(19.3080221737182,22.1871137703668,18.0556588567663));
#211079=CARTESIAN_POINT('Ctrl Pts',(21.5471480160826,20.3392521303006,18.1828346634478));
#211080=CARTESIAN_POINT('Ctrl Pts',(21.2053851573897,17.4562891879729,18.3100104701292));
#211081=CARTESIAN_POINT('Ctrl Pts',(18.5962798081749,16.1831645059201,18.4371862768106));
#211082=CARTESIAN_POINT('Ctrl Pts',(16.1135241872327,17.6878909612598,18.5643620834921));
#211083=CARTESIAN_POINT('Ctrl Pts',(16.0348924791393,20.5899754243741,18.6915378901735));
#211084=CARTESIAN_POINT('Ctrl Pts',(18.4325243964945,22.226935525381,18.8187136968549));
#211085=CARTESIAN_POINT('Ctrl Pts',(21.1067414672911,21.0969619702091,18.9458895035364));
#211086=CARTESIAN_POINT('Ctrl Pts',(21.6041155128897,18.2367353666694,19.0730653102178));
#211087=CARTESIAN_POINT('Ctrl Pts',(19.4683367108302,16.270336088174,19.2002411168992));
#211088=CARTESIAN_POINT('Ctrl Pts',(16.6588495624458,17.0018134428338,19.3274169235807));
#211089=CARTESIAN_POINT('Ctrl Pts',(15.7531841271558,19.760082322527,19.4545927302621));
#211090=CARTESIAN_POINT('Ctrl Pts',(17.5822322738009,22.0146022966338,19.5817685369435));
#211091=CARTESIAN_POINT('Ctrl Pts',(20.4679557667883,21.6969910872163,19.708944343625));
#211092=CARTESIAN_POINT('Ctrl Pts',(21.7628825724515,19.0986375219567,19.8361201503064));
#211093=CARTESIAN_POINT('Ctrl Pts',(20.2789974048699,16.6033692313319,19.9632959569879));
#211094=CARTESIAN_POINT('Ctrl Pts',(17.3776734098626,16.5004409492398,20.0904717636693));
#211095=CARTESIAN_POINT('Ctrl Pts',(15.7206941110155,18.8842811536826,20.2176475703507));
#211096=CARTESIAN_POINT('Ctrl Pts',(16.8282374165171,21.5678679452165,20.3448233770321));
#211097=CARTESIAN_POINT('Ctrl Pts',(19.6841967596975,22.0891702031096,20.4719991837136));
#211098=CARTESIAN_POINT('Ctrl Pts',(21.668415038227,19.9699385658392,20.5991749903951));
#211099=CARTESIAN_POINT('Ctrl Pts',(20.9604790789623,17.1544112786656,20.7263507970764));
#211100=CARTESIAN_POINT('Ctrl Pts',(18.2099071213465,16.2257085193901,20.8535266037579));
#211101=CARTESIAN_POINT('Ctrl Pts',(15.9401186134861,18.0357637096982,20.9807024104393));
#211102=CARTESIAN_POINT('Ctrl Pts',(16.233618466875,20.9241441193076,21.1078782171208));
#211103=CARTESIAN_POINT('Ctrl Pts',(18.8209175358886,22.2405921118336,21.2350540238022));
#211104=CARTESIAN_POINT('Ctrl Pts',(21.3287557883375,20.7780186528654,21.3622298304836));
#211105=CARTESIAN_POINT('Ctrl Pts',(21.4555258668686,17.8769523013118,21.4894056371651));
#211106=CARTESIAN_POINT('Ctrl Pts',(19.0865078840121,16.2014340153418,21.6165814438465));
#211107=CARTESIAN_POINT('Ctrl Pts',(16.3920658963632,17.2838096850018,21.7437572505279));
#211108=CARTESIAN_POINT('Ctrl Pts',(15.8501931606037,20.1407252761597,21.8709330572094));
#211109=CARTESIAN_POINT('Ctrl Pts',(17.2469900366476,21.4665547830909,21.9557169283303));
#211110=CARTESIAN_POINT('Ctrl Pts',(18.0714160324376,21.6871591224115,21.9981088638908));
#211111=CARTESIAN_POINT('Ctrl Pts',(20.3539256943887,20.5739122292573,2.60208521396521E-18));
#211112=CARTESIAN_POINT('Ctrl Pts',(20.4076089227952,20.5221116197655,-8.76976867613359E-16));
#211113=CARTESIAN_POINT('Ctrl Pts',(20.4581355934374,20.4674384227593,-2.52590746105995E-14));
#211114=CARTESIAN_POINT('Ctrl Pts',(20.505511973405,20.410263943529,-1.70176372993325E-15));
#211115=CARTESIAN_POINT('Ctrl Pts',(20.5545756561021,20.3510532037207,2.26945372756332E-14));
#211116=CARTESIAN_POINT('Ctrl Pts',(20.6002611628448,20.2891594084515,2.60865837895201E-14));
#211117=CARTESIAN_POINT('Ctrl Pts',(20.642547115175,20.2249453565119,1.84262327618256E-14));
#211118=CARTESIAN_POINT('Ctrl Pts',(20.6826816163244,20.163998427346,1.11556298740125E-14));
#211119=CARTESIAN_POINT('Ctrl Pts',(20.719753745937,20.1009604021271,-8.83402169628207E-15));
#211120=CARTESIAN_POINT('Ctrl Pts',(20.753716758437,20.0361087206568,9.29811783123569E-15));
#211121=CARTESIAN_POINT('Ctrl Pts',(20.7688150794711,20.0072787837823,1.71471824035106E-14));
#211122=CARTESIAN_POINT('Ctrl Pts',(20.7832985639006,19.9780900549027,2.84583620301588E-14));
#211123=CARTESIAN_POINT('Ctrl Pts',(20.7971611119739,19.9485653699547,5.09314812546791E-15));
#211124=CARTESIAN_POINT('Ctrl Pts',(20.8039895160331,19.9340221216659,-6.39236290215152E-15));
#211125=CARTESIAN_POINT('Ctrl Pts',(20.8106672398928,19.9193973462958,1.44353959261987E-14));
#211126=CARTESIAN_POINT('Ctrl Pts',(20.8171934366481,19.9046937060787,1.06720188242093E-14));
#211127=CARTESIAN_POINT('Ctrl Pts',(20.8232055554644,19.8911482928261,7.48952413932212E-15));
#211128=CARTESIAN_POINT('Ctrl Pts',(20.8290895460591,19.8775345581707,1.69617332493456E-15));
#211129=CARTESIAN_POINT('Ctrl Pts',(20.8348368052234,19.8638741231809,4.37844205336546E-15));
#211130=CARTESIAN_POINT('Ctrl Pts',(20.8659056669685,19.7900277637342,1.88375660372629E-14));
#211131=CARTESIAN_POINT('Ctrl Pts',(20.8930393190126,19.7146930410775,3.61062706447889E-14));
#211132=CARTESIAN_POINT('Ctrl Pts',(20.9162161295942,19.6382510927703,1.90264470845136E-14));
#211133=CARTESIAN_POINT('Ctrl Pts',(20.9398193031497,19.5604029105767,1.63242134604958E-15));
#211134=CARTESIAN_POINT('Ctrl Pts',(20.959319229244,19.4814055816633,1.27489672905939E-14));
#211135=CARTESIAN_POINT('Ctrl Pts',(20.9746521650443,19.4016261052126,4.85722573273506E-16));
#211136=CARTESIAN_POINT('Ctrl Pts',(20.9885844253233,19.32913454552,-1.06572652727376E-14));
#211137=CARTESIAN_POINT('Ctrl Pts',(20.9990759703875,19.2559962568405,3.89867626280975E-15));
#211138=CARTESIAN_POINT('Ctrl Pts',(21.0060451898833,19.1824707413237,1.37806432931598E-14));
#211139=CARTESIAN_POINT('Ctrl Pts',(21.0087031237876,19.1544294433498,1.74701789075424E-14));
#211140=CARTESIAN_POINT('Ctrl Pts',(21.0108483731097,19.1263317159654,-5.7355876066468E-15));
#211141=CARTESIAN_POINT('Ctrl Pts',(21.0124750503239,19.0981916687962,1.26704202685346E-14));
#211142=CARTESIAN_POINT('Ctrl Pts',(21.0133685656744,19.0827346599387,2.28408658292894E-14));
#211143=CARTESIAN_POINT('Ctrl Pts',(21.0141056048104,19.0672648807305,-1.46450263791898E-15));
#211144=CARTESIAN_POINT('Ctrl Pts',(21.0146850898148,19.0517846622215,5.06539254985228E-15));
#211145=CARTESIAN_POINT('Ctrl Pts',(21.0151328036157,19.0398245469222,1.02796891611799E-14));
#211146=CARTESIAN_POINT('Ctrl Pts',(21.0154863000461,19.0278615000918,2.25762263693188E-14));
#211147=CARTESIAN_POINT('Ctrl Pts',(21.015745158205,19.0159051388708,1.90403248723214E-14));
#211148=CARTESIAN_POINT('Ctrl Pts',(21.017551908051,18.9324534374073,-5.41087435524647E-15));
#211149=CARTESIAN_POINT('Ctrl Pts',(21.014756822678,18.8492079748143,-1.7965889298872E-14));
#211150=CARTESIAN_POINT('Ctrl Pts',(21.0073036571099,18.7665493842094,-9.43689570931383E-16));
#211151=CARTESIAN_POINT('Ctrl Pts',(20.9998648139147,18.6840496344554,1.63477607125224E-14));
#211152=CARTESIAN_POINT('Ctrl Pts',(20.9877861501509,18.60213349936,6.07683838498736E-15));
#211153=CARTESIAN_POINT('Ctrl Pts',(20.9709623839625,18.5211637972932,9.07607322631065E-15));
#211154=CARTESIAN_POINT('Ctrl Pts',(20.9545246627898,18.4420520591064,1.2427326863693E-14));
#211155=CARTESIAN_POINT('Ctrl Pts',(20.9335573250132,18.3638428657348,-1.29184203455733E-14));
#211156=CARTESIAN_POINT('Ctrl Pts',(20.9083260331535,18.2867626991381,-6.38378239159465E-16));
#211157=CARTESIAN_POINT('Ctrl Pts',(20.8979286030734,18.2549991395388,4.51921879028503E-15));
#211158=CARTESIAN_POINT('Ctrl Pts',(20.886806477603,18.223427374722,1.48021303909579E-14));
#211159=CARTESIAN_POINT('Ctrl Pts',(20.8749757625748,18.1920637286001,7.49400541621981E-15));
#211160=CARTESIAN_POINT('Ctrl Pts',(20.868424493201,18.1746960805925,3.22326148169017E-15));
#211161=CARTESIAN_POINT('Ctrl Pts',(20.8616536960862,18.1573871105346,8.68449611504115E-15));
#211162=CARTESIAN_POINT('Ctrl Pts',(20.8546784987878,18.1401696684741,5.24580379135386E-15));
#211163=CARTESIAN_POINT('Ctrl Pts',(20.8237193197693,18.06375062996,-9.59599133981877E-15));
#211164=CARTESIAN_POINT('Ctrl Pts',(20.7887042347096,17.9890383341861,1.00214989038782E-14));
#211165=CARTESIAN_POINT('Ctrl Pts',(20.7499612622237,17.916256394916,1.44606548957427E-14));
#211166=CARTESIAN_POINT('Ctrl Pts',(20.7091543143746,17.8395971039635,1.91363004497942E-14));
#211167=CARTESIAN_POINT('Ctrl Pts',(20.6642116622635,17.7650784733303,-4.62531541653634E-15));
#211168=CARTESIAN_POINT('Ctrl Pts',(20.6154560962815,17.692967425201,1.04916075827077E-14));
#211169=CARTESIAN_POINT('Ctrl Pts',(20.5667005302995,17.6208563770717,2.56085305819518E-14));
#211170=CARTESIAN_POINT('Ctrl Pts',(20.5141314518022,17.55115202568,2.07608830934162E-14));
#211171=CARTESIAN_POINT('Ctrl Pts',(20.4580183994378,17.484139989662,2.21211937656562E-14));
#211172=CARTESIAN_POINT('Ctrl Pts',(20.4361046684505,17.457969897886,2.30143573901407E-14));
#211173=CARTESIAN_POINT('Ctrl Pts',(20.4136499126721,17.4322106904206,1.67053283342637E-15));
#211174=CARTESIAN_POINT('Ctrl Pts',(20.3906682863214,17.4068806089605,9.04831765069503E-15));
#211175=CARTESIAN_POINT('Ctrl Pts',(20.3815365196799,17.3968156819022,1.20932955461059E-14));
#211176=CARTESIAN_POINT('Ctrl Pts',(20.3723208008609,17.3868177123508,-1.58786556649917E-14));
#211177=CARTESIAN_POINT('Ctrl Pts',(20.3630243250802,17.3768903879953,-1.62370117351429E-14));
#211178=CARTESIAN_POINT('Ctrl Pts',(20.3025146980146,17.3122746444938,-1.87508807042265E-14));
#211179=CARTESIAN_POINT('Ctrl Pts',(20.2387852814275,17.2508599884964,-1.29144917290363E-14));
#211180=CARTESIAN_POINT('Ctrl Pts',(20.1721441631346,17.1929207844063,-2.06501482580279E-14));
#211181=CARTESIAN_POINT('Ctrl Pts',(20.116951256814,17.1449348990317,-2.70569039828667E-14));
#211182=CARTESIAN_POINT('Ctrl Pts',(20.0597599943144,17.0993329745171,2.10331963193576E-15));
#211183=CARTESIAN_POINT('Ctrl Pts',(20.0007222400369,17.0562848434724,1.38777878078145E-15));
#211184=CARTESIAN_POINT('Ctrl Pts',(19.9812253415778,17.0420684314475,1.43084424546213E-15));
#211185=CARTESIAN_POINT('Ctrl Pts',(19.9615269094649,17.0281306668005,8.22589116977551E-16));
#211186=CARTESIAN_POINT('Ctrl Pts',(19.9416319850871,17.0144780743264,5.05151476204446E-15));
#211187=CARTESIAN_POINT('Ctrl Pts',(19.9257068710494,17.0035497044602,8.2357117562639E-15));
#211188=CARTESIAN_POINT('Ctrl Pts',(19.9096544915251,16.9928033016912,1.13873654213532E-14));
#211189=CARTESIAN_POINT('Ctrl Pts',(19.8934933769624,16.9822523936718,9.85322934354826E-15));
#211190=CARTESIAN_POINT('Ctrl Pts',(19.8189655612139,16.9335963355889,2.49494022146064E-15));
#211191=CARTESIAN_POINT('Ctrl Pts',(19.7420556121672,16.8890439678595,-1.1204578293946E-14));
#211192=CARTESIAN_POINT('Ctrl Pts',(19.6630443965311,16.8488858958507,-3.58046925441613E-15));
#211193=CARTESIAN_POINT('Ctrl Pts',(19.5852031544112,16.8093224720868,4.67551488835544E-15));
#211194=CARTESIAN_POINT('Ctrl Pts',(19.5053217346575,16.774023445591,-1.3425717557294E-14));
#211195=CARTESIAN_POINT('Ctrl Pts',(19.423636270734,16.7433040636654,1.66533453693773E-16));
#211196=CARTESIAN_POINT('Ctrl Pts',(19.4149415054419,16.7400342307853,1.73416518801677E-15));
#211197=CARTESIAN_POINT('Ctrl Pts',(19.4062262753773,16.736816326208,1.52237426317155E-14));
#211198=CARTESIAN_POINT('Ctrl Pts',(19.3974909960169,16.7336502196964,1.0547118733939E-15));
#211199=CARTESIAN_POINT('Ctrl Pts',(18.071416109725,16.7348411664207,0.0018909634849847));
#211200=CARTESIAN_POINT('Ctrl Pts',(17.2469902101003,16.9554454800088,0.0442828990454628));
#211201=CARTESIAN_POINT('Ctrl Pts',(15.8501940740727,18.2812783317349,0.129066770166419));
#211202=CARTESIAN_POINT('Ctrl Pts',(16.3920656588252,21.1381881653492,0.256242576847853));
#211203=CARTESIAN_POINT('Ctrl Pts',(19.0865079389648,22.2205670934987,0.383418383529288));
#211204=CARTESIAN_POINT('Ctrl Pts',(21.4555257828913,20.5450469055032,0.510594190210721));
#211205=CARTESIAN_POINT('Ctrl Pts',(21.3287556324384,17.643981848867,0.637769996892157));
#211206=CARTESIAN_POINT('Ctrl Pts',(18.8209175760198,16.1814077573175,0.76494580357359));
#211207=CARTESIAN_POINT('Ctrl Pts',(16.233618537572,17.4978560985894,0.892121610255025));
#211208=CARTESIAN_POINT('Ctrl Pts',(15.9401187499945,20.386236157729,1.01929741693646));
#211209=CARTESIAN_POINT('Ctrl Pts',(18.2099071291442,22.1962914055474,1.1464732236179));
#211210=CARTESIAN_POINT('Ctrl Pts',(20.9604789958506,21.2675886098998,1.27364903029933));
#211211=CARTESIAN_POINT('Ctrl Pts',(21.6684149124547,18.4520614803885,1.40082483698077));
#211212=CARTESIAN_POINT('Ctrl Pts',(19.6841967236086,16.3328299069189,1.5280006436622));
#211213=CARTESIAN_POINT('Ctrl Pts',(16.8282374931634,16.8541321563464,1.65517645034364));
#211214=CARTESIAN_POINT('Ctrl Pts',(15.7206942359514,19.5377188303282,1.78235225702507));
#211215=CARTESIAN_POINT('Ctrl Pts',(17.3776734650805,21.9215589406766,1.90952806370651));
#211216=CARTESIAN_POINT('Ctrl Pts',(20.2789973416443,21.8186306606476,2.03670387038793));
#211217=CARTESIAN_POINT('Ctrl Pts',(21.7628824476932,19.3233624738419,2.16387967706937));
#211218=CARTESIAN_POINT('Ctrl Pts',(20.4679556955709,16.7250090148042,2.2910554837508));
#211219=CARTESIAN_POINT('Ctrl Pts',(17.5822323211178,16.4073978188031,2.41823129043224));
#211220=CARTESIAN_POINT('Ctrl Pts',(15.7531842497881,18.6619176999891,2.54540709711367));
#211221=CARTESIAN_POINT('Ctrl Pts',(16.65884964778,21.4201864663384,2.67258290379511));
#211222=CARTESIAN_POINT('Ctrl Pts',(19.468336680636,22.1516637908563,2.79975871047654));
#211223=CARTESIAN_POINT('Ctrl Pts',(21.6041153948362,20.1852645932698,2.92693451715798));
#211224=CARTESIAN_POINT('Ctrl Pts',(21.1067413697027,17.3250381073553,3.05411032383941));
#211225=CARTESIAN_POINT('Ctrl Pts',(18.432524408893,16.1950645986679,3.18128613052084));
#211226=CARTESIAN_POINT('Ctrl Pts',(16.0348925901549,17.8320246323415,3.30846193720228));
#211227=CARTESIAN_POINT('Ctrl Pts',(16.1135242950128,20.7341089760952,3.43563774388371));
#211228=CARTESIAN_POINT('Ctrl Pts',(18.5962798138393,22.2388353695441,3.56281355056515));
#211229=CARTESIAN_POINT('Ctrl Pts',(21.2053850557409,20.9657107398561,3.68998935724659));
#211230=CARTESIAN_POINT('Ctrl Pts',(21.5471479003775,18.0827479161047,3.81716516392802));
#211231=CARTESIAN_POINT('Ctrl Pts',(19.3080221501088,16.2348863520412,3.94434097060946));
#211232=CARTESIAN_POINT('Ctrl Pts',(16.5422667049268,17.1174243415679,4.07151677729088));
#211233=CARTESIAN_POINT('Ctrl Pts',(15.7872905236753,19.9206880557286,4.19869258397231));
#211234=CARTESIAN_POINT('Ctrl Pts',(17.7357373935294,22.0728570269757,4.32586839065375));
#211235=CARTESIAN_POINT('Ctrl Pts',(20.6000282456582,21.5994498028477,4.45304419733518));
#211236=CARTESIAN_POINT('Ctrl Pts',(21.7523540011689,18.9347881285228,4.58022000401662));
#211237=CARTESIAN_POINT('Ctrl Pts',(20.1355273007852,16.5235337026348,4.70739581069805));
#211238=CARTESIAN_POINT('Ctrl Pts',(17.2328862905255,16.5778628016098,4.83457161737948));
#211239=CARTESIAN_POINT('Ctrl Pts',(15.7074239390844,19.0479318491813,4.96174742406093));
#211240=CARTESIAN_POINT('Ctrl Pts',(16.9586572730372,21.6676058039782,5.08892323074235));
#211241=CARTESIAN_POINT('Ctrl Pts',(19.8386573687817,22.0334964077772,5.21609903742379));
#211242=CARTESIAN_POINT('Ctrl Pts',(21.7052028914376,19.8099217413247,5.34327484410521));
#211243=CARTESIAN_POINT('Ctrl Pts',(20.8458541748489,17.0368735504825,5.47045065078667));
#211244=CARTESIAN_POINT('Ctrl Pts',(18.0490103292891,16.2584514355665,5.59762645746809));
#211245=CARTESIAN_POINT('Ctrl Pts',(15.8806019913527,18.188809372687,5.72480226414953));
#211246=CARTESIAN_POINT('Ctrl Pts',(16.3300092244964,21.0569637660617,5.85197807083096));
#211247=CARTESIAN_POINT('Ctrl Pts',(18.9849287856695,22.2315609775075,5.97915387751239));
#211248=CARTESIAN_POINT('Ctrl Pts',(21.4096367603877,20.634980969248,6.10632968419384));
#211249=CARTESIAN_POINT('Ctrl Pts',(21.3796140761966,17.73198680393,6.23350549087526));
#211250=CARTESIAN_POINT('Ctrl Pts',(18.9224046824235,16.1858954480944,6.3606812975567));
#211251=CARTESIAN_POINT('Ctrl Pts',(16.2923456862402,17.4151497594685,6.48785710423813));
#211252=CARTESIAN_POINT('Ctrl Pts',(15.9023529767735,20.2919852034935,6.61503291091956));
#211253=CARTESIAN_POINT('Ctrl Pts',(18.1102206592817,22.1770838168218,6.74220871760101));
#211254=CARTESIAN_POINT('Ctrl Pts',(20.8903671707866,21.3409846241399,6.86938452428244));
#211255=CARTESIAN_POINT('Ctrl Pts',(21.6921806423356,18.550756740565,6.99656033096387));
#211256=CARTESIAN_POINT('Ctrl Pts',(19.7800469799392,16.3662610682035,7.12373613764531));
#211257=CARTESIAN_POINT('Ctrl Pts',(16.9082301384463,16.7916368013544,7.25091194432673));
#211258=CARTESIAN_POINT('Ctrl Pts',(15.7114438248711,19.4366281066474,7.37808775100818));
#211259=CARTESIAN_POINT('Ctrl Pts',(17.2876652009831,21.8746196281511,7.50526355768959));
#211260=CARTESIAN_POINT('Ctrl Pts',(20.1908089855312,21.8689054637052,7.63243936437105));
#211261=CARTESIAN_POINT('Ctrl Pts',(21.7574209456176,19.4247280045279,7.75961517105247));
#211262=CARTESIAN_POINT('Ctrl Pts',(20.5502318427671,16.7844683666522,7.88679097773391));
#211263=CARTESIAN_POINT('Ctrl Pts',(17.6767627522393,16.3704008948346,8.01396678441534));
#211264=CARTESIAN_POINT('Ctrl Pts',(15.7732432169878,18.562406794542,8.14114259109678));
#211265=CARTESIAN_POINT('Ctrl Pts',(16.5860342648591,21.3494567040227,8.26831839777821));
#211266=CARTESIAN_POINT('Ctrl Pts',(19.3694505569332,22.1746053151545,8.39549420445964));
#211267=CARTESIAN_POINT('Ctrl Pts',(21.5698804035306,20.2808299917227,8.52267001114109));
#211268=CARTESIAN_POINT('Ctrl Pts',(21.1685659944773,17.4055520520233,8.64984581782252));
#211269=CARTESIAN_POINT('Ctrl Pts',(18.5336883916982,16.1866605458549,8.77702162450395));
#211270=CARTESIAN_POINT('Ctrl Pts',(16.0825842567954,17.7424127771882,8.90419743118537));
#211271=CARTESIAN_POINT('Ctrl Pts',(16.0639895008622,20.6455026346484,9.03137323786683));
#211272=CARTESIAN_POINT('Ctrl Pts',(18.4949636583467,22.2325253600935,9.15854904454826));
#211273=CARTESIAN_POINT('Ctrl Pts',(21.1452388230294,21.0474861046668,9.28572485122969));
#211274=CARTESIAN_POINT('Ctrl Pts',(21.5833520259422,18.1775848333912,9.41290065791111));
#211275=CARTESIAN_POINT('Ctrl Pts',(19.4073615957849,16.2557778365002,9.54007646459256));
#211276=CARTESIAN_POINT('Ctrl Pts',(16.6136036950289,17.0452037528466,9.66725227127399));
#211277=CARTESIAN_POINT('Ctrl Pts',(15.7651777974467,19.8216133014809,9.79442807795543));
#211278=CARTESIAN_POINT('Ctrl Pts',(17.6404620048199,22.0378230449422,9.92160388463686));
#211279=CARTESIAN_POINT('Ctrl Pts',(20.5189994501482,21.6605980970946,10.0487796913183));
#211280=CARTESIAN_POINT('Ctrl Pts',(21.7599106895262,19.0360189343673,10.1759554979997));
#211281=CARTESIAN_POINT('Ctrl Pts',(20.2247366804621,16.5719740388084,10.3031313046812));
#211282=CARTESIAN_POINT('Ctrl Pts',(17.3219042926274,16.5290716662188,10.4303071113626));
#211283=CARTESIAN_POINT('Ctrl Pts',(15.7145820717629,18.9466720806279,10.557482918044));
#211284=CARTESIAN_POINT('Ctrl Pts',(16.8773883938439,21.60677695502,10.6846587247255));
#211285=CARTESIAN_POINT('Ctrl Pts',(19.7435206302607,22.0689051718692,10.8118345314069));
#211286=CARTESIAN_POINT('Ctrl Pts',(21.6834803463302,19.9090827751282,10.9390103380884));
#211287=CARTESIAN_POINT('Ctrl Pts',(20.9174749100379,17.1088127601106,11.0661861447698));
#211288=CARTESIAN_POINT('Ctrl Pts',(18.1482667655227,16.2371690612364,11.1933619514512));
#211289=CARTESIAN_POINT('Ctrl Pts',(15.9164325089359,18.0938306719134,11.3205377581326));
#211290=CARTESIAN_POINT('Ctrl Pts',(16.2695415474392,20.9754258017613,11.4477135648141));
#211291=CARTESIAN_POINT('Ctrl Pts',(18.8836382546247,22.2382697711092,11.5748893714955));
#211292=CARTESIAN_POINT('Ctrl Pts',(21.3604511507894,20.7237816190169,11.702065178177));
#211293=CARTESIAN_POINT('Ctrl Pts',(21.4276581320481,17.8214102252931,11.8292409848584));
#211294=CARTESIAN_POINT('Ctrl Pts',(19.0236009644314,16.1939012021945,11.9564167915398));
#211295=CARTESIAN_POINT('Ctrl Pts',(16.353852886612,17.3343930638118,12.0835925982213));
#211296=CARTESIAN_POINT('Ctrl Pts',(15.8677420567354,20.1965553140193,12.2107684049027));
#211297=CARTESIAN_POINT('Ctrl Pts',(18.0112449897728,22.1545317340756,12.3379442115841));
#211298=CARTESIAN_POINT('Ctrl Pts',(20.8178307854584,21.4120004843013,12.4651200182656));
#211299=CARTESIAN_POINT('Ctrl Pts',(21.712631172611,18.6501878996771,12.592295824947));
#211300=CARTESIAN_POINT('Ctrl Pts',(19.8747223335935,16.4028856091748,12.7194716316284));
#211301=CARTESIAN_POINT('Ctrl Pts',(16.9902715547168,16.731853981019,12.8466474383099));
#211302=CARTESIAN_POINT('Ctrl Pts',(15.7055833963943,19.3352849521227,12.9738232449913));
#211303=CARTESIAN_POINT('Ctrl Pts',(17.199279507147,21.824692193648,13.1009990516727));
#211304=CARTESIAN_POINT('Ctrl Pts',(20.1009864145957,21.9161990715341,13.2281748583542));
#211305=CARTESIAN_POINT('Ctrl Pts',(21.7485681313984,19.5258537048782,13.3553506650356));
#211306=CARTESIAN_POINT('Ctrl Pts',(20.6304706928427,16.8466496060213,13.482526471717));
#211307=CARTESIAN_POINT('Ctrl Pts',(17.77247910185,16.3365902455044,13.6097022783985));
#211308=CARTESIAN_POINT('Ctrl Pts',(15.7966232561924,18.4636234287474,13.7368780850799));
#211309=CARTESIAN_POINT('Ctrl Pts',(16.5156282588163,21.2763282286931,13.8640538917614));
#211310=CARTESIAN_POINT('Ctrl Pts',(19.2698516462976,22.1942225675398,13.9912296984428));
#211311=CARTESIAN_POINT('Ctrl Pts',(21.5324644070049,20.3751953603434,14.1184055051242));
#211312=CARTESIAN_POINT('Ctrl Pts',(21.2276597665751,17.4880911681452,14.2455813118056));
#211313=CARTESIAN_POINT('Ctrl Pts',(18.635077064293,16.1816488933915,14.3727571184871));
#211314=CARTESIAN_POINT('Ctrl Pts',(16.1332500156721,17.6544482362164,14.4999329251685));
#211315=CARTESIAN_POINT('Ctrl Pts',(16.0174496569233,20.5552872118146,14.6271087318499));
#211316=CARTESIAN_POINT('Ctrl Pts',(18.3939156298175,22.2228261064472,14.7542845385314));
#211317=CARTESIAN_POINT('Ctrl Pts',(21.0823879043376,21.1272014834248,14.8814603452128));
#211318=CARTESIAN_POINT('Ctrl Pts',(21.6163600340197,18.2735809322375,15.0086361518943));
#211319=CARTESIAN_POINT('Ctrl Pts',(19.5059457319285,16.279984192933,15.1358119585757));
#211320=CARTESIAN_POINT('Ctrl Pts',(16.6873191331485,16.975412537255,15.2629877652571));
#211321=CARTESIAN_POINT('Ctrl Pts',(15.7463951983637,19.7218536224386,15.3901635719385));
#211322=CARTESIAN_POINT('Ctrl Pts',(17.5464132374134,21.9996182161866,15.51733937862));
#211323=CARTESIAN_POINT('Ctrl Pts',(20.4359684211888,21.7189986777498,15.6445151853014));
#211324=CARTESIAN_POINT('Ctrl Pts',(21.7640732145973,19.137446016431,15.7716909919829));
#211325=CARTESIAN_POINT('Ctrl Pts',(20.3122739011665,16.6233745697617,15.8988667986643));
#211326=CARTESIAN_POINT('Ctrl Pts',(17.4125062421414,16.4832888491888,16.0260426053457));
#211327=CARTESIAN_POINT('Ctrl Pts',(15.7251270847987,18.8457088086375,16.1532184120272));
#211328=CARTESIAN_POINT('Ctrl Pts',(16.7982020754384,21.543260763633,16.2803942187086));
#211329=CARTESIAN_POINT('Ctrl Pts',(19.6472515126938,22.1011082244237,16.40757002539));
#211330=CARTESIAN_POINT('Ctrl Pts',(21.6584493698341,20.0074607696524,16.5347458320715));
#211331=CARTESIAN_POINT('Ctrl Pts',(20.9866464419502,17.1831099926555,16.6619216387529));
#211332=CARTESIAN_POINT('Ctrl Pts',(18.2481802185833,16.2192224323484,16.7890974454343));
#211333=CARTESIAN_POINT('Ctrl Pts',(15.9554234912899,18.0001050997038,16.9162732521158));
#211334=CARTESIAN_POINT('Ctrl Pts',(16.2118382528302,20.8919086814673,17.0434490587972));
#211335=CARTESIAN_POINT('Ctrl Pts',(18.782179874386,22.2415828769435,17.1706248654786));
#211336=CARTESIAN_POINT('Ctrl Pts',(21.3083194515728,20.8108853820109,17.2978006721601));
#211337=CARTESIAN_POINT('Ctrl Pts',(21.4726807122266,17.9123923491693,17.4249764788415));
#211338=CARTESIAN_POINT('Ctrl Pts',(19.1244724011078,16.2052912352836,17.552152285523));
#211339=CARTESIAN_POINT('Ctrl Pts',(16.418029897423,17.2557413577005,17.6793280922044));
#211340=CARTESIAN_POINT('Ctrl Pts',(15.8363462175366,20.1000199273879,17.8065038988858));
#211341=CARTESIAN_POINT('Ctrl Pts',(17.9130800343833,22.1286778924994,17.9336797055672));
#211342=CARTESIAN_POINT('Ctrl Pts',(20.7429569676441,21.4805474827506,18.0608555122487));
#211343=CARTESIAN_POINT('Ctrl Pts',(21.7297405730228,18.7502481215919,18.1880313189301));
#211344=CARTESIAN_POINT('Ctrl Pts',(19.9681181392836,16.4426600113656,18.3152071256115));
#211345=CARTESIAN_POINT('Ctrl Pts',(17.0742689107603,16.6748520181929,18.442382932293));
#211346=CARTESIAN_POINT('Ctrl Pts',(15.7031199420884,19.2338023871561,18.5695587389744));
#211347=CARTESIAN_POINT('Ctrl Pts',(17.1126153089119,21.7718329813254,18.6967345456558));
#211348=CARTESIAN_POINT('Ctrl Pts',(20.0096304953375,21.9604582580674,18.8239103523373));
#211349=CARTESIAN_POINT('Ctrl Pts',(21.7363338768253,19.6266262342004,18.9510861590187));
#211350=CARTESIAN_POINT('Ctrl Pts',(20.708582272227,16.9114829360825,19.0782619657001));
#211351=CARTESIAN_POINT('Ctrl Pts',(17.8692739891718,16.3060038219983,19.2054377723816));
#211352=CARTESIAN_POINT('Ctrl Pts',(15.8232981502683,18.3656783929507,19.332613579063));
#211353=CARTESIAN_POINT('Ctrl Pts',(16.4477105996423,21.200883079277,19.4597893857445));
#211354=CARTESIAN_POINT('Ctrl Pts',(19.1696516713374,22.2104935320204,19.5869651924259));
#211355=CARTESIAN_POINT('Ctrl Pts',(21.4919093729839,20.4682548664865,19.7141409991073));
#211356=CARTESIAN_POINT('Ctrl Pts',(21.2839564023691,17.5725628414412,19.8413168057888));
#211357=CARTESIAN_POINT('Ctrl Pts',(18.7365766963097,16.1800353196856,19.9684926124702));
#211358=CARTESIAN_POINT('Ctrl Pts',(16.186833039821,17.5682295703764,20.0956684191516));
#211359=CARTESIAN_POINT('Ctrl Pts',(15.9739569578914,20.4635641116309,20.222844225833));
#211360=CARTESIAN_POINT('Ctrl Pts',(18.2932490910976,22.2097480848697,20.3500200325145));
#211361=CARTESIAN_POINT('Ctrl Pts',(21.0169027662538,21.2047682366741,20.4771958391959));
#211362=CARTESIAN_POINT('Ctrl Pts',(21.6461349636216,18.3706270360342,20.6043716458773));
#211363=CARTESIAN_POINT('Ctrl Pts',(19.6036638532537,16.3074811554586,20.7315474525588));
#211364=CARTESIAN_POINT('Ctrl Pts',(16.7633305706532,16.9081234172833,20.8587232592402));
#211365=CARTESIAN_POINT('Ctrl Pts',(15.7309633363042,19.6215316380409,20.9858990659217));
#211366=CARTESIAN_POINT('Ctrl Pts',(17.4536974694716,21.9582647385426,21.1130748726031));
#211367=CARTESIAN_POINT('Ctrl Pts',(20.3510265917206,21.7746258438458,21.2402506792845));
#211368=CARTESIAN_POINT('Ctrl Pts',(21.7648401891172,19.2388788921253,21.367426485966));
#211369=CARTESIAN_POINT('Ctrl Pts',(20.3980344469297,16.677825473566,21.4946022926474));
#211370=CARTESIAN_POINT('Ctrl Pts',(17.5046027110691,16.4402807821758,21.6217780993288));
#211371=CARTESIAN_POINT('Ctrl Pts',(15.7390235403886,18.7457046750729,21.7489539060103));
#211372=CARTESIAN_POINT('Ctrl Pts',(16.7212335728181,21.4760667201902,21.8761297126917));
#211373=CARTESIAN_POINT('Ctrl Pts',(19.5498596762323,22.1321442401452,22.0033055193731));
#211374=CARTESIAN_POINT('Ctrl Pts',(21.6307161859342,20.100377524994,22.1304999838292));
#211375=CARTESIAN_POINT('Ctrl Pts',(21.2446789959721,18.2129921435845,22.2153025127247));
#211376=CARTESIAN_POINT('Ctrl Pts',(20.6946892744878,17.5599162803241,22.2577131060598));
#211377=CARTESIAN_POINT('Ctrl Pts',(18.1101968784744,16.8797697475724,-0.0847274365222671));
#211378=CARTESIAN_POINT('Ctrl Pts',(17.3340242953481,17.0874621793657,-0.0423355009617889));
#211379=CARTESIAN_POINT('Ctrl Pts',(16.0189820756719,18.3356945672447,0.0424483701591674));
#211380=CARTESIAN_POINT('Ctrl Pts',(16.5291381343926,21.0253906167311,0.169624176840601));
#211381=CARTESIAN_POINT('Ctrl Pts',(19.065875791,22.0444183413159,0.296799983522036));
#211382=CARTESIAN_POINT('Ctrl Pts',(21.2962359728301,20.4669656763903,0.42397579020347));
#211383=CARTESIAN_POINT('Ctrl Pts',(21.1768856283234,17.7356987913358,0.551151596884905));
#211384=CARTESIAN_POINT('Ctrl Pts',(18.8158303252349,16.3587285734324,0.678327403566338));
#211385=CARTESIAN_POINT('Ctrl Pts',(16.3799648594531,17.5981257224815,0.805503210247773));
#211386=CARTESIAN_POINT('Ctrl Pts',(16.1036434964602,20.3174500578439,0.932679016929206));
#211387=CARTESIAN_POINT('Ctrl Pts',(18.2405820741981,22.0215634996219,1.05985482361064));
#211388=CARTESIAN_POINT('Ctrl Pts',(20.8301640752336,21.1472173052792,1.18703063029207));
#211389=CARTESIAN_POINT('Ctrl Pts',(21.4966647872182,18.4964818468598,1.31420643697351));
#211390=CARTESIAN_POINT('Ctrl Pts',(19.6285820913403,16.501288045487,1.44138224365494));
#211391=CARTESIAN_POINT('Ctrl Pts',(16.9397810066015,16.992078683811,1.56855805033638));
#211392=CARTESIAN_POINT('Ctrl Pts',(15.8970618110187,19.518596108525,1.69573385701782));
#211393=CARTESIAN_POINT('Ctrl Pts',(17.4570587119471,21.7629110154817,1.82290966369925));
#211394=CARTESIAN_POINT('Ctrl Pts',(20.1885692683029,21.6660070863072,1.95008547038068));
#211395=CARTESIAN_POINT('Ctrl Pts',(21.5856031755938,19.3167859434159,2.07726127706212));
#211396=CARTESIAN_POINT('Ctrl Pts',(20.3664679657325,16.8705130678377,2.20443708374355));
#211397=CARTESIAN_POINT('Ctrl Pts',(17.64964482037,16.5714915274638,2.33161289042498));
#211398=CARTESIAN_POINT('Ctrl Pts',(15.927650197406,18.6940552662862,2.45878869710642));
#211399=CARTESIAN_POINT('Ctrl Pts',(16.780307363717,21.2908836705225,2.58596450378785));
#211400=CARTESIAN_POINT('Ctrl Pts',(19.4253562499103,21.979547921279,2.71314031046929));
#211401=CARTESIAN_POINT('Ctrl Pts',(21.4361286945186,20.128241278265,2.84031611715073));
#211402=CARTESIAN_POINT('Ctrl Pts',(20.9678657711395,17.4354226988042,2.96749192383215));
#211403=CARTESIAN_POINT('Ctrl Pts',(18.4501696540519,16.3715860853484,3.0946677305136));
#211404=CARTESIAN_POINT('Ctrl Pts',(16.1928702618537,17.9127355062838,3.22184353719502));
#211405=CARTESIAN_POINT('Ctrl Pts',(16.2668996846349,20.6449620199907,3.34901934387646));
#211406=CARTESIAN_POINT('Ctrl Pts',(18.6043405209739,22.0616173825078,3.47619515055789));
#211407=CARTESIAN_POINT('Ctrl Pts',(21.0607358818871,20.8630082256189,3.60337095723933));
#211408=CARTESIAN_POINT('Ctrl Pts',(21.3824954846104,18.1487840570351,3.73054676392076));
#211409=CARTESIAN_POINT('Ctrl Pts',(19.2744248644109,16.4090770875045,3.8577225706022));
#211410=CARTESIAN_POINT('Ctrl Pts',(16.6705479736444,17.2399604832709,3.98489837728363));
#211411=CARTESIAN_POINT('Ctrl Pts',(15.9597602447928,19.8791502991104,4.11207418396507));
#211412=CARTESIAN_POINT('Ctrl Pts',(17.7941653025999,21.9053536856092,4.23924999064649));
#211413=CARTESIAN_POINT('Ctrl Pts',(20.4908103625543,21.4596547960069,4.36642579732794));
#211414=CARTESIAN_POINT('Ctrl Pts',(21.5756909548122,18.9509546983274,4.49360160400936));
#211415=CARTESIAN_POINT('Ctrl Pts',(20.0534964712626,16.6808300246996,4.62077741069081));
#211416=CARTESIAN_POINT('Ctrl Pts',(17.3207458725165,16.7319792633511,4.74795321737223));
#211417=CARTESIAN_POINT('Ctrl Pts',(15.8845682192929,19.0574761624978,4.87512902405368));
#211418=CARTESIAN_POINT('Ctrl Pts',(17.062567369186,21.5238216537891,5.0023048307351));
#211419=CARTESIAN_POINT('Ctrl Pts',(19.7740022170421,21.86829682763,5.12948063741654));
#211420=CARTESIAN_POINT('Ctrl Pts',(21.5312995805795,19.7748670925622,5.25665644409798));
#211421=CARTESIAN_POINT('Ctrl Pts',(20.7222481989278,17.1641242976074,5.3838322507794));
#211422=CARTESIAN_POINT('Ctrl Pts',(18.0891024993605,16.4312629161638,5.51100805746085));
#211423=CARTESIAN_POINT('Ctrl Pts',(16.0476102297768,18.2486377791988,5.63818386414227));
#211424=CARTESIAN_POINT('Ctrl Pts',(16.4707138382194,20.948920248883,5.76535967082371));
#211425=CARTESIAN_POINT('Ctrl Pts',(18.9702420247138,22.0547687577129,5.89253547750515));
#211426=CARTESIAN_POINT('Ctrl Pts',(21.253032816367,20.5516359355363,6.01971128418657));
#211427=CARTESIAN_POINT('Ctrl Pts',(21.2247673478128,17.8185528517555,6.14688709086802));
#211428=CARTESIAN_POINT('Ctrl Pts',(18.911377432097,16.3629536014721,6.27406289754945));
#211429=CARTESIAN_POINT('Ctrl Pts',(16.4352547317172,17.5202601521426,6.40123870423088));
#211430=CARTESIAN_POINT('Ctrl Pts',(16.0680881387646,20.2287155740725,6.52841451091232));
#211431=CARTESIAN_POINT('Ctrl Pts',(18.1467302133443,22.003480123343,6.65559031759375));
#211432=CARTESIAN_POINT('Ctrl Pts',(20.7641558671069,21.2163174803099,6.78276612427519));
#211433=CARTESIAN_POINT('Ctrl Pts',(21.5190395184827,18.5894005131322,6.90994193095662));
#211434=CARTESIAN_POINT('Ctrl Pts',(19.718822270698,16.5327624943404,7.03711773763806));
#211435=CARTESIAN_POINT('Ctrl Pts',(17.0150917145117,16.9332411568245,7.16429354431949));
#211436=CARTESIAN_POINT('Ctrl Pts',(15.8883528227805,19.4234221842643,7.29146935100092));
#211437=CARTESIAN_POINT('Ctrl Pts',(17.3723185953652,21.7187190420494,7.41864515768236));
#211438=CARTESIAN_POINT('Ctrl Pts',(20.1055425412228,21.7133393253515,7.54582096436379));
#211439=CARTESIAN_POINT('Ctrl Pts',(21.5804613330392,19.4122185903382,7.67299677104523));
#211440=CARTESIAN_POINT('Ctrl Pts',(20.4439285231071,16.9264922877238,7.80017257772666));
#211441=CARTESIAN_POINT('Ctrl Pts',(17.7386424233577,16.5366600185829,7.9273483844081));
#211442=CARTESIAN_POINT('Ctrl Pts',(15.946535121319,18.600368694133,8.05452419108952));
#211443=CARTESIAN_POINT('Ctrl Pts',(16.7117538358879,21.2242936927628,8.18169999777097));
#211444=CARTESIAN_POINT('Ctrl Pts',(19.3322578912771,22.0011466873821,8.30887580445239));
#211445=CARTESIAN_POINT('Ctrl Pts',(21.4038974634922,20.2182132723624,8.43605161113384));
#211446=CARTESIAN_POINT('Ctrl Pts',(21.0260718254785,17.5112241946562,8.56322741781526));
#211447=CARTESIAN_POINT('Ctrl Pts',(18.5454125496099,16.3636739183683,8.69040322449671));
#211448=CARTESIAN_POINT('Ctrl Pts',(16.237770554417,17.82836859699,8.81757903117813));
#211449=CARTESIAN_POINT('Ctrl Pts',(16.2202641420738,20.5615417720903,8.94475483785957));
#211450=CARTESIAN_POINT('Ctrl Pts',(18.5089543593347,22.0556766953737,9.071930644541));
#211451=CARTESIAN_POINT('Ctrl Pts',(21.0041099839982,20.9399973111998,9.19910645122244));
#211452=CARTESIAN_POINT('Ctrl Pts',(21.4165805972594,18.2380702076759,9.32628225790388));
#211453=CARTESIAN_POINT('Ctrl Pts',(19.3679500122646,16.4287458017761,9.4534580645853));
#211454=CARTESIAN_POINT('Ctrl Pts',(16.7377096383923,17.1719669365758,9.58063387126675));
#211455=CARTESIAN_POINT('Ctrl Pts',(15.9389417675414,19.7858743504024,9.70780967794817));
#211456=CARTESIAN_POINT('Ctrl Pts',(17.7044663440924,21.8723702284609,9.83498548462961));
#211457=CARTESIAN_POINT('Ctrl Pts',(20.4145241498733,21.5172241051722,9.96216129131105));
#211458=CARTESIAN_POINT('Ctrl Pts',(21.5828053532376,19.0462605057991,10.0893370979925));
#211459=CARTESIAN_POINT('Ctrl Pts',(20.1374844618078,16.7264351674692,10.2165129046739));
#211460=CARTESIAN_POINT('Ctrl Pts',(17.4045536867392,16.6860438535011,10.3436887113554));
#211461=CARTESIAN_POINT('Ctrl Pts',(15.8913073893432,18.9621430874931,10.4708645180368));
#211462=CARTESIAN_POINT('Ctrl Pts',(16.986055124823,21.4665530929081,10.5980403247182));
#211463=CARTESIAN_POINT('Ctrl Pts',(19.6844337935833,21.9016331309934,10.7252161313997));
#211464=CARTESIAN_POINT('Ctrl Pts',(21.5108484473051,19.8682242709185,10.8523919380811));
#211465=CARTESIAN_POINT('Ctrl Pts',(20.7896770012766,17.2318529342145,10.9795677447625));
#211466=CARTESIAN_POINT('Ctrl Pts',(18.182549496281,16.4112261906481,11.106743551444));
#211467=CARTESIAN_POINT('Ctrl Pts',(16.0813436015692,18.1592181436015,11.2339193581254));
#211468=CARTESIAN_POINT('Ctrl Pts',(16.4137853099934,20.8721546688561,11.3610951648069));
#211469=CARTESIAN_POINT('Ctrl Pts',(18.8748799877338,22.0610848883219,11.4882709714883));
#211470=CARTESIAN_POINT('Ctrl Pts',(21.2067260207266,20.6352391189707,11.6154467781697));
#211471=CARTESIAN_POINT('Ctrl Pts',(21.2699994043883,17.902742356213,11.7426225848512));
#211472=CARTESIAN_POINT('Ctrl Pts',(19.0066507363984,16.3704907820029,11.8697983915326));
#211473=CARTESIAN_POINT('Ctrl Pts',(16.4931619403762,17.4442301134199,11.996974198214));
#211474=CARTESIAN_POINT('Ctrl Pts',(16.0355029819632,20.1388711576679,12.1241500048955));
#211475=CARTESIAN_POINT('Ctrl Pts',(18.053547549985,21.9822480049345,12.2513258115769));
#211476=CARTESIAN_POINT('Ctrl Pts',(20.6958650072534,21.2831768107233,12.3785016182583));
#211477=CARTESIAN_POINT('Ctrl Pts',(21.5382930874419,18.6830120064713,12.5056774249398));
#211478=CARTESIAN_POINT('Ctrl Pts',(19.807956313961,16.5672434156512,12.6328532316212));
#211479=CARTESIAN_POINT('Ctrl Pts',(17.0923312796673,16.8769574009315,12.7600290383026));
#211480=CARTESIAN_POINT('Ctrl Pts',(15.8828354028266,19.3280106038356,12.8872048449841));
#211481=CARTESIAN_POINT('Ctrl Pts',(17.2891060806598,21.6717138402177,13.0143806516655));
#211482=CARTESIAN_POINT('Ctrl Pts',(20.0209772492569,21.7578648573255,13.1415564583469));
#211483=CARTESIAN_POINT('Ctrl Pts',(21.5721266704775,19.507425444098,13.2687322650284));
#211484=CARTESIAN_POINT('Ctrl Pts',(20.5194710255427,16.9850340841485,13.3959080717098));
#211485=CARTESIAN_POINT('Ctrl Pts',(17.8287565335022,16.5048282929666,13.5230838783912));
#211486=CARTESIAN_POINT('Ctrl Pts',(15.9685467362274,18.5073670790289,13.6502596850727));
#211487=CARTESIAN_POINT('Ctrl Pts',(16.6454686650766,21.1554453976977,13.7774354917541));
#211488=CARTESIAN_POINT('Ctrl Pts',(19.2384884648439,22.0196157498711,13.9046112984355));
#211489=CARTESIAN_POINT('Ctrl Pts',(21.3686714102025,20.3070554738911,14.031787105117));
#211490=CARTESIAN_POINT('Ctrl Pts',(21.0817068628502,17.5889323294909,14.1589629117984));
#211491=CARTESIAN_POINT('Ctrl Pts',(18.6408669839544,16.3589555959089,14.2861387184799));
#211492=CARTESIAN_POINT('Ctrl Pts',(16.2854708667935,17.7455525852409,14.4133145251613));
#211493=CARTESIAN_POINT('Ctrl Pts',(16.1764482564922,20.4766066216898,14.5404903318427));
#211494=CARTESIAN_POINT('Ctrl Pts',(18.4138206312956,22.0465451351444,14.6676661385241));
#211495=CARTESIAN_POINT('Ctrl Pts',(20.9449377043124,21.0150469808834,14.7948419452056));
#211496=CARTESIAN_POINT('Ctrl Pts',(21.4476566598927,18.3284476934456,14.922017751887));
#211497=CARTESIAN_POINT('Ctrl Pts',(19.4607640585489,16.4515353698976,15.0491935585684));
#211498=CARTESIAN_POINT('Ctrl Pts',(16.8071105415512,17.1062605727777,15.1763693652499));
#211499=CARTESIAN_POINT('Ctrl Pts',(15.9212585064325,19.6919535652726,15.3035451719313));
#211500=CARTESIAN_POINT('Ctrl Pts',(17.615922213236,21.8364015129747,15.4307209786127));
#211501=CARTESIAN_POINT('Ctrl Pts',(20.3363528936617,21.5722065233178,15.5578967852942));
#211502=CARTESIAN_POINT('Ctrl Pts',(21.5867242473895,19.1417511015219,15.6850725919756));
#211503=CARTESIAN_POINT('Ctrl Pts',(20.2198981641729,16.7748272460081,15.8122483986571));
#211504=CARTESIAN_POINT('Ctrl Pts',(17.4898527405687,16.642940686348,15.9394242053385));
#211505=CARTESIAN_POINT('Ctrl Pts',(15.9012352070049,18.8670891552265,16.0666000120199));
#211506=CARTESIAN_POINT('Ctrl Pts',(16.9115035498021,21.4067544786704,16.1937758187014));
#211507=CARTESIAN_POINT('Ctrl Pts',(19.5937992687688,21.931951351827,16.3209516253828));
#211508=CARTESIAN_POINT('Ctrl Pts',(21.4872825238012,19.9608442409695,16.4481274320642));
#211509=CARTESIAN_POINT('Ctrl Pts',(20.854799951232,17.3018015796049,16.5753032387457));
#211510=CARTESIAN_POINT('Ctrl Pts',(18.2766150550976,16.3943299707347,16.7024790454271));
#211511=CARTESIAN_POINT('Ctrl Pts',(16.1180524573998,18.0709782914572,16.8296548521085));
#211512=CARTESIAN_POINT('Ctrl Pts',(16.3594593660219,20.7935257720403,16.9568306587899));
#211513=CARTESIAN_POINT('Ctrl Pts',(18.7793599257057,22.0642040794035,17.0840064654714));
#211514=CARTESIAN_POINT('Ctrl Pts',(21.1576455689089,20.717244733731,17.2111822721528));
#211515=CARTESIAN_POINT('Ctrl Pts',(21.3123868310473,17.9883993329521,17.3383580788343));
#211516=CARTESIAN_POINT('Ctrl Pts',(19.1016182084348,16.3812141610339,17.4655338855157));
#211517=CARTESIAN_POINT('Ctrl Pts',(16.5535826965425,17.3701818600505,17.5927096921971));
#211518=CARTESIAN_POINT('Ctrl Pts',(16.0059447286121,20.0479859484101,17.7198854988786));
#211519=CARTESIAN_POINT('Ctrl Pts',(17.9611281499736,21.9579073783129,17.84706130556));
#211520=CARTESIAN_POINT('Ctrl Pts',(20.6253735238976,21.3477117809083,17.9742371122414));
#211521=CARTESIAN_POINT('Ctrl Pts',(21.5544010815252,18.7772157438201,18.1014129189229));
#211522=CARTESIAN_POINT('Ctrl Pts',(19.8958857006878,16.6046898380703,18.2285887256043));
#211523=CARTESIAN_POINT('Ctrl Pts',(17.1714123042272,16.8232917400757,18.3557645322858));
#211524=CARTESIAN_POINT('Ctrl Pts',(15.8805161335109,19.2324677726021,18.4829403389672));
#211525=CARTESIAN_POINT('Ctrl Pts',(17.2075143031097,21.6219484563438,18.6101161456486));
#211526=CARTESIAN_POINT('Ctrl Pts',(19.9349683552291,21.7995335714625,18.7372919523301));
#211527=CARTESIAN_POINT('Ctrl Pts',(21.5606084819066,19.6022997977881,18.8644677590115));
#211528=CARTESIAN_POINT('Ctrl Pts',(20.5930107655851,17.0460727454631,18.9916435656929));
#211529=CARTESIAN_POINT('Ctrl Pts',(17.919886054979,16.4760320805331,19.1188193723744));
#211530=CARTESIAN_POINT('Ctrl Pts',(15.9936603594759,18.4151547268051,19.2459951790558));
#211531=CARTESIAN_POINT('Ctrl Pts',(16.5815261991922,21.0844160225493,19.3731709857372));
#211532=CARTESIAN_POINT('Ctrl Pts',(19.1441531541393,22.0349343813413,19.5003467924186));
#211533=CARTESIAN_POINT('Ctrl Pts',(21.3304900460201,20.3946682445481,19.6275225991001));
#211534=CARTESIAN_POINT('Ctrl Pts',(21.1347084791815,17.6684599097052,19.7546984057815));
#211535=CARTESIAN_POINT('Ctrl Pts',(18.7364258833105,16.3574364640233,19.8818742124629));
#211536=CARTESIAN_POINT('Ctrl Pts',(16.3359176980786,17.6643802632539,20.0090500191444));
#211537=CARTESIAN_POINT('Ctrl Pts',(16.1355011676512,20.3902520376885,20.1362258258258));
#211538=CARTESIAN_POINT('Ctrl Pts',(18.3190460646205,22.0342325649128,20.2634016325072));
#211539=CARTESIAN_POINT('Ctrl Pts',(20.8832853850366,21.0880737832455,20.3905774391887));
#211540=CARTESIAN_POINT('Ctrl Pts',(21.4756888748341,18.4198137277981,20.5177532458701));
#211541=CARTESIAN_POINT('Ctrl Pts',(19.5527627775141,16.4774229462598,20.6449290525516));
#211542=CARTESIAN_POINT('Ctrl Pts',(16.8786730601742,17.0429098579489,20.772104859233));
#211543=CARTESIAN_POINT('Ctrl Pts',(15.9067298650559,19.5975033862937,20.8992806659144));
#211544=CARTESIAN_POINT('Ctrl Pts',(17.5286330619216,21.7974684377538,21.0264564725959));
#211545=CARTESIAN_POINT('Ctrl Pts',(20.2563826753269,21.6245778537434,21.1536322792773));
#211546=CARTESIAN_POINT('Ctrl Pts',(21.5874463311991,19.2372471517761,21.2808080859587));
#211547=CARTESIAN_POINT('Ctrl Pts',(20.300639179667,16.8260911603011,21.4079838926401));
#211548=CARTESIAN_POINT('Ctrl Pts',(17.5765588401915,16.6024498642087,21.5351596993216));
#211549=CARTESIAN_POINT('Ctrl Pts',(15.9143183086354,18.7729382233993,21.662335506003));
#211550=CARTESIAN_POINT('Ctrl Pts',(16.8390399827,21.3434932755793,21.7895113126845));
#211551=CARTESIAN_POINT('Ctrl Pts',(19.5021077373455,21.9611708420245,21.9166871193659));
#211552=CARTESIAN_POINT('Ctrl Pts',(21.4611725520066,20.0483226159722,22.0438815838219));
#211553=CARTESIAN_POINT('Ctrl Pts',(21.097729963592,18.2714051422367,22.1286841127175));
#211554=CARTESIAN_POINT('Ctrl Pts',(20.5799309194189,17.6565535467265,22.1710947060526));
#211555=CARTESIAN_POINT('Ctrl Pts',(18.1489776472236,17.0246983287242,-0.171345836529519));
#211556=CARTESIAN_POINT('Ctrl Pts',(17.4210583805961,17.2194788787227,-0.128953900969041));
#211557=CARTESIAN_POINT('Ctrl Pts',(16.1877700772709,18.3901108027545,-0.0441700298480844));
#211558=CARTESIAN_POINT('Ctrl Pts',(16.6662106099602,20.9125930681132,0.0830057768333494));
#211559=CARTESIAN_POINT('Ctrl Pts',(19.0452436430351,21.8682695891329,0.210181583514784));
#211560=CARTESIAN_POINT('Ctrl Pts',(21.1369461627689,20.3888844472776,0.337357390196218));
#211561=CARTESIAN_POINT('Ctrl Pts',(21.0250156242086,17.8274157338044,0.464533196877653));
#211562=CARTESIAN_POINT('Ctrl Pts',(18.81074307445,16.5360493895473,0.591709003559087));
#211563=CARTESIAN_POINT('Ctrl Pts',(16.5263111813342,17.6983953463737,0.718884810240521));
#211564=CARTESIAN_POINT('Ctrl Pts',(16.2671682429258,20.2486639579588,0.846060616921955));
#211565=CARTESIAN_POINT('Ctrl Pts',(18.271257019252,21.8468355936962,0.973236423603391));
#211566=CARTESIAN_POINT('Ctrl Pts',(20.6998491546166,21.0268460006587,1.10041223028482));
#211567=CARTESIAN_POINT('Ctrl Pts',(21.3249146619818,18.5409022133311,1.22758803696626));
#211568=CARTESIAN_POINT('Ctrl Pts',(19.5729674590718,16.669746184055,1.35476384364769));
#211569=CARTESIAN_POINT('Ctrl Pts',(17.0513245200395,17.1300252112755,1.48193965032912));
#211570=CARTESIAN_POINT('Ctrl Pts',(16.073429386086,19.4994733867219,1.60911545701056));
#211571=CARTESIAN_POINT('Ctrl Pts',(17.5364439588135,21.6042630902867,1.73629126369199));
#211572=CARTESIAN_POINT('Ctrl Pts',(20.0981411949616,21.5133835119668,1.86346707037343));
#211573=CARTESIAN_POINT('Ctrl Pts',(21.4083239034943,19.3102094129899,1.99064287705486));
#211574=CARTESIAN_POINT('Ctrl Pts',(20.2649802358942,17.0160171208712,2.1178186837363));
#211575=CARTESIAN_POINT('Ctrl Pts',(17.7170573196222,16.7355852361245,2.24499449041773));
#211576=CARTESIAN_POINT('Ctrl Pts',(16.1021161450239,18.7261928325832,2.37217029709916));
#211577=CARTESIAN_POINT('Ctrl Pts',(16.9017650796541,21.1615808747066,2.4993461037806));
#211578=CARTESIAN_POINT('Ctrl Pts',(19.3823758191848,21.8074320517016,2.62652191046204));
#211579=CARTESIAN_POINT('Ctrl Pts',(21.2681419942009,20.0712179632603,2.75369771714347));
#211580=CARTESIAN_POINT('Ctrl Pts',(20.8289901725761,17.5458072902532,2.8808735238249));
#211581=CARTESIAN_POINT('Ctrl Pts',(18.4678148992109,16.5481075720289,3.00804933050634));
#211582=CARTESIAN_POINT('Ctrl Pts',(16.3508479335524,17.9934463802261,3.13522513718777));
#211583=CARTESIAN_POINT('Ctrl Pts',(16.420275074257,20.5558150638861,3.26240094386921));
#211584=CARTESIAN_POINT('Ctrl Pts',(18.6124012281085,21.8843993954715,3.38957675055063));
#211585=CARTESIAN_POINT('Ctrl Pts',(20.9160867080332,20.7603057113817,3.51675255723208));
#211586=CARTESIAN_POINT('Ctrl Pts',(21.2178430688434,18.2148201979656,3.64392836391351));
#211587=CARTESIAN_POINT('Ctrl Pts',(19.2408275787131,16.5832678229678,3.77110417059494));
#211588=CARTESIAN_POINT('Ctrl Pts',(16.7988292423621,17.3624966249737,3.89827997727638));
#211589=CARTESIAN_POINT('Ctrl Pts',(16.1322299659104,19.8376125424924,4.02545578395781));
#211590=CARTESIAN_POINT('Ctrl Pts',(17.8525932116705,21.7378503442426,4.15263159063924));
#211591=CARTESIAN_POINT('Ctrl Pts',(20.3815924794505,21.3198597891662,4.27980739732068));
#211592=CARTESIAN_POINT('Ctrl Pts',(21.3990279084555,18.9671212681321,4.40698320400211));
#211593=CARTESIAN_POINT('Ctrl Pts',(19.97146564174,16.8381263467644,4.53415901068355));
#211594=CARTESIAN_POINT('Ctrl Pts',(17.4086054545075,16.8860957250923,4.66133481736498));
#211595=CARTESIAN_POINT('Ctrl Pts',(16.0617124995014,19.0670204758143,4.78851062404641));
#211596=CARTESIAN_POINT('Ctrl Pts',(17.1664774653348,21.3800375035998,4.91568643072785));
#211597=CARTESIAN_POINT('Ctrl Pts',(19.7093470653026,21.7030972474828,5.04286223740928));
#211598=CARTESIAN_POINT('Ctrl Pts',(21.3573962697213,19.7398124437998,5.17003804409073));
#211599=CARTESIAN_POINT('Ctrl Pts',(20.5986422230066,17.2913750447324,5.29721385077215));
#211600=CARTESIAN_POINT('Ctrl Pts',(18.1291946694319,16.6040743967612,5.42438965745359));
#211601=CARTESIAN_POINT('Ctrl Pts',(16.214618468201,18.3084661857105,5.55156546413503));
#211602=CARTESIAN_POINT('Ctrl Pts',(16.6114184519424,20.8408767317044,5.67874127081646));
#211603=CARTESIAN_POINT('Ctrl Pts',(18.9555552637581,21.8779765379183,5.80591707749789));
#211604=CARTESIAN_POINT('Ctrl Pts',(21.0964288723461,20.4682909018246,5.93309288417933));
#211605=CARTESIAN_POINT('Ctrl Pts',(21.069920619429,17.905118899581,6.06026869086075));
#211606=CARTESIAN_POINT('Ctrl Pts',(18.9003501817706,16.5400117548499,6.1874444975422));
#211607=CARTESIAN_POINT('Ctrl Pts',(16.5781637771942,17.6253705448169,6.31462030422363));
#211608=CARTESIAN_POINT('Ctrl Pts',(16.2338233007557,20.1654459446513,6.44179611090507));
#211609=CARTESIAN_POINT('Ctrl Pts',(18.1832397674068,21.8298764298645,6.5689719175865));
#211610=CARTESIAN_POINT('Ctrl Pts',(20.637944563427,21.09165033648,6.69614772426795));
#211611=CARTESIAN_POINT('Ctrl Pts',(21.3458983946297,18.6280442856993,6.82332353094937));
#211612=CARTESIAN_POINT('Ctrl Pts',(19.657597561457,16.6992639204773,6.9504993376308));
#211613=CARTESIAN_POINT('Ctrl Pts',(17.1219532905771,17.0748455122945,7.07767514431223));
#211614=CARTESIAN_POINT('Ctrl Pts',(16.0652618206899,19.4102162618813,7.20485095099367));
#211615=CARTESIAN_POINT('Ctrl Pts',(17.4569719897474,21.5628184559476,7.3320267576751));
#211616=CARTESIAN_POINT('Ctrl Pts',(20.0202760969144,21.5577731869978,7.45920256435654));
#211617=CARTESIAN_POINT('Ctrl Pts',(21.4035017204607,19.3997091761485,7.58637837103798));
#211618=CARTESIAN_POINT('Ctrl Pts',(20.3376252034471,17.0685162087954,7.7135541777194));
#211619=CARTESIAN_POINT('Ctrl Pts',(17.8005220944761,16.7029191423313,7.84072998440084));
#211620=CARTESIAN_POINT('Ctrl Pts',(16.1198270256501,18.638330593724,7.96790579108228));
#211621=CARTESIAN_POINT('Ctrl Pts',(16.8374734069165,21.099130681503,8.09508159776372));
#211622=CARTESIAN_POINT('Ctrl Pts',(19.2950652256212,21.8276880596097,8.22225740444514));
#211623=CARTESIAN_POINT('Ctrl Pts',(21.2379145234536,20.155596553002,8.34943321112658));
#211624=CARTESIAN_POINT('Ctrl Pts',(20.8835776564797,17.616896337289,8.47660901780802));
#211625=CARTESIAN_POINT('Ctrl Pts',(18.5571367075217,16.5406872908817,8.60378482448944));
#211626=CARTESIAN_POINT('Ctrl Pts',(16.3929568520385,17.9143244167918,8.73096063117089));
#211627=CARTESIAN_POINT('Ctrl Pts',(16.3765387832853,20.4775809095323,8.85813643785231));
#211628=CARTESIAN_POINT('Ctrl Pts',(18.5229450603227,21.878828030654,8.98531224453375));
#211629=CARTESIAN_POINT('Ctrl Pts',(20.8629811449671,20.8325085177327,9.11248805121519));
#211630=CARTESIAN_POINT('Ctrl Pts',(21.2498091685766,18.2985555819606,9.23966385789662));
#211631=CARTESIAN_POINT('Ctrl Pts',(19.3285384287442,16.6017137670521,9.36683966457805));
#211632=CARTESIAN_POINT('Ctrl Pts',(16.8618155817556,17.2987301203051,9.49401547125949));
#211633=CARTESIAN_POINT('Ctrl Pts',(16.1127057376362,19.7501353993238,9.62119127794092));
#211634=CARTESIAN_POINT('Ctrl Pts',(17.7684706833649,21.7069174119797,9.74836708462235));
#211635=CARTESIAN_POINT('Ctrl Pts',(20.3100488495983,21.3738501132499,9.87554289130379));
#211636=CARTESIAN_POINT('Ctrl Pts',(21.405700016949,19.0565020772309,10.0027186979853));
#211637=CARTESIAN_POINT('Ctrl Pts',(20.0502322431535,16.8808962961301,10.1298945046667));
#211638=CARTESIAN_POINT('Ctrl Pts',(17.487203080851,16.8430160407836,10.2570703113481));
#211639=CARTESIAN_POINT('Ctrl Pts',(16.0680327069235,18.9776140943582,10.3842461180296));
#211640=CARTESIAN_POINT('Ctrl Pts',(17.0947218558021,21.3263292307962,10.511421924711));
#211641=CARTESIAN_POINT('Ctrl Pts',(19.6253469569058,21.7343610901177,10.6385977313924));
#211642=CARTESIAN_POINT('Ctrl Pts',(21.3382165482799,19.8273657667087,10.7657735380739));
#211643=CARTESIAN_POINT('Ctrl Pts',(20.6618790925152,17.3548931083184,10.8929493447553));
#211644=CARTESIAN_POINT('Ctrl Pts',(18.2168322270393,16.5852833200597,11.0201251514367));
#211645=CARTESIAN_POINT('Ctrl Pts',(16.2462546942025,18.2246056152896,11.1473009581182));
#211646=CARTESIAN_POINT('Ctrl Pts',(16.5580290725475,20.768883535951,11.2744767647995));
#211647=CARTESIAN_POINT('Ctrl Pts',(18.8661217208428,21.8839000055346,11.401652571481));
#211648=CARTESIAN_POINT('Ctrl Pts',(21.0530008906637,20.5466966189245,11.5288283781625));
#211649=CARTESIAN_POINT('Ctrl Pts',(21.1123406767285,17.984074487133,11.6560041848439));
#211650=CARTESIAN_POINT('Ctrl Pts',(18.9897005083654,16.5470803618114,11.7831799915254));
#211651=CARTESIAN_POINT('Ctrl Pts',(16.6324709941403,17.554067163028,11.9103557982068));
#211652=CARTESIAN_POINT('Ctrl Pts',(16.2032639071911,20.0811870013163,12.0375316048882));
#211653=CARTESIAN_POINT('Ctrl Pts',(18.0958501101972,21.8099642757934,12.1647074115696));
#211654=CARTESIAN_POINT('Ctrl Pts',(20.5738992290484,21.1543531371454,12.2918832182511));
#211655=CARTESIAN_POINT('Ctrl Pts',(21.3639550022726,18.7158361132654,12.4190590249325));
#211656=CARTESIAN_POINT('Ctrl Pts',(19.7411902943285,16.7316012221275,12.546234831614));
#211657=CARTESIAN_POINT('Ctrl Pts',(17.1943910046178,17.0220608208441,12.6734106382954));
#211658=CARTESIAN_POINT('Ctrl Pts',(16.0600874092589,19.3207362555485,12.8005864449768));
#211659=CARTESIAN_POINT('Ctrl Pts',(17.3789326541725,21.5187354867873,12.9277622516583));
#211660=CARTESIAN_POINT('Ctrl Pts',(19.940968083918,21.5995306431169,13.0549380583397));
#211661=CARTESIAN_POINT('Ctrl Pts',(21.3956852095567,19.4889971833178,13.1821138650211));
#211662=CARTESIAN_POINT('Ctrl Pts',(20.4084713582425,17.1234185622757,13.3092896717026));
#211663=CARTESIAN_POINT('Ctrl Pts',(17.8850339651544,16.6730663404289,13.436465478384));
#211664=CARTESIAN_POINT('Ctrl Pts',(16.1404702162623,18.5511107293104,13.5636412850654));
#211665=CARTESIAN_POINT('Ctrl Pts',(16.7753090713368,21.0345625667023,13.6908170917469));
#211666=CARTESIAN_POINT('Ctrl Pts',(19.2071252833902,21.8450089322025,13.8179928984283));
#211667=CARTESIAN_POINT('Ctrl Pts',(21.2048784133999,20.2389155874388,13.9451687051097));
#211668=CARTESIAN_POINT('Ctrl Pts',(20.9357539591253,17.6897734908367,14.0723445117912));
#211669=CARTESIAN_POINT('Ctrl Pts',(18.6466569036158,16.5362622984264,14.1995203184726));
#211670=CARTESIAN_POINT('Ctrl Pts',(16.4376917179148,17.8366569342653,14.326696125154));
#211671=CARTESIAN_POINT('Ctrl Pts',(16.3354468560612,20.3979260315651,14.4538719318355));
#211672=CARTESIAN_POINT('Ctrl Pts',(18.4337256327737,21.8702641638416,14.5810477385169));
#211673=CARTESIAN_POINT('Ctrl Pts',(20.8074875042872,20.9028924783419,14.7082235451983));
#211674=CARTESIAN_POINT('Ctrl Pts',(21.2789532857658,18.3833144546537,14.8353993518798));
#211675=CARTESIAN_POINT('Ctrl Pts',(19.4155823851695,16.6230865468621,14.9625751585612));
#211676=CARTESIAN_POINT('Ctrl Pts',(16.9269019499539,17.2371086083006,15.0897509652427));
#211677=CARTESIAN_POINT('Ctrl Pts',(16.0961218145012,19.6620535081066,15.2169267719241));
#211678=CARTESIAN_POINT('Ctrl Pts',(17.6854311890587,21.6731848097627,15.3441025786055));
#211679=CARTESIAN_POINT('Ctrl Pts',(20.2367373661345,21.425414368886,15.4712783852869));
#211680=CARTESIAN_POINT('Ctrl Pts',(21.4093752801818,19.1460561866125,15.5984541919684));
#211681=CARTESIAN_POINT('Ctrl Pts',(20.1275224271794,16.9262799222545,15.7256299986498));
#211682=CARTESIAN_POINT('Ctrl Pts',(17.5671992389961,16.8025925235073,15.8528058053313));
#211683=CARTESIAN_POINT('Ctrl Pts',(16.0773433292112,18.8884695018156,15.9799816120127));
#211684=CARTESIAN_POINT('Ctrl Pts',(17.0248050241658,21.2702481937078,16.1071574186941));
#211685=CARTESIAN_POINT('Ctrl Pts',(19.5403470248439,21.7627944792304,16.2343332253756));
#211686=CARTESIAN_POINT('Ctrl Pts',(21.3161156777683,19.9142277122867,16.361509032057));
#211687=CARTESIAN_POINT('Ctrl Pts',(20.7229534605137,17.4204931665544,16.4886848387384));
#211688=CARTESIAN_POINT('Ctrl Pts',(18.3050498916118,16.5694375091209,16.6158606454198));
#211689=CARTESIAN_POINT('Ctrl Pts',(16.2806814235098,18.1418514832104,16.7430364521013));
#211690=CARTESIAN_POINT('Ctrl Pts',(16.5070804792137,20.6951428626135,16.8702122587827));
#211691=CARTESIAN_POINT('Ctrl Pts',(18.7765399770255,21.8868252818636,16.9973880654642));
#211692=CARTESIAN_POINT('Ctrl Pts',(21.0069716862451,20.6236040854512,17.1245638721456));
#211693=CARTESIAN_POINT('Ctrl Pts',(21.1520929498682,18.0644063167351,17.251739678827));
#211694=CARTESIAN_POINT('Ctrl Pts',(19.0787640157619,16.5571370867842,17.3789154855085));
#211695=CARTESIAN_POINT('Ctrl Pts',(16.6891354956622,17.4846223624005,17.5060912921899));
#211696=CARTESIAN_POINT('Ctrl Pts',(16.1755432396875,19.9959519694325,17.6332670988714));
#211697=CARTESIAN_POINT('Ctrl Pts',(18.0091762655641,21.7871368641264,17.7604429055528));
#211698=CARTESIAN_POINT('Ctrl Pts',(20.5077900801511,21.2148760790659,17.8876187122342));
#211699=CARTESIAN_POINT('Ctrl Pts',(21.3790615900277,18.8041833660481,18.0147945189156));
#211700=CARTESIAN_POINT('Ctrl Pts',(19.8236532620919,16.7667196647752,18.1419703255971));
#211701=CARTESIAN_POINT('Ctrl Pts',(17.2685556976942,16.9717314619586,18.2691461322785));
#211702=CARTESIAN_POINT('Ctrl Pts',(16.0579123249335,19.231133158048,18.3963219389599));
#211703=CARTESIAN_POINT('Ctrl Pts',(17.3024132973075,21.4720639313621,18.5234977456414));
#211704=CARTESIAN_POINT('Ctrl Pts',(19.8603062151207,21.6386088848577,18.6506735523228));
#211705=CARTESIAN_POINT('Ctrl Pts',(21.3848830869879,19.5779733613755,18.7778493590042));
#211706=CARTESIAN_POINT('Ctrl Pts',(20.4774392589433,17.1806625548439,18.9050251656857));
#211707=CARTESIAN_POINT('Ctrl Pts',(17.9704981207863,16.6460603390679,19.0322009723671));
#211708=CARTESIAN_POINT('Ctrl Pts',(16.1640225686834,18.4646310606594,19.1593767790485));
#211709=CARTESIAN_POINT('Ctrl Pts',(16.7153417987421,20.9679489658214,19.28655258573));
#211710=CARTESIAN_POINT('Ctrl Pts',(19.1186546369411,21.8593752306623,19.4137283924114));
#211711=CARTESIAN_POINT('Ctrl Pts',(21.1690707190565,20.3210816226097,19.5409041990928));
#211712=CARTESIAN_POINT('Ctrl Pts',(20.985460555994,17.7643569779692,19.6680800057743));
#211713=CARTESIAN_POINT('Ctrl Pts',(18.7362750703113,16.5348376083611,19.7952558124557));
#211714=CARTESIAN_POINT('Ctrl Pts',(16.485002356336,17.7605309561315,19.9224316191372));
#211715=CARTESIAN_POINT('Ctrl Pts',(16.2970453774111,20.3169399637462,20.0496074258186));
#211716=CARTESIAN_POINT('Ctrl Pts',(18.3448430381436,21.8587170449558,20.1767832325));
#211717=CARTESIAN_POINT('Ctrl Pts',(20.7496680038194,20.9713793298171,20.3039590391814));
#211718=CARTESIAN_POINT('Ctrl Pts',(21.3052427860467,18.4690004195621,20.4311348458629));
#211719=CARTESIAN_POINT('Ctrl Pts',(19.5018617017747,16.6473647370611,20.5583106525443));
#211720=CARTESIAN_POINT('Ctrl Pts',(16.9940155496951,17.1776962986144,20.6854864592258));
#211721=CARTESIAN_POINT('Ctrl Pts',(16.0824963938076,19.5734751345466,20.8126622659072));
#211722=CARTESIAN_POINT('Ctrl Pts',(17.6035686543715,21.6366721369649,20.9398380725886));
#211723=CARTESIAN_POINT('Ctrl Pts',(20.1617387589333,21.4745298636412,21.0670138792701));
#211724=CARTESIAN_POINT('Ctrl Pts',(21.4100524732811,19.2356154114268,21.1941896859515));
#211725=CARTESIAN_POINT('Ctrl Pts',(20.2032439124044,16.9743568470362,21.3213654926329));
#211726=CARTESIAN_POINT('Ctrl Pts',(17.6485149693138,16.7646189462416,21.4485412993143));
#211727=CARTESIAN_POINT('Ctrl Pts',(16.0896130768821,18.8001717717257,21.5757171059958));
#211728=CARTESIAN_POINT('Ctrl Pts',(16.9568463925819,21.2109198309685,21.7028929126772));
#211729=CARTESIAN_POINT('Ctrl Pts',(19.4543557984586,21.7901974439036,21.8300687193587));
#211730=CARTESIAN_POINT('Ctrl Pts',(21.2916289180791,19.9962677069502,21.9572631838147));
#211731=CARTESIAN_POINT('Ctrl Pts',(20.950780931212,18.329818140889,22.0420657127103));
#211732=CARTESIAN_POINT('Ctrl Pts',(20.46517256435,17.753190813129,22.0844763060453));
#211733=CARTESIAN_POINT('Ctrl Pts',(18.1877584159729,17.169626909876,-0.257964236536771));
#211734=CARTESIAN_POINT('Ctrl Pts',(17.5080924658439,17.3514955780797,-0.215572300976293));
#211735=CARTESIAN_POINT('Ctrl Pts',(16.3565580788699,18.4445270382643,-0.130788429855337));
#211736=CARTESIAN_POINT('Ctrl Pts',(16.8032830855277,20.7997955194952,-0.00361262317390214));
#211737=CARTESIAN_POINT('Ctrl Pts',(19.0246114950703,21.6921208369499,0.123563183507532));
#211738=CARTESIAN_POINT('Ctrl Pts',(20.9776563527076,20.3108032181647,0.250738990188966));
#211739=CARTESIAN_POINT('Ctrl Pts',(20.8731456200936,17.9191326762732,0.377914796870401));
#211740=CARTESIAN_POINT('Ctrl Pts',(18.8056558236651,16.7133702056622,0.505090603551835));
#211741=CARTESIAN_POINT('Ctrl Pts',(16.6726575032154,17.7986649702659,0.632266410233269));
#211742=CARTESIAN_POINT('Ctrl Pts',(16.4306929893915,20.1798778580737,0.759442216914703));
#211743=CARTESIAN_POINT('Ctrl Pts',(18.301931964306,21.6721076877706,0.886618023596138));
#211744=CARTESIAN_POINT('Ctrl Pts',(20.5695342339997,20.9064746960381,1.01379383027758));
#211745=CARTESIAN_POINT('Ctrl Pts',(21.1531645367453,18.5853225798024,1.14096963695901));
#211746=CARTESIAN_POINT('Ctrl Pts',(19.5173528268034,16.8382043226231,1.26814544364044));
#211747=CARTESIAN_POINT('Ctrl Pts',(17.1628680334775,17.2679717387401,1.39532125032188));
#211748=CARTESIAN_POINT('Ctrl Pts',(16.2497969611534,19.4803506649187,1.52249705700331));
#211749=CARTESIAN_POINT('Ctrl Pts',(17.6158292056801,21.4456151650917,1.64967286368475));
#211750=CARTESIAN_POINT('Ctrl Pts',(20.0077131216202,21.3607599376264,1.77684867036618));
#211751=CARTESIAN_POINT('Ctrl Pts',(21.2310446313948,19.3036328825639,1.90402447704762));
#211752=CARTESIAN_POINT('Ctrl Pts',(20.1634925060559,17.1615211739047,2.03120028372905));
#211753=CARTESIAN_POINT('Ctrl Pts',(17.7844698188743,16.8996789447851,2.15837609041049));
#211754=CARTESIAN_POINT('Ctrl Pts',(16.2765820926419,18.7583303988802,2.28555189709192));
#211755=CARTESIAN_POINT('Ctrl Pts',(17.0232227955911,21.0322780788906,2.41272770377336));
#211756=CARTESIAN_POINT('Ctrl Pts',(19.3393953884592,21.6353161821242,2.53990351045478));
#211757=CARTESIAN_POINT('Ctrl Pts',(21.1001552938832,20.0141946482555,2.66707931713622));
#211758=CARTESIAN_POINT('Ctrl Pts',(20.6901145740129,17.6561918817021,2.79425512381766));
#211759=CARTESIAN_POINT('Ctrl Pts',(18.4854601443698,16.7246290587094,2.92143093049909));
#211760=CARTESIAN_POINT('Ctrl Pts',(16.5088256052511,18.0741572541683,3.04860673718052));
#211761=CARTESIAN_POINT('Ctrl Pts',(16.5736504638791,20.4666681077815,3.17578254386197));
#211762=CARTESIAN_POINT('Ctrl Pts',(18.6204619352431,21.7071814084352,3.30295835054339));
#211763=CARTESIAN_POINT('Ctrl Pts',(20.7714375341794,20.6576031971447,3.43013415722483));
#211764=CARTESIAN_POINT('Ctrl Pts',(21.0531906530764,18.2808563388961,3.55730996390626));
#211765=CARTESIAN_POINT('Ctrl Pts',(19.2072302930153,16.7574585584311,3.6844857705877));
#211766=CARTESIAN_POINT('Ctrl Pts',(16.9271105110797,17.4850327666767,3.81166157726913));
#211767=CARTESIAN_POINT('Ctrl Pts',(16.3046996870279,19.7960747858742,3.93883738395057));
#211768=CARTESIAN_POINT('Ctrl Pts',(17.911021120741,21.5703470028761,4.066013190632));
#211769=CARTESIAN_POINT('Ctrl Pts',(20.2723745963467,21.1800647823256,4.19318899731344));
#211770=CARTESIAN_POINT('Ctrl Pts',(21.2223648620988,18.9832878379367,4.32036480399487));
#211771=CARTESIAN_POINT('Ctrl Pts',(19.8894348122174,16.9954226688293,4.44754061067631));
#211772=CARTESIAN_POINT('Ctrl Pts',(17.4964650364985,17.0402121868336,4.57471641735773));
#211773=CARTESIAN_POINT('Ctrl Pts',(16.23885677971,19.0765647891309,4.70189222403917));
#211774=CARTESIAN_POINT('Ctrl Pts',(17.2703875614835,21.2362533534106,4.8290680307206));
#211775=CARTESIAN_POINT('Ctrl Pts',(19.6446919135629,21.5378976673356,4.95624383740204));
#211776=CARTESIAN_POINT('Ctrl Pts',(21.1834929588632,19.7047577950374,5.08341964408348));
#211777=CARTESIAN_POINT('Ctrl Pts',(20.4750362470855,17.4186257918574,5.21059545076491));
#211778=CARTESIAN_POINT('Ctrl Pts',(18.1692868395033,16.7768858773585,5.33777125744635));
#211779=CARTESIAN_POINT('Ctrl Pts',(16.3816267066251,18.3682945922223,5.46494706412778));
#211780=CARTESIAN_POINT('Ctrl Pts',(16.7521230656655,20.7328332145257,5.59212287080921));
#211781=CARTESIAN_POINT('Ctrl Pts',(18.9408685028023,21.7011843181237,5.71929867749065));
#211782=CARTESIAN_POINT('Ctrl Pts',(20.9398249283253,20.3849458681128,5.84647448417208));
#211783=CARTESIAN_POINT('Ctrl Pts',(20.9150738910453,17.9916849474066,5.97365029085351));
#211784=CARTESIAN_POINT('Ctrl Pts',(18.889322931444,16.7170699082275,6.10082609753496));
#211785=CARTESIAN_POINT('Ctrl Pts',(16.7210728226713,17.7304809374911,6.22800190421637));
#211786=CARTESIAN_POINT('Ctrl Pts',(16.3995584627467,20.1021763152302,6.35517771089783));
#211787=CARTESIAN_POINT('Ctrl Pts',(18.2197493214694,21.6562727363857,6.48235351757925));
#211788=CARTESIAN_POINT('Ctrl Pts',(20.5117332597471,20.96698319265,6.6095293242607));
#211789=CARTESIAN_POINT('Ctrl Pts',(21.1727572707768,18.6666880582664,6.73670513094212));
#211790=CARTESIAN_POINT('Ctrl Pts',(19.5963728522159,16.8657653466142,6.86388093762356));
#211791=CARTESIAN_POINT('Ctrl Pts',(17.2288148666425,17.2164498677646,6.99105674430498));
#211792=CARTESIAN_POINT('Ctrl Pts',(16.2421708185993,19.3970103394982,7.11823255098643));
#211793=CARTESIAN_POINT('Ctrl Pts',(17.5416253841297,21.406917869846,7.24540835766785));
#211794=CARTESIAN_POINT('Ctrl Pts',(19.935009652606,21.4022070486441,7.3725841643493));
#211795=CARTESIAN_POINT('Ctrl Pts',(21.2265421078823,19.3871997619589,7.49975997103072));
#211796=CARTESIAN_POINT('Ctrl Pts',(20.2313218837872,17.210540129867,7.62693577771217));
#211797=CARTESIAN_POINT('Ctrl Pts',(17.8624017655944,16.8691782660797,7.75411158439359));
#211798=CARTESIAN_POINT('Ctrl Pts',(16.2931189299813,18.676292493315,7.88128739107503));
#211799=CARTESIAN_POINT('Ctrl Pts',(16.9631929779452,20.9739676702432,8.00846319775646));
#211800=CARTESIAN_POINT('Ctrl Pts',(19.2578725599652,21.6542294318373,8.13563900443789));
#211801=CARTESIAN_POINT('Ctrl Pts',(21.0719315834152,20.0929798336416,8.26281481111933));
#211802=CARTESIAN_POINT('Ctrl Pts',(20.7410834874809,17.7225684799219,8.38999061780077));
#211803=CARTESIAN_POINT('Ctrl Pts',(18.5688608654335,16.7177006633949,8.5171664244822));
#211804=CARTESIAN_POINT('Ctrl Pts',(16.5481431496601,18.0002802365935,8.64434223116363));
#211805=CARTESIAN_POINT('Ctrl Pts',(16.5328134244968,20.3936200469742,8.77151803784506));
#211806=CARTESIAN_POINT('Ctrl Pts',(18.5369357613108,21.7019793659344,8.89869384452652));
#211807=CARTESIAN_POINT('Ctrl Pts',(20.721852305936,20.7250197242656,9.02586965120793));
#211808=CARTESIAN_POINT('Ctrl Pts',(21.0830377398936,18.3590409562453,9.15304545788938));
#211809=CARTESIAN_POINT('Ctrl Pts',(19.2891268452239,16.774681732328,9.2802212645708));
#211810=CARTESIAN_POINT('Ctrl Pts',(16.985921525119,17.4254933040343,9.40739707125225));
#211811=CARTESIAN_POINT('Ctrl Pts',(16.2864697077309,19.7143964482452,9.53457287793367));
#211812=CARTESIAN_POINT('Ctrl Pts',(17.8324750226373,21.5414645954985,9.66174868461511));
#211813=CARTESIAN_POINT('Ctrl Pts',(20.2055735493235,21.2304761213276,9.78892449129655));
#211814=CARTESIAN_POINT('Ctrl Pts',(21.2285946806605,19.0667436486627,9.91610029797797));
#211815=CARTESIAN_POINT('Ctrl Pts',(19.9629800244992,17.0353574247909,10.0432761046594));
#211816=CARTESIAN_POINT('Ctrl Pts',(17.5698524749629,16.999988228066,10.1704519113408));
#211817=CARTESIAN_POINT('Ctrl Pts',(16.2447580245038,18.9930851012233,10.2976277180222));
#211818=CARTESIAN_POINT('Ctrl Pts',(17.2033885867812,21.1861053686842,10.4248035247037));
#211819=CARTESIAN_POINT('Ctrl Pts',(19.5662601202284,21.567089049242,10.5519793313851));
#211820=CARTESIAN_POINT('Ctrl Pts',(21.1655846492548,19.786507262499,10.6791551380666));
#211821=CARTESIAN_POINT('Ctrl Pts',(20.534081183754,17.4779332824223,10.806330944748));
#211822=CARTESIAN_POINT('Ctrl Pts',(18.2511149577974,16.7593404494715,10.9335067514294));
#211823=CARTESIAN_POINT('Ctrl Pts',(16.4111657868359,18.2899930869776,11.0606825581108));
#211824=CARTESIAN_POINT('Ctrl Pts',(16.7022728351016,20.6656124030459,11.1878583647923));
#211825=CARTESIAN_POINT('Ctrl Pts',(18.8573634539519,21.7067151227473,11.3150341714737));
#211826=CARTESIAN_POINT('Ctrl Pts',(20.8992757606008,20.4581541188783,11.4422099781552));
#211827=CARTESIAN_POINT('Ctrl Pts',(20.9546819490687,18.065406618053,11.5693857848366));
#211828=CARTESIAN_POINT('Ctrl Pts',(18.9727502803322,16.7236699416198,11.696561591518));
#211829=CARTESIAN_POINT('Ctrl Pts',(16.7717800479045,17.663904212636,11.8237373981994));
#211830=CARTESIAN_POINT('Ctrl Pts',(16.371024832419,20.0235028449647,11.9509132048809));
#211831=CARTESIAN_POINT('Ctrl Pts',(18.1381526704095,21.6376805466522,12.0780890115623));
#211832=CARTESIAN_POINT('Ctrl Pts',(20.4519334508432,21.0255294635675,12.2052648182438));
#211833=CARTESIAN_POINT('Ctrl Pts',(21.1896169171035,18.7486602200595,12.3324406249252));
#211834=CARTESIAN_POINT('Ctrl Pts',(19.6744242746961,16.8959590286039,12.4596164316066));
#211835=CARTESIAN_POINT('Ctrl Pts',(17.2964507295683,17.1671642407565,12.5867922382881));
#211836=CARTESIAN_POINT('Ctrl Pts',(16.2373394156911,19.3134619072614,12.7139680449695));
#211837=CARTESIAN_POINT('Ctrl Pts',(17.4687592276853,21.365757133357,12.8411438516509));
#211838=CARTESIAN_POINT('Ctrl Pts',(19.8609589185792,21.4411964289083,12.9683196583324));
#211839=CARTESIAN_POINT('Ctrl Pts',(21.2192437486358,19.4705689225376,13.0954954650138));
#211840=CARTESIAN_POINT('Ctrl Pts',(20.2974716909424,17.2618030404029,13.2226712716952));
#211841=CARTESIAN_POINT('Ctrl Pts',(17.9413113968065,16.8413043878911,13.3498470783767));
#211842=CARTESIAN_POINT('Ctrl Pts',(16.3123936962972,18.5948543795921,13.4770228850581));
#211843=CARTESIAN_POINT('Ctrl Pts',(16.9051494775971,20.9136797357071,13.6041986917395));
#211844=CARTESIAN_POINT('Ctrl Pts',(19.1757621019364,21.6704021145338,13.731374498421));
#211845=CARTESIAN_POINT('Ctrl Pts',(21.0410854165974,20.1707757009864,13.8585503051024));
#211846=CARTESIAN_POINT('Ctrl Pts',(20.7898010554004,17.7906146521824,13.9857261117838));
#211847=CARTESIAN_POINT('Ctrl Pts',(18.6524468232773,16.7135690009438,14.1129019184653));
#211848=CARTESIAN_POINT('Ctrl Pts',(16.5899125690362,17.9277612832899,14.2400777251467));
#211849=CARTESIAN_POINT('Ctrl Pts',(16.4944454556301,20.3192454414403,14.3672535318281));
#211850=CARTESIAN_POINT('Ctrl Pts',(18.4536306342518,21.6939831925389,14.4944293385096));
#211851=CARTESIAN_POINT('Ctrl Pts',(20.670037304262,20.7907379758005,14.621605145191));
#211852=CARTESIAN_POINT('Ctrl Pts',(21.1102499116389,18.438181215862,14.7487809518724));
#211853=CARTESIAN_POINT('Ctrl Pts',(19.37040071179,16.7946377238266,14.8759567585539));
#211854=CARTESIAN_POINT('Ctrl Pts',(17.0466933583566,17.3679566438234,15.0031325652353));
#211855=CARTESIAN_POINT('Ctrl Pts',(16.27098512257,19.6321534509405,15.1303083719167));
#211856=CARTESIAN_POINT('Ctrl Pts',(17.7549401648813,21.5099681065509,15.2574841785982));
#211857=CARTESIAN_POINT('Ctrl Pts',(20.1371218386074,21.278622214454,15.3846599852796));
#211858=CARTESIAN_POINT('Ctrl Pts',(21.2320263129741,19.1503612717033,15.5118357919611));
#211859=CARTESIAN_POINT('Ctrl Pts',(20.0351466901858,17.0777325985008,15.6390115986425));
#211860=CARTESIAN_POINT('Ctrl Pts',(17.6445457374235,16.9622443606664,15.7661874053239));
#211861=CARTESIAN_POINT('Ctrl Pts',(16.2534514514175,18.9098498484046,15.8933632120053));
#211862=CARTESIAN_POINT('Ctrl Pts',(17.1381064985295,21.1337419087451,16.0205390186868));
#211863=CARTESIAN_POINT('Ctrl Pts',(19.4868947809189,21.5936376066338,16.1477148253682));
#211864=CARTESIAN_POINT('Ctrl Pts',(21.1449488317356,19.8676111836039,16.2748906320497));
#211865=CARTESIAN_POINT('Ctrl Pts',(20.5911069697954,17.5391847535037,16.4020664387311));
#211866=CARTESIAN_POINT('Ctrl Pts',(18.3334847281261,16.7445450475071,16.5292422454125));
#211867=CARTESIAN_POINT('Ctrl Pts',(16.4433103896197,18.2127246749636,16.656418052094));
#211868=CARTESIAN_POINT('Ctrl Pts',(16.6547015924054,20.5967599531865,16.7835938587754));
#211869=CARTESIAN_POINT('Ctrl Pts',(18.7737200283452,21.7094464843237,16.9107696654568));
#211870=CARTESIAN_POINT('Ctrl Pts',(20.8562978035812,20.5299634371713,17.0379454721383));
#211871=CARTESIAN_POINT('Ctrl Pts',(20.9917990686889,18.140413300518,17.1651212788197));
#211872=CARTESIAN_POINT('Ctrl Pts',(19.0559098230889,16.7330600125345,17.2922970855011));
#211873=CARTESIAN_POINT('Ctrl Pts',(16.8246882947818,17.5990628647505,17.4194728921826));
#211874=CARTESIAN_POINT('Ctrl Pts',(16.3451417507631,19.9439179904547,17.546648698864));
#211875=CARTESIAN_POINT('Ctrl Pts',(18.0572243811545,21.6163663499399,17.6738245055454));
#211876=CARTESIAN_POINT('Ctrl Pts',(20.3902066364046,21.0820403772236,17.8010003122269));
#211877=CARTESIAN_POINT('Ctrl Pts',(21.2037220985302,18.8311509882762,17.9281761189083));
#211878=CARTESIAN_POINT('Ctrl Pts',(19.7514208234961,16.92874949148,18.0553519255897));
#211879=CARTESIAN_POINT('Ctrl Pts',(17.3656990911611,17.1201711838414,18.1825277322712));
#211880=CARTESIAN_POINT('Ctrl Pts',(16.2353085163561,19.229798543494,18.3097035389526));
#211881=CARTESIAN_POINT('Ctrl Pts',(17.3973122915052,21.3221794063805,18.4368793456341));
#211882=CARTESIAN_POINT('Ctrl Pts',(19.7856440750124,21.4776841982527,18.5640551523154));
#211883=CARTESIAN_POINT('Ctrl Pts',(21.2091576920692,19.5536469249632,18.6912309589969));
#211884=CARTESIAN_POINT('Ctrl Pts',(20.3618677523014,17.3152523642247,18.8184067656783));
#211885=CARTESIAN_POINT('Ctrl Pts',(18.0211101865936,16.8160885976028,18.9455825723598));
#211886=CARTESIAN_POINT('Ctrl Pts',(16.3343847778911,18.5141073945138,19.0727583790412));
#211887=CARTESIAN_POINT('Ctrl Pts',(16.849157398292,20.8514819090936,19.1999341857227));
#211888=CARTESIAN_POINT('Ctrl Pts',(19.093156119743,21.6838160799832,19.327109992404));
#211889=CARTESIAN_POINT('Ctrl Pts',(21.0076513920927,20.2474950006713,19.4542857990855));
#211890=CARTESIAN_POINT('Ctrl Pts',(20.8362126328065,17.8602540462332,19.5814616057669));
#211891=CARTESIAN_POINT('Ctrl Pts',(18.7361242573121,16.7122387526989,19.7086374124484));
#211892=CARTESIAN_POINT('Ctrl Pts',(16.6340870145935,17.8566816490089,19.8358132191298));
#211893=CARTESIAN_POINT('Ctrl Pts',(16.4585895871711,20.243627889804,19.9629890258113));
#211894=CARTESIAN_POINT('Ctrl Pts',(18.3706400116666,21.6832015249988,20.0901648324927));
#211895=CARTESIAN_POINT('Ctrl Pts',(20.6160506226023,20.8546848763886,20.2173406391741));
#211896=CARTESIAN_POINT('Ctrl Pts',(21.1347966972592,18.518187111326,20.3445164458556));
#211897=CARTESIAN_POINT('Ctrl Pts',(19.4509606260352,16.8173065278623,20.471692252537));
#211898=CARTESIAN_POINT('Ctrl Pts',(17.1093580392161,17.31248273928,20.5988680592184));
#211899=CARTESIAN_POINT('Ctrl Pts',(16.2582629225594,19.5494468827994,20.7260438658998));
#211900=CARTESIAN_POINT('Ctrl Pts',(17.6785042468215,21.475875836176,20.8532196725813));
#211901=CARTESIAN_POINT('Ctrl Pts',(20.0670948425395,21.324481873539,20.9803954792627));
#211902=CARTESIAN_POINT('Ctrl Pts',(21.2326586153631,19.2339836710777,21.1075712859442));
#211903=CARTESIAN_POINT('Ctrl Pts',(20.1058486451417,17.1226225337713,21.2347470926256));
#211904=CARTESIAN_POINT('Ctrl Pts',(17.7204710984363,16.9267880282744,21.361922899307));
#211905=CARTESIAN_POINT('Ctrl Pts',(16.2649078451288,18.8274053200522,21.4890987059885));
#211906=CARTESIAN_POINT('Ctrl Pts',(17.0746528024638,21.0783463863576,21.6162745126699));
#211907=CARTESIAN_POINT('Ctrl Pts',(19.4066038595716,21.6192240457828,21.7434503193513));
#211908=CARTESIAN_POINT('Ctrl Pts',(21.1220852841517,19.9442127979284,21.8706447838074));
#211909=CARTESIAN_POINT('Ctrl Pts',(20.803831898832,18.3882311395412,21.955447312703));
#211910=CARTESIAN_POINT('Ctrl Pts',(20.3504142092811,17.8498280795315,21.997857906038));
#211911=CARTESIAN_POINT('Ctrl Pts',(18.0722627314315,16.7380050975816,-1.38821246165044E-15));
#211912=CARTESIAN_POINT('Ctrl Pts',(17.9906109534297,16.7675693131061,3.14657425492808E-14));
#211913=CARTESIAN_POINT('Ctrl Pts',(17.9108508876399,16.801533969706,-6.59917533869226E-15));
#211914=CARTESIAN_POINT('Ctrl Pts',(17.833184560489,16.8395812357412,-8.91647866652079E-16));
#211915=CARTESIAN_POINT('Ctrl Pts',(17.753672918109,16.878532486837,4.95148776083561E-15));
#211916=CARTESIAN_POINT('Ctrl Pts',(17.6763549684744,16.9217633043155,1.81124826743322E-14));
#211917=CARTESIAN_POINT('Ctrl Pts',(17.6014769244535,16.9689790985685,1.02903796594944E-14));
#211918=CARTESIAN_POINT('Ctrl Pts',(17.5314114952628,17.0131602057565,2.97102440556189E-15));
#211919=CARTESIAN_POINT('Ctrl Pts',(17.4634822740683,17.0608314720463,-1.12028222644949E-14));
#211920=CARTESIAN_POINT('Ctrl Pts',(17.3979218193959,17.1117790406503,-1.23859256184744E-14));
#211921=CARTESIAN_POINT('Ctrl Pts',(17.3682534093495,17.1348346061396,-1.26972994741572E-14));
#211922=CARTESIAN_POINT('Ctrl Pts',(17.3390705414607,17.1585614233309,-2.36992619559033E-14));
#211923=CARTESIAN_POINT('Ctrl Pts',(17.310397157226,17.1829409553506,-2.57363574895919E-14));
#211924=CARTESIAN_POINT('Ctrl Pts',(17.2926919353297,17.1979948122865,-2.73746264744599E-14));
#211925=CARTESIAN_POINT('Ctrl Pts',(17.27518100039,17.2132975506653,-1.30461038077809E-14));
#211926=CARTESIAN_POINT('Ctrl Pts',(17.257870302469,17.2288449191993,8.43075609324728E-15));
#211927=CARTESIAN_POINT('Ctrl Pts',(17.2457082697189,17.239768083947,2.37421180105107E-14));
#211928=CARTESIAN_POINT('Ctrl Pts',(17.2336433007629,17.2508137998582,1.24222163529167E-14));
#211929=CARTESIAN_POINT('Ctrl Pts',(17.2216943574194,17.2619645032884,7.13318293321663E-15));
#211930=CARTESIAN_POINT('Ctrl Pts',(17.1582625823413,17.3211587677194,-2.04006785318585E-14));
#211931=CARTESIAN_POINT('Ctrl Pts',(17.0979931462804,17.3834003799274,-7.07776241633133E-15));
#211932=CARTESIAN_POINT('Ctrl Pts',(17.041116608508,17.4484111431914,-9.93649607039515E-15));
#211933=CARTESIAN_POINT('Ctrl Pts',(16.9849624648484,17.5125961987999,-1.27589206866276E-14));
#211934=CARTESIAN_POINT('Ctrl Pts',(16.9321151284134,17.5794813469652,-1.13917247600207E-14));
#211935=CARTESIAN_POINT('Ctrl Pts',(16.8828390026439,17.6488249957205,-1.36696209906972E-14));
#211936=CARTESIAN_POINT('Ctrl Pts',(16.8374017786414,17.7127663639275,-1.57700556265627E-14));
#211937=CARTESIAN_POINT('Ctrl Pts',(16.7950011366575,17.7787988087824,4.9988445844417E-15));
#211938=CARTESIAN_POINT('Ctrl Pts',(16.7558820673411,17.8467441370846,-6.6197047843275E-15));
#211939=CARTESIAN_POINT('Ctrl Pts',(16.7395100185488,17.8751805045547,-1.13588888870035E-14));
#211940=CARTESIAN_POINT('Ctrl Pts',(16.723713229623,17.903952012734,1.05054445318429E-15));
#211941=CARTESIAN_POINT('Ctrl Pts',(16.7085117731593,17.9330458325382,-3.71924713249427E-15));
#211942=CARTESIAN_POINT('Ctrl Pts',(16.6986550833365,17.9519103905663,-6.78822109791206E-15));
#211943=CARTESIAN_POINT('Ctrl Pts',(16.6890487140929,17.9709104592438,-1.73998603743695E-14));
#211944=CARTESIAN_POINT('Ctrl Pts',(16.6796984374459,17.9900425446149,-6.07847105982273E-15));
#211945=CARTESIAN_POINT('Ctrl Pts',(16.6737724856049,18.0021679416281,5.77327818760497E-16));
#211946=CARTESIAN_POINT('Ctrl Pts',(16.6679532270762,18.0143385914813,-2.27240940409281E-16));
#211947=CARTESIAN_POINT('Ctrl Pts',(16.6622433304787,18.0265499321002,-2.60902410786912E-15));
#211948=CARTESIAN_POINT('Ctrl Pts',(16.6271177976284,18.1016703548131,-1.76610440863303E-14));
#211949=CARTESIAN_POINT('Ctrl Pts',(16.5961057017263,18.1783725156421,1.14199974843153E-14));
#211950=CARTESIAN_POINT('Ctrl Pts',(16.5694538401813,18.2564278430498,-4.413136522885E-15));
#211951=CARTESIAN_POINT('Ctrl Pts',(16.5428019786364,18.3344831704575,-2.02462705300853E-14));
#211952=CARTESIAN_POINT('Ctrl Pts',(16.5205098793409,18.4138923942319,-1.04020717721636E-14));
#211953=CARTESIAN_POINT('Ctrl Pts',(16.5028786483266,18.4944362051925,-9.4091401336982E-15));
#211954=CARTESIAN_POINT('Ctrl Pts',(16.4850464602744,18.5758980374565,-8.6237439592604E-15));
#211955=CARTESIAN_POINT('Ctrl Pts',(16.4719827280125,18.6585216956155,2.62324771514716E-14));
#211956=CARTESIAN_POINT('Ctrl Pts',(16.4636117053936,18.7419152200439,1.9373391779709E-14));
#211957=CARTESIAN_POINT('Ctrl Pts',(16.4601585345833,18.7763162839797,1.65439174766097E-14));
#211958=CARTESIAN_POINT('Ctrl Pts',(16.4575045102803,18.8108481987005,1.22831063379818E-14));
#211959=CARTESIAN_POINT('Ctrl Pts',(16.4556467292437,18.845482524778,3.83026943495679E-15));
#211960=CARTESIAN_POINT('Ctrl Pts',(16.454914769638,18.859128335107,7.25867713128221E-16));
#211961=CARTESIAN_POINT('Ctrl Pts',(16.4543064277075,18.8727920340357,1.66417253216955E-14));
#211962=CARTESIAN_POINT('Ctrl Pts',(16.4538219965805,18.8864542247022,1.65978342181461E-14));
#211963=CARTESIAN_POINT('Ctrl Pts',(16.4509322011605,18.9679538101119,1.63150992925569E-14));
#211964=CARTESIAN_POINT('Ctrl Pts',(16.4524389841394,19.0495303086149,-1.1559845979381E-14));
#211965=CARTESIAN_POINT('Ctrl Pts',(16.458209072107,19.1308246613079,-1.14352971536391E-14));
#211966=CARTESIAN_POINT('Ctrl Pts',(16.4640075078912,19.2125184043422,-1.13101364330193E-14));
#211967=CARTESIAN_POINT('Ctrl Pts',(16.4741116098947,19.2939282562812,4.47511337812399E-16));
#211968=CARTESIAN_POINT('Ctrl Pts',(16.488437388537,19.3746780989798,9.6034291630076E-15));
#211969=CARTESIAN_POINT('Ctrl Pts',(16.5025242207701,19.4540810770198,1.86066311224743E-14));
#211970=CARTESIAN_POINT('Ctrl Pts',(16.5206935647305,19.5328467549076,-9.24683669832954E-15));
#211971=CARTESIAN_POINT('Ctrl Pts',(16.5429083611786,19.6105921329423,-6.10622663543836E-15));
#211972=CARTESIAN_POINT('Ctrl Pts',(16.5522119867793,19.6431521382123,-4.79092940769646E-15));
#211973=CARTESIAN_POINT('Ctrl Pts',(16.5622256486959,19.6755328027629,-3.85337688317397E-15));
#211974=CARTESIAN_POINT('Ctrl Pts',(16.5729486044555,19.7077040845634,-4.63518112781003E-15));
#211975=CARTESIAN_POINT('Ctrl Pts',(16.5784892728338,19.7243273373082,-5.02631740729074E-15));
#211976=CARTESIAN_POINT('Ctrl Pts',(16.5842201982241,19.7408967187103,7.50369055471448E-15));
#211977=CARTESIAN_POINT('Ctrl Pts',(16.59013339505,19.757386717525,3.58046925441613E-15));
#211978=CARTESIAN_POINT('Ctrl Pts',(16.6171691937068,19.8327808403536,-1.42609449952302E-14));
#211979=CARTESIAN_POINT('Ctrl Pts',(16.6480432448069,19.9066161661436,-5.97332593345049E-15));
#211980=CARTESIAN_POINT('Ctrl Pts',(16.6826949054327,19.9785209088995,4.21884749357559E-15));
#211981=CARTESIAN_POINT('Ctrl Pts',(16.708683650902,20.0324494659664,1.17631662849405E-14));
#211982=CARTESIAN_POINT('Ctrl Pts',(16.7367982565916,20.085291634914,-2.01726906480219E-14));
#211983=CARTESIAN_POINT('Ctrl Pts',(16.7670276708943,20.1368764988564,-7.7715611723761E-15));
#211984=CARTESIAN_POINT('Ctrl Pts',(16.776261941294,20.1526342828943,-4.1977974750146E-15));
#211985=CARTESIAN_POINT('Ctrl Pts',(16.7856936339531,20.1682746431805,1.04387754400567E-14));
#211986=CARTESIAN_POINT('Ctrl Pts',(16.7953226427023,20.1837924294014,1.13797860024079E-15));
#211987=CARTESIAN_POINT('Ctrl Pts',(16.803547563051,20.1970474340419,-6.69839811468132E-15));
#211988=CARTESIAN_POINT('Ctrl Pts',(16.8119141832479,20.2102092393014,2.41113709074752E-14));
#211989=CARTESIAN_POINT('Ctrl Pts',(16.8204178931759,20.2232683327282,1.87905246917808E-14));
#211990=CARTESIAN_POINT('Ctrl Pts',(16.8615694216389,20.2864644741072,-6.83040447856231E-15));
#211991=CARTESIAN_POINT('Ctrl Pts',(16.9059580723631,20.3473056667748,-2.18788826067377E-15));
#211992=CARTESIAN_POINT('Ctrl Pts',(16.9535504700224,20.4054521814502,4.52415882534751E-15));
#211993=CARTESIAN_POINT('Ctrl Pts',(16.997682676699,20.459371171234,1.18644907122736E-14));
#211994=CARTESIAN_POINT('Ctrl Pts',(17.0445702571952,20.51097318916,3.05264786508281E-14));
#211995=CARTESIAN_POINT('Ctrl Pts',(17.0942091691994,20.55995417271,1.27675647831893E-14));
#211996=CARTESIAN_POINT('Ctrl Pts',(17.0997977295932,20.5654686607127,1.06142302750383E-14));
#211997=CARTESIAN_POINT('Ctrl Pts',(17.1054211843278,20.5709498884042,1.6560443839516E-15));
#211998=CARTESIAN_POINT('Ctrl Pts',(17.1110791648801,20.5763977067475,3.95239396766556E-14));
#211999=CARTESIAN_POINT('Ctrl Pts',(20.3504145393176,-17.5908279157877,
0.00214189257971319));
#212000=CARTESIAN_POINT('Ctrl Pts',(20.8038322616566,-18.1292310654914,
0.0445524841607406));
#212001=CARTESIAN_POINT('Ctrl Pts',(21.1220877448274,-19.685210814566,0.129355011302246));
#212002=CARTESIAN_POINT('Ctrl Pts',(19.4066026967562,-21.3602255324577,
0.25654947400423));
#212003=CARTESIAN_POINT('Ctrl Pts',(17.0746532893504,-20.819345744412,0.383725280685664));
#212004=CARTESIAN_POINT('Ctrl Pts',(16.264907281043,-18.5684058059804,0.510901087367099));
#212005=CARTESIAN_POINT('Ctrl Pts',(17.7204711810805,-16.6677874925037,
0.638076894048533));
#212006=CARTESIAN_POINT('Ctrl Pts',(20.105848679288,-16.8636225373773,0.765252700729967));
#212007=CARTESIAN_POINT('Ctrl Pts',(21.2326588952387,-18.9749835563125,
0.892428507411401));
#212008=CARTESIAN_POINT('Ctrl Pts',(20.0670949402048,-21.0654821373604,
1.01960431409284));
#212009=CARTESIAN_POINT('Ctrl Pts',(17.678504162672,-21.2168760062151,1.14678012077427));
#212010=CARTESIAN_POINT('Ctrl Pts',(16.2582626864848,-19.2904469366441,
1.2739559274557));
#212011=CARTESIAN_POINT('Ctrl Pts',(17.1093578926688,-17.0534825509078,
1.40113173413714));
#212012=CARTESIAN_POINT('Ctrl Pts',(19.4509606903938,-16.5583063136444,
1.52830754081857));
#212013=CARTESIAN_POINT('Ctrl Pts',(21.1347969203461,-18.2591870432273,
1.65548334750001));
#212014=CARTESIAN_POINT('Ctrl Pts',(20.6160507961411,-20.5956850306546,
1.78265915418144));
#212015=CARTESIAN_POINT('Ctrl Pts',(18.3706399783416,-21.4242017524251,
1.90983496086288));
#212016=CARTESIAN_POINT('Ctrl Pts',(16.4585893765604,-19.9846279859987,
2.03701076754431));
#212017=CARTESIAN_POINT('Ctrl Pts',(16.6340868204421,-17.5976815233674,
2.16418657422575));
#212018=CARTESIAN_POINT('Ctrl Pts',(18.7361242574674,-16.453238521784,2.29136238090717));
#212019=CARTESIAN_POINT('Ctrl Pts',(20.8362128272701,-17.6012539211848,
2.41853818758862));
#212020=CARTESIAN_POINT('Ctrl Pts',(21.0076516023807,-19.9884950966021,
2.54571399427004));
#212021=CARTESIAN_POINT('Ctrl Pts',(19.0931561529689,-21.4248163086708,
2.67288980095148));
#212022=CARTESIAN_POINT('Ctrl Pts',(16.8491572239522,-20.5924820608467,
2.80006560763291));
#212023=CARTESIAN_POINT('Ctrl Pts',(16.3343845559425,-18.2551073300457,
2.92724141431435));
#212024=CARTESIAN_POINT('Ctrl Pts',(18.0211101206545,-16.557088376093,3.05441722099578));
#212025=CARTESIAN_POINT('Ctrl Pts',(20.3618679028699,-17.0562521888763,
3.18159302767722));
#212026=CARTESIAN_POINT('Ctrl Pts',(21.2091579210064,-19.2946469566574,
3.30876883435865));
#212027=CARTESIAN_POINT('Ctrl Pts',(19.7856441722836,-21.2186844079067,
3.43594464104009));
#212028=CARTESIAN_POINT('Ctrl Pts',(17.3973121678696,-21.0631796016525,
3.56312044772152));
#212029=CARTESIAN_POINT('Ctrl Pts',(16.2353082852419,-18.9707985452326,
3.69029625440296));
#212030=CARTESIAN_POINT('Ctrl Pts',(17.3656989646013,-16.8611709904523,
3.81747206108439));
#212031=CARTESIAN_POINT('Ctrl Pts',(19.7514209176014,-16.6697492803852,
3.94464786776582));
#212032=CARTESIAN_POINT('Ctrl Pts',(21.2037223269647,-18.5721509531424,
4.07182367444726));
#212033=CARTESIAN_POINT('Ctrl Pts',(20.390206789594,-20.8230405502836,4.19899948112869));
#212034=CARTESIAN_POINT('Ctrl Pts',(18.0572243185569,-21.357366572422,4.32617528781012));
#212035=CARTESIAN_POINT('Ctrl Pts',(16.3451415298078,-19.6849180582454,
4.45335109449157));
#212036=CARTESIAN_POINT('Ctrl Pts',(16.8246881181817,-17.340062715656,4.58052690117299));
#212037=CARTESIAN_POINT('Ctrl Pts',(19.0559098528636,-16.4740597833398,
4.70770270785444));
#212038=CARTESIAN_POINT('Ctrl Pts',(20.9917992775219,-17.8814132014949,
4.83487851453586));
#212039=CARTESIAN_POINT('Ctrl Pts',(20.8562979998813,-20.2709635591674,
4.9620543212173));
#212040=CARTESIAN_POINT('Ctrl Pts',(18.7737200320192,-21.4504467154151,
5.08923012789874));
#212041=CARTESIAN_POINT('Ctrl Pts',(16.6547014000827,-20.3377600813612,
5.21640593458017));
#212042=CARTESIAN_POINT('Ctrl Pts',(16.4433101777445,-17.9537245826292,
5.34358174126161));
#212043=CARTESIAN_POINT('Ctrl Pts',(18.3334846910807,-16.4855448193747,
5.47075754794303));
#212044=CARTESIAN_POINT('Ctrl Pts',(20.5911071415668,-17.2801845988706,
5.59793335462448));
#212045=CARTESIAN_POINT('Ctrl Pts',(21.144949054734,-19.6086112443364,5.7251091613059));
#212046=CARTESIAN_POINT('Ctrl Pts',(19.4868948505574,-21.3346378270135,
5.85228496798734));
#212047=CARTESIAN_POINT('Ctrl Pts',(17.1381063509189,-20.8747420865874,
5.97946077466877));
#212048=CARTESIAN_POINT('Ctrl Pts',(16.2534512219814,-18.6508498205501,
6.10663658135021));
#212049=CARTESIAN_POINT('Ctrl Pts',(17.6445456366553,-16.7032441526699,
6.23381238803165));
#212050=CARTESIAN_POINT('Ctrl Pts',(20.0351468105341,-16.8187324011862,
6.36098819471307));
#212051=CARTESIAN_POINT('Ctrl Pts',(21.2320265440266,-18.8913612660945,
6.48816400139451));
#212052=CARTESIAN_POINT('Ctrl Pts',(20.137121968388,-21.0196224056966,6.61533980807595));
#212053=CARTESIAN_POINT('Ctrl Pts',(17.7549400743242,-21.2509683191918,
6.74251561475738));
#212054=CARTESIAN_POINT('Ctrl Pts',(16.2709848947557,-19.3731534898947,
6.86969142143882));
#212055=CARTESIAN_POINT('Ctrl Pts',(17.0466932022907,-17.1089564733528,
6.99686722812024));
#212056=CARTESIAN_POINT('Ctrl Pts',(19.3704007706532,-16.5356375003274,
7.12404303480169));
#212057=CARTESIAN_POINT('Ctrl Pts',(21.1102501314279,-18.1791811443807,
7.25121884148312));
#212058=CARTESIAN_POINT('Ctrl Pts',(20.6700374833341,-20.5317381219169,
7.37839464816456));
#212059=CARTESIAN_POINT('Ctrl Pts',(18.4536306083194,-21.4349834222001,
7.50557045484598));
#212060=CARTESIAN_POINT('Ctrl Pts',(16.4944452484847,-20.0602455439464,
7.63274626152742));
#212061=CARTESIAN_POINT('Ctrl Pts',(16.5899123707208,-17.668761164598,7.75992206820886));
#212062=CARTESIAN_POINT('Ctrl Pts',(18.652446815734,-16.4545687699462,7.88709787489029));
#212063=CARTESIAN_POINT('Ctrl Pts',(20.7898012455497,-17.531614520805,8.01427368157173));
#212064=CARTESIAN_POINT('Ctrl Pts',(21.0410856299891,-19.9117757897599,
8.14144948825315));
#212065=CARTESIAN_POINT('Ctrl Pts',(19.175762142797,-21.4114023420139,8.2686252949346));
#212066=CARTESIAN_POINT('Ctrl Pts',(16.9051493084394,-20.6546798931949,
8.39580110161602));
#212067=CARTESIAN_POINT('Ctrl Pts',(16.312393472313,-18.3358543226023,8.52297690829747));
#212068=CARTESIAN_POINT('Ctrl Pts',(17.9413113234874,-16.5823041687085,
8.65015271497889));
#212069=CARTESIAN_POINT('Ctrl Pts',(20.2974718355542,-17.0028028601137,
8.77732852166035));
#212070=CARTESIAN_POINT('Ctrl Pts',(21.2192439785061,-19.2115689465461,
8.90450432834176));
#212071=CARTESIAN_POINT('Ctrl Pts',(19.8609590228163,-21.1821966351882,
9.0316801350232));
#212072=CARTESIAN_POINT('Ctrl Pts',(17.4687591106581,-21.1067573326593,
9.15885594170464));
#212073=CARTESIAN_POINT('Ctrl Pts',(16.2373391847649,-19.0544619167386,
9.28603174838607));
#212074=CARTESIAN_POINT('Ctrl Pts',(17.2964505966034,-16.908164051714,9.4132075550675));
#212075=CARTESIAN_POINT('Ctrl Pts',(19.6744243616797,-16.6369588144763,
9.54038336174894));
#212076=CARTESIAN_POINT('Ctrl Pts',(21.1896171442334,-18.4896601772957,
9.66755916843036));
#212077=CARTESIAN_POINT('Ctrl Pts',(20.4519336097419,-20.7665296314006,
9.79473497511182));
#212078=CARTESIAN_POINT('Ctrl Pts',(18.1381526152972,-21.3786807711059,
9.92191078179324));
#212079=CARTESIAN_POINT('Ctrl Pts',(16.3710246138578,-19.7645029201165,
10.0490865884747));
#212080=CARTESIAN_POINT('Ctrl Pts',(16.7717798664108,-17.4049040695389,
10.1762623951561));
#212081=CARTESIAN_POINT('Ctrl Pts',(18.9727503024152,-16.4646697115565,
10.3034382018376));
#212082=CARTESIAN_POINT('Ctrl Pts',(20.9546821544686,-17.8064065120923,
10.430614008519));
#212083=CARTESIAN_POINT('Ctrl Pts',(20.8992759608759,-20.1991542342326,
10.5577898152005));
#212084=CARTESIAN_POINT('Ctrl Pts',(18.8573634653625,-21.4477153535862,
10.6849656218819));
#212085=CARTESIAN_POINT('Ctrl Pts',(16.702272647179,-20.4066125375889,10.8121414285633));
#212086=CARTESIAN_POINT('Ctrl Pts',(16.4111655719875,-18.0309930017901,
10.9393172352448));
#212087=CARTESIAN_POINT('Ctrl Pts',(18.2511149131334,-16.5003402227076,
11.0664930419262));
#212088=CARTESIAN_POINT('Ctrl Pts',(20.5340813502507,-17.2189331221239,
11.1936688486076));
#212089=CARTESIAN_POINT('Ctrl Pts',(21.165584874162,-19.5275073157298,11.3208446552891));
#212090=CARTESIAN_POINT('Ctrl Pts',(19.5662601972076,-21.3080892671662,
11.4480204619705));
#212091=CARTESIAN_POINT('Ctrl Pts',(17.2033884452088,-20.9271055513698,
11.575196268652));
#212092=CARTESIAN_POINT('Ctrl Pts',(16.2447577942638,-18.7340850810675,
11.7023720753333));
#212093=CARTESIAN_POINT('Ctrl Pts',(17.5698523672862,-16.7409880235606,
11.8295478820148));
#212094=CARTESIAN_POINT('Ctrl Pts',(19.9629801381724,-16.7763572235568,
11.9567236886962));
#212095=CARTESIAN_POINT('Ctrl Pts',(21.2285949113957,-18.8077436353198,
12.0838994953777));
#212096=CARTESIAN_POINT('Ctrl Pts',(20.2055736854352,-20.9714763081171,
12.2110753020591));
#212097=CARTESIAN_POINT('Ctrl Pts',(17.8324749392518,-21.2824648110527,
12.3382511087405));
#212098=CARTESIAN_POINT('Ctrl Pts',(16.2864694813489,-19.4553964948066,
12.465426915422));
#212099=CARTESIAN_POINT('Ctrl Pts',(16.9859213634321,-17.1664931388855,
12.5926027221034));
#212100=CARTESIAN_POINT('Ctrl Pts',(19.2891268965698,-16.515681506983,12.7197785287849));
#212101=CARTESIAN_POINT('Ctrl Pts',(21.0830379571657,-18.100040877444,12.8469543354662));
#212102=CARTESIAN_POINT('Ctrl Pts',(20.7218524898006,-20.4660198643034,
12.9741301421477));
#212103=CARTESIAN_POINT('Ctrl Pts',(18.5369357430837,-21.4429795963352,
13.1013059488291));
#212104=CARTESIAN_POINT('Ctrl Pts',(16.5328132209002,-20.1346201563596,
13.2284817555106));
#212105=CARTESIAN_POINT('Ctrl Pts',(16.5481429474813,-17.7412801246093,
13.355657562192));
#212106=CARTESIAN_POINT('Ctrl Pts',(18.5688608501589,-16.4587004327796,
13.4828333688734));
#212107=CARTESIAN_POINT('Ctrl Pts',(20.7410836731242,-17.4635683422508,
13.6100091755549));
#212108=CARTESIAN_POINT('Ctrl Pts',(21.0719317996599,-19.8339799152194,
13.7371849822363));
#212109=CARTESIAN_POINT('Ctrl Pts',(19.2578726084204,-21.3952296578215,
13.8643607889177));
#212110=CARTESIAN_POINT('Ctrl Pts',(16.9631928141561,-20.7149678333072,
13.9915365955992));
#212111=CARTESIAN_POINT('Ctrl Pts',(16.2931187042143,-18.4172924438578,
14.1187124022806));
#212112=CARTESIAN_POINT('Ctrl Pts',(17.8624016849767,-16.6101780494751,
14.245888208962));
#212113=CARTESIAN_POINT('Ctrl Pts',(20.2313220222805,-16.9515399448363,
14.3730640156435));
#212114=CARTESIAN_POINT('Ctrl Pts',(21.2265423384276,-19.1281997782562,
14.5002398223249));
#212115=CARTESIAN_POINT('Ctrl Pts',(19.9350097636923,-21.1432072513177,
14.6274156290064));
#212116=CARTESIAN_POINT('Ctrl Pts',(17.5416252738421,-21.1479180729553,
14.7545914356878));
#212117=CARTESIAN_POINT('Ctrl Pts',(16.2421705881198,-19.1380103567032,
14.8817672423692));
#212118=CARTESIAN_POINT('Ctrl Pts',(17.2288147274218,-16.9574496832805,
15.0089430490507));
#212119=CARTESIAN_POINT('Ctrl Pts',(19.5963729319801,-16.6067651296939,
15.1361188557321));
#212120=CARTESIAN_POINT('Ctrl Pts',(21.1727574963474,-18.4076880079207,
15.2632946624135));
#212121=CARTESIAN_POINT('Ctrl Pts',(20.511733424177,-20.707983355068,15.3904704690949));
#212122=CARTESIAN_POINT('Ctrl Pts',(18.2197492739044,-21.397272962559,15.5176462757764));
#212123=CARTESIAN_POINT('Ctrl Pts',(16.3995582468247,-19.8431763976587,
15.6448220824578));
#212124=CARTESIAN_POINT('Ctrl Pts',(16.7210726364874,-17.471480800552,15.7719978891392));
#212125=CARTESIAN_POINT('Ctrl Pts',(18.8893229458104,-16.4580696775538,
15.8991736958207));
#212126=CARTESIAN_POINT('Ctrl Pts',(20.9150740927816,-17.732684834627,16.0263495025021));
#212127=CARTESIAN_POINT('Ctrl Pts',(20.939825132351,-20.1259459766957,16.1535253091836));
#212128=CARTESIAN_POINT('Ctrl Pts',(18.9408685219365,-21.4421845484509,
16.280701115865));
#212129=CARTESIAN_POINT('Ctrl Pts',(16.7521228823537,-20.4738333552863,
16.4078769225464));
#212130=CARTESIAN_POINT('Ctrl Pts',(16.3816264890446,-18.1092945142772,
16.5350527292279));
#212131=CARTESIAN_POINT('Ctrl Pts',(18.1692867872707,-16.5178856522175,
16.6622285359093));
#212132=CARTESIAN_POINT('Ctrl Pts',(20.475036408121,-17.1596256260734,16.7894043425907));
#212133=CARTESIAN_POINT('Ctrl Pts',(21.1834931854267,-19.445757840707,16.9165801492722));
#212134=CARTESIAN_POINT('Ctrl Pts',(19.6446919977966,-21.2788978825597,
17.0437559559536));
#212135=CARTESIAN_POINT('Ctrl Pts',(17.2703874261082,-20.9772535407345,
17.1709317626351));
#212136=CARTESIAN_POINT('Ctrl Pts',(16.2388565489241,-18.8175647766965,
17.2981075693165));
#212137=CARTESIAN_POINT('Ctrl Pts',(17.4964649220338,-16.7812119860487,
17.4252833759979));
#212138=CARTESIAN_POINT('Ctrl Pts',(19.8894349190882,-16.7364224639015,
17.5524591826793));
#212139=CARTESIAN_POINT('Ctrl Pts',(21.2223650922577,-18.7242878168747,
17.6796349893608));
#212140=CARTESIAN_POINT('Ctrl Pts',(20.2723747386373,-20.9210649644522,
17.8068107960422));
#212141=CARTESIAN_POINT('Ctrl Pts',(17.9110210446205,-21.3113472211018,
17.9339866027237));
#212142=CARTESIAN_POINT('Ctrl Pts',(16.3046994623321,-19.5370748399901,
18.061162409405));
#212143=CARTESIAN_POINT('Ctrl Pts',(16.9271103439532,-17.2260326070351,
18.1883382160865));
#212144=CARTESIAN_POINT('Ctrl Pts',(19.2072303367862,-16.498458331493,18.3155140227679));
#212145=CARTESIAN_POINT('Ctrl Pts',(21.0531908675876,-18.0218562528634,
18.4426898294494));
#212146=CARTESIAN_POINT('Ctrl Pts',(20.7714377226303,-20.3986033309466,
18.5698656361308));
#212147=CARTESIAN_POINT('Ctrl Pts',(18.6204619247414,-21.4481816393175,
18.6970414428122));
#212148=CARTESIAN_POINT('Ctrl Pts',(16.57365026406,-20.2076682239227,18.8242172494937));
#212149=CARTESIAN_POINT('Ctrl Pts',(16.508825399435,-17.8151571490185,18.9513930561751));
#212150=CARTESIAN_POINT('Ctrl Pts',(18.4854601213826,-16.4656288287323,
19.0785688628566));
#212151=CARTESIAN_POINT('Ctrl Pts',(20.6901147549395,-17.3971917378963,
19.205744669538));
#212152=CARTESIAN_POINT('Ctrl Pts',(21.1001555127428,-19.7551947225373,
19.3329204762194));
#212153=CARTESIAN_POINT('Ctrl Pts',(19.3393954444469,-21.3763164063757,
19.4600962829008));
#212154=CARTESIAN_POINT('Ctrl Pts',(17.0232226373686,-20.7732782473175,
19.5872720895823));
#212155=CARTESIAN_POINT('Ctrl Pts',(16.2765818653196,-18.4993303570677,
19.7144478962637));
#212156=CARTESIAN_POINT('Ctrl Pts',(17.784469731095,-16.6406787308973,19.8416237029452));
#212157=CARTESIAN_POINT('Ctrl Pts',(20.1634926381912,-16.9025209845322,
19.9687995096266));
#212158=CARTESIAN_POINT('Ctrl Pts',(21.2310448625075,-19.0446328907795,
20.095975316308));
#212159=CARTESIAN_POINT('Ctrl Pts',(20.0077132391621,-21.1017601371114,
20.2231511229895));
#212160=CARTESIAN_POINT('Ctrl Pts',(17.6158291027325,-21.1866153706034,
20.3503269296709));
#212161=CARTESIAN_POINT('Ctrl Pts',(16.2497967305417,-19.2213506919733,
20.4775027363524));
#212162=CARTESIAN_POINT('Ctrl Pts',(17.162867889616,-17.0089715551397,20.6046785430338));
#212163=CARTESIAN_POINT('Ctrl Pts',(19.517352896747,-16.5792041101632,20.7318543497152));
#212164=CARTESIAN_POINT('Ctrl Pts',(21.153164764767,-18.3263225093304,20.8590301563966));
#212165=CARTESIAN_POINT('Ctrl Pts',(20.5695343966718,-20.6474748753932,
20.9862059630781));
#212166=CARTESIAN_POINT('Ctrl Pts',(18.3019319358899,-21.4131078753525,
21.1133817697595));
#212167=CARTESIAN_POINT('Ctrl Pts',(16.4306927582234,-19.9208780183909,
21.2405575764409));
#212168=CARTESIAN_POINT('Ctrl Pts',(16.672657339533,-17.5396647158853,21.3677333831224));
#212169=CARTESIAN_POINT('Ctrl Pts',(18.8056557936095,-16.4543701890598,
21.4949091898038));
#212170=CARTESIAN_POINT('Ctrl Pts',(20.8731458592265,-17.6601321897591,
21.6220849964852));
#212171=CARTESIAN_POINT('Ctrl Pts',(20.9776565367662,-20.0518039395808,
21.7492608031667));
#212172=CARTESIAN_POINT('Ctrl Pts',(19.0246114636561,-21.4331200318623,
21.8764366098481));
#212173=CARTESIAN_POINT('Ctrl Pts',(16.8032831871667,-20.5407974041735,
22.0036124165295));
#212174=CARTESIAN_POINT('Ctrl Pts',(16.3565571918356,-18.1855239713029,
22.130788223211));
#212175=CARTESIAN_POINT('Ctrl Pts',(17.5080922582077,-17.0924952631291,
22.2155720943319));
#212176=CARTESIAN_POINT('Ctrl Pts',(18.187758323454,-16.9106265641217,22.2579640298924));
#212177=CARTESIAN_POINT('Ctrl Pts',(20.4651728847368,-17.4941906656173,
-0.084476497129225));
#212178=CARTESIAN_POINT('Ctrl Pts',(20.9507812774351,-18.0708180784204,
-0.0420659055481974));
#212179=CARTESIAN_POINT('Ctrl Pts',(21.2916315045783,-19.7372655677721,
0.0427366215933083));
#212180=CARTESIAN_POINT('Ctrl Pts',(19.454354539323,-21.53119898684,0.169931084295291));
#212181=CARTESIAN_POINT('Ctrl Pts',(16.9568469479949,-20.951919105231,0.297106890976727));
#212182=CARTESIAN_POINT('Ctrl Pts',(16.0896125232803,-18.5411723000033,
0.42428269765816));
#212183=CARTESIAN_POINT('Ctrl Pts',(17.648515078568,-16.5056184191814,0.551458504339596));
#212184=CARTESIAN_POINT('Ctrl Pts',(20.2032439208991,-16.7153568936381,
0.678634311021028));
#212185=CARTESIAN_POINT('Ctrl Pts',(21.41005272189,-18.9766152880434,0.805810117702464));
#212186=CARTESIAN_POINT('Ctrl Pts',(20.1617388362496,-21.2155301029391,
0.932985924383898));
#212187=CARTESIAN_POINT('Ctrl Pts',(17.6035685858491,-21.3776722727239,
1.06016173106533));
#212188=CARTESIAN_POINT('Ctrl Pts',(16.0824961916403,-19.3144751852875,
1.18733753774677));
#212189=CARTESIAN_POINT('Ctrl Pts',(16.9940154259929,-16.918696135723,1.3145133444282));
#212190=CARTESIAN_POINT('Ctrl Pts',(19.5018617560294,-16.3883645566231,
1.44168915110964));
#212191=CARTESIAN_POINT('Ctrl Pts',(21.3052429758379,-18.2100003608074,
1.56886495779107));
#212192=CARTESIAN_POINT('Ctrl Pts',(20.7496681511615,-20.7123794613962,
1.69604076447251));
#212193=CARTESIAN_POINT('Ctrl Pts',(18.344843009889,-21.599717237933,1.82321657115394));
#212194=CARTESIAN_POINT('Ctrl Pts',(16.2970451984157,-20.057940045637,1.95039237783538));
#212195=CARTESIAN_POINT('Ctrl Pts',(16.4850021913768,-17.5015308492868,
2.07756818451681));
#212196=CARTESIAN_POINT('Ctrl Pts',(18.7362750704342,-16.275837412191,2.20474399119824));
#212197=CARTESIAN_POINT('Ctrl Pts',(20.9854607212405,-17.5053568716867,
2.33191979787968));
#212198=CARTESIAN_POINT('Ctrl Pts',(21.1690708977422,-20.0620817041385,
2.45909560456111));
#212199=CARTESIAN_POINT('Ctrl Pts',(19.1186546651756,-21.6003754249779,
2.58627141124255));
#212200=CARTESIAN_POINT('Ctrl Pts',(16.7153416505994,-20.7089490947747,
2.71344721792398));
#212201=CARTESIAN_POINT('Ctrl Pts',(16.1640223800872,-18.2056310058767,
2.84062302460542));
#212202=CARTESIAN_POINT('Ctrl Pts',(17.9704980647556,-16.3870601508454,
2.96779883128685));
#212203=CARTESIAN_POINT('Ctrl Pts',(20.477439386886,-16.9216624058443,3.09497463796828));
#212204=CARTESIAN_POINT('Ctrl Pts',(21.3848832815229,-19.3189733883075,
3.22215044464972));
#212205=CARTESIAN_POINT('Ctrl Pts',(19.8603062977751,-21.3796090630069,
3.34932625133115));
#212206=CARTESIAN_POINT('Ctrl Pts',(17.3024131922505,-21.213064097291,3.47650205801259));
#212207=CARTESIAN_POINT('Ctrl Pts',(16.0579121285487,-18.9721331595253,
3.60367786469402));
#212208=CARTESIAN_POINT('Ctrl Pts',(17.2685555901523,-16.7127312976299,
3.73085367137545));
#212209=CARTESIAN_POINT('Ctrl Pts',(19.8236533420561,-16.5077194854014,
3.85802947805689));
#212210=CARTESIAN_POINT('Ctrl Pts',(21.3790617841357,-18.5451833361938,
3.98520528473832));
#212211=CARTESIAN_POINT('Ctrl Pts',(20.5077902103209,-20.9558762261203,
4.11238109141976));
#212212=CARTESIAN_POINT('Ctrl Pts',(18.009176212373,-21.5281370531764,4.23955689810119));
#212213=CARTESIAN_POINT('Ctrl Pts',(16.1755430519351,-19.7369520270363,
4.36673270478263));
#212214=CARTESIAN_POINT('Ctrl Pts',(16.6891353455996,-17.2256222357103,
4.49390851146406));
#212215=CARTESIAN_POINT('Ctrl Pts',(19.0787640410623,-16.2981368920303,
4.6210843181455));
#212216=CARTESIAN_POINT('Ctrl Pts',(21.15209312732,-17.805406232592,4.74826012482693));
#212217=CARTESIAN_POINT('Ctrl Pts',(21.0069718530473,-20.364604189115,4.87543593150836));
#212218=CARTESIAN_POINT('Ctrl Pts',(18.7765399801474,-21.6278254782292,
5.0026117381898));
#212219=CARTESIAN_POINT('Ctrl Pts',(16.5070803157911,-20.4361429715275,
5.12978754487123));
#212220=CARTESIAN_POINT('Ctrl Pts',(16.2806812434728,-17.8828514047509,
5.25696335155267));
#212221=CARTESIAN_POINT('Ctrl Pts',(18.3050498601331,-16.3104373152697,
5.38413915823409));
#212222=CARTESIAN_POINT('Ctrl Pts',(20.7229536064731,-17.1614930351577,
5.51131496491554));
#212223=CARTESIAN_POINT('Ctrl Pts',(21.3161158672572,-19.6552277638931,
5.63849077159696));
#212224=CARTESIAN_POINT('Ctrl Pts',(19.5403470840179,-21.503794666494,5.76566657827842));
#212225=CARTESIAN_POINT('Ctrl Pts',(17.0248048987365,-21.0112483448259,
5.89284238495983));
#212226=CARTESIAN_POINT('Ctrl Pts',(16.0773431342523,-18.6294694781468,
6.02001819164128));
#212227=CARTESIAN_POINT('Ctrl Pts',(17.5671991533703,-16.5435923467661,
6.1471939983227));
#212228=CARTESIAN_POINT('Ctrl Pts',(20.127522529443,-16.6672797545901,6.27436980500414));
#212229=CARTESIAN_POINT('Ctrl Pts',(21.4093754765144,-18.8870561818465,
6.40154561168558));
#212230=CARTESIAN_POINT('Ctrl Pts',(20.2367374764131,-21.1664145313908,
6.52872141836701));
#212231=CARTESIAN_POINT('Ctrl Pts',(17.6854311121095,-21.4141849904505,
6.65589722504845));
#212232=CARTESIAN_POINT('Ctrl Pts',(16.0961216209204,-19.4030535412072,
6.78307303172988));
#212233=CARTESIAN_POINT('Ctrl Pts',(16.9269018173399,-16.9781084634466,
6.91024883841132));
#212234=CARTESIAN_POINT('Ctrl Pts',(19.4155824351873,-16.3640863569478,
7.03742464509275));
#212235=CARTESIAN_POINT('Ctrl Pts',(21.2789534725274,-18.1243143939139,
7.16460045177418));
#212236=CARTESIAN_POINT('Ctrl Pts',(20.8074876564503,-20.6438926025015,
7.29177625845562));
#212237=CARTESIAN_POINT('Ctrl Pts',(18.4337256107381,-21.6112643589919,
7.41895206513705));
#212238=CARTESIAN_POINT('Ctrl Pts',(16.3354466800433,-20.1389261186678,
7.54612787181849));
#212239=CARTESIAN_POINT('Ctrl Pts',(16.4376915494001,-17.5776568334092,
7.67330367849992));
#212240=CARTESIAN_POINT('Ctrl Pts',(18.646656897206,-16.2772621021406,7.80047948518135));
#212241=CARTESIAN_POINT('Ctrl Pts',(20.9357541207011,-17.4307733792013,
7.92765529186279));
#212242=CARTESIAN_POINT('Ctrl Pts',(21.2048785947256,-19.9799156628723,
8.05483109854422));
#212243=CARTESIAN_POINT('Ctrl Pts',(19.2071253181107,-21.5860091254994,
8.18200690522566));
#212244=CARTESIAN_POINT('Ctrl Pts',(16.7753089275983,-20.7755627005247,
8.3091827119071));
#212245=CARTESIAN_POINT('Ctrl Pts',(16.1404700259359,-18.2921106808846,
8.43635851858852));
#212246=CARTESIAN_POINT('Ctrl Pts',(17.8850339028528,-16.4140661541825,
8.56353432526996));
#212247=CARTESIAN_POINT('Ctrl Pts',(20.4084714811236,-16.8644184090784,
8.69071013195139));
#212248=CARTESIAN_POINT('Ctrl Pts',(21.3956854048846,-19.2299972037186,
8.81788593863284));
#212249=CARTESIAN_POINT('Ctrl Pts',(19.9409681724916,-21.3405308183994,
8.94506174531426));
#212250=CARTESIAN_POINT('Ctrl Pts',(17.3789325547309,-21.2597356561407,
9.0722375519957));
#212251=CARTESIAN_POINT('Ctrl Pts',(16.0600872130337,-19.0617362636017,
9.19941335867713));
#212252=CARTESIAN_POINT('Ctrl Pts',(17.1943908916334,-16.7630606602087,
9.32658916535856));
#212253=CARTESIAN_POINT('Ctrl Pts',(19.7411903682412,-16.4726010401766,
9.45376497204));
#212254=CARTESIAN_POINT('Ctrl Pts',(21.3639551952721,-18.4568360769276,
9.58094077872143));
#212255=CARTESIAN_POINT('Ctrl Pts',(20.5738993640695,-20.8953532797583,
9.70811658540287));
#212256=CARTESIAN_POINT('Ctrl Pts',(18.0958500633667,-21.5509644665186,
9.83529239208431));
#212257=CARTESIAN_POINT('Ctrl Pts',(16.2032637214729,-19.8221870651751,
9.96246819876573));
#212258=CARTESIAN_POINT('Ctrl Pts',(16.6324708399194,-17.2950670414339,
10.0896440054472));
#212259=CARTESIAN_POINT('Ctrl Pts',(18.9897005271298,-16.2880801663194,
10.2168198121286));
#212260=CARTESIAN_POINT('Ctrl Pts',(21.1123408512631,-17.7250743970949,
10.3439956188101));
#212261=CARTESIAN_POINT('Ctrl Pts',(21.0530010608437,-20.2876967169446,
10.4711714254915));
#212262=CARTESIAN_POINT('Ctrl Pts',(18.8661217305387,-21.6249002016856,
10.598347232173));
#212263=CARTESIAN_POINT('Ctrl Pts',(16.5580289128638,-20.5098836502765,
10.7255230388544));
#212264=CARTESIAN_POINT('Ctrl Pts',(16.2462545116391,-17.965605542903,10.8526988455358));
#212265=CARTESIAN_POINT('Ctrl Pts',(18.2168321890867,-16.3262831273715,
10.9798746522173));
#212266=CARTESIAN_POINT('Ctrl Pts',(20.6618792339927,-17.0958929721078,
11.1070504588987));
#212267=CARTESIAN_POINT('Ctrl Pts',(21.3382167393905,-19.5683658119407,
11.2342262655802));
#212268=CARTESIAN_POINT('Ctrl Pts',(19.6253470223175,-21.4753612752947,
11.3614020722615));
#212269=CARTESIAN_POINT('Ctrl Pts',(17.0947217355035,-21.0673293860297,
11.488577878943));
#212270=CARTESIAN_POINT('Ctrl Pts',(16.0680325112813,-18.7186140772312,
11.6157536856244));
#212271=CARTESIAN_POINT('Ctrl Pts',(17.4872029893547,-16.584015867009,11.7429294923059));
#212272=CARTESIAN_POINT('Ctrl Pts',(20.0502323397452,-16.6218961251351,
11.8701052989873));
#212273=CARTESIAN_POINT('Ctrl Pts',(21.4057002130119,-18.797502065893,11.9972811056688));
#212274=CARTESIAN_POINT('Ctrl Pts',(20.3100489652569,-21.1148502719707,
12.1244569123501));
#212275=CARTESIAN_POINT('Ctrl Pts',(17.7684706125095,-21.4479175951428,
12.2516327190316));
#212276=CARTESIAN_POINT('Ctrl Pts',(16.1127055452724,-19.4911354388884,
12.378808525713));
#212277=CARTESIAN_POINT('Ctrl Pts',(16.8618154443651,-17.0397299799731,
12.5059843323945));
#212278=CARTESIAN_POINT('Ctrl Pts',(19.3285384723745,-16.3427135755694,
12.6331601390759));
#212279=CARTESIAN_POINT('Ctrl Pts',(21.2498093531994,-18.0395555150007,
12.7603359457573));
#212280=CARTESIAN_POINT('Ctrl Pts',(20.8629813012026,-20.5735086367272,
12.8875117524388));
#212281=CARTESIAN_POINT('Ctrl Pts',(18.5229450448345,-21.6198282264327,
13.0146875591202));
#212282=CARTESIAN_POINT('Ctrl Pts',(16.3765386102829,-20.2185810024805,
13.1418633658017));
#212283=CARTESIAN_POINT('Ctrl Pts',(16.3929566802409,-17.6553243216352,
13.2690391724831));
#212284=CARTESIAN_POINT('Ctrl Pts',(18.5571366945425,-16.2816870949206,
13.3962149791645));
#212285=CARTESIAN_POINT('Ctrl Pts',(20.8835778142264,-17.3578962203056,
13.5233907858459));
#212286=CARTESIAN_POINT('Ctrl Pts',(21.2379147072037,-19.8965966223211,
13.6505665925274));
#212287=CARTESIAN_POINT('Ctrl Pts',(19.2950652667951,-21.5686882516355,
13.7777423992088));
#212288=CARTESIAN_POINT('Ctrl Pts',(16.8374732677399,-20.8401308200636,
13.9049182058902));
#212289=CARTESIAN_POINT('Ctrl Pts',(16.1198268338089,-18.3793305516987,
14.0320940125717));
#212290=CARTESIAN_POINT('Ctrl Pts',(17.8005220259727,-16.4439189582757,
14.1592698192531));
#212291=CARTESIAN_POINT('Ctrl Pts',(20.3376253211293,-16.809516051569,14.2864456259346));
#212292=CARTESIAN_POINT('Ctrl Pts',(21.4035019163622,-19.140709189997,14.413621432616));
#212293=CARTESIAN_POINT('Ctrl Pts',(20.0202761913079,-21.2987733592159,
14.5407972392974));
#212294=CARTESIAN_POINT('Ctrl Pts',(17.4569718960327,-21.303818628536,14.6679730459788));
#212295=CARTESIAN_POINT('Ctrl Pts',(16.0652616248443,-19.1512162765007,
14.7951488526603));
#212296=CARTESIAN_POINT('Ctrl Pts',(17.1219531722769,-16.8158453555327,
14.9223246593417));
#212297=CARTESIAN_POINT('Ctrl Pts',(19.6575976292351,-16.4402637361534,
15.0495004660232));
#212298=CARTESIAN_POINT('Ctrl Pts',(21.3458985863041,-18.369044242919,15.1766762727046));
#212299=CARTESIAN_POINT('Ctrl Pts',(20.6379447031482,-20.8326504744915,
15.303852079386));
#212300=CARTESIAN_POINT('Ctrl Pts',(18.1832397269893,-21.5708766220509,
15.4310278860674));
#212301=CARTESIAN_POINT('Ctrl Pts',(16.2338231172801,-19.9064460146934,
15.5582036927489));
#212302=CARTESIAN_POINT('Ctrl Pts',(16.578163618988,-17.3663704284554,15.6853794994303));
#212303=CARTESIAN_POINT('Ctrl Pts',(18.9003501939781,-16.2810115588392,
15.8125553061118));
#212304=CARTESIAN_POINT('Ctrl Pts',(21.0699207908507,-17.6461188037487,
15.9397311127932));
#212305=CARTESIAN_POINT('Ctrl Pts',(21.0964290457131,-20.2092909940909,
16.0669069194746));
#212306=CARTESIAN_POINT('Ctrl Pts',(18.955555280017,-21.6189767336345,16.194082726156));
#212307=CARTESIAN_POINT('Ctrl Pts',(16.6114182961767,-20.581876851313,16.3212585328375));
#212308=CARTESIAN_POINT('Ctrl Pts',(16.214618283316,-18.0494661194781,16.4484343395189));
#212309=CARTESIAN_POINT('Ctrl Pts',(18.1291946250482,-16.3450742054518,
16.5756101462004));
#212310=CARTESIAN_POINT('Ctrl Pts',(20.5986423598435,-17.0323749038605,
16.7027859528818));
#212311=CARTESIAN_POINT('Ctrl Pts',(21.3573964622394,-19.4808124826067,
16.8299617595632));
#212312=CARTESIAN_POINT('Ctrl Pts',(19.7093471368785,-21.4440974303654,
16.9571375662447));
#212313=CARTESIAN_POINT('Ctrl Pts',(17.1664773503022,-21.1210376627748,
17.0843133729261));
#212314=CARTESIAN_POINT('Ctrl Pts',(16.0617123033954,-18.8080204652485,
17.2114891796075));
#212315=CARTESIAN_POINT('Ctrl Pts',(17.4086053572432,-16.6270955544791,
17.338664986289));
#212316=CARTESIAN_POINT('Ctrl Pts',(19.9714657325515,-16.579126172631,17.4658407929704));
#212317=CARTESIAN_POINT('Ctrl Pts',(21.3990281040287,-18.708121250235,17.5930165996518));
#212318=CARTESIAN_POINT('Ctrl Pts',(20.3815926003592,-21.0608599439249,
17.7201924063333));
#212319=CARTESIAN_POINT('Ctrl Pts',(17.8525931469884,-21.4788505296758,
17.8473682130147));
#212320=CARTESIAN_POINT('Ctrl Pts',(16.1322297749793,-19.5786125884764,
17.9745440196961));
#212321=CARTESIAN_POINT('Ctrl Pts',(16.7988291003494,-17.1034964893213,
18.1017198263776));
#212322=CARTESIAN_POINT('Ctrl Pts',(19.2408276159067,-16.3242676301314,
18.228895633059));
#212323=CARTESIAN_POINT('Ctrl Pts',(21.2178432511203,-17.955820124861,18.3560714397405));
#212324=CARTESIAN_POINT('Ctrl Pts',(20.9160868681659,-20.5013058250774,
18.4832472464219));
#212325=CARTESIAN_POINT('Ctrl Pts',(18.6124012191849,-21.6253995916595,
18.6104230531033));
#212326=CARTESIAN_POINT('Ctrl Pts',(16.4202749044646,-20.2968151625747,
18.7375988597848));
#212327=CARTESIAN_POINT('Ctrl Pts',(16.3508477586638,-17.7344462908773,
18.8647746664662));
#212328=CARTESIAN_POINT('Ctrl Pts',(18.4678148796782,-16.2891073766096,
18.9919504731476));
#212329=CARTESIAN_POINT('Ctrl Pts',(20.8289903263147,-17.286807168058,19.119126279829));
#212330=CARTESIAN_POINT('Ctrl Pts',(21.2681421801737,-19.8122180263779,
19.2463020865105));
#212331=CARTESIAN_POINT('Ctrl Pts',(19.3823758667575,-21.5484322422587,
19.3734778931919));
#212332=CARTESIAN_POINT('Ctrl Pts',(16.9017649452107,-20.9025810178173,
19.5006536998734));
#212333=CARTESIAN_POINT('Ctrl Pts',(16.1021159518554,-18.4671927970664,
19.6278295065548));
#212334=CARTESIAN_POINT('Ctrl Pts',(17.7170572450437,-16.4765850543542,
19.7550053132362));
#212335=CARTESIAN_POINT('Ctrl Pts',(20.2649803481551,-16.757016959998,19.8821811199177));
#212336=CARTESIAN_POINT('Ctrl Pts',(21.4083240999114,-19.0512094198929,
20.0093569265991));
#212337=CARTESIAN_POINT('Ctrl Pts',(20.0981412947811,-21.2543836816181,
20.1365327332805));
#212338=CARTESIAN_POINT('Ctrl Pts',(17.5364438714413,-21.345263264656,20.2637085399619));
#212339=CARTESIAN_POINT('Ctrl Pts',(16.0734291899427,-19.2404734101847,
20.3908843466434));
#212340=CARTESIAN_POINT('Ctrl Pts',(17.0513243981187,-16.8710250544057,
20.5180601533248));
#212341=CARTESIAN_POINT('Ctrl Pts',(19.5729675179493,-16.4107460050722,
20.6452359600063));
#212342=CARTESIAN_POINT('Ctrl Pts',(21.3249148566822,-18.2819021506609,
20.7724117666877));
#212343=CARTESIAN_POINT('Ctrl Pts',(20.6998492912724,-20.7678461580482,
20.8995875733692));
#212344=CARTESIAN_POINT('Ctrl Pts',(18.2712569976611,-21.5878357442275,
21.0267633800505));
#212345=CARTESIAN_POINT('Ctrl Pts',(16.2671680424845,-19.989664109829,21.153939186732));
#212346=CARTESIAN_POINT('Ctrl Pts',(16.5263110482178,-17.4393951028376,
21.2811149934134));
#212347=CARTESIAN_POINT('Ctrl Pts',(18.8107430407941,-16.2770494228818,
21.4082908000949));
#212348=CARTESIAN_POINT('Ctrl Pts',(21.0250158365398,-17.568415239189,21.5354666067763));
#212349=CARTESIAN_POINT('Ctrl Pts',(21.1369463139771,-20.1298851974028,
21.6626424134577));
#212350=CARTESIAN_POINT('Ctrl Pts',(19.0452436034431,-21.6092686761098,
21.7898182201392));
#212351=CARTESIAN_POINT('Ctrl Pts',(16.6662107583285,-20.6535950540795,
21.9169940268206));
#212352=CARTESIAN_POINT('Ctrl Pts',(16.1877691759169,-18.1311075337387,
22.044169833502));
#212353=CARTESIAN_POINT('Ctrl Pts',(17.4210581833076,-16.960478579468,22.128953704623));
#212354=CARTESIAN_POINT('Ctrl Pts',(18.1489775593156,-16.7656980002009,
22.1713456401835));
#212355=CARTESIAN_POINT('Ctrl Pts',(20.5799312301559,-17.397553415447,-0.171094886838164));
#212356=CARTESIAN_POINT('Ctrl Pts',(21.0977302932136,-18.0124050913494,
-0.128684295257136));
#212357=CARTESIAN_POINT('Ctrl Pts',(21.4611752643293,-19.7893203209783,
-0.0438817681156302));
#212358=CARTESIAN_POINT('Ctrl Pts',(19.5021063818899,-21.7021724412225,
0.0833126945863534));
#212359=CARTESIAN_POINT('Ctrl Pts',(16.8390406066394,-21.0844924660501,
0.210488501267787));
#212360=CARTESIAN_POINT('Ctrl Pts',(15.9143177655174,-18.5139387940262,
0.337664307949223));
#212361=CARTESIAN_POINT('Ctrl Pts',(17.5765589760555,-16.343449345859,0.464840114630657));
#212362=CARTESIAN_POINT('Ctrl Pts',(20.3006391625102,-16.567091249899,0.592015921312092));
#212363=CARTESIAN_POINT('Ctrl Pts',(21.5874465485414,-18.9782470197745,
0.719191727993526));
#212364=CARTESIAN_POINT('Ctrl Pts',(20.2563827322944,-21.3655780685178,
0.846367534674961));
#212365=CARTESIAN_POINT('Ctrl Pts',(17.5286330090264,-21.5384685392327,
0.973543341356394));
#212366=CARTESIAN_POINT('Ctrl Pts',(15.906729696796,-19.3385034339308,1.10071914803782));
#212367=CARTESIAN_POINT('Ctrl Pts',(16.8786729593171,-16.7839097205383,
1.22789495471926));
#212368=CARTESIAN_POINT('Ctrl Pts',(19.5527628216649,-16.2184227996018,
1.35507076140069));
#212369=CARTESIAN_POINT('Ctrl Pts',(21.4756890313297,-18.1608136783876,
1.48224656808212));
#212370=CARTESIAN_POINT('Ctrl Pts',(20.8832855061817,-20.8290738921377,
1.60942237476356));
#212371=CARTESIAN_POINT('Ctrl Pts',(18.3190460414365,-21.7752327234411,
1.73659818144499));
#212372=CARTESIAN_POINT('Ctrl Pts',(16.1355010202711,-20.1312521052755,
1.86377398812643));
#212373=CARTESIAN_POINT('Ctrl Pts',(16.3359175623115,-17.4053801752063,
1.99094979480786));
#212374=CARTESIAN_POINT('Ctrl Pts',(18.7364258834009,-16.0984363025981,
2.1181256014893));
#212375=CARTESIAN_POINT('Ctrl Pts',(21.134708615211,-17.4094598221888,2.24530140817073));
#212376=CARTESIAN_POINT('Ctrl Pts',(21.3304901931038,-20.135668311675,2.37247721485217));
#212377=CARTESIAN_POINT('Ctrl Pts',(19.1441531773822,-21.7759345412849,
2.49965302153361));
#212378=CARTESIAN_POINT('Ctrl Pts',(16.5815260772467,-20.8254161287028,
2.62682882821504));
#212379=CARTESIAN_POINT('Ctrl Pts',(15.993660204232,-18.1561546817078,2.75400463489647));
#212380=CARTESIAN_POINT('Ctrl Pts',(17.9198860088567,-16.2170319255978,
2.8811804415779));
#212381=CARTESIAN_POINT('Ctrl Pts',(20.5930108709022,-16.7870726228123,
3.00835624825935));
#212382=CARTESIAN_POINT('Ctrl Pts',(21.5606086420394,-19.3432998199575,
3.13553205494078));
#212383=CARTESIAN_POINT('Ctrl Pts',(19.9349684232667,-21.5405337181072,
3.26270786162222));
#212384=CARTESIAN_POINT('Ctrl Pts',(17.2075142166313,-21.3629485929295,
3.38988366830364));
#212385=CARTESIAN_POINT('Ctrl Pts',(15.8805159718554,-18.9734677738182,
3.51705947498509));
#212386=CARTESIAN_POINT('Ctrl Pts',(17.1714122157033,-16.5642916048074,
3.64423528166652));
#212387=CARTESIAN_POINT('Ctrl Pts',(19.8958857665108,-16.3456896904175,
3.77141108834796));
#212388=CARTESIAN_POINT('Ctrl Pts',(21.5544012413067,-18.5182157192451,
3.89858689502939));
#212389=CARTESIAN_POINT('Ctrl Pts',(20.6253736310478,-21.0887119019572,
4.02576270171082));
#212390=CARTESIAN_POINT('Ctrl Pts',(17.9611281061891,-21.6989075339308,
4.15293850839226));
#212391=CARTESIAN_POINT('Ctrl Pts',(16.0059445740623,-19.7889859958273,
4.28011431507369));
#212392=CARTESIAN_POINT('Ctrl Pts',(16.5535825730174,-17.1111817557645,
4.40729012175513));
#212393=CARTESIAN_POINT('Ctrl Pts',(19.101618229261,-16.1222140007207,4.53446592843656));
#212394=CARTESIAN_POINT('Ctrl Pts',(21.3123869771181,-17.7293992636892,
4.661641735118));
#212395=CARTESIAN_POINT('Ctrl Pts',(21.1576457062134,-20.4582448190628,
4.78881754179943));
#212396=CARTESIAN_POINT('Ctrl Pts',(18.7793599282756,-21.8052042410433,
4.91599334848086));
#212397=CARTESIAN_POINT('Ctrl Pts',(16.3594592314995,-20.5345258616938,
5.0431691551623));
#212398=CARTESIAN_POINT('Ctrl Pts',(16.1180523092011,-17.8119782268727,
5.17034496184372));
#212399=CARTESIAN_POINT('Ctrl Pts',(18.2766150291857,-16.1353298111647,
5.29752076852517));
#212400=CARTESIAN_POINT('Ctrl Pts',(20.8548000713794,-17.0428014714449,
5.4246965752066));
#212401=CARTESIAN_POINT('Ctrl Pts',(21.4872826797803,-19.7018442834496,
5.55187238188803));
#212402=CARTESIAN_POINT('Ctrl Pts',(19.5937993174784,-21.6729515059744,
5.67904818856948));
#212403=CARTESIAN_POINT('Ctrl Pts',(16.9115034465541,-21.1477546030643,
5.8062239952509));
#212404=CARTESIAN_POINT('Ctrl Pts',(15.901235046523,-18.6080891357435,5.93339980193234));
#212405=CARTESIAN_POINT('Ctrl Pts',(17.4898526700851,-16.3839405408623,
6.06057560861377));
#212406=CARTESIAN_POINT('Ctrl Pts',(20.2198982483519,-16.515827107994,6.1877514152952));
#212407=CARTESIAN_POINT('Ctrl Pts',(21.5867244090021,-18.8827510975986,
6.31492722197664));
#212408=CARTESIAN_POINT('Ctrl Pts',(20.3363529844384,-21.3132066570849,
6.44210302865808));
#212409=CARTESIAN_POINT('Ctrl Pts',(17.6159221498948,-21.577401661709,6.56927883533951));
#212410=CARTESIAN_POINT('Ctrl Pts',(15.921258347085,-19.4329535925197,6.69645464202095));
#212411=CARTESIAN_POINT('Ctrl Pts',(16.8071104323889,-16.8472604535401,
6.82363044870238));
#212412=CARTESIAN_POINT('Ctrl Pts',(19.4607640997214,-16.1925352135684,
6.95080625538382));
#212413=CARTESIAN_POINT('Ctrl Pts',(21.4476568136269,-18.0694476434471,
7.07798206206525));
#212414=CARTESIAN_POINT('Ctrl Pts',(20.9449378295665,-20.7560470830862,
7.20515786874668));
#212415=CARTESIAN_POINT('Ctrl Pts',(18.4138206131569,-21.7875452957837,
7.33233367542812));
#212416=CARTESIAN_POINT('Ctrl Pts',(16.1764481116018,-20.2176066933892,
7.45950948210955));
#212417=CARTESIAN_POINT('Ctrl Pts',(16.2854707280793,-17.4865525022204,
7.586685288791));
#212418=CARTESIAN_POINT('Ctrl Pts',(18.6408669786781,-16.0999554343349,
7.7138610954724));
#212419=CARTESIAN_POINT('Ctrl Pts',(21.0817069958525,-17.3299322375973,
7.84103690215387));
#212420=CARTESIAN_POINT('Ctrl Pts',(21.3686715594619,-20.0480555359847,
7.96821270883528));
#212421=CARTESIAN_POINT('Ctrl Pts',(19.2384884934243,-21.7606159089848,
8.09538851551673));
#212422=CARTESIAN_POINT('Ctrl Pts',(16.6454685467572,-20.8964455078546,
8.22256432219815));
#212423=CARTESIAN_POINT('Ctrl Pts',(15.9685465795588,-18.2483670391668,
8.3497401288796));
#212424=CARTESIAN_POINT('Ctrl Pts',(17.8287564822182,-16.2458281396566,
8.47691593556102));
#212425=CARTESIAN_POINT('Ctrl Pts',(20.5194711266932,-16.726033958043,8.60409174224246));
#212426=CARTESIAN_POINT('Ctrl Pts',(21.5721268312631,-19.248425460891,8.7312675489239));
#212427=CARTESIAN_POINT('Ctrl Pts',(20.0209773221669,-21.4988650016106,
8.85844335560533));
#212428=CARTESIAN_POINT('Ctrl Pts',(17.2891059988037,-21.4127139796221,
8.98561916228676));
#212429=CARTESIAN_POINT('Ctrl Pts',(15.8828352413023,-19.0690106104647,
9.1127949689682));
#212430=CARTESIAN_POINT('Ctrl Pts',(17.0923311866634,-16.6179572687033,
9.23997077564963));
#212431=CARTESIAN_POINT('Ctrl Pts',(19.8079563748028,-16.308243265877,9.36714658233107));
#212432=CARTESIAN_POINT('Ctrl Pts',(21.5382932463107,-18.4240119765596,
9.4943223890125));
#212433=CARTESIAN_POINT('Ctrl Pts',(20.6958651183971,-21.0241769281162,
9.62149819569394));
#212434=CARTESIAN_POINT('Ctrl Pts',(18.0535475114361,-21.7232481619313,
9.74867400237537));
#212435=CARTESIAN_POINT('Ctrl Pts',(16.0355028290879,-19.8798712102337,
9.8758498090568));
#212436=CARTESIAN_POINT('Ctrl Pts',(16.4931618134281,-17.1852300133289,
10.0030256157383));
#212437=CARTESIAN_POINT('Ctrl Pts',(19.0066507518444,-16.1114906210823,
10.1302014224197));
#212438=CARTESIAN_POINT('Ctrl Pts',(21.2699995480578,-17.6437422820976,
10.2573772291012));
#212439=CARTESIAN_POINT('Ctrl Pts',(21.2067261608115,-20.3762391996566,
10.3845530357826));
#212440=CARTESIAN_POINT('Ctrl Pts',(18.874879995715,-21.802085049785,10.511728842464));
#212441=CARTESIAN_POINT('Ctrl Pts',(16.4137851785486,-20.613154762964,10.6389046491454));
#212442=CARTESIAN_POINT('Ctrl Pts',(16.0813434512909,-17.9002180840159,
10.7660804558269));
#212443=CARTESIAN_POINT('Ctrl Pts',(18.1825494650401,-16.1522260320353,
10.8932562625083));
#212444=CARTESIAN_POINT('Ctrl Pts',(20.7896771177347,-16.9728528220917,
11.0204320691897));
#212445=CARTESIAN_POINT('Ctrl Pts',(21.5108486046191,-19.6092243081515,
11.1476078758712));
#212446=CARTESIAN_POINT('Ctrl Pts',(19.6844338474274,-21.6426332834231,
11.2747836825526));
#212447=CARTESIAN_POINT('Ctrl Pts',(16.9860550257985,-21.2075532206898,
11.4019594892341));
#212448=CARTESIAN_POINT('Ctrl Pts',(15.8913072282989,-18.7031430733949,
11.5291352959155));
#212449=CARTESIAN_POINT('Ctrl Pts',(17.4045536114233,-16.4270437104573,
11.6563111025969));
#212450=CARTESIAN_POINT('Ctrl Pts',(20.1374845413179,-16.4674350267135,
11.7834869092783));
#212451=CARTESIAN_POINT('Ctrl Pts',(21.5828055146281,-18.7872604964663,
11.9106627159598));
#212452=CARTESIAN_POINT('Ctrl Pts',(20.4145242450785,-21.2582242358244,
12.0378385226412));
#212453=CARTESIAN_POINT('Ctrl Pts',(17.7044662857673,-21.613370379233,12.1650143293227));
#212454=CARTESIAN_POINT('Ctrl Pts',(15.9389416091958,-19.5268743829703,
12.2921901360041));
#212455=CARTESIAN_POINT('Ctrl Pts',(16.7377095252982,-16.9129668210605,
12.4193659426856));
#212456=CARTESIAN_POINT('Ctrl Pts',(19.3679500481791,-16.1697456441558,
12.5465417493669));
#212457=CARTESIAN_POINT('Ctrl Pts',(21.416580749233,-17.9790701525573,12.6737175560484));
#212458=CARTESIAN_POINT('Ctrl Pts',(21.0041101126047,-20.6809974091509,
12.8008933627298));
#212459=CARTESIAN_POINT('Ctrl Pts',(18.5089543465855,-21.7966768565304,
12.9280691694113));
#212460=CARTESIAN_POINT('Ctrl Pts',(16.2202639996657,-20.3025418486013,
13.0552449760927));
#212461=CARTESIAN_POINT('Ctrl Pts',(16.2377704130005,-17.5693685186612,
13.1824207827741));
#212462=CARTESIAN_POINT('Ctrl Pts',(18.545412538926,-16.1046737570615,13.3095965894556));
#212463=CARTESIAN_POINT('Ctrl Pts',(21.0260719553289,-17.2522240983603,
13.436772396137));
#212464=CARTESIAN_POINT('Ctrl Pts',(21.4038976147472,-19.9592133294229,
13.5639482028184));
#212465=CARTESIAN_POINT('Ctrl Pts',(19.3322579251698,-21.7421468454496,
13.6911240094999));
#212466=CARTESIAN_POINT('Ctrl Pts',(16.7117537213236,-20.96529380682,13.8182998161813));
#212467=CARTESIAN_POINT('Ctrl Pts',(15.9465349634034,-18.3413686595396,
13.9454756228628));
#212468=CARTESIAN_POINT('Ctrl Pts',(17.7386423669686,-16.2776598670762,
14.0726514295442));
#212469=CARTESIAN_POINT('Ctrl Pts',(20.443928619978,-16.6674921583018,14.1998272362256));
#212470=CARTESIAN_POINT('Ctrl Pts',(21.5804614942969,-19.1532186017375,
14.327003042907));
#212471=CARTESIAN_POINT('Ctrl Pts',(20.1055426189236,-21.454339467114,14.4541788495885));
#212472=CARTESIAN_POINT('Ctrl Pts',(17.3723185182233,-21.4597191841168,
14.5813546562699));
#212473=CARTESIAN_POINT('Ctrl Pts',(15.8883526615688,-19.1644221962985,
14.7085304629514));
#212474=CARTESIAN_POINT('Ctrl Pts',(17.015091617132,-16.6742410277849,14.8357062696328));
#212475=CARTESIAN_POINT('Ctrl Pts',(19.7188223264901,-16.2737623426128,
14.9628820763142));
#212476=CARTESIAN_POINT('Ctrl Pts',(21.5190396762608,-18.3304004779172,
15.0900578829957));
#212477=CARTESIAN_POINT('Ctrl Pts',(20.7641559821193,-20.9573175939151,
15.2172336896771));
#212478=CARTESIAN_POINT('Ctrl Pts',(18.1467301800744,-21.7444802815428,
15.3444094963585));
#212479=CARTESIAN_POINT('Ctrl Pts',(16.0680879877353,-19.9697156317281,
15.4715853030399));
#212480=CARTESIAN_POINT('Ctrl Pts',(16.4352546014886,-17.2612600563589,
15.5987611097214));
#212481=CARTESIAN_POINT('Ctrl Pts',(18.9113774421457,-16.1039534401246,
15.7259369164028));
#212482=CARTESIAN_POINT('Ctrl Pts',(21.2247674889198,-17.5595527728704,
15.8531127230842));
#212483=CARTESIAN_POINT('Ctrl Pts',(21.2530329590753,-20.2926360114859,
15.9802885297657));
#212484=CARTESIAN_POINT('Ctrl Pts',(18.9702420380974,-21.7957689188181,
16.1074643364471));
#212485=CARTESIAN_POINT('Ctrl Pts',(16.4707137099997,-20.6899203473398,
16.2346401431286));
#212486=CARTESIAN_POINT('Ctrl Pts',(16.0476100775874,-17.9896377246791,
16.36181594981));
#212487=CARTESIAN_POINT('Ctrl Pts',(18.0891024628257,-16.1722627586861,
16.4889917564914));
#212488=CARTESIAN_POINT('Ctrl Pts',(20.722248311566,-16.9051241816477,16.6161675631729));
#212489=CARTESIAN_POINT('Ctrl Pts',(21.5312997390521,-19.5158671245064,
16.7433433698543));
#212490=CARTESIAN_POINT('Ctrl Pts',(19.7740022759604,-21.6092969781711,
16.8705191765357));
#212491=CARTESIAN_POINT('Ctrl Pts',(17.062567274496,-21.2648217848151,16.9976949832172));
#212492=CARTESIAN_POINT('Ctrl Pts',(15.8845680578669,-18.7984761538005,
17.1248707898986));
#212493=CARTESIAN_POINT('Ctrl Pts',(17.3207457924527,-16.4729791229096,
17.25204659658));
#212494=CARTESIAN_POINT('Ctrl Pts',(20.0534965460147,-16.4218298813604,
17.3792224032615));
#212495=CARTESIAN_POINT('Ctrl Pts',(21.5756911157996,-18.6919546835953,
17.5063982099429));
#212496=CARTESIAN_POINT('Ctrl Pts',(20.4908104620813,-21.2006549233978,
17.6335740166243));
#212497=CARTESIAN_POINT('Ctrl Pts',(17.7941652493564,-21.6463538382498,
17.7607498233058));
#212498=CARTESIAN_POINT('Ctrl Pts',(15.9597600876265,-19.6201503369626,
17.8879256299872));
#212499=CARTESIAN_POINT('Ctrl Pts',(16.6705478567457,-16.9809603716076,
18.0151014366687));
#212500=CARTESIAN_POINT('Ctrl Pts',(19.2744248950271,-16.1500769287699,
18.1422772433501));
#212501=CARTESIAN_POINT('Ctrl Pts',(21.382495634653,-17.8897839968585,18.2694530500315));
#212502=CARTESIAN_POINT('Ctrl Pts',(21.0607360137015,-20.6040083192082,
18.3966288567129));
#212503=CARTESIAN_POINT('Ctrl Pts',(18.6043405136283,-21.8026175440015,
18.5238046633944));
#212504=CARTESIAN_POINT('Ctrl Pts',(16.2668995448691,-20.3859621012267,
18.6509804700758));
#212505=CARTESIAN_POINT('Ctrl Pts',(16.1928701178928,-17.6537354327361,
18.7781562767572));
#212506=CARTESIAN_POINT('Ctrl Pts',(18.4501696379737,-16.1125859244869,
18.9053320834387));
#212507=CARTESIAN_POINT('Ctrl Pts',(20.9678658976898,-17.1764225982197,
19.0325078901201));
#212508=CARTESIAN_POINT('Ctrl Pts',(21.4361288476046,-19.8692413302184,
19.1596836968015));
#212509=CARTESIAN_POINT('Ctrl Pts',(19.4253562890682,-21.7205480781417,
19.286859503483));
#212510=CARTESIAN_POINT('Ctrl Pts',(16.7803072530527,-21.0318837883171,
19.4140353101644));
#212511=CARTESIAN_POINT('Ctrl Pts',(15.9276500383912,-18.435055237065,19.5412111168458));
#212512=CARTESIAN_POINT('Ctrl Pts',(17.6496447589923,-16.3124913778111,
19.6683869235273));
#212513=CARTESIAN_POINT('Ctrl Pts',(20.366468058119,-16.6115129354638,19.7955627302087));
#212514=CARTESIAN_POINT('Ctrl Pts',(21.5856033373152,-19.0577859490064,
19.9227385368901));
#212515=CARTESIAN_POINT('Ctrl Pts',(20.1885693504001,-21.4070072261248,
20.0499143435716));
#212516=CARTESIAN_POINT('Ctrl Pts',(17.45705864015,-21.5039111587085,20.177090150253));
#212517=CARTESIAN_POINT('Ctrl Pts',(15.8970616493438,-19.2595961283962,
20.3042659569345));
#212518=CARTESIAN_POINT('Ctrl Pts',(16.9397809066213,-16.7330785536716,
20.4314417636159));
#212519=CARTESIAN_POINT('Ctrl Pts',(19.6285821391517,-16.2422878999811,
20.5586175702973));
#212520=CARTESIAN_POINT('Ctrl Pts',(21.4966649485975,-18.2374817919912,
20.6857933769788));
#212521=CARTESIAN_POINT('Ctrl Pts',(20.8301641858729,-20.8882174407032,
20.8129691836602));
#212522=CARTESIAN_POINT('Ctrl Pts',(18.2405820594323,-21.7625636131024,
20.9401449903416));
#212523=CARTESIAN_POINT('Ctrl Pts',(16.1036433267455,-20.0584502012673,
21.0673207970231));
#212524=CARTESIAN_POINT('Ctrl Pts',(16.3799647569026,-17.3391254897899,
21.1944966037045));
#212525=CARTESIAN_POINT('Ctrl Pts',(18.8158302879787,-16.0997286567039,
21.3216724103859));
#212526=CARTESIAN_POINT('Ctrl Pts',(21.1768858138531,-17.4766982886188,
21.4488482170674));
#212527=CARTESIAN_POINT('Ctrl Pts',(21.2962360911878,-20.207966455225,21.5760240237488));
#212528=CARTESIAN_POINT('Ctrl Pts',(19.0658757432302,-21.7854173203574,
21.7031998304302));
#212529=CARTESIAN_POINT('Ctrl Pts',(16.5291383294904,-20.7663927039858,
21.8303756371117));
#212530=CARTESIAN_POINT('Ctrl Pts',(16.0189811599981,-18.0766910961744,
21.9575514437931));
#212531=CARTESIAN_POINT('Ctrl Pts',(17.3340241084075,-16.828461895807,22.0423353149141));
#212532=CARTESIAN_POINT('Ctrl Pts',(18.110196795177,-16.6207694362802,22.0847272504745));
#212533=CARTESIAN_POINT('Ctrl Pts',(20.694689575575,-17.3009161652768,-0.257713276547101));
#212534=CARTESIAN_POINT('Ctrl Pts',(21.2446793089921,-17.9539921042784,
-0.215302684966074));
#212535=CARTESIAN_POINT('Ctrl Pts',(21.6307190240804,-19.8413750741844,
-0.130500157824568));
#212536=CARTESIAN_POINT('Ctrl Pts',(19.5498582244566,-21.8731458956047,
-0.00330569512258456));
#212537=CARTESIAN_POINT('Ctrl Pts',(16.721234265284,-21.2170658268692,0.123870111558849));
#212538=CARTESIAN_POINT('Ctrl Pts',(15.7390230077546,-18.486705288049,0.251045918240284));
#212539=CARTESIAN_POINT('Ctrl Pts',(17.504602873543,-16.1812802725366,0.378221724921718));
#212540=CARTESIAN_POINT('Ctrl Pts',(20.3980344041213,-16.4188256061599,
0.505397531603153));
#212541=CARTESIAN_POINT('Ctrl Pts',(21.7648403751927,-18.9798787515055,
0.632573338284587));
#212542=CARTESIAN_POINT('Ctrl Pts',(20.3510266283393,-21.5156260340964,
0.759749144966022));
#212543=CARTESIAN_POINT('Ctrl Pts',(17.4536974322035,-21.6992648057414,
0.886924951647455));
#212544=CARTESIAN_POINT('Ctrl Pts',(15.7309632019515,-19.3625316825742,
1.01410075832889));
#212545=CARTESIAN_POINT('Ctrl Pts',(16.7633304926413,-16.6491233053535,
1.14127656501032));
#212546=CARTESIAN_POINT('Ctrl Pts',(19.6036638873005,-16.0484810425805,
1.26845237169176));
#212547=CARTESIAN_POINT('Ctrl Pts',(21.6461350868215,-18.1116269959678,
1.39562817837319));
#212548=CARTESIAN_POINT('Ctrl Pts',(21.0169028612021,-20.9457683228794,
1.52280398505463));
#212549=CARTESIAN_POINT('Ctrl Pts',(18.293249072984,-21.9507482089492,1.64997979173606));
#212550=CARTESIAN_POINT('Ctrl Pts',(15.9739568421265,-20.2045641649137,
1.7771555984175));
#212551=CARTESIAN_POINT('Ctrl Pts',(16.1868329332462,-17.3092295011259,
1.90433140509893));
#212552=CARTESIAN_POINT('Ctrl Pts',(18.7365766963677,-15.9210351930051,
2.03150721178036));
#212553=CARTESIAN_POINT('Ctrl Pts',(21.2839565091815,-17.3135627726908,
2.1586830184618));
#212554=CARTESIAN_POINT('Ctrl Pts',(21.4919094884653,-20.2092549192115,
2.28585882514323));
#212555=CARTESIAN_POINT('Ctrl Pts',(19.1696516895889,-21.951493657592,2.41303463182467));
#212556=CARTESIAN_POINT('Ctrl Pts',(16.4477105038941,-20.9418831626308,
2.5402104385061));
#212557=CARTESIAN_POINT('Ctrl Pts',(15.8232980283766,-18.1066783575389,
2.66738624518754));
#212558=CARTESIAN_POINT('Ctrl Pts',(17.8692739529578,-16.0470037003502,
2.79456205186897));
#212559=CARTESIAN_POINT('Ctrl Pts',(20.7085823549184,-16.6524828397803,
2.9217378585504));
#212560=CARTESIAN_POINT('Ctrl Pts',(21.7363340025561,-19.3676262516076,
3.04891366523184));
#212561=CARTESIAN_POINT('Ctrl Pts',(20.0096305487582,-21.7014583732074,
3.17608947191327));
#212562=CARTESIAN_POINT('Ctrl Pts',(17.1126152410121,-21.5128330885679,
3.30326527859471));
#212563=CARTESIAN_POINT('Ctrl Pts',(15.703119815162,-18.9748023881108,3.43044108527614));
#212564=CARTESIAN_POINT('Ctrl Pts',(17.0742688412544,-16.4158519119851,
3.55761689195758));
#212565=CARTESIAN_POINT('Ctrl Pts',(19.9681181909656,-16.1836598954335,
3.68479269863901));
#212566=CARTESIAN_POINT('Ctrl Pts',(21.7297406984776,-18.4912481022967,
3.81196850532045));
#212567=CARTESIAN_POINT('Ctrl Pts',(20.7429570517748,-21.221547577794,3.93914431200188));
#212568=CARTESIAN_POINT('Ctrl Pts',(17.9130800000052,-21.8696780146852,
4.06632011868332));
#212569=CARTESIAN_POINT('Ctrl Pts',(15.8363460961894,-19.8410199646181,
4.19349592536474));
#212570=CARTESIAN_POINT('Ctrl Pts',(16.4180298004353,-16.9967412758189,
4.32067173204619));
#212571=CARTESIAN_POINT('Ctrl Pts',(19.1244724174598,-15.9462911094113,
4.44784753872761));
#212572=CARTESIAN_POINT('Ctrl Pts',(21.4726808269163,-17.6533922947864,
4.57502334540905));
#212573=CARTESIAN_POINT('Ctrl Pts',(21.3083195593796,-20.5518854490104,
4.70219915209049));
#212574=CARTESIAN_POINT('Ctrl Pts',(18.7821798764038,-21.9825830038574,
4.82937495877192));
#212575=CARTESIAN_POINT('Ctrl Pts',(16.2118381472079,-20.6329087518601,
4.95655076545335));
#212576=CARTESIAN_POINT('Ctrl Pts',(15.9554233749293,-17.7411050489944,
5.08372657213479));
#212577=CARTESIAN_POINT('Ctrl Pts',(18.2481801982382,-15.9602223070596,
5.21090237881622));
#212578=CARTESIAN_POINT('Ctrl Pts',(20.9866465362858,-16.9241099077319,
5.33807818549766));
#212579=CARTESIAN_POINT('Ctrl Pts',(21.6584494923035,-19.7484608030062,
5.46525399217908));
#212580=CARTESIAN_POINT('Ctrl Pts',(19.6472515509388,-21.8421083454548,
5.59242979886053));
#212581=CARTESIAN_POINT('Ctrl Pts',(16.7982019943716,-21.2842608613029,
5.71960560554195));
#212582=CARTESIAN_POINT('Ctrl Pts',(15.7251269587939,-18.5867087933401,
5.8467814122234));
#212583=CARTESIAN_POINT('Ctrl Pts',(17.4125061868001,-16.2242887349586,
5.97395721890483));
#212584=CARTESIAN_POINT('Ctrl Pts',(20.3122739672608,-16.3643744613978,
6.10113302558626));
#212585=CARTESIAN_POINT('Ctrl Pts',(21.7640733414898,-18.8784460133507,
6.2283088322677));
#212586=CARTESIAN_POINT('Ctrl Pts',(20.4359684924635,-21.459998782779,6.35548463894913));
#212587=CARTESIAN_POINT('Ctrl Pts',(17.54641318768,-21.7406183329676,6.48266044563057));
#212588=CARTESIAN_POINT('Ctrl Pts',(15.7463950732497,-19.4628536438322,
6.609836252312));
#212589=CARTESIAN_POINT('Ctrl Pts',(16.687319047438,-16.7164124436336,6.73701205899344));
#212590=CARTESIAN_POINT('Ctrl Pts',(19.5059457642557,-16.0209840701888,
6.86418786567487));
#212591=CARTESIAN_POINT('Ctrl Pts',(21.6163601547263,-18.0145808929804,
6.99136367235631));
#212592=CARTESIAN_POINT('Ctrl Pts',(21.0823880026828,-20.8682015636709,
7.11853947903774));
#212593=CARTESIAN_POINT('Ctrl Pts',(18.3939156155757,-21.9638262325756,
7.24571528571917));
#212594=CARTESIAN_POINT('Ctrl Pts',(16.0174495431603,-20.2962872681105,
7.37289109240061));
#212595=CARTESIAN_POINT('Ctrl Pts',(16.1332499067586,-17.3954481710317,
7.50006689908204));
#212596=CARTESIAN_POINT('Ctrl Pts',(18.6350770601501,-15.9226487665292,
7.62724270576348));
#212597=CARTESIAN_POINT('Ctrl Pts',(21.2276598710039,-17.2290910959936,
7.75441851244491));
#212598=CARTESIAN_POINT('Ctrl Pts',(21.5324645241983,-20.1161954090971,
7.88159431912634));
#212599=CARTESIAN_POINT('Ctrl Pts',(19.2698516687381,-21.9352226924704,
8.00877012580778));
#212600=CARTESIAN_POINT('Ctrl Pts',(16.515628165916,-21.0173283151844,8.13594593248921));
#212601=CARTESIAN_POINT('Ctrl Pts',(15.7966231331818,-18.2046233974491,
8.26312173917066));
#212602=CARTESIAN_POINT('Ctrl Pts',(17.7724790615836,-16.0775901251306,
8.39029754585207));
#212603=CARTESIAN_POINT('Ctrl Pts',(20.6304707722626,-16.5876495070077,
8.51747335253352));
#212604=CARTESIAN_POINT('Ctrl Pts',(21.7485682576417,-19.2668537180634,
8.64464915921496));
#212605=CARTESIAN_POINT('Ctrl Pts',(20.1009864718422,-21.6571991848217,
8.77182496589638));
#212606=CARTESIAN_POINT('Ctrl Pts',(17.1992794428765,-21.5656923031035,
8.89900077257782));
#212607=CARTESIAN_POINT('Ctrl Pts',(15.7055832695711,-19.0762849573277,
9.02617657925926));
#212608=CARTESIAN_POINT('Ctrl Pts',(16.9902714816934,-16.4728538771981,
9.15335238594069));
#212609=CARTESIAN_POINT('Ctrl Pts',(19.8747223813643,-16.1438854915773,
9.28052819262213));
#212610=CARTESIAN_POINT('Ctrl Pts',(21.7126312973492,-18.3911878761916,
9.40770399930354));
#212611=CARTESIAN_POINT('Ctrl Pts',(20.8178308727247,-21.1530005764741,
9.53487980598502));
#212612=CARTESIAN_POINT('Ctrl Pts',(18.0112449595055,-21.8955318573441,
9.66205561266641));
#212613=CARTESIAN_POINT('Ctrl Pts',(15.8677419367031,-19.9375553552922,
9.78923141934788));
#212614=CARTESIAN_POINT('Ctrl Pts',(16.3538527869367,-17.0753929852239,
9.91640722602929));
#212615=CARTESIAN_POINT('Ctrl Pts',(19.0236009765592,-15.9349010758452,
10.0435830327108));
#212616=CARTESIAN_POINT('Ctrl Pts',(21.4276582448523,-17.5624101671002,
10.1707588393922));
#212617=CARTESIAN_POINT('Ctrl Pts',(21.3604512607793,-20.4647816823687,
10.2979346460737));
#212618=CARTESIAN_POINT('Ctrl Pts',(18.8836382608913,-21.9792698978844,
10.4251104527551));
#212619=CARTESIAN_POINT('Ctrl Pts',(16.2695414442335,-20.7164258756515,
10.5522862594365));
#212620=CARTESIAN_POINT('Ctrl Pts',(15.9164323909425,-17.8348306251289,
10.6794620661178));
#212621=CARTESIAN_POINT('Ctrl Pts',(18.1482667409934,-15.9781689366991,
10.8066378727994));
#212622=CARTESIAN_POINT('Ctrl Pts',(20.9174750014767,-16.8498126720757,
10.9338136794808));
#212623=CARTESIAN_POINT('Ctrl Pts',(21.6834804698477,-19.6500828043623,
11.0609894861623));
#212624=CARTESIAN_POINT('Ctrl Pts',(19.7435206725372,-21.8099052915517,
11.1881652928437));
#212625=CARTESIAN_POINT('Ctrl Pts',(16.8773883160933,-21.3477770553498,
11.315341099525));
#212626=CARTESIAN_POINT('Ctrl Pts',(15.7145819453165,-18.6876720695586,
11.4425169062065));
#212627=CARTESIAN_POINT('Ctrl Pts',(17.321904233492,-16.2700715539058,11.569692712888));
#212628=CARTESIAN_POINT('Ctrl Pts',(20.2247367428907,-16.3129739282918,
11.6968685195694));
#212629=CARTESIAN_POINT('Ctrl Pts',(21.7599108162444,-18.7770189270395,
11.8240443262509));
#212630=CARTESIAN_POINT('Ctrl Pts',(20.5189995249001,-21.4015981996781,
11.9512201329323));
#212631=CARTESIAN_POINT('Ctrl Pts',(17.6404619590251,-21.7788231633232,
12.0783959396136));
#212632=CARTESIAN_POINT('Ctrl Pts',(15.7651776731192,-19.5626133270522,
12.2055717462952));
#212633=CARTESIAN_POINT('Ctrl Pts',(16.6136036062314,-16.7862036621481,
12.3327475529766));
#212634=CARTESIAN_POINT('Ctrl Pts',(19.4073616239837,-15.9967777127422,
12.459923359658));
#212635=CARTESIAN_POINT('Ctrl Pts',(21.5833521452667,-17.9185847901141,
12.5870991663395));
#212636=CARTESIAN_POINT('Ctrl Pts',(21.1452389240066,-20.7884861815747,
12.7142749730209));
#212637=CARTESIAN_POINT('Ctrl Pts',(18.4949636483364,-21.9735254866281,
12.8414507797022));
#212638=CARTESIAN_POINT('Ctrl Pts',(16.0639893890483,-20.3865026947222,
12.9686265863838));
#212639=CARTESIAN_POINT('Ctrl Pts',(16.0825841457601,-17.4834127156872,
13.0958023930652));
#212640=CARTESIAN_POINT('Ctrl Pts',(18.5336883833095,-15.9276604192025,
13.2229781997466));
#212641=CARTESIAN_POINT('Ctrl Pts',(21.1685660964313,-17.1465519764151,
13.3501540064281));
#212642=CARTESIAN_POINT('Ctrl Pts',(21.5698805222909,-20.0218300365248,
13.4773298131095));
#212643=CARTESIAN_POINT('Ctrl Pts',(19.3694505835445,-21.9156054392635,
13.604505619791));
#212644=CARTESIAN_POINT('Ctrl Pts',(16.5860341749072,-21.0904567935765,
13.7316814264724));
#212645=CARTESIAN_POINT('Ctrl Pts',(15.773243092998,-18.3034067673804,13.8588572331538));
#212646=CARTESIAN_POINT('Ctrl Pts',(17.6767627079645,-16.1114007758768,
13.9860330398352));
#212647=CARTESIAN_POINT('Ctrl Pts',(20.5502319188267,-16.5254682650346,
14.1132088465167));
#212648=CARTESIAN_POINT('Ctrl Pts',(21.7574210722316,-19.1657280134782,
14.2403846531981));
#212649=CARTESIAN_POINT('Ctrl Pts',(20.1908090465392,-21.6099055750122,
14.3675604598796));
#212650=CARTESIAN_POINT('Ctrl Pts',(17.2876651404139,-21.6156197396974,
14.494736266561));
#212651=CARTESIAN_POINT('Ctrl Pts',(15.7114436982933,-19.1776281160963,
14.6219120732424));
#212652=CARTESIAN_POINT('Ctrl Pts',(16.9082300619871,-16.532636700037,14.7490878799238));
#212653=CARTESIAN_POINT('Ctrl Pts',(19.7800470237451,-16.1072609490722,
14.8762636866053));
#212654=CARTESIAN_POINT('Ctrl Pts',(21.6921807662175,-18.2917567129154,
15.0034394932867));
#212655=CARTESIAN_POINT('Ctrl Pts',(20.8903672610905,-21.0819847133387,
15.1306152999681));
#212656=CARTESIAN_POINT('Ctrl Pts',(18.1102206331594,-21.9180839410347,
15.2577911066496));
#212657=CARTESIAN_POINT('Ctrl Pts',(15.9023528581907,-20.0329852487628,
15.384966913331));
#212658=CARTESIAN_POINT('Ctrl Pts',(16.2923455839892,-17.1561496842624,
15.5121427200124));
#212659=CARTESIAN_POINT('Ctrl Pts',(18.9224046903134,-15.9268953214099,
15.6393185266939));
#212660=CARTESIAN_POINT('Ctrl Pts',(21.3796141869889,-17.4729867419922,
15.7664943333753));
#212661=CARTESIAN_POINT('Ctrl Pts',(21.4096368724374,-20.375981028881,15.8936701400568));
#212662=CARTESIAN_POINT('Ctrl Pts',(18.9849287961779,-21.9725611040017,
16.0208459467382));
#212663=CARTESIAN_POINT('Ctrl Pts',(16.3300091238228,-20.7979638433666,
16.1480217534196));
#212664=CARTESIAN_POINT('Ctrl Pts',(15.8806018718589,-17.9298093298801,
16.2751975601011));
#212665=CARTESIAN_POINT('Ctrl Pts',(18.0490103006032,-15.9994513119205,
16.4023733667825));
#212666=CARTESIAN_POINT('Ctrl Pts',(20.8458542632885,-16.7778734594348,
16.5295491734639));
#212667=CARTESIAN_POINT('Ctrl Pts',(21.7052030158649,-19.5509217664062,
16.6567249801454));
#212668=CARTESIAN_POINT('Ctrl Pts',(19.8386574150423,-21.7744965259768,
16.7839007868268));
#212669=CARTESIAN_POINT('Ctrl Pts',(16.9586571986901,-21.4086059068554,
16.9110765935082));
#212670=CARTESIAN_POINT('Ctrl Pts',(15.7074238123383,-18.7889318423525,
17.0382524001897));
#212671=CARTESIAN_POINT('Ctrl Pts',(17.2328862276622,-16.3188626913401,
17.1654282068711));
#212672=CARTESIAN_POINT('Ctrl Pts',(20.135527359478,-16.2645335900898,17.2926040135526));
#212673=CARTESIAN_POINT('Ctrl Pts',(21.7523541275707,-18.6757881169556,
17.4197798202339));
#212674=CARTESIAN_POINT('Ctrl Pts',(20.6000283238033,-21.3404499028704,
17.5469556269154));
#212675=CARTESIAN_POINT('Ctrl Pts',(17.7357373517245,-21.8138571468239,
17.6741314335968));
#212676=CARTESIAN_POINT('Ctrl Pts',(15.7872904002738,-19.6616880854488,
17.8013072402783));
#212677=CARTESIAN_POINT('Ctrl Pts',(16.5422666131419,-16.8584242538939,
17.9284830469597));
#212678=CARTESIAN_POINT('Ctrl Pts',(19.3080221741474,-15.9758862274083,
18.0556588536411));
#212679=CARTESIAN_POINT('Ctrl Pts',(21.5471480181857,-17.8237478688561,
18.1828346603226));
#212680=CARTESIAN_POINT('Ctrl Pts',(21.2053851592371,-20.7067108133391,
18.310010467004));
#212681=CARTESIAN_POINT('Ctrl Pts',(18.5962798080717,-21.9798354963434,
18.4371862736854));
#212682=CARTESIAN_POINT('Ctrl Pts',(16.1135241852737,-20.4751090398787,
18.5643620803669));
#212683=CARTESIAN_POINT('Ctrl Pts',(16.0348924771216,-17.5730245745949,
18.6915378870483));
#212684=CARTESIAN_POINT('Ctrl Pts',(18.4325243962693,-15.9360644723642,
18.8187136937297));
#212685=CARTESIAN_POINT('Ctrl Pts',(21.1067414690649,-17.0660380283814,
18.9458895004112));
#212686=CARTESIAN_POINT('Ctrl Pts',(21.6041155150354,-19.9262646340588,
19.0730653070926));
#212687=CARTESIAN_POINT('Ctrl Pts',(19.4683367113789,-21.8926639140248,
19.200241113774));
#212688=CARTESIAN_POINT('Ctrl Pts',(16.6588495608948,-21.1611865588169,
19.3274169204555));
#212689=CARTESIAN_POINT('Ctrl Pts',(15.7531841249269,-18.4029176770637,
19.4545927271369));
#212690=CARTESIAN_POINT('Ctrl Pts',(17.582232272941,-16.148397701268,19.5817685338184));
#212691=CARTESIAN_POINT('Ctrl Pts',(20.4679557680829,-16.4660089109295,
19.7089443404998));
#212692=CARTESIAN_POINT('Ctrl Pts',(21.762882574719,-19.0643624781199,19.8361201471812));
#212693=CARTESIAN_POINT('Ctrl Pts',(20.278997406019,-21.5596307706316,19.9632959538627));
#212694=CARTESIAN_POINT('Ctrl Pts',(17.3776734088588,-21.662559052761,20.0904717605441));
#212695=CARTESIAN_POINT('Ctrl Pts',(15.7206941087448,-19.2787188466078,
20.2176475672255));
#212696=CARTESIAN_POINT('Ctrl Pts',(16.828237415124,-16.5951320529376,20.344823373907));
#212697=CARTESIAN_POINT('Ctrl Pts',(19.6841967603538,-16.0738297948901,
20.4719991805884));
#212698=CARTESIAN_POINT('Ctrl Pts',(21.6684150405127,-18.1930614333217,
20.5991749872697));
#212699=CARTESIAN_POINT('Ctrl Pts',(20.9604790804735,-21.0085887233582,
20.7263507939513));
#212700=CARTESIAN_POINT('Ctrl Pts',(18.2099071212035,-21.9372914819773,
20.8535266006327));
#212701=CARTESIAN_POINT('Ctrl Pts',(15.9401186110067,-20.1272362927054,
20.9807024073141));
#212702=CARTESIAN_POINT('Ctrl Pts',(16.2336184655874,-17.2388558767421,
21.1078782139956));
#212703=CARTESIAN_POINT('Ctrl Pts',(18.8209175351634,-15.9224078905259,
21.2350540206769));
#212704=CARTESIAN_POINT('Ctrl Pts',(21.3287557911663,-17.3849813380486,
21.3622298273584));
#212705=CARTESIAN_POINT('Ctrl Pts',(21.4555258683986,-20.286047713047,21.4894056340398));
#212706=CARTESIAN_POINT('Ctrl Pts',(19.0865078830173,-21.9615659646048,
21.6165814407213));
#212707=CARTESIAN_POINT('Ctrl Pts',(16.3920659006521,-20.879190353892,21.7437572474027));
#212708=CARTESIAN_POINT('Ctrl Pts',(15.8501931440795,-18.0222746586101,
21.8709330540842));
#212709=CARTESIAN_POINT('Ctrl Pts',(17.2469900335074,-16.6964452121458,
21.9557169252051));
#212710=CARTESIAN_POINT('Ctrl Pts',(18.0714160310384,-16.4758408723594,
21.9981088607656));
#212711=CARTESIAN_POINT('Ctrl Pts',(20.3539256943887,-17.5890877707427,
-4.33680868994202E-19));
#212712=CARTESIAN_POINT('Ctrl Pts',(20.4076089239479,-17.6408883813468,
1.14879278225653E-14));
#212713=CARTESIAN_POINT('Ctrl Pts',(20.4581355958119,-17.6955615793788,
3.22355904239226E-15));
#212714=CARTESIAN_POINT('Ctrl Pts',(20.505511977026,-17.7527360595703,3.08607306376274E-15));
#212715=CARTESIAN_POINT('Ctrl Pts',(20.5545756607811,-17.8119468000931,
2.94369054311896E-15));
#212716=CARTESIAN_POINT('Ctrl Pts',(20.6002611686401,-17.873840595982,1.23841336720853E-14));
#212717=CARTESIAN_POINT('Ctrl Pts',(20.6425471220966,-17.9380546484764,
1.20702059458466E-14));
#212718=CARTESIAN_POINT('Ctrl Pts',(20.6826816235519,-17.9990015770098,
1.17722504368497E-14));
#212719=CARTESIAN_POINT('Ctrl Pts',(20.7197537535956,-18.0620396014582,
1.56295612152767E-14));
#212720=CARTESIAN_POINT('Ctrl Pts',(20.7537167666138,-18.1268912820608,
3.65679708735911E-15));
#212721=CARTESIAN_POINT('Ctrl Pts',(20.7688150878339,-18.1557212184648,
-1.85535512480841E-15));
#212722=CARTESIAN_POINT('Ctrl Pts',(20.7832985724702,-18.1849099468526,
-9.481700208412E-17));
#212723=CARTESIAN_POINT('Ctrl Pts',(20.7971611207678,-18.2144346312911,
-4.68375338513738E-15));
#212724=CARTESIAN_POINT('Ctrl Pts',(20.8057380545325,-18.2327019265545,
-7.25563266417811E-15));
#212725=CARTESIAN_POINT('Ctrl Pts',(20.8140776656103,-18.2510987616938,
5.43075649196809E-15));
#212726=CARTESIAN_POINT('Ctrl Pts',(20.8221770088969,-18.269617013417,1.47659662275146E-14));
#212727=CARTESIAN_POINT('Ctrl Pts',(20.8264660877165,-18.2794235172817,
1.97095090477139E-14));
#212728=CARTESIAN_POINT('Ctrl Pts',(20.8306870781385,-18.2892625308288,
2.34250044198635E-14));
#212729=CARTESIAN_POINT('Ctrl Pts',(20.8348368140281,-18.2991258749815,
2.40155118014229E-14));
#212730=CARTESIAN_POINT('Ctrl Pts',(20.8659056770803,-18.372972234574,2.92160735740311E-14));
#212731=CARTESIAN_POINT('Ctrl Pts',(20.8930393303568,-18.4483069573626,
1.37453420125155E-14));
#212732=CARTESIAN_POINT('Ctrl Pts',(20.9162161420459,-18.5247489058203,
2.05252481677576E-14));
#212733=CARTESIAN_POINT('Ctrl Pts',(20.9398193164082,-18.6025970871082,
2.74298780749852E-14));
#212734=CARTESIAN_POINT('Ctrl Pts',(20.9593192432915,-18.6815944151039,
-7.79267749674098E-15));
#212735=CARTESIAN_POINT('Ctrl Pts',(20.9746521798114,-18.7613738906736,
2.88657986402541E-15));
#212736=CARTESIAN_POINT('Ctrl Pts',(20.9885844406082,-18.8338654488575,
1.25902787264266E-14));
#212737=CARTESIAN_POINT('Ctrl Pts',(20.9990759862006,-18.9070037360458,
7.24757628038241E-15));
#212738=CARTESIAN_POINT('Ctrl Pts',(21.0060452061984,-18.9805292501327,
6.84174938925253E-15));
#212739=CARTESIAN_POINT('Ctrl Pts',(21.0087031403799,-19.0085705484655,
6.67475528854553E-15));
#212740=CARTESIAN_POINT('Ctrl Pts',(21.0108483899423,-19.0366682762212,
1.44685164024077E-15));
#212741=CARTESIAN_POINT('Ctrl Pts',(21.0124750673575,-19.0648083237754,
9.10382880192628E-15));
#212742=CARTESIAN_POINT('Ctrl Pts',(21.0133685834701,-19.0802653441188,
1.32694517658755E-14));
#212743=CARTESIAN_POINT('Ctrl Pts',(21.014105623128,-19.0957351348357,1.68885348715346E-14));
#212744=CARTESIAN_POINT('Ctrl Pts',(21.0146851084115,-19.1112153648711,
-3.7470027081099E-15));
#212745=CARTESIAN_POINT('Ctrl Pts',(21.0151328224698,-19.1231754901941,
-2.01423518057422E-14));
#212746=CARTESIAN_POINT('Ctrl Pts',(21.0154863189935,-19.1351385470168,
5.5845216903151E-15));
#212747=CARTESIAN_POINT('Ctrl Pts',(21.0157451770828,-19.1470949182306,
6.34214902817121E-15));
#212748=CARTESIAN_POINT('Ctrl Pts',(21.0175519249061,-19.2305466184455,
1.17423994501049E-14));
#212749=CARTESIAN_POINT('Ctrl Pts',(21.0147568373932,-19.3137920798114,
-1.49327707601934E-14));
#212750=CARTESIAN_POINT('Ctrl Pts',(21.0073036695044,-19.3964506692726,
-1.12410081243297E-14));
#212751=CARTESIAN_POINT('Ctrl Pts',(20.9998648261745,-19.4789503936919,
-7.14671687260285E-15));
#212752=CARTESIAN_POINT('Ctrl Pts',(20.9877861648147,-19.5608665038776,
-8.09133270479139E-15));
#212753=CARTESIAN_POINT('Ctrl Pts',(20.9709624036051,-19.6418361818354,
-1.15740750317173E-14));
#212754=CARTESIAN_POINT('Ctrl Pts',(20.9545246825771,-19.7209479191819,
-1.49826315955414E-14));
#212755=CARTESIAN_POINT('Ctrl Pts',(20.9335573448041,-19.799157111958,-9.03506803208643E-15));
#212756=CARTESIAN_POINT('Ctrl Pts',(20.9083260528412,-19.8762372781696,
-1.765254609154E-14));
#212757=CARTESIAN_POINT('Ctrl Pts',(20.8979286223519,-19.9080008387303,
-2.11749609793981E-14));
#212758=CARTESIAN_POINT('Ctrl Pts',(20.886806496403,-19.9395726045308,-6.78433755510298E-15));
#212759=CARTESIAN_POINT('Ctrl Pts',(20.8749757808311,-19.9709362516545,
5.4678483962789E-15));
#212760=CARTESIAN_POINT('Ctrl Pts',(20.8684245113494,-19.9883038997047,
1.2315661009052E-14));
#212761=CARTESIAN_POINT('Ctrl Pts',(20.8616537141196,-20.0056128698145,
-8.32710061231184E-15));
#212762=CARTESIAN_POINT('Ctrl Pts',(20.8546785166995,-20.0228303119358,
-5.13478148889135E-15));
#212763=CARTESIAN_POINT('Ctrl Pts',(20.8236218670382,-20.0994899440325,
8.84067847874355E-15));
#212764=CARTESIAN_POINT('Ctrl Pts',(20.7884837604207,-20.1744320701159,
2.95709367352313E-15));
#212765=CARTESIAN_POINT('Ctrl Pts',(20.7495952387339,-20.247430956818,1.0019762797242E-14));
#212766=CARTESIAN_POINT('Ctrl Pts',(20.7099066604874,-20.3219316552531,
1.72277327582215E-14));
#212767=CARTESIAN_POINT('Ctrl Pts',(20.6663114480379,-20.3944090798839,
-1.83234150877214E-14));
#212768=CARTESIAN_POINT('Ctrl Pts',(20.6191066061375,-20.4646182429735,
-4.46864767411626E-15));
#212769=CARTESIAN_POINT('Ctrl Pts',(20.571128607974,-20.535977344332,9.61304349920823E-15));
#212770=CARTESIAN_POINT('Ctrl Pts',(20.5194213554847,-20.6049941328661,
2.46291640853547E-15));
#212771=CARTESIAN_POINT('Ctrl Pts',(20.4642461984926,-20.6713939737934,
-2.96984659087229E-15));
#212772=CARTESIAN_POINT('Ctrl Pts',(20.440364318256,-20.7001343188184,-5.32135046289197E-15));
#212773=CARTESIAN_POINT('Ctrl Pts',(20.4158321356603,-20.7283840869128,
-6.72565667072835E-15));
#212774=CARTESIAN_POINT('Ctrl Pts',(20.3906682941055,-20.7561193805442,
-3.1641356201817E-15));
#212775=CARTESIAN_POINT('Ctrl Pts',(20.3815365270621,-20.7661843080224,
-1.76561806683548E-15));
#212776=CARTESIAN_POINT('Ctrl Pts',(20.3723208078371,-20.7761822779911,
4.05228345890246E-16));
#212777=CARTESIAN_POINT('Ctrl Pts',(20.3630243316464,-20.7861096027615,
-2.22044604925031E-16));
#212778=CARTESIAN_POINT('Ctrl Pts',(20.3025147033051,-20.8507253474758,
-4.84969820433169E-15));
#212779=CARTESIAN_POINT('Ctrl Pts',(20.2387852854453,-20.9121400047012,
-1.86639630302913E-14));
#212780=CARTESIAN_POINT('Ctrl Pts',(20.1721441659296,-20.9700792099884,
-2.05391259555654E-14));
#212781=CARTESIAN_POINT('Ctrl Pts',(20.1169512585411,-21.0180650964023,
-2.20921564932416E-14));
#212782=CARTESIAN_POINT('Ctrl Pts',(20.0597599950038,-21.0636670219304,
-1.76874795853289E-14));
#212783=CARTESIAN_POINT('Ctrl Pts',(20.0007222397457,-21.1067151539364,
-1.05748743095546E-14));
#212784=CARTESIAN_POINT('Ctrl Pts',(19.9812253420094,-21.1209315655156,
-8.39014400518185E-15));
#212785=CARTESIAN_POINT('Ctrl Pts',(19.9615269106471,-21.1348693297411,
1.57955388576365E-14));
#212786=CARTESIAN_POINT('Ctrl Pts',(19.941631987048,-21.1485219218181,5.80091530366644E-15));
#212787=CARTESIAN_POINT('Ctrl Pts',(19.9257068710437,-21.1594502931437,
-2.07749129685265E-15));
#212788=CARTESIAN_POINT('Ctrl Pts',(19.9096544895287,-21.170196697329,-1.40009963692834E-14));
#212789=CARTESIAN_POINT('Ctrl Pts',(19.8934933729568,-21.1807476067171,
-1.42386102908176E-14));
#212790=CARTESIAN_POINT('Ctrl Pts',(19.8189655561075,-21.2294036657816,
-1.49307265937708E-14));
#212791=CARTESIAN_POINT('Ctrl Pts',(19.7420556060774,-21.2739560343907,
-1.3588777424594E-14));
#212792=CARTESIAN_POINT('Ctrl Pts',(19.6630443896218,-21.3141141071315,
-1.16295861829485E-14));
#212793=CARTESIAN_POINT('Ctrl Pts',(19.585203146919,-21.3536775315024,-9.64882108030855E-15));
#212794=CARTESIAN_POINT('Ctrl Pts',(19.5053217267533,-21.3889765584864,
-2.19053443386609E-14));
#212795=CARTESIAN_POINT('Ctrl Pts',(19.4236362626317,-21.4196959407397,
-5.55111512312578E-17));
#212796=CARTESIAN_POINT('Ctrl Pts',(19.4149414973774,-21.4229657736325,
2.2126898693708E-15));
#212797=CARTESIAN_POINT('Ctrl Pts',(19.4062262673531,-21.4261836782215,
-3.67255004627579E-14));
#212798=CARTESIAN_POINT('Ctrl Pts',(19.3974909880357,-21.4293497847436,
-2.27595720048157E-15));
#212799=CARTESIAN_POINT('Ctrl Pts',(18.0714161019496,-21.428158862637,0.00189098085166763));
#212800=CARTESIAN_POINT('Ctrl Pts',(17.2469901926503,-21.2075545464601,
0.0442829164121458));
#212801=CARTESIAN_POINT('Ctrl Pts',(15.8501939821074,-19.8817220316731,
0.129066787533101));
#212802=CARTESIAN_POINT('Ctrl Pts',(16.3920656827787,-17.0248116182672,
0.256242594214536));
#212803=CARTESIAN_POINT('Ctrl Pts',(19.0865079334355,-15.9424330181619,
0.38341840089597));
#212804=CARTESIAN_POINT('Ctrl Pts',(21.4555257912919,-17.6179530146914,
0.510594207577404));
#212805=CARTESIAN_POINT('Ctrl Pts',(21.3287556480917,-20.5190182015967,
0.63777001425884));
#212806=CARTESIAN_POINT('Ctrl Pts',(18.8209175719769,-21.9815922294721,
0.764945820940273));
#212807=CARTESIAN_POINT('Ctrl Pts',(16.2336185304982,-20.6651439233068,
0.892121627621708));
#212808=CARTESIAN_POINT('Ctrl Pts',(15.9401187363004,-17.7767638289518,
1.01929743430314));
#212809=CARTESIAN_POINT('Ctrl Pts',(18.2099071283678,-15.9667085869429,
1.14647324098458));
#212810=CARTESIAN_POINT('Ctrl Pts',(20.9604790041794,-16.8954113789202,
1.27364904766601));
#212811=CARTESIAN_POINT('Ctrl Pts',(21.6684149250655,-19.7109385242504,
1.40082485434745));
#212812=CARTESIAN_POINT('Ctrl Pts',(19.6841967272255,-21.8301701041092,
1.52800066102888));
#212813=CARTESIAN_POINT('Ctrl Pts',(16.8282374854801,-21.3088678538367,
1.65517646771032));
#212814=CARTESIAN_POINT('Ctrl Pts',(15.720694223426,-18.6252811680681,1.78235227439175));
#212815=CARTESIAN_POINT('Ctrl Pts',(17.3776734595451,-16.2414410482877,
1.90952808107318));
#212816=CARTESIAN_POINT('Ctrl Pts',(20.2789973479827,-16.3443693285228,
2.03670388775462));
#212817=CARTESIAN_POINT('Ctrl Pts',(21.7628824602006,-18.839637525737,2.16387969443605));
#212818=CARTESIAN_POINT('Ctrl Pts',(20.4679557027106,-21.4379909954235,
2.29105550111749));
#212819=CARTESIAN_POINT('Ctrl Pts',(17.5822323163742,-21.7556021927696,
2.41823130779892));
#212820=CARTESIAN_POINT('Ctrl Pts',(15.7531842374939,-19.5010823022681,
2.54540711448036));
#212821=CARTESIAN_POINT('Ctrl Pts',(16.6588496392251,-16.7428135245559,
2.67258292116179));
#212822=CARTESIAN_POINT('Ctrl Pts',(19.468336683663,-16.0113361970163,2.79975872784322));
#212823=CARTESIAN_POINT('Ctrl Pts',(21.6041154066714,-17.977735402714,2.92693453452466));
#212824=CARTESIAN_POINT('Ctrl Pts',(21.1067413794861,-20.8379619004206,
3.05411034120609));
#212825=CARTESIAN_POINT('Ctrl Pts',(18.43252440765,-21.9679354137682,3.18128614788753));
#212826=CARTESIAN_POINT('Ctrl Pts',(16.0348925790254,-20.3309753733442,
3.30846195456896));
#212827=CARTESIAN_POINT('Ctrl Pts',(16.1135242842076,-17.4288910176245,
3.43563776125039));
#212828=CARTESIAN_POINT('Ctrl Pts',(18.5962798132715,-15.924164617971,3.56281356793183));
#212829=CARTESIAN_POINT('Ctrl Pts',(21.2053850659314,-17.1972892529086,
3.68998937461327));
#212830=CARTESIAN_POINT('Ctrl Pts',(21.5471479119772,-20.0802520885476,
3.8171651812947));
#212831=CARTESIAN_POINT('Ctrl Pts',(19.3080221524756,-21.9281136602303,
3.94434098797614));
#212832=CARTESIAN_POINT('Ctrl Pts',(16.5422666958893,-21.0455756670647,
4.07151679465757));
#212833=CARTESIAN_POINT('Ctrl Pts',(15.7872905115249,-18.242311941345,4.198692601339));
#212834=CARTESIAN_POINT('Ctrl Pts',(17.7357373894132,-16.0901429612237,
4.32586840802044));
#212835=CARTESIAN_POINT('Ctrl Pts',(20.6000282533525,-16.5635501873038,
4.45304421470187));
#212836=CARTESIAN_POINT('Ctrl Pts',(21.7523540136146,-19.2282118726162,
4.5802200213833));
#212837=CARTESIAN_POINT('Ctrl Pts',(20.1355273065643,-21.6394663084466,
4.70739582806474));
#212838=CARTESIAN_POINT('Ctrl Pts',(17.2328862843358,-21.5851372092476,
4.83457163474617));
#212839=CARTESIAN_POINT('Ctrl Pts',(15.7074239266047,-19.115068151491,4.96174744142761));
#212840=CARTESIAN_POINT('Ctrl Pts',(16.9586572657169,-16.4953941858922,
5.08892324810904));
#212841=CARTESIAN_POINT('Ctrl Pts',(19.8386573733367,-16.1295035805846,
5.21609905479048));
#212842=CARTESIAN_POINT('Ctrl Pts',(21.705202903689,-18.3530782562058,5.34327486147191));
#212843=CARTESIAN_POINT('Ctrl Pts',(20.8458541835568,-21.1261264584823,
5.47045066815334));
#212844=CARTESIAN_POINT('Ctrl Pts',(18.0490103264645,-21.9045485766079,
5.59762647483478));
#212845=CARTESIAN_POINT('Ctrl Pts',(15.8806019795871,-19.9741906315278,
5.72480228151621));
#212846=CARTESIAN_POINT('Ctrl Pts',(16.3300092145838,-17.1060362263267,
5.85197808819766));
#212847=CARTESIAN_POINT('Ctrl Pts',(18.9849287867042,-15.9314390100375,
5.97915389487907));
#212848=CARTESIAN_POINT('Ctrl Pts',(21.4096367714204,-17.5280190248805,
6.10632970156052));
#212849=CARTESIAN_POINT('Ctrl Pts',(21.3796140871054,-20.4310132021685,
6.23350550824194));
#212850=CARTESIAN_POINT('Ctrl Pts',(18.9224046832003,-21.9771045643792,
6.36068131492339));
#212851=CARTESIAN_POINT('Ctrl Pts',(16.2923456761723,-20.7478502479364,
6.48785712160482));
#212852=CARTESIAN_POINT('Ctrl Pts',(15.9023529650977,-17.8710147920491,
6.61503292828625));
#212853=CARTESIAN_POINT('Ctrl Pts',(18.1102206567097,-15.9859161709479,
6.74220873496769));
#212854=CARTESIAN_POINT('Ctrl Pts',(20.8903671796782,-16.8220153670774,
6.86938454164913));
#212855=CARTESIAN_POINT('Ctrl Pts',(21.6921806545333,-19.6122432621575,
6.99656034833056));
#212856=CARTESIAN_POINT('Ctrl Pts',(19.7800469842523,-21.7967389435265,
7.12373615501199));
#212857=CARTESIAN_POINT('Ctrl Pts',(16.9082301309179,-21.3713632086215,
7.25091196169343));
#212858=CARTESIAN_POINT('Ctrl Pts',(15.711443812408,-18.7263718924222,7.37808776837486));
#212859=CARTESIAN_POINT('Ctrl Pts',(17.2876651950193,-16.2883803608658,
7.5052635750563));
#212860=CARTESIAN_POINT('Ctrl Pts',(20.1908089915383,-16.2940945253353,
7.63243938173773));
#212861=CARTESIAN_POINT('Ctrl Pts',(21.7574209580843,-18.7382719945909,
7.75961518841917));
#212862=CARTESIAN_POINT('Ctrl Pts',(20.5502318502561,-21.3785316433533,
7.8867909951006));
#212863=CARTESIAN_POINT('Ctrl Pts',(17.6767627478799,-21.7925991168781,
8.01396680178203));
#212864=CARTESIAN_POINT('Ctrl Pts',(15.7732432047795,-19.6005932081323,
8.14114260846348));
#212865=CARTESIAN_POINT('Ctrl Pts',(16.5860342560023,-16.8135432871596,
8.26831841514489));
#212866=CARTESIAN_POINT('Ctrl Pts',(19.3694505595535,-15.9883946726254,
8.39549422182634));
#212867=CARTESIAN_POINT('Ctrl Pts',(21.5698804152241,-17.8821700038661,
8.52267002850777));
#212868=CARTESIAN_POINT('Ctrl Pts',(21.1685660045158,-20.7574479554213,
8.6498458351892));
#212869=CARTESIAN_POINT('Ctrl Pts',(18.5336883908723,-21.9763394666155,
8.77702164187065));
#212870=CARTESIAN_POINT('Ctrl Pts',(16.0825842458626,-20.4205872288672,
8.90419744855206));
#212871=CARTESIAN_POINT('Ctrl Pts',(16.0639894898528,-17.5174973594366,
9.03137325523352));
#212872=CARTESIAN_POINT('Ctrl Pts',(18.4949636573611,-15.9304746274477,
9.15854906191495));
#212873=CARTESIAN_POINT('Ctrl Pts',(21.1452388329719,-17.1155138877607,
9.28572486859637));
#212874=CARTESIAN_POINT('Ctrl Pts',(21.5833520376912,-19.98541517087,9.4129006752778));
#212875=CARTESIAN_POINT('Ctrl Pts',(19.4073615985613,-21.9072221756853,
9.54007648195925));
#212876=CARTESIAN_POINT('Ctrl Pts',(16.6136036862856,-21.1177962560837,
9.66725228864067));
#212877=CARTESIAN_POINT('Ctrl Pts',(15.7651777852051,-18.3413866960012,
9.79442809532212));
#212878=CARTESIAN_POINT('Ctrl Pts',(17.6404620003109,-16.1251769434017,
9.92160390200354));
#212879=CARTESIAN_POINT('Ctrl Pts',(20.5189994575086,-16.5024018928049,
10.048779708685));
#212880=CARTESIAN_POINT('Ctrl Pts',(21.7599107020031,-19.1269810663543,
10.1759555153665));
#212881=CARTESIAN_POINT('Ctrl Pts',(20.2247366866089,-21.5910259720733,
10.3031313220479));
#212882=CARTESIAN_POINT('Ctrl Pts',(17.3219042868047,-21.6339283448398,
10.4303071287293));
#212883=CARTESIAN_POINT('Ctrl Pts',(15.7145820593127,-19.2163279204619,
10.5574829354107));
#212884=CARTESIAN_POINT('Ctrl Pts',(16.8773883861884,-16.5562230351012,
10.6846587420922));
#212885=CARTESIAN_POINT('Ctrl Pts',(19.7435206344235,-16.0940948163466,
10.8118345487736));
#212886=CARTESIAN_POINT('Ctrl Pts',(21.683480358492,-18.2539172219934,10.9390103554551));
#212887=CARTESIAN_POINT('Ctrl Pts',(20.9174749190411,-21.0541872485576,
11.0661861621365));
#212888=CARTESIAN_POINT('Ctrl Pts',(18.1482667631075,-21.9258309510259,
11.1933619688179));
#212889=CARTESIAN_POINT('Ctrl Pts',(15.9164324973179,-20.069169332693,11.3205377754993));
#212890=CARTESIAN_POINT('Ctrl Pts',(16.2695415372774,-17.1875741909633,
11.4477135821808));
#212891=CARTESIAN_POINT('Ctrl Pts',(18.8836382552418,-15.9247302164082,
11.5748893888622));
#212892=CARTESIAN_POINT('Ctrl Pts',(21.3604511616193,-17.4392183747454,
11.7020651955437));
#212893=CARTESIAN_POINT('Ctrl Pts',(21.427658143155,-20.3415897804367,11.8292410022251));
#212894=CARTESIAN_POINT('Ctrl Pts',(19.0236009656254,-21.9690988102461,
11.9564168089065));
#212895=CARTESIAN_POINT('Ctrl Pts',(16.3538528767977,-20.828606943926,12.083592615588));
#212896=CARTESIAN_POINT('Ctrl Pts',(15.8677420449167,-17.9664446819167,
12.2107684222694));
#212897=CARTESIAN_POINT('Ctrl Pts',(18.0112449867927,-16.008468253787,12.3379442289508));
#212898=CARTESIAN_POINT('Ctrl Pts',(20.817830794051,-16.7509995066233,12.4651200356323));
#212899=CARTESIAN_POINT('Ctrl Pts',(21.712631184893,-19.5128121026353,12.5922958423137));
#212900=CARTESIAN_POINT('Ctrl Pts',(19.874722338297,-21.7601144024042,12.7194716489951));
#212901=CARTESIAN_POINT('Ctrl Pts',(16.9902715475267,-21.4311460292034,
12.8466474556766));
#212902=CARTESIAN_POINT('Ctrl Pts',(15.7055833839069,-18.8277150473647,
12.973823262358));
#212903=CARTESIAN_POINT('Ctrl Pts',(17.1992795008189,-16.3383077955748,
13.1009990690394));
#212904=CARTESIAN_POINT('Ctrl Pts',(20.1009864202325,-16.2468009173113,
13.2281748757209));
#212905=CARTESIAN_POINT('Ctrl Pts',(21.7485681438287,-18.6371462938237,
13.3553506824023));
#212906=CARTESIAN_POINT('Ctrl Pts',(20.6304707006625,-21.3163504037278,
13.4825264890837));
#212907=CARTESIAN_POINT('Ctrl Pts',(17.7724790978853,-21.8264097663479,
13.6097022957652));
#212908=CARTESIAN_POINT('Ctrl Pts',(15.7966232440805,-19.6993765743343,
13.7368781024466));
#212909=CARTESIAN_POINT('Ctrl Pts',(16.5156282496692,-16.8866717627907,
13.864053909128));
#212910=CARTESIAN_POINT('Ctrl Pts',(19.2698516485073,-15.9687774201593,
13.9912297158095));
#212911=CARTESIAN_POINT('Ctrl Pts',(21.532464418544,-17.7878046348562,14.1184055224909));
#212912=CARTESIAN_POINT('Ctrl Pts',(21.2276597768573,-20.674908838959,14.2455813291723));
#212913=CARTESIAN_POINT('Ctrl Pts',(18.6350770638849,-21.9813511190996,
14.3727571358538));
#212914=CARTESIAN_POINT('Ctrl Pts',(16.1332500049482,-20.5085517702016,
14.4999329425352));
#212915=CARTESIAN_POINT('Ctrl Pts',(16.0174496457219,-17.6077127826422,
14.6271087492167));
#212916=CARTESIAN_POINT('Ctrl Pts',(18.3939156284153,-15.940173881134,14.7542845558981));
#212917=CARTESIAN_POINT('Ctrl Pts',(21.082387914021,-17.0357985086741,14.8814603625795));
#212918=CARTESIAN_POINT('Ctrl Pts',(21.6163600459046,-19.889419071628,15.008636169261));
#212919=CARTESIAN_POINT('Ctrl Pts',(19.5059457351114,-21.8830158191527,
15.1358119759424));
#212920=CARTESIAN_POINT('Ctrl Pts',(16.6873191247092,-21.1875874719631,
15.2629877826238));
#212921=CARTESIAN_POINT('Ctrl Pts',(15.7463951860447,-18.4411463754548,
15.3901635893052));
#212922=CARTESIAN_POINT('Ctrl Pts',(17.5464132325167,-16.1633817723147,
15.5173393959867));
#212923=CARTESIAN_POINT('Ctrl Pts',(20.4359684282068,-16.4440013119089,
15.6445152026681));
#212924=CARTESIAN_POINT('Ctrl Pts',(21.7640732270913,-19.0255539838723,
15.7716910093496));
#212925=CARTESIAN_POINT('Ctrl Pts',(20.3122739076741,-21.539625440908,15.898866816031));
#212926=CARTESIAN_POINT('Ctrl Pts',(17.4125062366922,-21.6797111620585,
16.0260426227124));
#212927=CARTESIAN_POINT('Ctrl Pts',(15.725127072392,-19.3172911928685,16.1532184293939));
#212928=CARTESIAN_POINT('Ctrl Pts',(16.7982020674565,-16.6197392267502,
16.2803942360753));
#212929=CARTESIAN_POINT('Ctrl Pts',(19.6472515164596,-16.0618917636594,
16.4075700427567));
#212930=CARTESIAN_POINT('Ctrl Pts',(21.6584493818928,-18.1555392270637,
16.5347458494382));
#212931=CARTESIAN_POINT('Ctrl Pts',(20.9866464512386,-20.9798900157063,
16.6619216561196));
#212932=CARTESIAN_POINT('Ctrl Pts',(18.24818021658,-21.9437775799877,16.789097462801));
#212933=CARTESIAN_POINT('Ctrl Pts',(15.9554234798327,-20.162894905289,16.9162732694825));
#212934=CARTESIAN_POINT('Ctrl Pts',(16.2118382424305,-17.2710913116015,
17.0434490761639));
#212935=CARTESIAN_POINT('Ctrl Pts',(18.7821798745847,-15.9214171105603,
17.1706248828453));
#212936=CARTESIAN_POINT('Ctrl Pts',(21.3083194621878,-17.3521146113923,
17.2978006895268));
#212937=CARTESIAN_POINT('Ctrl Pts',(21.4726807235191,-20.2506076561855,
17.4249764962082));
#212938=CARTESIAN_POINT('Ctrl Pts',(19.1244724027178,-21.9577087771101,
17.5521523028896));
#212939=CARTESIAN_POINT('Ctrl Pts',(16.4180298878732,-20.9072586503617,
17.6793281095711));
#212940=CARTESIAN_POINT('Ctrl Pts',(15.8363462055885,-18.0629800689462,
17.8065039162525));
#212941=CARTESIAN_POINT('Ctrl Pts',(17.9130800309984,-16.0343220954698,
17.9336797229339));
#212942=CARTESIAN_POINT('Ctrl Pts',(20.7429569759279,-16.6824525078913,
18.0608555296154));
#212943=CARTESIAN_POINT('Ctrl Pts',(21.7297405853753,-19.412751880308,18.1880313362968));
#212944=CARTESIAN_POINT('Ctrl Pts',(19.9681181443722,-21.7203400000494,
18.3152071429782));
#212945=CARTESIAN_POINT('Ctrl Pts',(17.0742689039165,-21.4881479922645,
18.4423829496597));
#212946=CARTESIAN_POINT('Ctrl Pts',(15.7031199295909,-18.9291976127498,
18.5695587563411));
#212947=CARTESIAN_POINT('Ctrl Pts',(17.1126153022265,-16.3911670081152,
18.6967345630226));
#212948=CARTESIAN_POINT('Ctrl Pts',(20.0096305005975,-16.2025417305957,
18.823910369704));
#212949=CARTESIAN_POINT('Ctrl Pts',(21.7363338892051,-18.5363737640858,
18.9510861763854));
#212950=CARTESIAN_POINT('Ctrl Pts',(20.7085822803688,-21.2515170733997,
19.0782619830668));
#212951=CARTESIAN_POINT('Ctrl Pts',(17.8692739856059,-21.8569961899794,
19.2054377897483));
#212952=CARTESIAN_POINT('Ctrl Pts',(15.8232981382665,-19.7973216105359,
19.3326135964297));
#212953=CARTESIAN_POINT('Ctrl Pts',(16.4477105902148,-16.9621169125157,
19.4597894031112));
#212954=CARTESIAN_POINT('Ctrl Pts',(19.1696516731346,-15.9525064556156,
19.5869652097926));
#212955=CARTESIAN_POINT('Ctrl Pts',(21.4919093843545,-17.6947451283222,
19.714141016474));
#212956=CARTESIAN_POINT('Ctrl Pts',(21.2839564128859,-20.5904371653283,
19.8413168231554));
#212957=CARTESIAN_POINT('Ctrl Pts',(18.7365766963153,-21.9829646927876,
19.9684926298369));
#212958=CARTESIAN_POINT('Ctrl Pts',(16.1868330293274,-20.5947704364421,
20.0956684365183));
#212959=CARTESIAN_POINT('Ctrl Pts',(15.9739569464928,-17.6994358831224,
20.2228442431997));
#212960=CARTESIAN_POINT('Ctrl Pts',(18.2932490893143,-15.9532519029135,
20.3500200498812));
#212961=CARTESIAN_POINT('Ctrl Pts',(21.0169027756026,-16.9582317548374,
20.4771958565626));
#212962=CARTESIAN_POINT('Ctrl Pts',(21.6461349757523,-19.7923729679124,
20.6043716632441));
#212963=CARTESIAN_POINT('Ctrl Pts',(19.6036638566053,-21.8555188556529,
20.7315474699255));
#212964=CARTESIAN_POINT('Ctrl Pts',(16.7633305629729,-21.2548765937423,
20.8587232766069));
#212965=CARTESIAN_POINT('Ctrl Pts',(15.7309633230734,-18.5414683575651,
20.9858990832884));
#212966=CARTESIAN_POINT('Ctrl Pts',(17.4536974658068,-16.2047352548569,
21.1130748899698));
#212967=CARTESIAN_POINT('Ctrl Pts',(20.3510265953171,-16.3883741373928,
21.2402506966512));
#212968=CARTESIAN_POINT('Ctrl Pts',(21.7648402074573,-18.9241211217718,
21.3674265033327));
#212969=CARTESIAN_POINT('Ctrl Pts',(20.3980344426769,-21.4851745132896,
21.4946023100141));
#212970=CARTESIAN_POINT('Ctrl Pts',(17.5046027271422,-21.7227192681557,
21.6217781166956));
#212971=CARTESIAN_POINT('Ctrl Pts',(15.7390234877918,-19.4172952643212,
21.748953923377));
#212972=CARTESIAN_POINT('Ctrl Pts',(16.7212336413073,-16.6869333681719,
21.8761297300584));
#212973=CARTESIAN_POINT('Ctrl Pts',(19.5498595326579,-16.0308555962028,
22.0033055367398));
#212974=CARTESIAN_POINT('Ctrl Pts',(21.6307164666946,-18.0626227175078,
22.1305000010223));
#212975=CARTESIAN_POINT('Ctrl Pts',(21.244679026905,-19.9500078602896,22.2153025297443));
#212976=CARTESIAN_POINT('Ctrl Pts',(20.6946893042483,-20.6030837310342,
22.2577131229058));
#212977=CARTESIAN_POINT('Ctrl Pts',(18.1101968702393,-21.2832302832024,
-0.084727418129243));
#212978=CARTESIAN_POINT('Ctrl Pts',(17.3340242768668,-21.0755378486675,
-0.0423354825687649));
#212979=CARTESIAN_POINT('Ctrl Pts',(16.0189819851084,-19.8273057761765,
0.0424483885521913));
#212980=CARTESIAN_POINT('Ctrl Pts',(16.5291381537116,-17.1376091768898,
0.169624195233626));
#212981=CARTESIAN_POINT('Ctrl Pts',(19.0658757862808,-16.118581759655,0.29680000191506));
#212982=CARTESIAN_POINT('Ctrl Pts',(21.2962359844956,-17.6960342466338,
0.423975808596494));
#212983=CARTESIAN_POINT('Ctrl Pts',(21.1768856466422,-20.4273012583374,
0.551151615277929));
#212984=CARTESIAN_POINT('Ctrl Pts',(18.8158303215486,-21.8042714183123,
0.678327421959364));
#212985=CARTESIAN_POINT('Ctrl Pts',(16.379964849342,-20.5648743004978,0.805503228640797));
#212986=CARTESIAN_POINT('Ctrl Pts',(16.103643479711,-17.8455499279943,0.932679035322232));
#212987=CARTESIAN_POINT('Ctrl Pts',(18.2405820727437,-16.1414364891873,
1.05985484200366));
#212988=CARTESIAN_POINT('Ctrl Pts',(20.8301640861484,-17.0157826813563,
1.1870306486851));
#212989=CARTESIAN_POINT('Ctrl Pts',(21.4966648031415,-19.6665181585552,
1.31420645536653));
#212990=CARTESIAN_POINT('Ctrl Pts',(19.6285820960571,-21.6617119688685,
1.44138226204797));
#212991=CARTESIAN_POINT('Ctrl Pts',(16.9397809967372,-21.1709213290295,
1.5685580687294));
#212992=CARTESIAN_POINT('Ctrl Pts',(15.897061795067,-18.6444038895142,1.69573387541083));
#212993=CARTESIAN_POINT('Ctrl Pts',(17.4570587048633,-16.400088970387,1.82290968209227));
#212994=CARTESIAN_POINT('Ctrl Pts',(20.188569276403,-16.4969928998977,1.9500854887737));
#212995=CARTESIAN_POINT('Ctrl Pts',(21.58560319155,-18.8462140560325,2.07726129545514));
#212996=CARTESIAN_POINT('Ctrl Pts',(20.3664679748478,-21.2924869452229,
2.20443710213657));
#212997=CARTESIAN_POINT('Ctrl Pts',(17.6496448143142,-21.5915084873017,
2.33161290881801));
#212998=CARTESIAN_POINT('Ctrl Pts',(15.9276501817169,-19.4689447365969,
2.45878871549944));
#212999=CARTESIAN_POINT('Ctrl Pts',(16.7803073527985,-16.8721163178553,
2.58596452218088));
#213000=CARTESIAN_POINT('Ctrl Pts',(19.4253562537738,-16.1834520632443,
2.71314032886231));
#213001=CARTESIAN_POINT('Ctrl Pts',(21.4361287096228,-18.034758716609,2.84031613554374));
#213002=CARTESIAN_POINT('Ctrl Pts',(20.9678657836256,-20.72757731112,2.96749194222518));
#213003=CARTESIAN_POINT('Ctrl Pts',(18.4501696524655,-21.7914139305229,
3.09466774890661));
#213004=CARTESIAN_POINT('Ctrl Pts',(16.1928702476498,-20.2502645009728,
3.22184355558806));
#213005=CARTESIAN_POINT('Ctrl Pts',(16.2668996708449,-17.5180379719942,
3.34901936226947));
#213006=CARTESIAN_POINT('Ctrl Pts',(18.6043405202492,-16.1013826015585,
3.47619516895092));
#213007=CARTESIAN_POINT('Ctrl Pts',(21.0607358948925,-17.2999917651471,
3.60337097563235));
#213008=CARTESIAN_POINT('Ctrl Pts',(21.3824954994144,-20.0142159489022,
3.73054678231378));
#213009=CARTESIAN_POINT('Ctrl Pts',(19.2744248674316,-21.7539229281569,
3.85772258899522));
#213010=CARTESIAN_POINT('Ctrl Pts',(16.6705479621107,-20.9230395277464,
3.98489839567665));
#213011=CARTESIAN_POINT('Ctrl Pts',(15.9597602292861,-18.2838496971548,
4.11207420235809));
#213012=CARTESIAN_POINT('Ctrl Pts',(17.7941652973467,-16.2576462993305,
4.23925000903952));
#213013=CARTESIAN_POINT('Ctrl Pts',(20.4908103723742,-16.7033451914242,
4.36642581572096));
#213014=CARTESIAN_POINT('Ctrl Pts',(21.5756909706959,-19.2120453031261,
4.49360162240239));
#213015=CARTESIAN_POINT('Ctrl Pts',(20.053496478638,-21.4821699894429,4.62077742908383));
#213016=CARTESIAN_POINT('Ctrl Pts',(17.320745864617,-21.4310207505056,4.74795323576526));
#213017=CARTESIAN_POINT('Ctrl Pts',(15.8845682033658,-19.1055238383603,
4.8751290424467));
#213018=CARTESIAN_POINT('Ctrl Pts',(17.0625673598435,-16.6391783332833,
5.00230484912813));
#213019=CARTESIAN_POINT('Ctrl Pts',(19.7740022228553,-16.294703157517,5.12948065580956));
#213020=CARTESIAN_POINT('Ctrl Pts',(21.5312995962151,-18.388132904286,5.256656462491));
#213021=CARTESIAN_POINT('Ctrl Pts',(20.7222482100412,-20.9988757138337,
5.38383226917243));
#213022=CARTESIAN_POINT('Ctrl Pts',(18.0891024957557,-21.7317370993736,
5.51100807585386));
#213023=CARTESIAN_POINT('Ctrl Pts',(16.0476102147611,-19.9143622261804,
5.6381838825353));
#213024=CARTESIAN_POINT('Ctrl Pts',(16.4707138255686,-17.2140797414027,
5.76535968921673));
#213025=CARTESIAN_POINT('Ctrl Pts',(18.9702420260344,-16.1082312263917,
5.89253549589816));
#213026=CARTESIAN_POINT('Ctrl Pts',(21.2530328304472,-17.6113640569702,
6.01971130257961));
#213027=CARTESIAN_POINT('Ctrl Pts',(21.2247673617351,-20.3444471560277,
6.14688710926103));
#213028=CARTESIAN_POINT('Ctrl Pts',(18.9113774330884,-21.8000464144471,
6.27406291594248));
#213029=CARTESIAN_POINT('Ctrl Pts',(16.4352547188683,-20.6427398573077,
6.4012387226239));
#213030=CARTESIAN_POINT('Ctrl Pts',(16.0680881238634,-17.934284420239,6.52841452930535));
#213031=CARTESIAN_POINT('Ctrl Pts',(18.1467302100618,-16.1595198610482,
6.65559033598677));
#213032=CARTESIAN_POINT('Ctrl Pts',(20.7641558784545,-16.9466825084813,
6.78276614266821));
#213033=CARTESIAN_POINT('Ctrl Pts',(21.5190395340498,-19.5735994903424,
6.90994194934964));
#213034=CARTESIAN_POINT('Ctrl Pts',(19.7188222762027,-21.6302375206298,
7.03711775603107));
#213035=CARTESIAN_POINT('Ctrl Pts',(17.0150917049037,-21.2297588559072,
7.16429356271251));
#213036=CARTESIAN_POINT('Ctrl Pts',(15.8883528068746,-18.7395778145483,
7.29146936939395));
#213037=CARTESIAN_POINT('Ctrl Pts',(17.3723185877541,-16.4442809439337,
7.41864517607538));
#213038=CARTESIAN_POINT('Ctrl Pts',(20.1055425488892,-16.4496606606615,
7.54582098275682));
#213039=CARTESIAN_POINT('Ctrl Pts',(21.5804613489495,-18.7507814085371,
7.67299678943824));
#213040=CARTESIAN_POINT('Ctrl Pts',(20.4439285326649,-21.2365077250456,
7.80017259611969));
#213041=CARTESIAN_POINT('Ctrl Pts',(17.7386424177941,-21.6263399963654,
7.92734840280111));
#213042=CARTESIAN_POINT('Ctrl Pts',(15.9465351057383,-19.5626313092801,
8.05452420948256));
#213043=CARTESIAN_POINT('Ctrl Pts',(16.7117538245844,-16.9387062959837,
8.18170001616398));
#213044=CARTESIAN_POINT('Ctrl Pts',(19.3322578946213,-16.1618532970222,
8.30887582284543));
#213045=CARTESIAN_POINT('Ctrl Pts',(21.4038974784157,-17.9447867220078,
8.43605162952684));
#213046=CARTESIAN_POINT('Ctrl Pts',(21.0260718382901,-20.6517758148449,
8.5632274362083));
#213047=CARTESIAN_POINT('Ctrl Pts',(18.5454125485558,-21.799326097547,8.69040324288972));
#213048=CARTESIAN_POINT('Ctrl Pts',(16.2377705404641,-20.3346314107382,
8.81757904957116));
#213049=CARTESIAN_POINT('Ctrl Pts',(16.2202641280231,-17.6014582203607,
8.94475485625259));
#213050=CARTESIAN_POINT('Ctrl Pts',(18.5089543580768,-16.1073232887258,
9.07193066293403));
#213051=CARTESIAN_POINT('Ctrl Pts',(21.0041099966872,-17.223002679136,9.19910646961547));
#213052=CARTESIAN_POINT('Ctrl Pts',(21.4165806122538,-19.9249297977624,
9.32628227629688));
#213053=CARTESIAN_POINT('Ctrl Pts',(19.3679500158079,-21.7342542137755,
9.45345808297834));
#213054=CARTESIAN_POINT('Ctrl Pts',(16.7377096272338,-20.9910330748214,
9.58063388965975));
#213055=CARTESIAN_POINT('Ctrl Pts',(15.9389417519183,-18.3771256463843,
9.70780969634122));
#213056=CARTESIAN_POINT('Ctrl Pts',(17.7044663383378,-16.2906297566631,
9.83498550302262));
#213057=CARTESIAN_POINT('Ctrl Pts',(20.4145241592668,-16.6457758819371,
9.96216130970408));
#213058=CARTESIAN_POINT('Ctrl Pts',(21.5828053691612,-19.1167394951217,
10.0893371163855));
#213059=CARTESIAN_POINT('Ctrl Pts',(20.1374844696525,-21.4365648464185,
10.2165129230669));
#213060=CARTESIAN_POINT('Ctrl Pts',(17.4045536793081,-21.4769561606121,
10.3436887297484));
#213061=CARTESIAN_POINT('Ctrl Pts',(15.8913073734538,-19.2008569138979,
10.4708645364298));
#213062=CARTESIAN_POINT('Ctrl Pts',(16.9860551150528,-16.6964468944843,
10.5980403431112));
#213063=CARTESIAN_POINT('Ctrl Pts',(19.6844337988958,-16.2613668539671,
10.7252161497927));
#213064=CARTESIAN_POINT('Ctrl Pts',(21.5108484628264,-18.294775725408,10.8523919564741));
#213065=CARTESIAN_POINT('Ctrl Pts',(20.7896770127668,-20.9311470768482,
10.9795677631555));
#213066=CARTESIAN_POINT('Ctrl Pts',(18.1825494931985,-21.7517738250013,
11.106743569837));
#213067=CARTESIAN_POINT('Ctrl Pts',(16.081343586742,-20.0037818622775,11.2339193765184));
#213068=CARTESIAN_POINT('Ctrl Pts',(16.4137852970245,-17.2908453218587,
11.3610951831999));
#213069=CARTESIAN_POINT('Ctrl Pts',(18.8748799885214,-16.1019150957474,
11.4882709898813));
#213070=CARTESIAN_POINT('Ctrl Pts',(21.206726034548,-17.5277608730685,11.6154467965627));
#213071=CARTESIAN_POINT('Ctrl Pts',(21.2699994185634,-20.2602576510996,
11.7426226032442));
#213072=CARTESIAN_POINT('Ctrl Pts',(19.0066507379223,-21.7925092338742,
11.8697984099256));
#213073=CARTESIAN_POINT('Ctrl Pts',(16.4931619278508,-20.7187698964554,
11.996974216607));
#213074=CARTESIAN_POINT('Ctrl Pts',(16.0355029668799,-18.0241288371456,
12.1241500232885));
#213075=CARTESIAN_POINT('Ctrl Pts',(18.0535475461816,-16.1807519795754,
12.2513258299699));
#213076=CARTESIAN_POINT('Ctrl Pts',(20.6958650182194,-16.8798231776942,
12.3785016366513));
#213077=CARTESIAN_POINT('Ctrl Pts',(21.5382931031166,-19.4799879964801,
12.5056774433328));
#213078=CARTESIAN_POINT('Ctrl Pts',(19.8079563199639,-21.5957565991263,
12.6328532500142));
#213079=CARTESIAN_POINT('Ctrl Pts',(17.092331270491,-21.2860426121147,12.7600290566956));
#213080=CARTESIAN_POINT('Ctrl Pts',(15.8828353868898,-18.8349893955103,
12.8872048633771));
#213081=CARTESIAN_POINT('Ctrl Pts',(17.2891060725835,-16.491286146028,13.0143806700585));
#213082=CARTESIAN_POINT('Ctrl Pts',(20.0209772564507,-16.4051351284387,
13.1415564767399));
#213083=CARTESIAN_POINT('Ctrl Pts',(21.5721266863414,-18.6555745542452,
13.2687322834214));
#213084=CARTESIAN_POINT('Ctrl Pts',(20.5194710355226,-21.1779659282937,
13.3959080901028));
#213085=CARTESIAN_POINT('Ctrl Pts',(17.8287565284422,-21.6581717221597,
13.5230838967842));
#213086=CARTESIAN_POINT('Ctrl Pts',(15.9685467207697,-19.6556329249039,
13.6502597034657));
#213087=CARTESIAN_POINT('Ctrl Pts',(16.6454686534027,-17.0075545914336,
13.7774355101471));
#213088=CARTESIAN_POINT('Ctrl Pts',(19.2384884676639,-16.14338423443,13.9046113168286));
#213089=CARTESIAN_POINT('Ctrl Pts',(21.3686714249291,-17.8559445199825,
14.03178712351));
#213090=CARTESIAN_POINT('Ctrl Pts',(21.0817068759728,-20.5740676795759,
14.1589629301914));
#213091=CARTESIAN_POINT('Ctrl Pts',(18.6408669834337,-21.8040444200327,
14.2861387368729));
#213092=CARTESIAN_POINT('Ctrl Pts',(16.2854708531072,-20.4174474229502,
14.4133145435543));
#213093=CARTESIAN_POINT('Ctrl Pts',(16.1764482421967,-17.6863933712359,
14.5404903502357));
#213094=CARTESIAN_POINT('Ctrl Pts',(18.413820629506,-16.1164548490061,14.6676661569172));
#213095=CARTESIAN_POINT('Ctrl Pts',(20.9449377166707,-17.1479530090328,
14.7948419635986));
#213096=CARTESIAN_POINT('Ctrl Pts',(21.4476566750608,-19.8345523114875,
14.92201777028));
#213097=CARTESIAN_POINT('Ctrl Pts',(19.4607640626112,-21.7114646455266,
15.0491935769614));
#213098=CARTESIAN_POINT('Ctrl Pts',(16.8071105307807,-21.0567394389867,
15.1763693836429));
#213099=CARTESIAN_POINT('Ctrl Pts',(15.9212584907105,-18.471046432039,15.3035451903243));
#213100=CARTESIAN_POINT('Ctrl Pts',(17.6159222069866,-16.3265984723504,
15.4307209970058));
#213101=CARTESIAN_POINT('Ctrl Pts',(20.3363529026182,-16.5907934634841,
15.5578968036872));
#213102=CARTESIAN_POINT('Ctrl Pts',(21.5867242633349,-19.0212488988654,
15.6850726103686));
#213103=CARTESIAN_POINT('Ctrl Pts',(20.2198981724784,-21.388172767609,15.8122484170501));
#213104=CARTESIAN_POINT('Ctrl Pts',(17.4898527336144,-21.5200593280063,
15.9394242237315));
#213105=CARTESIAN_POINT('Ctrl Pts',(15.9012351911711,-19.2959108466956,
16.0666000304129));
#213106=CARTESIAN_POINT('Ctrl Pts',(16.9115035396152,-16.7562455090563,
16.1937758370943));
#213107=CARTESIAN_POINT('Ctrl Pts',(19.5937992735749,-16.2310486329641,
16.3209516437758));
#213108=CARTESIAN_POINT('Ctrl Pts',(21.4872825391909,-18.2021557548393,
16.4481274504572));
#213109=CARTESIAN_POINT('Ctrl Pts',(20.8547999630863,-20.8611984310668,
16.5753032571387));
#213110=CARTESIAN_POINT('Ctrl Pts',(18.2766150525408,-21.7686700450093,
16.7024790638201));
#213111=CARTESIAN_POINT('Ctrl Pts',(16.1180524427778,-20.092021714915,16.8296548705015));
#213112=CARTESIAN_POINT('Ctrl Pts',(16.3594593527494,-17.3694742191139,
16.956830677183));
#213113=CARTESIAN_POINT('Ctrl Pts',(18.7793599259594,-16.0987959046484,
17.0840064838644));
#213114=CARTESIAN_POINT('Ctrl Pts',(21.1576455824562,-17.4457552578498,
17.2111822905458));
#213115=CARTESIAN_POINT('Ctrl Pts',(21.3123868454594,-20.1746006738818,
17.3383580972273));
#213116=CARTESIAN_POINT('Ctrl Pts',(19.1016182104896,-21.7817858547834,
17.4655339039087));
#213117=CARTESIAN_POINT('Ctrl Pts',(16.5535826843549,-20.7928181502387,
17.5927097105901));
#213118=CARTESIAN_POINT('Ctrl Pts',(16.0059447133635,-18.1150140469113,
17.7198855172716));
#213119=CARTESIAN_POINT('Ctrl Pts',(17.9611281456538,-16.2050926063331,
17.847061323953));
#213120=CARTESIAN_POINT('Ctrl Pts',(20.6253735344697,-16.8152882071486,
17.9742371306345));
#213121=CARTESIAN_POINT('Ctrl Pts',(21.55440109729,-19.3857842586047,18.1014129373159));
#213122=CARTESIAN_POINT('Ctrl Pts',(19.8958857071821,-21.5583101764979,
18.2285887439973));
#213123=CARTESIAN_POINT('Ctrl Pts',(17.171412295493,-21.3397082732704,18.3557645506787));
#213124=CARTESIAN_POINT('Ctrl Pts',(15.8805161175613,-18.9305322272779,
18.4829403573602));
#213125=CARTESIAN_POINT('Ctrl Pts',(17.2075142945774,-16.54105153018,18.6101161640416));
#213126=CARTESIAN_POINT('Ctrl Pts',(19.9349683619421,-16.3634664140689,
18.7372919707231));
#213127=CARTESIAN_POINT('Ctrl Pts',(21.5606084977061,-18.5607002000248,
18.8644677774045));
#213128=CARTESIAN_POINT('Ctrl Pts',(20.5930107759761,-21.1169272666383,
18.9916435840859));
#213129=CARTESIAN_POINT('Ctrl Pts',(17.9198860504282,-21.6869679347534,
19.1188193907673));
#213130=CARTESIAN_POINT('Ctrl Pts',(15.9936603441588,-19.7478452776443,
19.2459951974488));
#213131=CARTESIAN_POINT('Ctrl Pts',(16.5815261871606,-17.078583966977,19.3731710041302));
#213132=CARTESIAN_POINT('Ctrl Pts',(19.1441531564327,-16.1280656028778,
19.5003468108116));
#213133=CARTESIAN_POINT('Ctrl Pts',(21.3304900605322,-17.768331748829,19.6275226174931));
#213134=CARTESIAN_POINT('Ctrl Pts',(21.1347084926027,-20.4945400989296,
19.7546984241745));
#213135=CARTESIAN_POINT('Ctrl Pts',(18.7364258833193,-21.8055635519036,
19.881874230856));
#213136=CARTESIAN_POINT('Ctrl Pts',(16.335917684683,-20.4986197454331,20.0090500375374));
#213137=CARTESIAN_POINT('Ctrl Pts',(16.13550115311,-17.7727479556429,20.1362258442188));
#213138=CARTESIAN_POINT('Ctrl Pts',(18.3190460623333,-16.1287674194462,
20.2634016509003));
#213139=CARTESIAN_POINT('Ctrl Pts',(20.8832853969895,-17.0749262060105,
20.3905774575817));
#213140=CARTESIAN_POINT('Ctrl Pts',(21.4756888902747,-19.7431862770776,
20.5177532642631));
#213141=CARTESIAN_POINT('Ctrl Pts',(19.5527627818701,-21.6855770682093,
20.6449290709446));
#213142=CARTESIAN_POINT('Ctrl Pts',(16.8786730502231,-21.1200901556103,
20.772104877626));
#213143=CARTESIAN_POINT('Ctrl Pts',(15.9067298484541,-18.5654966090028,
20.8992806843074));
#213144=CARTESIAN_POINT('Ctrl Pts',(17.5286330567039,-16.3655315522399,
21.0264564909889));
#213145=CARTESIAN_POINT('Ctrl Pts',(20.256382680945,-16.5384221250544,21.1536322976703));
#213146=CARTESIAN_POINT('Ctrl Pts',(21.5874463526494,-18.9257528612692,
21.2808081043517));
#213147=CARTESIAN_POINT('Ctrl Pts',(20.3006391779602,-21.3369088308205,
21.4079839110332));
#213148=CARTESIAN_POINT('Ctrl Pts',(17.5765588536269,-21.5605501870015,
21.5351597177146));
#213149=CARTESIAN_POINT('Ctrl Pts',(15.9143182549829,-19.3900617201843,
21.6623355243961));
#213150=CARTESIAN_POINT('Ctrl Pts',(16.8390400444023,-16.8195068044844,
21.7895113310775));
#213151=CARTESIAN_POINT('Ctrl Pts',(19.5021076033005,-16.2018289998698,
21.9166871377589));
#213152=CARTESIAN_POINT('Ctrl Pts',(21.4611728203329,-18.1146776111084,
22.0438816020413));
#213153=CARTESIAN_POINT('Ctrl Pts',(21.0977299961801,-19.8915948627883,
22.1286841307634));
#213154=CARTESIAN_POINT('Ctrl Pts',(20.5799309501441,-20.506446466246,22.171094723925));
#213155=CARTESIAN_POINT('Ctrl Pts',(18.1489776385292,-21.138301703768,-0.171345817110153));
#213156=CARTESIAN_POINT('Ctrl Pts',(17.4210583610835,-20.9435211508747,
-0.128953881549675));
#213157=CARTESIAN_POINT('Ctrl Pts',(16.1877699881095,-19.77288952068,-0.0441700104287193));
#213158=CARTESIAN_POINT('Ctrl Pts',(16.6662106246443,-17.2504067355124,
0.0830057962527148));
#213159=CARTESIAN_POINT('Ctrl Pts',(19.0452436391262,-16.2947305011482,
0.210181602934149));
#213160=CARTESIAN_POINT('Ctrl Pts',(21.1369461776993,-17.7741154785761,
0.337357409615584));
#213161=CARTESIAN_POINT('Ctrl Pts',(21.0250156451928,-20.3355843150782,
0.464533216297019));
#213162=CARTESIAN_POINT('Ctrl Pts',(18.8107430711202,-21.6269506071525,
0.591709022978452));
#213163=CARTESIAN_POINT('Ctrl Pts',(16.5263111681857,-20.4646046776889,
0.718884829659889));
#213164=CARTESIAN_POINT('Ctrl Pts',(16.2671682231216,-17.9143360270367,
0.84606063634132));
#213165=CARTESIAN_POINT('Ctrl Pts',(18.2712570171198,-16.3161643914318,
0.973236443022757));
#213166=CARTESIAN_POINT('Ctrl Pts',(20.6998491681173,-17.1361539837924,
1.10041224970419));
#213167=CARTESIAN_POINT('Ctrl Pts',(21.3249146812175,-19.6220977928601,
1.22758805638563));
#213168=CARTESIAN_POINT('Ctrl Pts',(19.5729674648886,-21.4932538336279,
1.35476386306706));
#213169=CARTESIAN_POINT('Ctrl Pts',(17.0513245079943,-21.0329748042223,
1.4819396697485));
#213170=CARTESIAN_POINT('Ctrl Pts',(16.0734293667079,-18.6635266109603,
1.60911547642993));
#213171=CARTESIAN_POINT('Ctrl Pts',(17.5364439501815,-16.5587368924863,
1.73629128311137));
#213172=CARTESIAN_POINT('Ctrl Pts',(20.0981412048233,-16.6496164712725,
1.8634670897928));
#213173=CARTESIAN_POINT('Ctrl Pts',(21.4083239228994,-18.852790586328,1.99064289647423));
#213174=CARTESIAN_POINT('Ctrl Pts',(20.264980246985,-21.1469828950223,2.11781870315567));
#213175=CARTESIAN_POINT('Ctrl Pts',(17.717057312254,-21.4274147818336,2.2449945098371));
#213176=CARTESIAN_POINT('Ctrl Pts',(16.1021161259398,-19.4368071709258,
2.37217031651854));
#213177=CARTESIAN_POINT('Ctrl Pts',(16.9017650663717,-17.0014191111546,
2.49934612319997));
#213178=CARTESIAN_POINT('Ctrl Pts',(19.3823758238848,-16.3555679294722,
2.62652192988141));
#213179=CARTESIAN_POINT('Ctrl Pts',(21.2681420125742,-18.0917820305039,
2.75369773656284));
#213180=CARTESIAN_POINT('Ctrl Pts',(20.8289901877649,-20.6171927218193,
2.88087354324428));
#213181=CARTESIAN_POINT('Ctrl Pts',(18.467814897281,-21.6148924472776,3.0080493499257));
#213182=CARTESIAN_POINT('Ctrl Pts',(16.3508479162741,-20.1695536286012,
3.13522515660715));
#213183=CARTESIAN_POINT('Ctrl Pts',(16.4202750574822,-17.6071849263638,
3.26240096328857));
#213184=CARTESIAN_POINT('Ctrl Pts',(18.612401227227,-16.278600585146,3.38957676997001));
#213185=CARTESIAN_POINT('Ctrl Pts',(20.9160867238537,-17.4026942773856,
3.51675257665145));
#213186=CARTESIAN_POINT('Ctrl Pts',(21.2178430868515,-19.9481798092568,
3.64392838333288));
#213187=CARTESIAN_POINT('Ctrl Pts',(19.2408275823876,-21.5797321960836,
3.77110419001432));
#213188=CARTESIAN_POINT('Ctrl Pts',(16.7988292283319,-20.8005033884281,
3.89827999669575));
#213189=CARTESIAN_POINT('Ctrl Pts',(16.1322299470473,-18.3253874529646,
4.02545580337718));
#213190=CARTESIAN_POINT('Ctrl Pts',(17.8525932052803,-16.4251496374373,
4.15263161005862));
#213191=CARTESIAN_POINT('Ctrl Pts',(20.3815924913958,-16.8431401955444,
4.27980741674006));
#213192=CARTESIAN_POINT('Ctrl Pts',(21.3990279277772,-19.1958787336361,
4.40698322342148));
#213193=CARTESIAN_POINT('Ctrl Pts',(19.9714656507117,-21.3248736704392,
4.53415903010293));
#213194=CARTESIAN_POINT('Ctrl Pts',(17.4086054448983,-21.2769042917635,
4.66133483678435));
#213195=CARTESIAN_POINT('Ctrl Pts',(16.0617124801271,-19.0959795252294,
4.78851064346579));
#213196=CARTESIAN_POINT('Ctrl Pts',(17.1664774539701,-16.7829624806744,
4.91568645014722));
#213197=CARTESIAN_POINT('Ctrl Pts',(19.709347072374,-16.4599027344493,5.04286225682866));
#213198=CARTESIAN_POINT('Ctrl Pts',(21.3573962887413,-18.4231875523662,
5.1700380635101));
#213199=CARTESIAN_POINT('Ctrl Pts',(20.5986422365255,-20.8716249691852,
5.29721387019152));
#213200=CARTESIAN_POINT('Ctrl Pts',(18.1291946650469,-21.5589256221392,
5.42438967687296));
#213201=CARTESIAN_POINT('Ctrl Pts',(16.2146184499352,-19.8545338208328,
5.55156548355439));
#213202=CARTESIAN_POINT('Ctrl Pts',(16.6114184365535,-17.3221232564787,
5.67874129023583));
#213203=CARTESIAN_POINT('Ctrl Pts',(18.9555552653643,-16.2850234427458,
5.80591709691726));
#213204=CARTESIAN_POINT('Ctrl Pts',(21.096428889474,-17.69470908906,5.9330929035987));
#213205=CARTESIAN_POINT('Ctrl Pts',(21.0699206363647,-20.2578811098868,
6.06026871028013));
#213206=CARTESIAN_POINT('Ctrl Pts',(18.9003501829765,-21.6229882645151,
6.18744451696157));
#213207=CARTESIAN_POINT('Ctrl Pts',(16.5781637615641,-20.537629466679,6.31462032364299));
#213208=CARTESIAN_POINT('Ctrl Pts',(16.2338232826291,-17.9975540484287,
6.44179613032444));
#213209=CARTESIAN_POINT('Ctrl Pts',(18.1832397634138,-16.3331235511484,
6.56897193700587));
#213210=CARTESIAN_POINT('Ctrl Pts',(20.6379445772308,-17.0713496498852,
6.69614774368731));
#213211=CARTESIAN_POINT('Ctrl Pts',(21.3458984135663,-19.5349557185273,
6.82332355036874));
#213212=CARTESIAN_POINT('Ctrl Pts',(19.6575975681531,-21.4637360977331,
6.95049935705017));
#213213=CARTESIAN_POINT('Ctrl Pts',(17.1219532788895,-21.0881545031928,
7.07767516373161));
#213214=CARTESIAN_POINT('Ctrl Pts',(16.0652618013412,-18.7527837366743,
7.20485097041304));
#213215=CARTESIAN_POINT('Ctrl Pts',(17.4569719804889,-16.6001815270014,
7.33202677709449));
#213216=CARTESIAN_POINT('Ctrl Pts',(20.0202761062402,-16.6052267959878,
7.4592025837759));
#213217=CARTESIAN_POINT('Ctrl Pts',(21.4035017398149,-18.7632908224833,
7.58637839045736));
#213218=CARTESIAN_POINT('Ctrl Pts',(20.3376252150735,-21.094483806738,7.71355419713877));
#213219=CARTESIAN_POINT('Ctrl Pts',(17.8005220877082,-21.4600808758526,
7.84073000382022));
#213220=CARTESIAN_POINT('Ctrl Pts',(16.1198270066971,-19.5246694104279,
7.96790581050164));
#213221=CARTESIAN_POINT('Ctrl Pts',(16.8374733931665,-17.0638693048078,
8.09508161718309));
#213222=CARTESIAN_POINT('Ctrl Pts',(19.295065229689,-16.335311921419,8.22225742386451));
#213223=CARTESIAN_POINT('Ctrl Pts',(21.2379145416073,-18.0074034401497,
8.34943323054596));
#213224=CARTESIAN_POINT('Ctrl Pts',(20.8835776720644,-20.5461036742685,
8.47660903722738));
#213225=CARTESIAN_POINT('Ctrl Pts',(18.5571367062394,-21.6223127284784,
8.60378484390882));
#213226=CARTESIAN_POINT('Ctrl Pts',(16.3929568350657,-20.2486755926092,
8.73096065059025));
#213227=CARTESIAN_POINT('Ctrl Pts',(16.3765387661935,-17.6854190812848,
8.85813645727169));
#213228=CARTESIAN_POINT('Ctrl Pts',(18.5229450587927,-16.2841719500039,
8.98531226395313));
#213229=CARTESIAN_POINT('Ctrl Pts',(20.8629811604026,-17.3304914705113,
9.11248807063455));
#213230=CARTESIAN_POINT('Ctrl Pts',(21.2498091868164,-19.8644444246549,
9.23966387731599));
#213231=CARTESIAN_POINT('Ctrl Pts',(19.3285384330547,-21.5612862518657,
9.36683968399743));
#213232=CARTESIAN_POINT('Ctrl Pts',(16.861815568182,-20.864269893559,9.49401549067886));
#213233=CARTESIAN_POINT('Ctrl Pts',(16.1127057186315,-18.4128645967674,
9.6211912973603));
#213234=CARTESIAN_POINT('Ctrl Pts',(17.7684706763648,-16.4560825699245,
9.74836710404172));
#213235=CARTESIAN_POINT('Ctrl Pts',(20.310048861025,-16.7891498710692,9.87554291072316));
#213236=CARTESIAN_POINT('Ctrl Pts',(21.4057000363191,-19.1064979238893,
10.0027187174046));
#213237=CARTESIAN_POINT('Ctrl Pts',(20.0502322526962,-21.2821037207635,
10.129894524086));
#213238=CARTESIAN_POINT('Ctrl Pts',(17.4872030718116,-21.3199839763846,
10.2570703307675));
#213239=CARTESIAN_POINT('Ctrl Pts',(16.068032687595,-19.1853859073339,10.3842461374489));
#213240=CARTESIAN_POINT('Ctrl Pts',(17.0947218439171,-16.8366707538674,
10.5114219441303));
#213241=CARTESIAN_POINT('Ctrl Pts',(19.6253469633683,-16.4286388915877,
10.6385977508117));
#213242=CARTESIAN_POINT('Ctrl Pts',(21.3382165671608,-18.3356342288226,
10.7657735574932));
#213243=CARTESIAN_POINT('Ctrl Pts',(20.6618791064926,-20.8081069051386,
10.8929493641746));
#213244=CARTESIAN_POINT('Ctrl Pts',(18.2168322232895,-21.577716698977,11.0201251708561));
#213245=CARTESIAN_POINT('Ctrl Pts',(16.2462546761661,-19.9383943918618,
11.1473009775375));
#213246=CARTESIAN_POINT('Ctrl Pts',(16.5580290567716,-17.3941164527542,
11.2744767842189));
#213247=CARTESIAN_POINT('Ctrl Pts',(18.8661217218008,-16.2790999750865,
11.4016525909004));
#213248=CARTESIAN_POINT('Ctrl Pts',(21.0530009074768,-17.6163033713916,
11.5288283975818));
#213249=CARTESIAN_POINT('Ctrl Pts',(21.1123406939717,-20.1789255217625,
11.6560042042632));
#213250=CARTESIAN_POINT('Ctrl Pts',(18.989700510219,-21.6159196575024,11.7831800109447));
#213251=CARTESIAN_POINT('Ctrl Pts',(16.6324709789039,-20.6089328489849,
11.9103558176261));
#213252=CARTESIAN_POINT('Ctrl Pts',(16.203263888843,-18.0818129923747,12.0375316243075));
#213253=CARTESIAN_POINT('Ctrl Pts',(18.0958501055707,-16.3530357053638,
12.164707430989));
#213254=CARTESIAN_POINT('Ctrl Pts',(20.5738992423879,-17.0086468487652,
12.2918832376704));
#213255=CARTESIAN_POINT('Ctrl Pts',(21.3639550213402,-19.4471638903247,
12.4190590443519));
#213256=CARTESIAN_POINT('Ctrl Pts',(19.7411903016307,-21.4313987958485,
12.5462348510332));
#213257=CARTESIAN_POINT('Ctrl Pts',(17.1943909934554,-21.140939195026,12.6734106577147));
#213258=CARTESIAN_POINT('Ctrl Pts',(16.0600873898727,-18.8422637436558,
12.8005864643961));
#213259=CARTESIAN_POINT('Ctrl Pts',(17.3789326443482,-16.6442644964813,
12.9277622710776));
#213260=CARTESIAN_POINT('Ctrl Pts',(19.9409680926688,-16.563469339566,13.054938077759));
#213261=CARTESIAN_POINT('Ctrl Pts',(21.3956852288542,-18.6740028146668,
13.1821138844404));
#213262=CARTESIAN_POINT('Ctrl Pts',(20.4084713703825,-21.0395814528595,
13.3092896911219));
#213263=CARTESIAN_POINT('Ctrl Pts',(17.8850339589992,-21.4899336779714,
13.4364654978033));
#213264=CARTESIAN_POINT('Ctrl Pts',(16.1404701974589,-19.6118892754737,
13.5636413044848));
#213265=CARTESIAN_POINT('Ctrl Pts',(16.7753090571362,-17.1284374200765,
13.6908171111662));
#213266=CARTESIAN_POINT('Ctrl Pts',(19.2071252868205,-16.3179910487006,
13.8179929178476));
#213267=CARTESIAN_POINT('Ctrl Pts',(21.2048784313142,-17.9240844051089,
13.945168724529));
#213268=CARTESIAN_POINT('Ctrl Pts',(20.9357539750881,-20.4732265201925,
14.0723445312105));
#213269=CARTESIAN_POINT('Ctrl Pts',(18.6466569029825,-21.6267377209658,
14.1995203378919));
#213270=CARTESIAN_POINT('Ctrl Pts',(16.4376917012663,-20.3263430756987,
14.3266961445733));
#213271=CARTESIAN_POINT('Ctrl Pts',(16.3354468386715,-17.7650739598295,
14.4538719512548));
#213272=CARTESIAN_POINT('Ctrl Pts',(18.4337256305968,-16.2927358168784,
14.5810477579362));
#213273=CARTESIAN_POINT('Ctrl Pts',(20.8074875193202,-17.2601075093917,
14.7082235646177));
#213274=CARTESIAN_POINT('Ctrl Pts',(21.2789533042171,-19.7796855513471,
14.8353993712991));
#213275=CARTESIAN_POINT('Ctrl Pts',(19.4155823901109,-21.5399134719006,
14.9625751779805));
#213276=CARTESIAN_POINT('Ctrl Pts',(16.9269019368522,-20.9258914060103,
15.089750984662));
#213277=CARTESIAN_POINT('Ctrl Pts',(16.0961217953763,-18.5009464886232,
15.2169267913434));
#213278=CARTESIAN_POINT('Ctrl Pts',(17.6854311814566,-16.489815172386,15.3441025980248));
#213279=CARTESIAN_POINT('Ctrl Pts',(20.2367373770296,-16.7375856150594,
15.4712784047062));
#213280=CARTESIAN_POINT('Ctrl Pts',(21.4093752995786,-19.0169438138584,
15.5984542113877));
#213281=CARTESIAN_POINT('Ctrl Pts',(20.1275224372825,-21.2367200943101,
15.7256300180691));
#213282=CARTESIAN_POINT('Ctrl Pts',(17.5671992305365,-21.3604074939539,
15.8528058247506));
#213283=CARTESIAN_POINT('Ctrl Pts',(16.0773433099501,-19.2745305005226,
15.979981631432));
#213284=CARTESIAN_POINT('Ctrl Pts',(17.0248050117741,-16.8927517913624,
16.1071574381134));
#213285=CARTESIAN_POINT('Ctrl Pts',(19.5403470306901,-16.4002055022689,
16.2343332447949));
#213286=CARTESIAN_POINT('Ctrl Pts',(21.3161156964891,-18.2487722826149,
16.3615090514763));
#213287=CARTESIAN_POINT('Ctrl Pts',(20.7229534749337,-20.7425068464271,
16.4886848581577));
#213288=CARTESIAN_POINT('Ctrl Pts',(18.3050498885018,-21.5935625100306,
16.6158606648392));
#213289=CARTESIAN_POINT('Ctrl Pts',(16.2806814057228,-20.021148524541,16.7430364715206));
#213290=CARTESIAN_POINT('Ctrl Pts',(16.5070804630683,-17.4678571266262,
16.870212278202));
#213291=CARTESIAN_POINT('Ctrl Pts',(18.776539977334,-16.2761746987364,16.9973880848835));
#213292=CARTESIAN_POINT('Ctrl Pts',(21.0069717027245,-17.5393959043074,
17.1245638915649));
#213293=CARTESIAN_POINT('Ctrl Pts',(21.1520929673995,-20.0985936915781,
17.2517396982463));
#213294=CARTESIAN_POINT('Ctrl Pts',(19.0787640182614,-21.6058629324566,
17.3789155049278));
#213295=CARTESIAN_POINT('Ctrl Pts',(16.6891354808367,-20.6783776501158,
17.5060913116092));
#213296=CARTESIAN_POINT('Ctrl Pts',(16.1755432211384,-18.1670480248764,
17.6332671182907));
#213297=CARTESIAN_POINT('Ctrl Pts',(18.0091762603091,-16.3758631171963,
17.760442924972));
#213298=CARTESIAN_POINT('Ctrl Pts',(20.5077900930114,-16.9481239064058,
17.8876187316535));
#213299=CARTESIAN_POINT('Ctrl Pts',(21.3790616092047,-19.3588166369015,
18.0147945383349));
#213300=CARTESIAN_POINT('Ctrl Pts',(19.8236532699919,-21.3962803529462,
18.1419703450164));
#213301=CARTESIAN_POINT('Ctrl Pts',(17.2685556870694,-21.1912685542763,
18.2691461516978));
#213302=CARTESIAN_POINT('Ctrl Pts',(16.0579123055315,-18.931866841806,18.3963219583793));
#213303=CARTESIAN_POINT('Ctrl Pts',(17.3024132869284,-16.6909360522447,
18.5234977650607));
#213304=CARTESIAN_POINT('Ctrl Pts',(19.8603062232868,-16.5243910975421,
18.6506735717421));
#213305=CARTESIAN_POINT('Ctrl Pts',(21.3848831062071,-18.5850266359637,
18.7778493784235));
#213306=CARTESIAN_POINT('Ctrl Pts',(20.4774392715833,-20.9823374598767,
18.905025185105));
#213307=CARTESIAN_POINT('Ctrl Pts',(17.9704981152505,-21.5169396795275,
19.0322009917864));
#213308=CARTESIAN_POINT('Ctrl Pts',(16.164022550051,-19.6983689447528,19.1593767984678));
#213309=CARTESIAN_POINT('Ctrl Pts',(16.7153417841063,-17.1950510214384,
19.2865526051493));
#213310=CARTESIAN_POINT('Ctrl Pts',(19.1186546397307,-16.3036247501402,
19.4137284118307));
#213311=CARTESIAN_POINT('Ctrl Pts',(21.1690707367099,-17.8419183693358,
19.5409042185122));
#213312=CARTESIAN_POINT('Ctrl Pts',(20.9854605723195,-20.3986430325311,
19.6680800251936));
#213313=CARTESIAN_POINT('Ctrl Pts',(18.7362750703233,-21.6281624110196,
19.795255831875));
#213314=CARTESIAN_POINT('Ctrl Pts',(16.4850023400387,-20.4024690544242,
19.9224316385565));
#213315=CARTESIAN_POINT('Ctrl Pts',(16.2970453597273,-17.8460600281632,
20.0496074452379));
#213316=CARTESIAN_POINT('Ctrl Pts',(18.3448430353522,-16.3042829359788,
20.1767832519193));
#213317=CARTESIAN_POINT('Ctrl Pts',(20.7496680183763,-17.1916206571837,
20.3039590586007));
#213318=CARTESIAN_POINT('Ctrl Pts',(21.305242804797,-19.6939995862426,20.4311348652822));
#213319=CARTESIAN_POINT('Ctrl Pts',(19.5018617071349,-21.5156352807656,
20.5583106719636));
#213320=CARTESIAN_POINT('Ctrl Pts',(16.9940155374735,-20.9853037174782,
20.6854864786451));
#213321=CARTESIAN_POINT('Ctrl Pts',(16.082496373835,-18.5895248604405,20.8126622853265));
#213322=CARTESIAN_POINT('Ctrl Pts',(17.6035686476012,-16.5263278496229,
20.9398380920079));
#213323=CARTESIAN_POINT('Ctrl Pts',(20.1617387665729,-16.6884701127161,
21.0670138986894));
#213324=CARTESIAN_POINT('Ctrl Pts',(21.4100524978415,-18.9273846007665,
21.1941897053708));
#213325=CARTESIAN_POINT('Ctrl Pts',(20.2032439132434,-21.1886431483515,
21.3213655120522));
#213326=CARTESIAN_POINT('Ctrl Pts',(17.6485149801115,-21.3983811058473,
21.4485413187337));
#213327=CARTESIAN_POINT('Ctrl Pts',(16.0896130221739,-19.3628281760474,
21.5757171254151));
#213328=CARTESIAN_POINT('Ctrl Pts',(16.9568464474972,-16.9520802407969,
21.7028929320966));
#213329=CARTESIAN_POINT('Ctrl Pts',(19.4543556739431,-16.3728024035369,
21.8300687387779));
#213330=CARTESIAN_POINT('Ctrl Pts',(21.291629173971,-18.1667325047092,21.9572632030605));
#213331=CARTESIAN_POINT('Ctrl Pts',(20.9507809654552,-19.8331818652868,
22.0420657317825));
#213332=CARTESIAN_POINT('Ctrl Pts',(20.4651725960397,-20.4098092014579,
22.084476324944));
#213333=CARTESIAN_POINT('Ctrl Pts',(18.187758406819,-20.9933731243335,-0.257964216091064));
#213334=CARTESIAN_POINT('Ctrl Pts',(17.5080924453001,-20.811504453082,-0.215572280530586));
#213335=CARTESIAN_POINT('Ctrl Pts',(16.3565579911106,-19.7184732651834,
-0.13078840940963));
#213336=CARTESIAN_POINT('Ctrl Pts',(16.8032830955771,-17.3632042941351,
-0.00361260272819575));
#213337=CARTESIAN_POINT('Ctrl Pts',(19.0246114919716,-16.4708792426415,
0.123563203953239));
#213338=CARTESIAN_POINT('Ctrl Pts',(20.977656370903,-17.8521967105184,0.250739010634673));
#213339=CARTESIAN_POINT('Ctrl Pts',(20.8731456437434,-20.2438673718189,
0.377914817316107));
#213340=CARTESIAN_POINT('Ctrl Pts',(18.805655820692,-21.4496297959928,0.505090623997542));
#213341=CARTESIAN_POINT('Ctrl Pts',(16.6726574870295,-20.3643350548799,
0.632266430678976));
#213342=CARTESIAN_POINT('Ctrl Pts',(16.4306929665323,-17.9831221260791,
0.75944223736041));
#213343=CARTESIAN_POINT('Ctrl Pts',(18.3019319614957,-16.490892293676,0.886618044041845));
#213344=CARTESIAN_POINT('Ctrl Pts',(20.5695342500862,-17.2565252862285,
1.01379385072328));
#213345=CARTESIAN_POINT('Ctrl Pts',(21.1531645592934,-19.5776774271649,
1.14096965740471));
#213346=CARTESIAN_POINT('Ctrl Pts',(19.5173528337202,-21.3247956983873,
1.26814546408615));
#213347=CARTESIAN_POINT('Ctrl Pts',(17.1628680192514,-20.8950282794151,
1.39532127076758));
#213348=CARTESIAN_POINT('Ctrl Pts',(16.249796938349,-18.6826493324063,1.52249707744901));
#213349=CARTESIAN_POINT('Ctrl Pts',(17.6158291954999,-16.7173848145856,
1.64967288413045));
#213350=CARTESIAN_POINT('Ctrl Pts',(20.0077131332437,-16.8022400426472,
1.77684869081188));
#213351=CARTESIAN_POINT('Ctrl Pts',(21.2310446542488,-18.8593671166236,
1.90402449749332));
#213352=CARTESIAN_POINT('Ctrl Pts',(20.1634925191223,-21.0014788448218,
2.03120030417475));
#213353=CARTESIAN_POINT('Ctrl Pts',(17.7844698101939,-21.2633210763656,
2.15837611085619));
#213354=CARTESIAN_POINT('Ctrl Pts',(16.2765820701628,-19.4046696052545,
2.28555191753762));
#213355=CARTESIAN_POINT('Ctrl Pts',(17.0232227799449,-17.1307219044541,
2.41272772421906));
#213356=CARTESIAN_POINT('Ctrl Pts',(19.3393953939956,-16.5276837957002,
2.53990353090049));
#213357=CARTESIAN_POINT('Ctrl Pts',(21.1001553155256,-18.148805344399,2.66707933758192));
#213358=CARTESIAN_POINT('Ctrl Pts',(20.6901145919042,-20.5068081325184,
2.79425514426337));
#213359=CARTESIAN_POINT('Ctrl Pts',(18.4854601420967,-21.4383709640324,
2.92143095094479));
#213360=CARTESIAN_POINT('Ctrl Pts',(16.5088255848986,-20.0888427562296,
3.04860675762623));
#213361=CARTESIAN_POINT('Ctrl Pts',(16.5736504441196,-17.6963318807336,
3.17578256430766));
#213362=CARTESIAN_POINT('Ctrl Pts',(18.6204619342047,-16.4558185687336,
3.3029583709891));
#213363=CARTESIAN_POINT('Ctrl Pts',(20.7714375528147,-17.5053967896241,
3.43013417767053));
#213364=CARTESIAN_POINT('Ctrl Pts',(21.0531906742887,-19.8821436696115,
3.55730998435197));
#213365=CARTESIAN_POINT('Ctrl Pts',(19.2072302973436,-21.4055414640101,
3.6844857910334));
#213366=CARTESIAN_POINT('Ctrl Pts',(16.9271104945531,-20.6779672491097,
3.81166159771483));
#213367=CARTESIAN_POINT('Ctrl Pts',(16.3046996648085,-18.3669252087745,
3.93883740439627));
#213368=CARTESIAN_POINT('Ctrl Pts',(17.9110211132137,-16.5926529755442,
4.0660132110777));
#213369=CARTESIAN_POINT('Ctrl Pts',(20.2723746104174,-16.9829351996645,
4.19318901775914));
#213370=CARTESIAN_POINT('Ctrl Pts',(21.2223648848585,-19.179712164146,4.32036482444056));
#213371=CARTESIAN_POINT('Ctrl Pts',(19.8894348227856,-21.1675773514354,
4.44754063112201));
#213372=CARTESIAN_POINT('Ctrl Pts',(17.4964650251793,-21.1227878330214,
4.57471643780344));
#213373=CARTESIAN_POINT('Ctrl Pts',(16.2388567568882,-19.0864352120986,
4.70189224448488));
#213374=CARTESIAN_POINT('Ctrl Pts',(17.2703875480967,-16.9267466280655,
4.8290680511663));
#213375=CARTESIAN_POINT('Ctrl Pts',(19.6446919218926,-16.6251023113816,
4.95624385784775));
#213376=CARTESIAN_POINT('Ctrl Pts',(21.1834929812674,-18.4582422004466,
5.08341966452918));
#213377=CARTESIAN_POINT('Ctrl Pts',(20.4750362630098,-20.7443742245365,
5.21059547121061));
#213378=CARTESIAN_POINT('Ctrl Pts',(18.1692868343382,-21.386114144905,5.33777127789205));
#213379=CARTESIAN_POINT('Ctrl Pts',(16.3816266851093,-19.7947054154853,
5.46494708457348));
#213380=CARTESIAN_POINT('Ctrl Pts',(16.7521230475383,-17.4301667715549,
5.59212289125491));
#213381=CARTESIAN_POINT('Ctrl Pts',(18.9408685046945,-16.4618156591,5.71929869793635));
#213382=CARTESIAN_POINT('Ctrl Pts',(20.9398249485008,-17.7780541211498,
5.84647450461778));
#213383=CARTESIAN_POINT('Ctrl Pts',(20.9150739109944,-20.1713150637459,
5.97365031129922));
#213384=CARTESIAN_POINT('Ctrl Pts',(18.8893229328647,-21.4459301145832,
6.10082611798065));
#213385=CARTESIAN_POINT('Ctrl Pts',(16.7210728042601,-20.4325190760503,
6.22800192466209));
#213386=CARTESIAN_POINT('Ctrl Pts',(16.3995584413949,-18.0608236766186,
6.35517773134351));
#213387=CARTESIAN_POINT('Ctrl Pts',(18.2197493167659,-16.5067272412486,
6.48235353802496));
#213388=CARTESIAN_POINT('Ctrl Pts',(20.5117332760072,-17.1960167912891,
6.60952934470639));
#213389=CARTESIAN_POINT('Ctrl Pts',(21.1727572930827,-19.4963119467122,
6.73670515138783));
#213390=CARTESIAN_POINT('Ctrl Pts',(19.5963728601034,-21.2972346748364,
6.86388095806926));
#213391=CARTESIAN_POINT('Ctrl Pts',(17.2288148528754,-20.9465501504785,
6.99105676475069));
#213392=CARTESIAN_POINT('Ctrl Pts',(16.2421707958078,-18.7659896588004,
7.11823257143212));
#213393=CARTESIAN_POINT('Ctrl Pts',(17.5416253732237,-16.7560821100692,
7.24540837811357));
#213394=CARTESIAN_POINT('Ctrl Pts',(19.935009663591,-16.7607929313141,7.37258418479499));
#213395=CARTESIAN_POINT('Ctrl Pts',(21.2265421306802,-18.7758002364295,
7.49975999147643));
#213396=CARTESIAN_POINT('Ctrl Pts',(20.2313218974823,-20.9524598884302,
7.62693579815786));
#213397=CARTESIAN_POINT('Ctrl Pts',(17.8624017576224,-21.2938217553397,
7.7541116048393));
#213398=CARTESIAN_POINT('Ctrl Pts',(16.2931189076558,-19.4867075115756,
7.88128741152073));
#213399=CARTESIAN_POINT('Ctrl Pts',(16.9631929617487,-17.189032313632,8.00846321820217));
#213400=CARTESIAN_POINT('Ctrl Pts',(19.2578725647568,-16.5087705458158,
8.1356390248836));
#213401=CARTESIAN_POINT('Ctrl Pts',(21.0719316047989,-18.0700201582916,
8.26281483156504));
#213402=CARTESIAN_POINT('Ctrl Pts',(20.7410835058385,-20.440431533692,8.38999063824647));
#213403=CARTESIAN_POINT('Ctrl Pts',(18.5688608639229,-21.4452993594099,
8.5171664449279));
#213404=CARTESIAN_POINT('Ctrl Pts',(16.5481431296672,-20.1627197744802,
8.64434225160934));
#213405=CARTESIAN_POINT('Ctrl Pts',(16.5328134043638,-17.7693799422089,
8.77151805829078));
#213406=CARTESIAN_POINT('Ctrl Pts',(18.5369357595085,-16.461020611282,8.89869386497221));
#213407=CARTESIAN_POINT('Ctrl Pts',(20.7218523241179,-17.4379802618865,
9.02586967165363));
#213408=CARTESIAN_POINT('Ctrl Pts',(21.0830377613791,-19.8039590515472,
9.15304547833508));
#213409=CARTESIAN_POINT('Ctrl Pts',(19.2891268503013,-21.3883182899558,
9.28022128501651));
#213410=CARTESIAN_POINT('Ctrl Pts',(16.9859215091302,-20.7375067122967,
9.40739709169795));
#213411=CARTESIAN_POINT('Ctrl Pts',(16.2864696853447,-18.4486035471503,
9.53457289837939));
#213412=CARTESIAN_POINT('Ctrl Pts',(17.8324750143917,-16.621535383186,9.6617487050608));
#213413=CARTESIAN_POINT('Ctrl Pts',(20.2055735627831,-16.9325238602014,
9.78892451174226));
#213414=CARTESIAN_POINT('Ctrl Pts',(21.2285947034771,-19.0962563526568,
9.91610031842368));
#213415=CARTESIAN_POINT('Ctrl Pts',(19.9629800357399,-21.1276425951086,
10.0432761251051));
#213416=CARTESIAN_POINT('Ctrl Pts',(17.569852464315,-21.1630117921569,10.1704519317865));
#213417=CARTESIAN_POINT('Ctrl Pts',(16.2447580017361,-19.1699149007699,
10.297627738468));
#213418=CARTESIAN_POINT('Ctrl Pts',(17.2033885727816,-16.9768946132505,
10.4248035451494));
#213419=CARTESIAN_POINT('Ctrl Pts',(19.5662601278407,-16.5959109292081,
10.5519793518308));
#213420=CARTESIAN_POINT('Ctrl Pts',(21.1655846714952,-18.3764927322373,
10.6791551585123));
#213421=CARTESIAN_POINT('Ctrl Pts',(20.5340812002182,-20.6850667334291,
10.8063309651937));
#213422=CARTESIAN_POINT('Ctrl Pts',(18.2511149533807,-21.4036595729525,
10.9335067718751));
#213423=CARTESIAN_POINT('Ctrl Pts',(16.4111657655901,-19.8730069214463,
11.0606825785565));
#213424=CARTESIAN_POINT('Ctrl Pts',(16.7022728165186,-17.4973875836496,
11.187858385238));
#213425=CARTESIAN_POINT('Ctrl Pts',(18.8573634550803,-16.4562848544257,
11.3150341919194));
#213426=CARTESIAN_POINT('Ctrl Pts',(20.8992757804055,-17.7048458697147,
11.4422099986009));
#213427=CARTESIAN_POINT('Ctrl Pts',(20.9546819693801,-20.0975933924253,
11.5693858052823));
#213428=CARTESIAN_POINT('Ctrl Pts',(18.9727502825159,-21.4393300811306,
11.6965616119637));
#213429=CARTESIAN_POINT('Ctrl Pts',(16.7717800299571,-20.4990958015143,
11.8237374186452));
#213430=CARTESIAN_POINT('Ctrl Pts',(16.3710248108061,-18.1394971476037,
11.9509132253266));
#213431=CARTESIAN_POINT('Ctrl Pts',(18.1381526649597,-16.5253194311522,
12.078089032008));
#213432=CARTESIAN_POINT('Ctrl Pts',(20.4519334665563,-17.137470519836,12.2052648386895));
#213433=CARTESIAN_POINT('Ctrl Pts',(21.1896169395636,-19.4143397841694,
12.3324406453709));
#213434=CARTESIAN_POINT('Ctrl Pts',(19.6744242832976,-21.2670409925706,
12.4596164520523));
#213435=CARTESIAN_POINT('Ctrl Pts',(17.2964507164197,-20.9958357779372,
12.5867922587338));
#213436=CARTESIAN_POINT('Ctrl Pts',(16.2373393928556,-18.8495380918013,
12.7139680654152));
#213437=CARTESIAN_POINT('Ctrl Pts',(17.4687592161129,-16.7972428469345,
12.8411438720966));
#213438=CARTESIAN_POINT('Ctrl Pts',(19.8609589288869,-16.7218035506933,
12.9683196787781));
#213439=CARTESIAN_POINT('Ctrl Pts',(21.219243771367,-18.6924310750883,13.0954954854595));
#213440=CARTESIAN_POINT('Ctrl Pts',(20.2974717052425,-20.9011969774254,
13.222671292141));
#213441=CARTESIAN_POINT('Ctrl Pts',(17.9413113895561,-21.3216956337831,
13.3498470988224));
#213442=CARTESIAN_POINT('Ctrl Pts',(16.3123936741481,-19.5681456260435,
13.4770229055038));
#213443=CARTESIAN_POINT('Ctrl Pts',(16.9051494608696,-17.2493202487194,
13.6041987121852));
#213444=CARTESIAN_POINT('Ctrl Pts',(19.1757621059772,-16.4925978629714,
13.7313745188667));
#213445=CARTESIAN_POINT('Ctrl Pts',(21.0410854376991,-17.9922242902351,
13.8585503255481));
#213446=CARTESIAN_POINT('Ctrl Pts',(20.7898010742036,-20.3723853608092,
13.9857261322295));
#213447=CARTESIAN_POINT('Ctrl Pts',(18.6524468225313,-21.449431021899,14.112901938911));
#213448=CARTESIAN_POINT('Ctrl Pts',(16.5899125494253,-20.2352387284471,
14.2400777455924));
#213449=CARTESIAN_POINT('Ctrl Pts',(16.4944454351462,-17.8437545484231,
14.3672535522739));
#213450=CARTESIAN_POINT('Ctrl Pts',(18.4536306316875,-16.4690167847506,
14.4944293589553));
#213451=CARTESIAN_POINT('Ctrl Pts',(20.67003732197,-17.3722620097506,14.6216051656367));
#213452=CARTESIAN_POINT('Ctrl Pts',(21.1102499333731,-19.7248187912068,
14.7487809723181));
#213453=CARTESIAN_POINT('Ctrl Pts',(19.3704007176107,-21.3683622982746,
14.8759567789996));
#213454=CARTESIAN_POINT('Ctrl Pts',(17.0466933429237,-20.7950433730338,
15.003132585681));
#213455=CARTESIAN_POINT('Ctrl Pts',(16.2709851000421,-18.5308465452073,
15.1303083923625));
#213456=CARTESIAN_POINT('Ctrl Pts',(17.7549401559266,-16.6530318724217,
15.2574841990439));
#213457=CARTESIAN_POINT('Ctrl Pts',(20.137121851441,-16.8843777666347,15.3846600057253));
#213458=CARTESIAN_POINT('Ctrl Pts',(21.2320263358222,-19.0126387288515,
15.5118358124068));
#213459=CARTESIAN_POINT('Ctrl Pts',(20.0351467020866,-21.085267421011,15.6390116190882));
#213460=CARTESIAN_POINT('Ctrl Pts',(17.6445457274587,-21.2007556599016,
15.7661874257696));
#213461=CARTESIAN_POINT('Ctrl Pts',(16.2534514287292,-19.2531501543497,
15.893363232451));
#213462=CARTESIAN_POINT('Ctrl Pts',(17.1381064839328,-17.0292580736685,
16.0205390391325));
#213463=CARTESIAN_POINT('Ctrl Pts',(19.4868947878054,-16.5693623715735,
16.1477148458139));
#213464=CARTESIAN_POINT('Ctrl Pts',(21.1449488537871,-18.2953888103906,
16.2748906524954));
#213465=CARTESIAN_POINT('Ctrl Pts',(20.5911069867814,-20.6238152617876,
16.4020664591768));
#213466=CARTESIAN_POINT('Ctrl Pts',(18.3334847244627,-21.4184549750521,
16.5292422658582));
#213467=CARTESIAN_POINT('Ctrl Pts',(16.4433103686679,-19.950275334167,16.6564180725397));
#213468=CARTESIAN_POINT('Ctrl Pts',(16.6547015733873,-17.5662400341386,
16.7835938792211));
#213469=CARTESIAN_POINT('Ctrl Pts',(18.7737200287087,-16.4535534928245,
16.9107696859025));
#213470=CARTESIAN_POINT('Ctrl Pts',(20.8562978229928,-17.633036550765,17.037945492584));
#213471=CARTESIAN_POINT('Ctrl Pts',(20.9917990893397,-20.0225867092743,
17.1651212992654));
#213472=CARTESIAN_POINT('Ctrl Pts',(19.0559098260331,-21.4299400101298,
17.2922971059468));
#213473=CARTESIAN_POINT('Ctrl Pts',(16.8246882773183,-20.563937149993,17.4194729126283));
#213474=CARTESIAN_POINT('Ctrl Pts',(16.3451417289135,-18.2190820028416,
17.5466487193097));
#213475=CARTESIAN_POINT('Ctrl Pts',(18.0572243749644,-16.5466336280595,
17.6738245259911));
#213476=CARTESIAN_POINT('Ctrl Pts',(20.3902066515531,-17.0809596056631,
17.8010003326726));
#213477=CARTESIAN_POINT('Ctrl Pts',(21.2037221211194,-19.3318490151982,
17.928176139354));
#213478=CARTESIAN_POINT('Ctrl Pts',(19.7514208328018,-21.2342505293946,
18.0553519460354));
#213479=CARTESIAN_POINT('Ctrl Pts',(17.3656990786459,-21.0428288352822,
18.1825277527169));
#213480=CARTESIAN_POINT('Ctrl Pts',(16.2353084935018,-18.9332014563341,
18.3097035593983));
#213481=CARTESIAN_POINT('Ctrl Pts',(17.3973122792794,-16.8408205743096,
18.4368793660797));
#213482=CARTESIAN_POINT('Ctrl Pts',(19.7856440846313,-16.6853157810153,
18.5640551727612));
#213483=CARTESIAN_POINT('Ctrl Pts',(21.2091577147082,-18.6093530719028,
18.6912309794426));
#213484=CARTESIAN_POINT('Ctrl Pts',(20.3618677671906,-20.8477476531151,
18.8184067861241));
#213485=CARTESIAN_POINT('Ctrl Pts',(18.0211101800729,-21.3469114243016,
18.9455825928055));
#213486=CARTESIAN_POINT('Ctrl Pts',(16.3343847559432,-19.6488926118612,
19.072758399487));
#213487=CARTESIAN_POINT('Ctrl Pts',(16.849157381052,-17.3115180758999,19.1999342061683));
#213488=CARTESIAN_POINT('Ctrl Pts',(19.0931561230287,-16.4791838974025,
19.3271100128498));
#213489=CARTESIAN_POINT('Ctrl Pts',(21.0076514128875,-17.9155049898426,
19.4542858195312));
#213490=CARTESIAN_POINT('Ctrl Pts',(20.8362126520363,-20.3027459661324,
19.5814616262127));
#213491=CARTESIAN_POINT('Ctrl Pts',(18.7361242573274,-21.4507612701356,
19.7086374328941));
#213492=CARTESIAN_POINT('Ctrl Pts',(16.6340869953943,-20.3063183634152,
19.8358132395755));
#213493=CARTESIAN_POINT('Ctrl Pts',(16.4585895663445,-17.9193721006837,
19.9629890462569));
#213494=CARTESIAN_POINT('Ctrl Pts',(18.3706400083713,-16.4797984525115,
20.0901648529384));
#213495=CARTESIAN_POINT('Ctrl Pts',(20.6160506397633,-17.3083151083569,
20.2173406596198));
#213496=CARTESIAN_POINT('Ctrl Pts',(21.1347967193193,-19.6448128954076,
20.3445164663014));
#213497=CARTESIAN_POINT('Ctrl Pts',(19.4509606323996,-21.3456934933219,
20.4716922729828));
#213498=CARTESIAN_POINT('Ctrl Pts',(17.1093580247237,-20.8505172793461,
20.5988680796641));
#213499=CARTESIAN_POINT('Ctrl Pts',(16.2582628992159,-18.6135531118782,
20.7260438863456));
#213500=CARTESIAN_POINT('Ctrl Pts',(17.6785042384983,-16.6871241470058,
20.853219693027));
#213501=CARTESIAN_POINT('Ctrl Pts',(20.0670948522008,-16.8385181003778,
20.9803954997085));
#213502=CARTESIAN_POINT('Ctrl Pts',(21.2326586430337,-18.9290163402638,
21.1075713063899));
#213503=CARTESIAN_POINT('Ctrl Pts',(20.1058486485267,-21.0403774658824,
21.2347471130713));
#213504=CARTESIAN_POINT('Ctrl Pts',(17.7204711065961,-21.2362120246932,
21.3619229197527));
#213505=CARTESIAN_POINT('Ctrl Pts',(16.264907789365,-19.3355946319105,21.4890987264342));
#213506=CARTESIAN_POINT('Ctrl Pts',(17.0746528505921,-17.0846536771093,
21.6162745331156));
#213507=CARTESIAN_POINT('Ctrl Pts',(19.4066037445858,-16.543775807204,21.743450339797));
#213508=CARTESIAN_POINT('Ctrl Pts',(21.1220855276092,-18.2187873983098,
21.8706448040796));
#213509=CARTESIAN_POINT('Ctrl Pts',(20.8038319347303,-19.7747688677855,
21.9554473328015));
#213510=CARTESIAN_POINT('Ctrl Pts',(20.3504142419353,-20.3131719366696,
21.9978579259631));
#213511=CARTESIAN_POINT('Ctrl Pts',(18.0722627314315,-21.4249949024184,
-8.32884108903365E-16));
#213512=CARTESIAN_POINT('Ctrl Pts',(17.9903580532758,-21.3953391176122,
1.14284362820775E-14));
#213513=CARTESIAN_POINT('Ctrl Pts',(17.9103568112513,-21.3612556170403,
1.33837946700833E-14));
#213514=CARTESIAN_POINT('Ctrl Pts',(17.8324629519401,-21.3230651201994,
-1.18308141061618E-15));
#213515=CARTESIAN_POINT('Ctrl Pts',(17.7532833251911,-21.2842442258188,
-1.59904079594309E-14));
#213516=CARTESIAN_POINT('Ctrl Pts',(17.676280547661,-21.2411789324049,-3.34052718883277E-15));
#213517=CARTESIAN_POINT('Ctrl Pts',(17.6016979156783,-21.1941602566529,
3.01494940124769E-15));
#213518=CARTESIAN_POINT('Ctrl Pts',(17.5268866858167,-21.1469974673284,
9.38990570702805E-15));
#213519=CARTESIAN_POINT('Ctrl Pts',(17.454509827292,-21.0958562232334,-7.05390108614649E-15));
#213520=CARTESIAN_POINT('Ctrl Pts',(17.3848517335724,-21.0409959625991,
-1.83394965880268E-14));
#213521=CARTESIAN_POINT('Ctrl Pts',(17.3596729290501,-21.0211660231794,
-2.24188187153734E-14));
#213522=CARTESIAN_POINT('Ctrl Pts',(17.3348497590451,-21.0008499098405,
-1.906235806488E-14));
#213523=CARTESIAN_POINT('Ctrl Pts',(17.3103971449292,-20.9800590889455,
-1.05540576278429E-14));
#213524=CARTESIAN_POINT('Ctrl Pts',(17.2929747331899,-20.9652456935222,
-4.68390922674883E-15));
#213525=CARTESIAN_POINT('Ctrl Pts',(17.2757404518089,-20.9501913039064,
-5.50447044822256E-16));
#213526=CARTESIAN_POINT('Ctrl Pts',(17.2586999683651,-20.9348999714627,
-1.45786160921091E-14));
#213527=CARTESIAN_POINT('Ctrl Pts',(17.2462568322336,-20.9237340833671,
-2.48221292944806E-14));
#213528=CARTESIAN_POINT('Ctrl Pts',(17.2339149535825,-20.9124397717598,
-2.54522446515586E-14));
#213529=CARTESIAN_POINT('Ctrl Pts',(17.2216943473019,-20.9010355554554,
-1.92693083711504E-14));
#213530=CARTESIAN_POINT('Ctrl Pts',(17.1582585289398,-20.8418375273512,
1.29026392568497E-14));
#213531=CARTESIAN_POINT('Ctrl Pts',(17.0979854521548,-20.7795917637398,
-1.84358832270529E-14));
#213532=CARTESIAN_POINT('Ctrl Pts',(17.0411057216722,-20.7145765131158,
-1.86101134502792E-14));
#213533=CARTESIAN_POINT('Ctrl Pts',(16.984562346582,-20.6499457268686,-1.87833133719448E-14));
#213534=CARTESIAN_POINT('Ctrl Pts',(16.9313717910639,-20.5825772843491,
-1.74089365841943E-14));
#213535=CARTESIAN_POINT('Ctrl Pts',(16.8818041708662,-20.5127177725604,
2.4980018054066E-16));
#213536=CARTESIAN_POINT('Ctrl Pts',(16.8334274591682,-20.4445367009721,
1.74842692555363E-14));
#213537=CARTESIAN_POINT('Ctrl Pts',(16.7885013791215,-20.3739820606686,
2.0753501284633E-15));
#213538=CARTESIAN_POINT('Ctrl Pts',(16.7473244499658,-20.3012692713251,
1.06858966120171E-15));
#213539=CARTESIAN_POINT('Ctrl Pts',(16.7339895188643,-20.2777216184046,
7.42555599363664E-16));
#213540=CARTESIAN_POINT('Ctrl Pts',(16.721048178709,-20.2539475653071,-1.12813719766283E-15));
#213541=CARTESIAN_POINT('Ctrl Pts',(16.708511751901,-20.2299543047592,1.70696790036118E-15));
#213542=CARTESIAN_POINT('Ctrl Pts',(16.6986550608892,-20.2110897463642,
3.81121037099786E-15));
#213543=CARTESIAN_POINT('Ctrl Pts',(16.689048690518,-20.1920896772321,-1.29321329154552E-14));
#213544=CARTESIAN_POINT('Ctrl Pts',(16.6796984128078,-20.1729575913137,
3.7470027081099E-15));
#213545=CARTESIAN_POINT('Ctrl Pts',(16.673772461475,-20.1608321963725,1.4257350817072E-14));
#213546=CARTESIAN_POINT('Ctrl Pts',(16.6679532034413,-20.1486615485784,
-2.13375587759138E-14));
#213547=CARTESIAN_POINT('Ctrl Pts',(16.6622433073212,-20.1364502099952,
-2.15105711021124E-14));
#213548=CARTESIAN_POINT('Ctrl Pts',(16.6271177740505,-20.0613297926252,
-2.27890517030476E-14));
#213549=CARTESIAN_POINT('Ctrl Pts',(16.596105677901,-19.9846276360536,1.38706764190184E-14));
#213550=CARTESIAN_POINT('Ctrl Pts',(16.5694538163414,-19.9065723114556,
7.48012762841199E-15));
#213551=CARTESIAN_POINT('Ctrl Pts',(16.5428019547817,-19.8285169868576,
4.05397723666108E-16));
#213552=CARTESIAN_POINT('Ctrl Pts',(16.5205098557042,-19.7491077644459,
-1.49783758356987E-14));
#213553=CARTESIAN_POINT('Ctrl Pts',(16.502878625203,-19.66856395302,-1.87350135405495E-14));
#213554=CARTESIAN_POINT('Ctrl Pts',(16.4850541528343,-19.5871373650609,
-2.27945971057644E-14));
#213555=CARTESIAN_POINT('Ctrl Pts',(16.4719940148662,-19.5045499555443,
-7.13018664987758E-15));
#213556=CARTESIAN_POINT('Ctrl Pts',(16.4636225525689,-19.4211931726568,
-1.67643676718399E-14));
#213557=CARTESIAN_POINT('Ctrl Pts',(16.4601640820937,-19.3867563010228,
-2.07983225502737E-14));
#213558=CARTESIAN_POINT('Ctrl Pts',(16.4575064389052,-19.3521882740751,
1.67910904244036E-14));
#213559=CARTESIAN_POINT('Ctrl Pts',(16.4556467099008,-19.3175176204782,
1.35447209004269E-14));
#213560=CARTESIAN_POINT('Ctrl Pts',(16.4549147504963,-19.3038718092329,
1.22971584021043E-14));
#213561=CARTESIAN_POINT('Ctrl Pts',(16.4543064087743,-19.2902081093511,
-1.28578812753533E-14));
#213562=CARTESIAN_POINT('Ctrl Pts',(16.4538219778623,-19.2765459176976,
-1.26842980563424E-14));
#213563=CARTESIAN_POINT('Ctrl Pts',(16.4509249680159,-19.194842824923,-1.16389388342459E-14));
#213564=CARTESIAN_POINT('Ctrl Pts',(16.4524464982906,-19.1130624309727,
-8.75788806185453E-15));
#213565=CARTESIAN_POINT('Ctrl Pts',(16.458252360817,-19.0315664983848,5.71764857681956E-15));
#213566=CARTESIAN_POINT('Ctrl Pts',(16.4640582233434,-18.9500705657969,
2.01931852154936E-14));
#213567=CARTESIAN_POINT('Ctrl Pts',(16.474148825966,-18.868858075135,-1.49069399145082E-14));
#213568=CARTESIAN_POINT('Ctrl Pts',(16.4884408456005,-18.7883024616738,
-1.04083408558608E-14));
#213569=CARTESIAN_POINT('Ctrl Pts',(16.5025319927713,-18.7088790468066,
-6.09247964456401E-15));
#213570=CARTESIAN_POINT('Ctrl Pts',(16.5207077570521,-18.6300932899197,
1.349074868505E-14));
#213571=CARTESIAN_POINT('Ctrl Pts',(16.5429310587135,-18.5523284952265,
-1.60982338570648E-15));
#213572=CARTESIAN_POINT('Ctrl Pts',(16.5522282722733,-18.5197952598546,
-7.77797097015512E-15));
#213573=CARTESIAN_POINT('Ctrl Pts',(16.5622343667201,-18.4874410976137,
-4.30226113493849E-15));
#213574=CARTESIAN_POINT('Ctrl Pts',(16.572948601838,-18.4552959778321,-1.75415237890775E-14));
#213575=CARTESIAN_POINT('Ctrl Pts',(16.578489270918,-18.4386727220153,-2.43817434326259E-14));
#213576=CARTESIAN_POINT('Ctrl Pts',(16.5842201970324,-18.4221033375436,
1.47432613954525E-14));
#213577=CARTESIAN_POINT('Ctrl Pts',(16.5901333946024,-18.4056133356731,
1.04360964314765E-14));
#213578=CARTESIAN_POINT('Ctrl Pts',(16.6168665563098,-18.3310631652543,
-9.14610413127907E-15));
#213579=CARTESIAN_POINT('Ctrl Pts',(16.6473525954954,-18.2580371498547,
-2.56830120342859E-14));
#213580=CARTESIAN_POINT('Ctrl Pts',(16.6815326594994,-18.186894548015,-5.8564264548977E-15));
#213581=CARTESIAN_POINT('Ctrl Pts',(16.7078448582386,-18.1321281708012,
9.40630272034479E-15));
#213582=CARTESIAN_POINT('Ctrl Pts',(16.7363470804512,-18.0784782971011,
1.13991640136532E-14));
#213583=CARTESIAN_POINT('Ctrl Pts',(16.7670276804213,-18.0261235050124,
7.49400541621981E-15));
#213584=CARTESIAN_POINT('Ctrl Pts',(16.7762619506765,-18.01036571997,6.10196084666463E-15));
#213585=CARTESIAN_POINT('Ctrl Pts',(16.7856936431618,-17.9947253587034,
-4.23954215232061E-15));
#213586=CARTESIAN_POINT('Ctrl Pts',(16.795322651707,-17.9792075715296,-2.24820162486594E-15));
#213587=CARTESIAN_POINT('Ctrl Pts',(16.8035475707392,-17.9659525679159,
-3.76426044640903E-16));
#213588=CARTESIAN_POINT('Ctrl Pts',(16.8119141895608,-17.9527907636739,
-4.11143789873392E-15));
#213589=CARTESIAN_POINT('Ctrl Pts',(16.8204178980527,-17.9397316712593,
-3.41393580072236E-15));
#213590=CARTESIAN_POINT('Ctrl Pts',(16.8615694249279,-17.8765355265444,
7.90562951105821E-16));
#213591=CARTESIAN_POINT('Ctrl Pts',(16.9059580734959,-17.8156943310143,
1.33637921099262E-14));
#213592=CARTESIAN_POINT('Ctrl Pts',(16.9535504683774,-17.7575478141846,
1.74860126378462E-15));
#213593=CARTESIAN_POINT('Ctrl Pts',(16.9976826813803,-17.7036288115269,
-9.07571888140078E-15));
#213594=CARTESIAN_POINT('Ctrl Pts',(17.044570268779,-17.6520267822693,9.32681404607894E-15));
#213595=CARTESIAN_POINT('Ctrl Pts',(17.0942091882108,-17.6030457893103,
4.27435864480685E-15));
#213596=CARTESIAN_POINT('Ctrl Pts',(17.0997977486715,-17.5975313010074,
3.76786346256753E-15));
#213597=CARTESIAN_POINT('Ctrl Pts',(17.10542120347,-17.592050073031,7.85802203456014E-15));
#213598=CARTESIAN_POINT('Ctrl Pts',(17.1110791840834,-17.5866022544178,
1.97064586870965E-14));
#213599=CARTESIAN_POINT('Ctrl Pts',(-17.1175855514924,-17.590827960842,
0.00214194799035405));
#213600=CARTESIAN_POINT('Ctrl Pts',(-16.6641678381752,-18.1292310858663,
0.0445525400540117));
#213601=CARTESIAN_POINT('Ctrl Pts',(-16.345912932243,-19.6852113602882,
0.129355067678147));
#213602=CARTESIAN_POINT('Ctrl Pts',(-18.0613969831487,-21.3602251232166,
0.256549530862762));
#213603=CARTESIAN_POINT('Ctrl Pts',(-20.393346844718,-20.8193459211516,
0.383725337544195));
#213604=CARTESIAN_POINT('Ctrl Pts',(-21.203092563641,-18.5684056721843,
0.510901144225632));
#213605=CARTESIAN_POINT('Ctrl Pts',(-19.7475288416972,-16.6677876400165,
0.638076950907064));
#213606=CARTESIAN_POINT('Ctrl Pts',(-17.3621513300928,-16.8636225363617,
0.765252757588499));
#213607=CARTESIAN_POINT('Ctrl Pts',(-16.2353411818156,-18.9749835879209,
0.892428564269934));
#213608=CARTESIAN_POINT('Ctrl Pts',(-17.4009050866724,-21.0654820647258,
1.01960437095136));
#213609=CARTESIAN_POINT('Ctrl Pts',(-19.7894958141682,-21.2168759594155,
1.1467801776328));
#213610=CARTESIAN_POINT('Ctrl Pts',(-21.2097372485274,-19.2904469218172,
1.27395598431423));
#213611=CARTESIAN_POINT('Ctrl Pts',(-20.3586420669921,-17.0534826027649,
1.40113179099567));
#213612=CARTESIAN_POINT('Ctrl Pts',(-18.0170393273216,-16.558306372611,
1.5283075976771));
#213613=CARTESIAN_POINT('Ctrl Pts',(-16.3332031410643,-18.2591870619742,
1.65548340435853));
#213614=CARTESIAN_POINT('Ctrl Pts',(-16.8519492516291,-20.5956849881885,
1.78265921103997));
#213615=CARTESIAN_POINT('Ctrl Pts',(-19.097360012485,-21.424201689821,1.9098350177214));
#213616=CARTESIAN_POINT('Ctrl Pts',(-21.0094105654639,-19.9846279595186,
2.03701082440284));
#213617=CARTESIAN_POINT('Ctrl Pts',(-20.8339131261131,-17.5976815579533,
2.16418663108427));
#213618=CARTESIAN_POINT('Ctrl Pts',(-18.7318757425753,-16.4532385853486,
2.29136243776571));
#213619=CARTESIAN_POINT('Ctrl Pts',(-16.6317872262606,-17.6012539556073,
2.41853824444714));
#213620=CARTESIAN_POINT('Ctrl Pts',(-16.460348455506,-19.9884950701948,
2.54571405112858));
#213621=CARTESIAN_POINT('Ctrl Pts',(-18.3748438561772,-21.4248162457191,
2.67288985781001));
#213622=CARTESIAN_POINT('Ctrl Pts',(-20.6188427280565,-20.592482019073,
2.80006566449145));
#213623=CARTESIAN_POINT('Ctrl Pts',(-21.1336153829609,-18.2551073477921,
2.92724147117288));
#213624=CARTESIAN_POINT('Ctrl Pts',(-19.4468898611942,-16.5570884370688,
3.05441727785431));
#213625=CARTESIAN_POINT('Ctrl Pts',(-17.1061321385776,-17.056252237145,
3.18159308453575));
#213626=CARTESIAN_POINT('Ctrl Pts',(-16.2588421420139,-19.2946469479328,
3.30876889121718));
#213627=CARTESIAN_POINT('Ctrl Pts',(-17.6823558544925,-21.2186843501945,
3.43594469789862));
#213628=CARTESIAN_POINT('Ctrl Pts',(-20.0706877980967,-21.0631795478994,
3.56312050458005));
#213629=CARTESIAN_POINT('Ctrl Pts',(-21.2326916511383,-18.970798544754,
3.69029631126149));
#213630=CARTESIAN_POINT('Ctrl Pts',(-20.1023010005601,-16.8611710436873,
3.81747211794292));
#213631=CARTESIAN_POINT('Ctrl Pts',(-17.7165791083032,-16.6697493384941,
3.94464792462435));
#213632=CARTESIAN_POINT('Ctrl Pts',(-16.2642777359172,-18.5721509628136,
4.07182373130579));
#213633=CARTESIAN_POINT('Ctrl Pts',(-17.077793252575,-20.8230405026448,
4.19899953798722));
#213634=CARTESIAN_POINT('Ctrl Pts',(-19.4107756642115,-21.3573665111786,
4.32617534466866));
#213635=CARTESIAN_POINT('Ctrl Pts',(-21.1228584093689,-19.6849180395844,
4.45335115135009));
#213636=CARTESIAN_POINT('Ctrl Pts',(-20.6433118332049,-17.3400627566978,
4.58052695803153));
#213637=CARTESIAN_POINT('Ctrl Pts',(-18.4120901553326,-16.474059846431,
4.70770276471296));
#213638=CARTESIAN_POINT('Ctrl Pts',(-16.4762007799643,-17.8814132287533,
4.8348785713944));
#213639=CARTESIAN_POINT('Ctrl Pts',(-16.6117020541549,-20.2709635255851,
4.96205437807583));
#213640=CARTESIAN_POINT('Ctrl Pts',(-18.694279968992,-21.4504466518017,
5.08923018475726));
#213641=CARTESIAN_POINT('Ctrl Pts',(-20.8132985469758,-20.3377600460781,
5.2164059914387));
#213642=CARTESIAN_POINT('Ctrl Pts',(-21.0246897639318,-17.9537246080465,
5.34358179812013));
#213643=CARTESIAN_POINT('Ctrl Pts',(-19.1345152987216,-16.4855448821736,
5.47075760480157));
#213644=CARTESIAN_POINT('Ctrl Pts',(-16.8768929057173,-17.2801846414369,
5.597933411483));
#213645=CARTESIAN_POINT('Ctrl Pts',(-16.3230510066515,-19.6086112276183,
5.72510921816443));
#213646=CARTESIAN_POINT('Ctrl Pts',(-17.9811051686122,-21.3346377663488,
5.85228502484587));
#213647=CARTESIAN_POINT('Ctrl Pts',(-20.3298936084476,-20.8747420376322,
5.97946083152731));
#213648=CARTESIAN_POINT('Ctrl Pts',(-21.2145487148608,-18.6508498282177,
6.10663663820873));
#213649=CARTESIAN_POINT('Ctrl Pts',(-19.8234543356058,-16.7032442099259,
6.23381244489018));
#213650=CARTESIAN_POINT('Ctrl Pts',(-17.4328532225945,-16.8187324555017,
6.36098825157161));
#213651=CARTESIAN_POINT('Ctrl Pts',(-16.2359735195759,-18.8913612676384,
6.48816405825305));
#213652=CARTESIAN_POINT('Ctrl Pts',(-17.3308780673371,-21.0196223530527,
6.61533986493447));
#213653=CARTESIAN_POINT('Ctrl Pts',(-19.7130599007477,-21.2509682606574,
6.74251567161592));
#213654=CARTESIAN_POINT('Ctrl Pts',(-21.1970150425329,-19.3731534791717,
6.86969147829734));
#213655=CARTESIAN_POINT('Ctrl Pts',(-20.4213067547485,-17.1089565202789,
6.99686728497878));
#213656=CARTESIAN_POINT('Ctrl Pts',(-18.0975992455503,-16.5356375618508,
7.12404309166021));
#213657=CARTESIAN_POINT('Ctrl Pts',(-16.3577499290741,-18.1791811640576,
7.25121889834165));
#213658=CARTESIAN_POINT('Ctrl Pts',(-16.7979625659597,-20.5317380816948,
7.37839470502308));
#213659=CARTESIAN_POINT('Ctrl Pts',(-19.014369384542,-21.4349833589804,
7.50557051170451));
#213660=CARTESIAN_POINT('Ctrl Pts',(-20.9735546944935,-20.0602455157292,
7.63274631838594));
#213661=CARTESIAN_POINT('Ctrl Pts',(-20.8780875746881,-17.6687611972708,
7.75992212506739));
#213662=CARTESIAN_POINT('Ctrl Pts',(-18.8155531821895,-16.4545688335337,
7.88709793174882));
#213663=CARTESIAN_POINT('Ctrl Pts',(-16.6781988067934,-17.5316145569697,
8.01427373843027));
#213664=CARTESIAN_POINT('Ctrl Pts',(-16.4269144287518,-19.9117757653229,
8.14144954511167));
#213665=CARTESIAN_POINT('Ctrl Pts',(-18.2922378684508,-21.4114022793946,
8.26862535179315));
#213666=CARTESIAN_POINT('Ctrl Pts',(-20.5628506449959,-20.6546798498427,
8.39580115847454));
#213667=CARTESIAN_POINT('Ctrl Pts',(-21.15560646603,-18.3358543382901,8.52297696515602));
#213668=CARTESIAN_POINT('Ctrl Pts',(-19.5266886563297,-16.5823042290437,
8.65015277183742));
#213669=CARTESIAN_POINT('Ctrl Pts',(-17.1705282042537,-17.0028029097426,
8.77732857851889));
#213670=CARTESIAN_POINT('Ctrl Pts',(-16.2487560847711,-19.2115689399372,
8.90450438520028));
#213671=CARTESIAN_POINT('Ctrl Pts',(-17.6070410058773,-21.1821965784047,
9.03168019188174));
#213672=CARTESIAN_POINT('Ctrl Pts',(-19.9992408571273,-21.1067572777967,
9.15885599856315));
#213673=CARTESIAN_POINT('Ctrl Pts',(-21.2306607516671,-19.0544619141298,
9.28603180524462));
#213674=CARTESIAN_POINT('Ctrl Pts',(-20.1715493667948,-16.9081641037524,
9.41320761192604));
#213675=CARTESIAN_POINT('Ctrl Pts',(-17.7935756622645,-16.6369588734199,
9.54038341860746));
#213676=CARTESIAN_POINT('Ctrl Pts',(-16.2783829182894,-18.4896601890674,
9.66755922528891));
#213677=CARTESIAN_POINT('Ctrl Pts',(-17.0160664339986,-20.7665295852005,
9.79473503197033));
#213678=CARTESIAN_POINT('Ctrl Pts',(-19.3298473695317,-21.3786807093197,
9.92191083865178));
#213679=CARTESIAN_POINT('Ctrl Pts',(-21.0969753259781,-19.7645028994292,
10.0490866453332));
#213680=CARTESIAN_POINT('Ctrl Pts',(-20.6962200836287,-17.4049041089298,
10.1762624520146));
#213681=CARTESIAN_POINT('Ctrl Pts',(-18.4952497036636,-16.4646697748868,
10.3034382586961));
#213682=CARTESIAN_POINT('Ctrl Pts',(-16.5133179020725,-17.8064065412604,
10.4306140653775));
#213683=CARTESIAN_POINT('Ctrl Pts',(-16.5687240942544,-20.1991542024786,
10.5577898720589));
#213684=CARTESIAN_POINT('Ctrl Pts',(-18.6106365377785,-21.4477152900423,
10.6849656787404));
#213685=CARTESIAN_POINT('Ctrl Pts',(-20.7657273010908,-20.4066125005527,
10.8121414854218));
#213686=CARTESIAN_POINT('Ctrl Pts',(-21.0568343688704,-18.0309930252399,
10.9393172921033));
#213687=CARTESIAN_POINT('Ctrl Pts',(-19.2168850745718,-16.5003402851297,
11.0664930987847));
#213688=CARTESIAN_POINT('Ctrl Pts',(-16.9339186955814,-17.2189331662498,
11.1936689054661));
#213689=CARTESIAN_POINT('Ctrl Pts',(-16.302415187749,-19.5275073010768,
11.3208447121476));
#213690=CARTESIAN_POINT('Ctrl Pts',(-17.9017398239826,-21.3080892071774,
11.448020518829));
#213691=CARTESIAN_POINT('Ctrl Pts',(-20.26461151582,-20.9271055010812,11.5751963255104));
#213692=CARTESIAN_POINT('Ctrl Pts',(-21.2232421423571,-18.7340850866159,
11.7023721321919));
#213693=CARTESIAN_POINT('Ctrl Pts',(-19.8981476030732,-16.7409880798555,
11.8295479388733));
#213694=CARTESIAN_POINT('Ctrl Pts',(-17.5050198931187,-16.7763572789512,
11.9567237455547));
#213695=CARTESIAN_POINT('Ctrl Pts',(-16.2394051521196,-18.8077436389928,
12.0838995522362));
#213696=CARTESIAN_POINT('Ctrl Pts',(-17.2624263520327,-20.9714762566988,
12.2110753589176));
#213697=CARTESIAN_POINT('Ctrl Pts',(-19.6355250377943,-21.2824647517163,
12.3382511655991));
#213698=CARTESIAN_POINT('Ctrl Pts',(-21.181530456334,-19.4553964819894,
12.4654269722804));
#213699=CARTESIAN_POINT('Ctrl Pts',(-20.4820785920598,-17.1664931843466,
12.5926027789619));
#213700=CARTESIAN_POINT('Ctrl Pts',(-18.1788731175643,-16.5156815690145,
12.7197785856433));
#213701=CARTESIAN_POINT('Ctrl Pts',(-16.3849621026435,-18.1000408991359,
12.8469543923248));
#213702=CARTESIAN_POINT('Ctrl Pts',(-16.7461475608124,-20.4660198257546,
12.9741301990062));
#213703=CARTESIAN_POINT('Ctrl Pts',(-18.9310642518988,-21.4429795329118,
13.1013060056876));
#213704=CARTESIAN_POINT('Ctrl Pts',(-20.9351867230549,-20.1346201262487,
13.2284818123691));
#213705=CARTESIAN_POINT('Ctrl Pts',(-20.9198569968642,-17.7412801554356,
13.3556576190505));
#213706=CARTESIAN_POINT('Ctrl Pts',(-18.8991391456364,-16.4587004962619,
13.4828334257319));
#213707=CARTESIAN_POINT('Ctrl Pts',(-16.7269163779785,-17.463568380148,
13.6100092324134));
#213708=CARTESIAN_POINT('Ctrl Pts',(-16.3960682598664,-19.8339798927631,
13.7371850390948));
#213709=CARTESIAN_POINT('Ctrl Pts',(-18.210127404918,-21.395229595614,13.8643608457763));
#213710=CARTESIAN_POINT('Ctrl Pts',(-20.5048071407569,-20.71496778842,13.9915366524577));
#213711=CARTESIAN_POINT('Ctrl Pts',(-21.174881233638,-18.417292457472,14.1187124591391));
#213712=CARTESIAN_POINT('Ctrl Pts',(-19.6055982928313,-16.6101781091006,
14.2458882658205));
#213713=CARTESIAN_POINT('Ctrl Pts',(-17.236678015843,-16.9515399957704,
14.373064072502));
#213714=CARTESIAN_POINT('Ctrl Pts',(-16.2414577250354,-19.12819977377,14.5002398791834));
#213715=CARTESIAN_POINT('Ctrl Pts',(-17.5329902668867,-21.1432071955271,
14.6274156858649));
#213716=CARTESIAN_POINT('Ctrl Pts',(-19.9263746957985,-21.1479180170447,
14.7545914925463));
#213717=CARTESIAN_POINT('Ctrl Pts',(-21.2258293484353,-19.1380103519671,
14.8817672992277));
#213718=CARTESIAN_POINT('Ctrl Pts',(-20.2391852342543,-16.9574497340641,
15.0089431059091));
#213719=CARTESIAN_POINT('Ctrl Pts',(-17.8716270899769,-16.6067651894063,
15.1361189125906));
#213720=CARTESIAN_POINT('Ctrl Pts',(-16.2952425657462,-18.4076880217795,
15.263294719272));
#213721=CARTESIAN_POINT('Ctrl Pts',(-16.9562666210861,-20.7079833103585,
15.3904705259535));
#213722=CARTESIAN_POINT('Ctrl Pts',(-19.2482507130021,-21.3972729002994,
15.5176463326349));
#213723=CARTESIAN_POINT('Ctrl Pts',(-21.0684416937376,-19.8431763749684,
15.6448221393163));
#213724=CARTESIAN_POINT('Ctrl Pts',(-20.746927312261,-17.4714808382477,
15.7719979459977));
#213725=CARTESIAN_POINT('Ctrl Pts',(-18.5786770581442,-16.4580697410522,
15.8991737526792));
#213726=CARTESIAN_POINT('Ctrl Pts',(-16.552925962751,-17.7326848656722,
16.0263495593606));
#213727=CARTESIAN_POINT('Ctrl Pts',(-16.5281749238118,-20.1259459468057,
16.1535253660421));
#213728=CARTESIAN_POINT('Ctrl Pts',(-18.5271314833305,-21.4421844850479,
16.2807011727235));
#213729=CARTESIAN_POINT('Ctrl Pts',(-20.7158770671853,-20.4738333165386,
16.4078769794049));
#213730=CARTESIAN_POINT('Ctrl Pts',(-21.0863734510612,-18.1092945357334,
16.5350527860864));
#213731=CARTESIAN_POINT('Ctrl Pts',(-19.298713198351,-16.5178857141929,
16.6622285927678));
#213732=CARTESIAN_POINT('Ctrl Pts',(-16.9929636362077,-17.1596256717093,
16.7894043994492));
#213733=CARTESIAN_POINT('Ctrl Pts',(-16.2845068769401,-19.4457578281354,
16.9165802061307));
#213734=CARTESIAN_POINT('Ctrl Pts',(-17.8233080253906,-21.2788978233141,
17.0437560128121));
#213735=CARTESIAN_POINT('Ctrl Pts',(-20.1976125366265,-20.9772534891692,
17.1709318194935));
#213736=CARTESIAN_POINT('Ctrl Pts',(-21.2291433875466,-18.8175647801194,
17.298107626175));
#213737=CARTESIAN_POINT('Ctrl Pts',(-19.9715350464571,-16.7812120413194,
17.4252834328564));
#213738=CARTESIAN_POINT('Ctrl Pts',(-17.5785651103304,-16.7364225203127,
17.5524592395378));
#213739=CARTESIAN_POINT('Ctrl Pts',(-16.2456349710989,-18.7242878226724,
17.6796350462193));
#213740=CARTESIAN_POINT('Ctrl Pts',(-17.1956253005315,-20.9210649143176,
17.8068108529007));
#213741=CARTESIAN_POINT('Ctrl Pts',(-19.5569789344254,-21.31134716103,17.9339866595822));
#213742=CARTESIAN_POINT('Ctrl Pts',(-21.163300475815,-19.5370748250935,
18.0611624662636));
#213743=CARTESIAN_POINT('Ctrl Pts',(-20.5408896100412,-17.2260326509801,
18.188338272945));
#213744=CARTESIAN_POINT('Ctrl Pts',(-18.2607696752627,-16.4984583939631,
18.3155140796264));
#213745=CARTESIAN_POINT('Ctrl Pts',(-16.4148091914615,-18.0218562765459,
18.4426898863079));
#213746=CARTESIAN_POINT('Ctrl Pts',(-16.6965623292452,-20.3986032941145,
18.5698656929893));
#213747=CARTESIAN_POINT('Ctrl Pts',(-18.8475380723677,-21.4481815757617,
18.6970414996708));
#213748=CARTESIAN_POINT('Ctrl Pts',(-20.894349680935,-20.2076681919521,
18.8242173063522));
#213749=CARTESIAN_POINT('Ctrl Pts',(-20.9591745439093,-17.8151571779635,
18.9513931130336));
#213750=CARTESIAN_POINT('Ctrl Pts',(-18.9825398722896,-16.4656288920389,
19.078568919715));
#213751=CARTESIAN_POINT('Ctrl Pts',(-16.7778852948647,-17.3971917774822,
19.2057447263965));
#213752=CARTESIAN_POINT('Ctrl Pts',(-16.3678445475033,-19.7551947020895,
19.3329205330779));
#213753=CARTESIAN_POINT('Ctrl Pts',(-18.1286045709649,-21.3763163446451,
19.4600963397593));
#213754=CARTESIAN_POINT('Ctrl Pts',(-20.4447773190769,-20.773278200954,
19.5872721464408));
#213755=CARTESIAN_POINT('Ctrl Pts',(-21.1914180721045,-18.4993303685776,
19.7144479531222));
#213756=CARTESIAN_POINT('Ctrl Pts',(-19.6835302447416,-16.6406787897749,
19.8416237598037));
#213757=CARTESIAN_POINT('Ctrl Pts',(-17.304507398182,-16.9025210366613,
19.9687995664851));
#213758=CARTESIAN_POINT('Ctrl Pts',(-16.2369552011117,-19.0446328885181,
20.0959753731665));
#213759=CARTESIAN_POINT('Ctrl Pts',(-17.4602867931939,-21.1017600821981,
20.223151179848));
#213760=CARTESIAN_POINT('Ctrl Pts',(-19.8521708689288,-21.1866153140319,
20.3503269865294));
#213761=CARTESIAN_POINT('Ctrl Pts',(-21.2182032059767,-19.221350684525,
20.4775027932109));
#213762=CARTESIAN_POINT('Ctrl Pts',(-20.3051320707828,-17.0089716056813,
20.6046785998922));
#213763=CARTESIAN_POINT('Ctrl Pts',(-17.9506471225061,-16.5792041686457,
20.7318544065737));
#213764=CARTESIAN_POINT('Ctrl Pts',(-16.3148352980017,-18.3263225287329,
20.8590302132551));
#213765=CARTESIAN_POINT('Ctrl Pts',(-16.8984656481068,-20.647474826016,
20.9862060199366));
#213766=CARTESIAN_POINT('Ctrl Pts',(-19.1660680562885,-21.4131078237249,
21.113381826618));
#213767=CARTESIAN_POINT('Ctrl Pts',(-21.0373071781416,-19.9208779742462,
21.2405576332995));
#213768=CARTESIAN_POINT('Ctrl Pts',(-20.7953426154092,-17.5396647859301,
21.3677334399809));
#213769=CARTESIAN_POINT('Ctrl Pts',(-18.6623441981192,-16.4543701936005,
21.4949092466623));
#213770=CARTESIAN_POINT('Ctrl Pts',(-16.5948542065943,-17.6601323237235,
21.6220850533437));
#213771=CARTESIAN_POINT('Ctrl Pts',(-16.4903435139124,-20.0518037409453,
21.7492608600252));
#213772=CARTESIAN_POINT('Ctrl Pts',(-18.4433885276789,-21.4331202535291,
21.8764366667066));
#213773=CARTESIAN_POINT('Ctrl Pts',(-20.6647168408145,-20.5407968853708,
22.0036124733881));
#213774=CARTESIAN_POINT('Ctrl Pts',(-21.1114425640841,-18.1855248151863,
22.1307882800695));
#213775=CARTESIAN_POINT('Ctrl Pts',(-19.9599076846608,-17.0924953497883,
22.2155721511904));
#213776=CARTESIAN_POINT('Ctrl Pts',(-19.2802416510892,-16.9106266592565,
22.2579640867509));
#213777=CARTESIAN_POINT('Ctrl Pts',(-17.0028272034401,-17.4941907062238,
-0.0844764445356067));
#213778=CARTESIAN_POINT('Ctrl Pts',(-16.5172188178569,-18.0708180956198,
-0.042065852471949));
#213779=CARTESIAN_POINT('Ctrl Pts',(-16.1763692071458,-19.7372661563571,
0.042736675152187));
#213780=CARTESIAN_POINT('Ctrl Pts',(-18.0136451140781,-21.531198562073,
0.169931138336801));
#213781=CARTESIAN_POINT('Ctrl Pts',(-20.5111532049132,-20.9519193050085,
0.297106945018235));
#213782=CARTESIAN_POINT('Ctrl Pts',(-21.3783873242474,-18.5411721545534,
0.424282751699669));
#213783=CARTESIAN_POINT('Ctrl Pts',(-19.8194849515203,-16.5056185643353,
0.551458558381104));
#213784=CARTESIAN_POINT('Ctrl Pts',(-17.2647560814413,-16.7153568808188,
0.678634365062538));
#213785=CARTESIAN_POINT('Ctrl Pts',(-16.0579473465983,-18.9766153220251,
0.805810171743973));
#213786=CARTESIAN_POINT('Ctrl Pts',(-17.306261185047,-21.2155300370204,
0.932985978425408));
#213787=CARTESIAN_POINT('Ctrl Pts',(-19.8644313952761,-21.3776722353249,
1.06016178510684));
#213788=CARTESIAN_POINT('Ctrl Pts',(-21.3855037526656,-19.3144751713091,
1.18733759178828));
#213789=CARTESIAN_POINT('Ctrl Pts',(-20.4739845399306,-16.9186961805966,
1.31451339846971));
#213790=CARTESIAN_POINT('Ctrl Pts',(-17.9661382589161,-16.3883646063293,
1.44168920515115));
#213791=CARTESIAN_POINT('Ctrl Pts',(-16.1627570764457,-18.2100003769934,
1.56886501183258));
#213792=CARTESIAN_POINT('Ctrl Pts',(-16.7183318894278,-20.7123794251487,
1.69604081851402));
#213793=CARTESIAN_POINT('Ctrl Pts',(-19.1231569823275,-21.5997171847722,
1.82321662519545));
#213794=CARTESIAN_POINT('Ctrl Pts',(-21.1709547522747,-20.0579400230779,
1.95039243187689));
#213795=CARTESIAN_POINT('Ctrl Pts',(-20.9829977631806,-17.5015308787203,
2.07756823855832));
#213796=CARTESIAN_POINT('Ctrl Pts',(-18.7317249295996,-16.2758374662316,
2.20474404523976));
#213797=CARTESIAN_POINT('Ctrl Pts',(-16.4825393242813,-17.5053569009653,
2.33191985192118));
#213798=CARTESIAN_POINT('Ctrl Pts',(-16.2989291514817,-20.062081681679,
2.45909565860262));
#213799=CARTESIAN_POINT('Ctrl Pts',(-18.3493453426023,-21.6003753714481,
2.58627146528406));
#213800=CARTESIAN_POINT('Ctrl Pts',(-20.7526583085904,-20.708949059251,
2.71344727196549));
#213801=CARTESIAN_POINT('Ctrl Pts',(-21.3039775679586,-18.2056310209682,
2.84062307864693));
#213802=CARTESIAN_POINT('Ctrl Pts',(-19.4975019198092,-16.3870602026966,
2.96779888532836));
#213803=CARTESIAN_POINT('Ctrl Pts',(-16.9905606483594,-16.9216624468904,
3.09497469200979));
#213804=CARTESIAN_POINT('Ctrl Pts',(-16.0831167720671,-19.3189733808883,
3.22215049869123));
#213805=CARTESIAN_POINT('Ctrl Pts',(-17.6076937249943,-21.3796090139306,
3.34932630537266));
#213806=CARTESIAN_POINT('Ctrl Pts',(-20.1655867788085,-21.2130640515812,
3.4765021120541));
#213807=CARTESIAN_POINT('Ctrl Pts',(-21.4100878173515,-18.9721331591185,
3.60367791873553));
#213808=CARTESIAN_POINT('Ctrl Pts',(-20.1994443802222,-16.7127313428988,
3.73085372541697));
#213809=CARTESIAN_POINT('Ctrl Pts',(-17.6443466799723,-16.507719534815,
3.8580295320984));
#213810=CARTESIAN_POINT('Ctrl Pts',(-16.0889382693367,-18.545183344418,
3.98520533877984));
#213811=CARTESIAN_POINT('Ctrl Pts',(-16.9602098255379,-20.95587618561,4.11238114546127));
#213812=CARTESIAN_POINT('Ctrl Pts',(-19.458823772974,-21.5281370010973,
4.2395569521427));
#213813=CARTESIAN_POINT('Ctrl Pts',(-21.2924568963431,-19.7369520111678,
4.36673275882414));
#213814=CARTESIAN_POINT('Ctrl Pts',(-20.7788646130614,-17.2256222706107,
4.49390856550557));
#213815=CARTESIAN_POINT('Ctrl Pts',(-18.3892359659074,-16.2981369456807,
4.62108437218701));
#213816=CARTESIAN_POINT('Ctrl Pts',(-16.3159069215641,-17.8054062557716,
4.74826017886844));
#213817=CARTESIAN_POINT('Ctrl Pts',(-16.4610281929029,-20.3646041605579,
4.87543598554988));
#213818=CARTESIAN_POINT('Ctrl Pts',(-18.6914600207125,-21.6278254241348,
5.00261179223131));
#213819=CARTESIAN_POINT('Ctrl Pts',(-20.9609196391894,-20.436142941524,
5.12978759891275));
#213820=CARTESIAN_POINT('Ctrl Pts',(-21.187318706931,-17.8828514263649,
5.25696340559418));
#213821=CARTESIAN_POINT('Ctrl Pts',(-19.1629501311951,-16.3104373686715,
5.38413921227561));
#213822=CARTESIAN_POINT('Ctrl Pts',(-16.7450464337355,-17.1614930713546,
5.51131501895704));
#213823=CARTESIAN_POINT('Ctrl Pts',(-16.1518841849429,-19.6552277496765,
5.63849082563848));
#213824=CARTESIAN_POINT('Ctrl Pts',(-17.9276529322832,-21.503794614907,
5.76566663231992));
#213825=CARTESIAN_POINT('Ctrl Pts',(-20.4431950667104,-21.0112483031962,
5.89284243900135));
#213826=CARTESIAN_POINT('Ctrl Pts',(-21.3906568120407,-18.629469484667,
6.02001824568278));
#213827=CARTESIAN_POINT('Ctrl Pts',(-19.9008008230416,-16.5435923954545,
6.14719405236422));
#213828=CARTESIAN_POINT('Ctrl Pts',(-17.3404774987283,-16.667279800778,
6.27436985904566));
#213829=CARTESIAN_POINT('Ctrl Pts',(-16.0586245775708,-18.8870561831594,
6.40154566572708));
#213830=CARTESIAN_POINT('Ctrl Pts',(-17.2312625539661,-21.1664144866242,
6.52872147240852));
#213831=CARTESIAN_POINT('Ctrl Pts',(-19.7825688666926,-21.414184940675,
6.65589727908996));
#213832=CARTESIAN_POINT('Ctrl Pts',(-21.3718783257522,-19.4030535320888,
6.78307308577139));
#213833=CARTESIAN_POINT('Ctrl Pts',(-20.5410981461279,-16.9781085033506,
6.91024889245283));
#213834=CARTESIAN_POINT('Ctrl Pts',(-18.0524175785914,-16.3640864092651,
7.03742469913425));
#213835=CARTESIAN_POINT('Ctrl Pts',(-16.1890465789213,-18.1243144106463,
7.1646005058157));
#213836=CARTESIAN_POINT('Ctrl Pts',(-16.6605123854672,-20.6438925682982,
7.29177631249713));
#213837=CARTESIAN_POINT('Ctrl Pts',(-19.0342743831914,-21.6112643052322,
7.41895211917856));
#213838=CARTESIAN_POINT('Ctrl Pts',(-21.1325532714676,-20.1389260946729,
7.54612792586));
#213839=CARTESIAN_POINT('Ctrl Pts',(-21.0303084041777,-17.5776568611929,
7.67330373254143));
#213840=CARTESIAN_POINT('Ctrl Pts',(-18.8213431010281,-16.277262156213,
7.80047953922286));
#213841=CARTESIAN_POINT('Ctrl Pts',(-16.5322459238095,-17.4307734099542,
7.92765534590431));
#213842=CARTESIAN_POINT('Ctrl Pts',(-16.2631214552256,-19.979915642092,
8.05483115258573));
#213843=CARTESIAN_POINT('Ctrl Pts',(-18.260874691454,-21.5860090722502,
8.18200695926717));
#213844=CARTESIAN_POINT('Ctrl Pts',(-20.6926910328048,-20.7755626636597,
8.30918276594861));
#213845=CARTESIAN_POINT('Ctrl Pts',(-21.3275299216332,-18.2921106942249,
8.43635857263003));
#213846=CARTESIAN_POINT('Ctrl Pts',(-19.5829660799844,-16.4140662054893,
8.56353437931147));
#213847=CARTESIAN_POINT('Ctrl Pts',(-17.0595285527274,-16.8644184512809,
8.69071018599291));
#213848=CARTESIAN_POINT('Ctrl Pts',(-16.0723146489239,-19.2299971980985,
8.81788599267433));
#213849=CARTESIAN_POINT('Ctrl Pts',(-17.5270318519084,-21.3405307701129,
8.94506179935578));
#213850=CARTESIAN_POINT('Ctrl Pts',(-20.089067417875,-21.2597356094876,
9.07223760603719));
#213851=CARTESIAN_POINT('Ctrl Pts',(-21.4079127329105,-19.0617362613832,
9.19941341271865));
#213852=CARTESIAN_POINT('Ctrl Pts',(-20.2736090772418,-16.7630607044602,
9.32658921940007));
#213853=CARTESIAN_POINT('Ctrl Pts',(-17.7268096521201,-16.4726010903001,
9.45376502608151));
#213854=CARTESIAN_POINT('Ctrl Pts',(-16.104044857895,-18.4568360869378,
9.58094083276294));
#213855=CARTESIAN_POINT('Ctrl Pts',(-16.8941006731258,-20.8953532404716,
9.70811663944438));
#213856=CARTESIAN_POINT('Ctrl Pts',(-19.3721499237325,-21.5509644139779,
9.83529244612582));
#213857=CARTESIAN_POINT('Ctrl Pts',(-21.2647362273657,-19.8221870475835,
9.96246825280725));
#213858=CARTESIAN_POINT('Ctrl Pts',(-20.835529117596,-17.2950670749305,
10.0896440594887));
#213859=CARTESIAN_POINT('Ctrl Pts',(-18.4782994780394,-16.2880802201732,
10.2168198661701));
#213860=CARTESIAN_POINT('Ctrl Pts',(-16.3556591968173,-17.7250744218984,
10.3439956728516));
#213861=CARTESIAN_POINT('Ctrl Pts',(-16.414998986037,-20.2876966899422,
10.471171479533));
#213862=CARTESIAN_POINT('Ctrl Pts',(-18.6018782721322,-21.6249001476502,
10.5983472862144));
#213863=CARTESIAN_POINT('Ctrl Pts',(-20.9099710431467,-20.5098836187822,
10.7255230928959));
#213864=CARTESIAN_POINT('Ctrl Pts',(-21.2217454380686,-17.965605562844,
10.8526988995773));
#213865=CARTESIAN_POINT('Ctrl Pts',(-19.2511678004582,-16.3262831804529,
10.9798747062588));
#213866=CARTESIAN_POINT('Ctrl Pts',(-16.8061208049812,-17.0958930096308,
11.1070505129402));
#213867=CARTESIAN_POINT('Ctrl Pts',(-16.1297833132563,-19.5683657994802,
11.2342263196216));
#213868=CARTESIAN_POINT('Ctrl Pts',(-17.8426529957019,-21.4753612242825,
11.361402126303));
#213869=CARTESIAN_POINT('Ctrl Pts',(-20.3732782313567,-21.0673293432663,
11.4885779329845));
#213870=CARTESIAN_POINT('Ctrl Pts',(-21.3999674348234,-18.7186140819493,
11.6157537396659));
#213871=CARTESIAN_POINT('Ctrl Pts',(-19.98079698544,-16.5840159148801,11.7429295463474));
#213872=CARTESIAN_POINT('Ctrl Pts',(-17.4177676868637,-16.6218961722405,
11.8701053530288));
#213873=CARTESIAN_POINT('Ctrl Pts',(-16.0622998409991,-18.7975020690164,
11.9972811597103));
#213874=CARTESIAN_POINT('Ctrl Pts',(-17.1579510666044,-21.1148502282466,
12.1244569663916));
#213875=CARTESIAN_POINT('Ctrl Pts',(-19.6995293679712,-21.4479175446854,
12.2516327730731));
#213876=CARTESIAN_POINT('Ctrl Pts',(-21.3552944017355,-19.4911354279892,
12.3788085797545));
#213877=CARTESIAN_POINT('Ctrl Pts',(-20.6061845177868,-17.0397300186315,
12.505984386436));
#213878=CARTESIAN_POINT('Ctrl Pts',(-18.1394615396447,-16.3427136283187,
12.6331601931174));
#213879=CARTESIAN_POINT('Ctrl Pts',(-16.2181906976602,-18.0395555334466,
12.7603359997988));
#213880=CARTESIAN_POINT('Ctrl Pts',(-16.6050187418368,-20.5735086039467,
12.8875118064803));
#213881=CARTESIAN_POINT('Ctrl Pts',(-18.9450549508987,-21.6198281725,13.0146876131617));
#213882=CARTESIAN_POINT('Ctrl Pts',(-21.0914613420586,-20.2185809768753,
13.1418634198431));
#213883=CARTESIAN_POINT('Ctrl Pts',(-21.0750432724325,-17.6553243478488,
13.2690392265246));
#213884=CARTESIAN_POINT('Ctrl Pts',(-18.9108633018819,-16.2816871489036,
13.396215033206));
#213885=CARTESIAN_POINT('Ctrl Pts',(-16.5844222292293,-17.3578962525319,
13.5233908398874));
#213886=CARTESIAN_POINT('Ctrl Pts',(-16.2300853434153,-19.8965966032252,
13.6505666465689));
#213887=CARTESIAN_POINT('Ctrl Pts',(-18.1729347445473,-21.5686881987366,
13.7777424532503));
#213888=CARTESIAN_POINT('Ctrl Pts',(-20.6305266939199,-20.8401307818932,
13.9049182599318));
#213889=CARTESIAN_POINT('Ctrl Pts',(-21.348173113343,-18.3793305632757,
14.0320940666132));
#213890=CARTESIAN_POINT('Ctrl Pts',(-19.6674779551561,-16.443919008979,
14.1592698732946));
#213891=CARTESIAN_POINT('Ctrl Pts',(-17.1303747112896,-16.8095160948814,
14.2864456799761));
#213892=CARTESIAN_POINT('Ctrl Pts',(-16.0644981376042,-19.140709186182,
14.4136214866575));
#213893=CARTESIAN_POINT('Ctrl Pts',(-17.4477238346954,-21.2987733117736,
14.5407972933389));
#213894=CARTESIAN_POINT('Ctrl Pts',(-20.0110280781508,-21.3038185809918,
14.6679731000203));
#213895=CARTESIAN_POINT('Ctrl Pts',(-21.4027383212044,-19.1512162724734,
14.7951489067018));
#213896=CARTESIAN_POINT('Ctrl Pts',(-20.3460467951339,-16.8158453987172,
14.9223247133832));
#213897=CARTESIAN_POINT('Ctrl Pts',(-17.8104023894363,-16.4402637869306,
15.0495005200647));
#213898=CARTESIAN_POINT('Ctrl Pts',(-16.1221014664979,-18.3690442547039,
15.1766763267461));
#213899=CARTESIAN_POINT('Ctrl Pts',(-16.8300553353419,-20.8326504364724,
15.3038521334275));
#213900=CARTESIAN_POINT('Ctrl Pts',(-19.2847602618764,-21.5708765691077,
15.4310279401089));
#213901=CARTESIAN_POINT('Ctrl Pts',(-21.2341768321763,-19.9064459953984,
15.5582037467904));
#213902=CARTESIAN_POINT('Ctrl Pts',(-20.8898363374295,-17.3663704605105,
15.6853795534718));
#213903=CARTESIAN_POINT('Ctrl Pts',(-18.5676498093848,-16.2810116128359,
15.8125553601533));
#213904=CARTESIAN_POINT('Ctrl Pts',(-16.3980792563722,-17.6461188301484,
15.9397311668347));
#213905=CARTESIAN_POINT('Ctrl Pts',(-16.3715710020456,-20.2092909686735,
16.0669069735161));
#213906=CARTESIAN_POINT('Ctrl Pts',(-18.5124447244619,-21.618976679719,
16.1940827801976));
#213907=CARTESIAN_POINT('Ctrl Pts',(-20.8565816609132,-20.5818768183634,
16.321258586879));
#213908=CARTESIAN_POINT('Ctrl Pts',(-21.2533816657522,-18.0494661377238,
16.4484343935604));
#213909=CARTESIAN_POINT('Ctrl Pts',(-19.338805362725,-16.3450742581534,
16.5756102002418));
#213910=CARTESIAN_POINT('Ctrl Pts',(-16.869357677852,-17.0323749426676,
16.7027860069233));
#213911=CARTESIAN_POINT('Ctrl Pts',(-16.1106035907951,-19.4808124719162,
16.8299618136047));
#213912=CARTESIAN_POINT('Ctrl Pts',(-17.7586528828391,-21.4440973799852,
16.9571376202862));
#213913=CARTESIAN_POINT('Ctrl Pts',(-20.3015226180088,-21.1210376189256,
17.0843134269676));
#213914=CARTESIAN_POINT('Ctrl Pts',(-21.4062876425816,-18.8080204681591,
17.211489233649));
#213915=CARTESIAN_POINT('Ctrl Pts',(-20.0593946159625,-16.6270956014793,
17.3386650403305));
#213916=CARTESIAN_POINT('Ctrl Pts',(-17.4965342924651,-16.5791262206009,
17.4658408470119));
#213917=CARTESIAN_POINT('Ctrl Pts',(-16.0689719498474,-18.7081212551652,
17.5930166536933));
#213918=CARTESIAN_POINT('Ctrl Pts',(-17.0864074329483,-21.0608599012923,
17.7201924603748));
#213919=CARTESIAN_POINT('Ctrl Pts',(-19.6154068351929,-21.4788504785931,
17.8473682670562));
#213920=CARTESIAN_POINT('Ctrl Pts',(-21.3357701724232,-19.5786125758088,
17.9745440737377));
#213921=CARTESIAN_POINT('Ctrl Pts',(-20.6691708605291,-17.1034965266906,
18.1017198804191));
#213922=CARTESIAN_POINT('Ctrl Pts',(-18.2271723943392,-16.3242676832537,
18.2288956871005));
#213923=CARTESIAN_POINT('Ctrl Pts',(-16.2501567990929,-17.9558201449997,
18.3560714937819));
#213924=CARTESIAN_POINT('Ctrl Pts',(-16.5519131759471,-20.5013057937568,
18.4832473004634));
#213925=CARTESIAN_POINT('Ctrl Pts',(-18.8555987783568,-21.6253995376139,
18.6104231071448));
#213926=CARTESIAN_POINT('Ctrl Pts',(-21.0477250487613,-20.2968151353882,
18.7375989138263));
#213927=CARTESIAN_POINT('Ctrl Pts',(-21.1171521931581,-17.7344463154909,
18.8647747205077));
#213928=CARTESIAN_POINT('Ctrl Pts',(-19.000185114941,-16.2891074304433,
18.9919505271891));
#213929=CARTESIAN_POINT('Ctrl Pts',(-16.6390097160369,-17.2868072017201,
19.1191263338706));
#213930=CARTESIAN_POINT('Ctrl Pts',(-16.1998578710576,-19.8122180089903,
19.246302140552));
#213931=CARTESIAN_POINT('Ctrl Pts',(-18.0856241463476,-21.5484321897643,
19.3734779472334));
#213932=CARTESIAN_POINT('Ctrl Pts',(-20.566235017753,-20.9025809783934,
19.5006537539149));
#213933=CARTESIAN_POINT('Ctrl Pts',(-21.3658839949308,-18.4671928068505,
19.6278295605963));
#213934=CARTESIAN_POINT('Ctrl Pts',(-19.7509427344116,-16.4765851044279,
19.7550053672777));
#213935=CARTESIAN_POINT('Ctrl Pts',(-17.2030196827703,-16.757017004315,
19.8821811739592));
#213936=CARTESIAN_POINT('Ctrl Pts',(-16.0596759541972,-19.0512094179914,
20.0093569806406));
#213937=CARTESIAN_POINT('Ctrl Pts',(-17.3698587327168,-21.2543836348827,
20.136532787322));
#213938=CARTESIAN_POINT('Ctrl Pts',(-19.9315561044895,-21.3452632166212,
20.2637085940035));
#213939=CARTESIAN_POINT('Ctrl Pts',(-21.394570756024,-19.2404734037209,
20.3908844006849));
#213940=CARTESIAN_POINT('Ctrl Pts',(-20.4166755682946,-16.8710250976204,
20.5180602073664));
#213941=CARTESIAN_POINT('Ctrl Pts',(-17.8950324982703,-16.4107460543773,
20.6452360140478));
#213942=CARTESIAN_POINT('Ctrl Pts',(-16.1430851969531,-18.281902167926,
20.7724118207292));
#213943=CARTESIAN_POINT('Ctrl Pts',(-16.7681507463741,-20.7678461146898,
20.8995876274106));
#213944=CARTESIAN_POINT('Ctrl Pts',(-19.1967429963892,-21.58783570276,21.0267634340921));
#213945=CARTESIAN_POINT('Ctrl Pts',(-21.2008319023016,-19.989664067993,
21.1539392407735));
#213946=CARTESIAN_POINT('Ctrl Pts',(-20.9416889151052,-17.4393951699213,
21.2811150474549));
#213947=CARTESIAN_POINT('Ctrl Pts',(-18.6572569499448,-16.2770494137143,
21.4082908541364));
#213948=CARTESIAN_POINT('Ctrl Pts',(-16.4429842219372,-17.568415375407,
21.5354666608178));
#213949=CARTESIAN_POINT('Ctrl Pts',(-16.3310537276957,-20.1298849908433,
21.6626424674993));
#213950=CARTESIAN_POINT('Ctrl Pts',(-18.4227563856442,-21.6092689274519,
21.7898182741806));
#213951=CARTESIAN_POINT('Ctrl Pts',(-20.8017892824853,-20.6535945073695,
21.9169940808621));
#213952=CARTESIAN_POINT('Ctrl Pts',(-21.2802305760296,-18.1311084332283,
22.0441698875435));
#213953=CARTESIAN_POINT('Ctrl Pts',(-20.0469417623915,-16.9604786618337,
22.1289537586645));
#213954=CARTESIAN_POINT('Ctrl Pts',(-19.319022416489,-16.7656980906223,
22.171345694225));
#213955=CARTESIAN_POINT('Ctrl Pts',(-16.8880688553878,-17.3975534516058,
-0.171094837061568));
#213956=CARTESIAN_POINT('Ctrl Pts',(-16.3702697975385,-18.0124051053735,
-0.12868424499791));
#213957=CARTESIAN_POINT('Ctrl Pts',(-16.0068254820486,-19.7893209524259,
-0.043881717373774));
#213958=CARTESIAN_POINT('Ctrl Pts',(-17.9658932450075,-21.7021720009294,
0.0833127458108395));
#213959=CARTESIAN_POINT('Ctrl Pts',(-20.6289595651085,-21.0844926888652,
0.210488552492275));
#213960=CARTESIAN_POINT('Ctrl Pts',(-21.5536820848537,-18.5139386369225,
0.337664359173709));
#213961=CARTESIAN_POINT('Ctrl Pts',(-19.8914410613435,-16.3434494886539,
0.464840165855143));
#213962=CARTESIAN_POINT('Ctrl Pts',(-17.1673608327897,-16.567091225276,
0.592015972536577));
#213963=CARTESIAN_POINT('Ctrl Pts',(-15.8805535113812,-18.9782470561293,
0.719191779218012));
#213964=CARTESIAN_POINT('Ctrl Pts',(-17.2116172834215,-21.365578009315,
0.846367585899446));
#213965=CARTESIAN_POINT('Ctrl Pts',(-19.939366976384,-21.5384685112341,
0.97354339258088));
#213966=CARTESIAN_POINT('Ctrl Pts',(-21.5612702568039,-19.3385034208011,
1.10071919926231));
#213967=CARTESIAN_POINT('Ctrl Pts',(-20.5893270128691,-16.7839097584284,
1.22789500594375));
#213968=CARTESIAN_POINT('Ctrl Pts',(-17.9152371905106,-16.2184228400477,
1.35507081262518));
#213969=CARTESIAN_POINT('Ctrl Pts',(-15.9923110118271,-18.1608136920126,
1.48224661930662));
#213970=CARTESIAN_POINT('Ctrl Pts',(-16.5847145272265,-20.8290738621089,
1.60942242598805));
#213971=CARTESIAN_POINT('Ctrl Pts',(-19.1489539521699,-21.7752326797234,
1.73659823266948));
#213972=CARTESIAN_POINT('Ctrl Pts',(-21.3324989390857,-20.1312520866371,
1.86377403935092));
#213973=CARTESIAN_POINT('Ctrl Pts',(-21.1320824002478,-17.4053801994873,
1.99094984603235));
#213974=CARTESIAN_POINT('Ctrl Pts',(-18.731574116624,-16.0984363471145,
2.11812565271379));
#213975=CARTESIAN_POINT('Ctrl Pts',(-16.3332914223019,-17.4094598463232,
2.24530145939522));
#213976=CARTESIAN_POINT('Ctrl Pts',(-16.1375098474575,-20.1356682931634,
2.37247726607666));
#213977=CARTESIAN_POINT('Ctrl Pts',(-18.3238468290274,-21.7759344971771,
2.49965307275809));
#213978=CARTESIAN_POINT('Ctrl Pts',(-20.8864738891242,-20.8254160994288,
2.62682887943953));
#213979=CARTESIAN_POINT('Ctrl Pts',(-21.4743397529562,-18.1561546941444,
2.75400468612096));
#213980=CARTESIAN_POINT('Ctrl Pts',(-19.5481139784241,-16.2170319683244,
2.88118049280239));
#213981=CARTESIAN_POINT('Ctrl Pts',(-16.8749891581411,-16.7870726566358,
3.00835629948383));
#213982=CARTESIAN_POINT('Ctrl Pts',(-15.9073914021204,-19.3432998138438,
3.13553210616526));
#213983=CARTESIAN_POINT('Ctrl Pts',(-17.533031595496,-21.5405336776668,
3.2627079128467));
#213984=CARTESIAN_POINT('Ctrl Pts',(-20.2604857595204,-21.3629485552631,
3.38988371952813));
#213985=CARTESIAN_POINT('Ctrl Pts',(-21.5874839835647,-18.9734677734828,
3.51705952620957));
#213986=CARTESIAN_POINT('Ctrl Pts',(-20.2965877598843,-16.5642916421105,
3.644235332891));
#213987=CARTESIAN_POINT('Ctrl Pts',(-17.5721142516412,-16.3456897311358,
3.77141113957244));
#213988=CARTESIAN_POINT('Ctrl Pts',(-15.9135988027563,-18.5182157260222,
3.89858694625387));
#213989=CARTESIAN_POINT('Ctrl Pts',(-16.8426263985009,-21.0887118685754,
4.0257627529353));
#213990=CARTESIAN_POINT('Ctrl Pts',(-19.5068718817363,-21.6989074910159,
4.15293855961674));
#213991=CARTESIAN_POINT('Ctrl Pts',(-21.4620553833173,-19.7889859827511,
4.28011436629817));
#213992=CARTESIAN_POINT('Ctrl Pts',(-20.9144173929179,-17.1111817845236,
4.40729017297961));
#213993=CARTESIAN_POINT('Ctrl Pts',(-18.3663817764822,-16.1222140449305,
4.53446597966104));
#213994=CARTESIAN_POINT('Ctrl Pts',(-16.1556130631639,-17.7293992827899,
4.66164178634248));
#213995=CARTESIAN_POINT('Ctrl Pts',(-16.310354331651,-20.4582447955307,
4.78881759302391));
#213996=CARTESIAN_POINT('Ctrl Pts',(-18.6886400724331,-21.8052041964678,
4.91599339970535));
#213997=CARTESIAN_POINT('Ctrl Pts',(-21.1085407314031,-20.5345258369701,
5.04316920638678));
#213998=CARTESIAN_POINT('Ctrl Pts',(-21.34994764993,-17.8119782446832,5.17034501306821));
#213999=CARTESIAN_POINT('Ctrl Pts',(-19.1913849636685,-16.1353298551694,
5.29752081974965));
#214000=CARTESIAN_POINT('Ctrl Pts',(-16.6131999617537,-17.0428015012722,
5.42469662643108));
#214001=CARTESIAN_POINT('Ctrl Pts',(-15.9807173632341,-19.7018442717348,
5.55187243311253));
#214002=CARTESIAN_POINT('Ctrl Pts',(-17.8742006959542,-21.672951463465,
5.67904823979394));
#214003=CARTESIAN_POINT('Ctrl Pts',(-20.556496524973,-21.1477545687602,
5.80622404647539));
#214004=CARTESIAN_POINT('Ctrl Pts',(-21.5667649092207,-18.6080891411163,
5.93339985315682));
#214005=CARTESIAN_POINT('Ctrl Pts',(-19.9781473104775,-16.3839405809831,
6.06057565983826));
#214006=CARTESIAN_POINT('Ctrl Pts',(-17.2481017748621,-16.5158271460542,
6.18775146651969));
#214007=CARTESIAN_POINT('Ctrl Pts',(-15.8812756355658,-18.8827510986805,
6.31492727320112));
#214008=CARTESIAN_POINT('Ctrl Pts',(-17.1316470405952,-21.3132066201958,
6.44210307988256));
#214009=CARTESIAN_POINT('Ctrl Pts',(-19.8520778326375,-21.5774016206925,
6.569278886564));
#214010=CARTESIAN_POINT('Ctrl Pts',(-21.5467416089716,-19.4329535850057,
6.69645469324542));
#214011=CARTESIAN_POINT('Ctrl Pts',(-20.6608895375072,-16.8472604864224,
6.82363049992686));
#214012=CARTESIAN_POINT('Ctrl Pts',(-18.0072359116326,-16.1925352566794,
6.95080630660829));
#214013=CARTESIAN_POINT('Ctrl Pts',(-16.0203432287685,-18.0694476572352,
7.07798211328973));
#214014=CARTESIAN_POINT('Ctrl Pts',(-16.5230622049748,-20.7560470549016,
7.20515791997116));
#214015=CARTESIAN_POINT('Ctrl Pts',(-19.0541793818409,-21.7875452514841,
7.3323337266526));
#214016=CARTESIAN_POINT('Ctrl Pts',(-21.2915518484416,-20.2176066736166,
7.45950953333402));
#214017=CARTESIAN_POINT('Ctrl Pts',(-21.1825292336674,-17.4865525251151,
7.58668534001548));
#214018=CARTESIAN_POINT('Ctrl Pts',(-18.8271330198668,-16.0999554788923,
7.71386114669689));
#214019=CARTESIAN_POINT('Ctrl Pts',(-16.3862930408257,-17.3299322629389,
7.84103695337835));
#214020=CARTESIAN_POINT('Ctrl Pts',(-16.0993284816994,-20.0480555188611,
7.96821276005976));
#214021=CARTESIAN_POINT('Ctrl Pts',(-18.2295115144572,-21.760615865106,
8.09538856674121));
#214022=CARTESIAN_POINT('Ctrl Pts',(-20.8225314206137,-20.8964454774766,
8.22256437342263));
#214023=CARTESIAN_POINT('Ctrl Pts',(-21.4994533772365,-18.2483670501596,
8.34974018010408));
#214024=CARTESIAN_POINT('Ctrl Pts',(-19.6392435036391,-16.245828181935,
8.4769159867855));
#214025=CARTESIAN_POINT('Ctrl Pts',(-16.9485289012012,-16.7260339928192,
8.60409179346695));
#214026=CARTESIAN_POINT('Ctrl Pts',(-15.8958732130767,-19.2484254562599,
8.73126760014836));
#214027=CARTESIAN_POINT('Ctrl Pts',(-17.4470226979395,-21.4988649618209,
8.85844340682981));
#214028=CARTESIAN_POINT('Ctrl Pts',(-20.1788939786226,-21.4127139411785,
8.98561921351124));
#214029=CARTESIAN_POINT('Ctrl Pts',(-21.5851647141539,-19.0690106086366,
9.11279502019268));
#214030=CARTESIAN_POINT('Ctrl Pts',(-20.3756687876888,-16.617957305168,
9.23997082687412));
#214031=CARTESIAN_POINT('Ctrl Pts',(-17.6600436419756,-16.3082433071803,
9.36714663355554));
#214032=CARTESIAN_POINT('Ctrl Pts',(-15.9297067975006,-18.4240119848083,
9.49432244023699));
#214033=CARTESIAN_POINT('Ctrl Pts',(-16.772134912253,-21.0241768957426,
9.62149824691841));
#214034=CARTESIAN_POINT('Ctrl Pts',(-19.4144524779331,-21.7232481186362,
9.74867405359986));
#214035=CARTESIAN_POINT('Ctrl Pts',(-21.4324971287534,-19.8798711957376,
9.87584986028127));
#214036=CARTESIAN_POINT('Ctrl Pts',(-20.9748381515633,-17.1852300409311,
10.0030256669627));
#214037=CARTESIAN_POINT('Ctrl Pts',(-18.461349252415,-16.1114906654595,
10.1302014736441));
#214038=CARTESIAN_POINT('Ctrl Pts',(-16.1980004915621,-17.6437423025364,
10.2573772803256));
#214039=CARTESIAN_POINT('Ctrl Pts',(-16.2612738778198,-20.3762391774058,
10.384553087007));
#214040=CARTESIAN_POINT('Ctrl Pts',(-18.5931200064859,-21.8020850052583,
10.5117288936884));
#214041=CARTESIAN_POINT('Ctrl Pts',(-21.0542147852026,-20.6131547370118,
10.6389047003698));
#214042=CARTESIAN_POINT('Ctrl Pts',(-21.3866565072667,-17.900218100448,
10.7660805070513));
#214043=CARTESIAN_POINT('Ctrl Pts',(-19.2854505263445,-16.152226075776,
10.8932563137327));
#214044=CARTESIAN_POINT('Ctrl Pts',(-16.678322914381,-16.9728528530119,
11.0204321204142));
#214045=CARTESIAN_POINT('Ctrl Pts',(-15.9571514387634,-19.6092242978837,
11.1476079270956));
#214046=CARTESIAN_POINT('Ctrl Pts',(-17.7835661674212,-21.6426332413875,
11.274783733777));
#214047=CARTESIAN_POINT('Ctrl Pts',(-20.4819449468934,-21.2075531854514,
11.4019595404585));
#214048=CARTESIAN_POINT('Ctrl Pts',(-21.5766927272896,-18.7031430772827,
11.5291353471399));
#214049=CARTESIAN_POINT('Ctrl Pts',(-20.0634463678067,-16.4270437499047,
11.6563111538213));
#214050=CARTESIAN_POINT('Ctrl Pts',(-17.3305154806086,-16.4674350655298,
11.7834869605028));
#214051=CARTESIAN_POINT('Ctrl Pts',(-15.8851945298786,-18.78726049904,11.9106627671842));
#214052=CARTESIAN_POINT('Ctrl Pts',(-17.0534757811762,-21.2582241997943,
12.0378385738656));
#214053=CARTESIAN_POINT('Ctrl Pts',(-19.7635336981482,-21.6133703376545,
12.1650143805471));
#214054=CARTESIAN_POINT('Ctrl Pts',(-21.5290583471371,-19.526874373989,
12.2921901872285));
#214055=CARTESIAN_POINT('Ctrl Pts',(-20.7302904435136,-16.9129668529163,
12.4193659939099));
#214056=CARTESIAN_POINT('Ctrl Pts',(-18.1000499617251,-16.1697456876228,
12.5465418005913));
#214057=CARTESIAN_POINT('Ctrl Pts',(-16.0514192926768,-17.9790701677574,
12.6737176072728));
#214058=CARTESIAN_POINT('Ctrl Pts',(-16.4638899228612,-20.6809973821388,
12.8008934139542));
#214059=CARTESIAN_POINT('Ctrl Pts',(-18.9590456498985,-21.7966768120881,
12.9280692206357));
#214060=CARTESIAN_POINT('Ctrl Pts',(-21.2477359610623,-20.3025418275019,
13.0552450273171));
#214061=CARTESIAN_POINT('Ctrl Pts',(-21.2302295480009,-17.569368540262,
13.1824208339985));
#214062=CARTESIAN_POINT('Ctrl Pts',(-18.9225874581277,-16.1046738015453,
13.30959664068));
#214063=CARTESIAN_POINT('Ctrl Pts',(-16.44192808048,-17.2522241249159,13.4367724473614));
#214064=CARTESIAN_POINT('Ctrl Pts',(-16.0641024269644,-19.9592133136872,
13.5639482540428));
#214065=CARTESIAN_POINT('Ctrl Pts',(-18.1357420841767,-21.7421468018591,
13.6911240607243));
#214066=CARTESIAN_POINT('Ctrl Pts',(-20.7562462470829,-20.9652937753664,
13.8182998674057));
#214067=CARTESIAN_POINT('Ctrl Pts',(-21.521464993048,-18.3413686690794,
13.9454756740872));
#214068=CARTESIAN_POINT('Ctrl Pts',(-19.7293576174809,-16.2776599088574,
14.0726514807686));
#214069=CARTESIAN_POINT('Ctrl Pts',(-17.0240714067361,-16.6674921939926,
14.19982728745));
#214070=CARTESIAN_POINT('Ctrl Pts',(-15.8875385501732,-19.1532185985939,
14.3270030941314));
#214071=CARTESIAN_POINT('Ctrl Pts',(-17.3624574025039,-21.4543394280201,
14.4541789008129));
#214072=CARTESIAN_POINT('Ctrl Pts',(-20.0956814605031,-21.4597191449386,
14.5813547074943));
#214073=CARTESIAN_POINT('Ctrl Pts',(-21.5796472939737,-19.1644221929799,
14.7085305141757));
#214074=CARTESIAN_POINT('Ctrl Pts',(-20.4529083560135,-16.6742410633702,
14.8357063208572));
#214075=CARTESIAN_POINT('Ctrl Pts',(-17.7491776888957,-16.2737623844548,
14.9628821275386));
#214076=CARTESIAN_POINT('Ctrl Pts',(-15.9489603672498,-18.3304004876284,
15.0900579342201));
#214077=CARTESIAN_POINT('Ctrl Pts',(-16.7038440495977,-20.9573175625861,
15.2172337409015));
#214078=CARTESIAN_POINT('Ctrl Pts',(-19.3212698107507,-21.7444802379159,
15.3444095475829));
#214079=CARTESIAN_POINT('Ctrl Pts',(-21.3999119706151,-19.9697156158284,
15.4715853542643));
#214080=CARTESIAN_POINT('Ctrl Pts',(-21.032745362598,-17.2612600827733,
15.5987611609458));
#214081=CARTESIAN_POINT('Ctrl Pts',(-18.5566225606254,-16.1039534846195,
15.7259369676272));
#214082=CARTESIAN_POINT('Ctrl Pts',(-16.2432325499933,-17.5595527946246,
15.8531127743086));
#214083=CARTESIAN_POINT('Ctrl Pts',(-16.2149670802795,-20.2926359905412,
15.9802885809901));
#214084=CARTESIAN_POINT('Ctrl Pts',(-18.4977579655933,-21.7957688743899,
16.1074643876715));
#214085=CARTESIAN_POINT('Ctrl Pts',(-20.997286254641,-20.6899203201883,
16.234640194353));
#214086=CARTESIAN_POINT('Ctrl Pts',(-21.4203898804431,-17.9896377397141,
16.3618160010344));
#214087=CARTESIAN_POINT('Ctrl Pts',(-19.378897527099,-16.1722628021139,
16.4889918077158));
#214088=CARTESIAN_POINT('Ctrl Pts',(-16.7457517194962,-16.9051242136259,
16.6161676143973));
#214089=CARTESIAN_POINT('Ctrl Pts',(-15.9367003046499,-19.5158671156972,
16.7433434210787));
#214090=CARTESIAN_POINT('Ctrl Pts',(-17.6939977402874,-21.6092969366562,
16.8705192277601));
#214091=CARTESIAN_POINT('Ctrl Pts',(-20.4054326993911,-21.2648217486819,
16.9976950344416));
#214092=CARTESIAN_POINT('Ctrl Pts',(-21.5834318976165,-18.798476156199,
17.124870841123));
#214093=CARTESIAN_POINT('Ctrl Pts',(-20.147254185468,-16.4729791616393,
17.2520466478045));
#214094=CARTESIAN_POINT('Ctrl Pts',(-17.4145034745997,-16.4218299208892,
17.3792224544858));
#214095=CARTESIAN_POINT('Ctrl Pts',(-15.8923089285959,-18.691954687658,
17.5063982611673));
#214096=CARTESIAN_POINT('Ctrl Pts',(-16.9771895653652,-21.2006548882669,
17.6335740678487));
#214097=CARTESIAN_POINT('Ctrl Pts',(-19.6738347359605,-21.646353796156,
17.7607498745302));
#214098=CARTESIAN_POINT('Ctrl Pts',(-21.5082398690315,-19.6201503265241,
17.8879256812116));
#214099=CARTESIAN_POINT('Ctrl Pts',(-20.7974521110171,-16.980960402401,
18.015101487893));
#214100=CARTESIAN_POINT('Ctrl Pts',(-18.1935751134159,-16.1500769725442,
18.1422772945745));
#214101=CARTESIAN_POINT('Ctrl Pts',(-16.0855044067243,-17.8897840134535,
18.2694531012559));
#214102=CARTESIAN_POINT('Ctrl Pts',(-16.407264022649,-20.6040082933991,
18.3966289079374));
#214103=CARTESIAN_POINT('Ctrl Pts',(-18.8636594843459,-21.8026174994662,
18.5238047146188));
#214104=CARTESIAN_POINT('Ctrl Pts',(-21.2011004165875,-20.3859620788242,
18.6509805213002));
#214105=CARTESIAN_POINT('Ctrl Pts',(-21.275129842407,-17.6537354530185,
18.7781563279817));
#214106=CARTESIAN_POINT('Ctrl Pts',(-19.0178303575923,-16.1125859688478,
18.9053321346631));
#214107=CARTESIAN_POINT('Ctrl Pts',(-16.500134137209,-17.1764226259579,
19.0325079413445));
#214108=CARTESIAN_POINT('Ctrl Pts',(-16.031871194612,-19.8692413158911,
19.1596837480259));
#214109=CARTESIAN_POINT('Ctrl Pts',(-18.0426437217303,-21.7205480348836,
19.2868595547074));
#214110=CARTESIAN_POINT('Ctrl Pts',(-20.6876927164292,-21.0318837558328,
19.4140353613888));
#214111=CARTESIAN_POINT('Ctrl Pts',(-21.5403499177572,-18.4350552451234,
19.5412111680702));
#214112=CARTESIAN_POINT('Ctrl Pts',(-19.8183552240814,-16.3124914190809,
19.6683869747517));
#214113=CARTESIAN_POINT('Ctrl Pts',(-17.1015319673585,-16.6115129719686,
19.7955627814331));
#214114=CARTESIAN_POINT('Ctrl Pts',(-15.8823967072827,-19.0577859474646,
19.9227385881146));
#214115=CARTESIAN_POINT('Ctrl Pts',(-17.2794306722399,-21.4070071875673,
20.049914394796));
#214116=CARTESIAN_POINT('Ctrl Pts',(-20.0109413400502,-21.5039111192106,
20.1770902014775));
#214117=CARTESIAN_POINT('Ctrl Pts',(-21.5709383060712,-19.2595961229167,
20.3042660081589));
#214118=CARTESIAN_POINT('Ctrl Pts',(-20.5282190658065,-16.7330785895595,
20.4314418148403));
#214119=CARTESIAN_POINT('Ctrl Pts',(-17.8394178740343,-16.242287940109,
20.5586176215217));
#214120=CARTESIAN_POINT('Ctrl Pts',(-15.9713350959043,-18.2374818071192,
20.6857934282033));
#214121=CARTESIAN_POINT('Ctrl Pts',(-16.6378358446413,-20.8882174033637,
20.8129692348846));
#214122=CARTESIAN_POINT('Ctrl Pts',(-19.2274179364899,-21.762563581795,
20.9401450415661));
#214123=CARTESIAN_POINT('Ctrl Pts',(-21.3643566264617,-20.0584501617399,
21.0673208482475));
#214124=CARTESIAN_POINT('Ctrl Pts',(-21.0880352148013,-17.3391255539126,
21.1944966549289));
#214125=CARTESIAN_POINT('Ctrl Pts',(-18.6521697017704,-16.099728633828,
21.3216724616103));
#214126=CARTESIAN_POINT('Ctrl Pts',(-16.2911142372801,-17.4766984270906,
21.4488482682918));
#214127=CARTESIAN_POINT('Ctrl Pts',(-16.171763941479,-20.2079662407414,
21.5760240749733));
#214128=CARTESIAN_POINT('Ctrl Pts',(-18.4021242436095,-21.7854176013747,
21.7031998816546));
#214129=CARTESIAN_POINT('Ctrl Pts',(-20.9388617241559,-20.7663921293681,
21.8303756883361));
#214130=CARTESIAN_POINT('Ctrl Pts',(-21.4490185879752,-18.0766920512704,
21.9575514950176));
#214131=CARTESIAN_POINT('Ctrl Pts',(-20.1339758401221,-16.8284619738791,
22.0423353661385));
#214132=CARTESIAN_POINT('Ctrl Pts',(-19.3578031818887,-16.6207695219882,
22.0847273016989));
#214133=CARTESIAN_POINT('Ctrl Pts',(-16.7733105073354,-17.3009161969877,
-0.257713229587528));
#214134=CARTESIAN_POINT('Ctrl Pts',(-16.2233207772202,-17.9539921151271,
-0.21530263752387));
#214135=CARTESIAN_POINT('Ctrl Pts',(-15.8372817569514,-19.8413757484949,
-0.130500109899735));
#214136=CARTESIAN_POINT('Ctrl Pts',(-17.9181413759371,-21.8731454397858,
-0.00330564671512121));
#214137=CARTESIAN_POINT('Ctrl Pts',(-20.7467659253037,-21.217066072722,
0.123870159966314));
#214138=CARTESIAN_POINT('Ctrl Pts',(-21.7289768454601,-18.4867051192915,
0.251045966647748));
#214139=CARTESIAN_POINT('Ctrl Pts',(-19.9633971711666,-16.1812804129726,
0.378221773329183));
#214140=CARTESIAN_POINT('Ctrl Pts',(-17.0699655841381,-16.4188255697332,
0.505397580010616));
#214141=CARTESIAN_POINT('Ctrl Pts',(-15.703159676164,-18.9798787902335,
0.632573386692052));
#214142=CARTESIAN_POINT('Ctrl Pts',(-17.1169733817962,-21.5156259816095,
0.759749193373485));
#214143=CARTESIAN_POINT('Ctrl Pts',(-20.0143025574919,-21.6992647871434,
0.88692500005492));
#214144=CARTESIAN_POINT('Ctrl Pts',(-21.7370367609421,-19.362531670293,
1.01410080673636));
#214145=CARTESIAN_POINT('Ctrl Pts',(-20.7046694858076,-16.6491233362602,
1.14127661341778));
#214146=CARTESIAN_POINT('Ctrl Pts',(-17.8643361221052,-16.0484810737661,
1.26845242009923));
#214147=CARTESIAN_POINT('Ctrl Pts',(-15.8218649472086,-18.1116270070318,
1.39562822678066));
#214148=CARTESIAN_POINT('Ctrl Pts',(-16.4510971650251,-20.9457682990692,
1.52280403346208));
#214149=CARTESIAN_POINT('Ctrl Pts',(-19.1747509220124,-21.9507481746746,
1.64997984014353));
#214150=CARTESIAN_POINT('Ctrl Pts',(-21.4940431258966,-20.2045641501962,
1.77715564682495));
#214151=CARTESIAN_POINT('Ctrl Pts',(-21.2811670373152,-17.3092295202543,
1.9043314535064));
#214152=CARTESIAN_POINT('Ctrl Pts',(-18.7314233036483,-15.9210352279973,
2.03150726018784));
#214153=CARTESIAN_POINT('Ctrl Pts',(-16.1840435203226,-17.3135627916812,
2.15868306686927));
#214154=CARTESIAN_POINT('Ctrl Pts',(-15.9760905434333,-20.2092549046476,
2.2858588735507));
#214155=CARTESIAN_POINT('Ctrl Pts',(-18.2983483154525,-21.9514936229061,
2.41303468023214));
#214156=CARTESIAN_POINT('Ctrl Pts',(-21.020289469658,-20.9418831396066,
2.54021048691357));
#214157=CARTESIAN_POINT('Ctrl Pts',(-21.644701937954,-18.1066783673205,
2.667386293595));
#214158=CARTESIAN_POINT('Ctrl Pts',(-19.598726037039,-16.0470037339522,
2.79456210027644));
#214159=CARTESIAN_POINT('Ctrl Pts',(-16.7594176679228,-16.6524828663812,
2.92173790695787));
#214160=CARTESIAN_POINT('Ctrl Pts',(-15.7316660321737,-19.3676262467993,
3.04891371363931));
#214161=CARTESIAN_POINT('Ctrl Pts',(-17.4583694659978,-21.7014583414031,
3.17608952032074));
#214162=CARTESIAN_POINT('Ctrl Pts',(-20.3553847402323,-21.512833058945,
3.30326532700218));
#214163=CARTESIAN_POINT('Ctrl Pts',(-21.7648801497778,-18.9748023878472,
3.43044113368361));
#214164=CARTESIAN_POINT('Ctrl Pts',(-20.3937311395464,-16.4158519413221,
3.55761694036505));
#214165=CARTESIAN_POINT('Ctrl Pts',(-17.4998818233102,-16.1836599274567,
3.68479274704648));
#214166=CARTESIAN_POINT('Ctrl Pts',(-15.7382593361759,-18.4912481076264,
3.81196855372791));
#214167=CARTESIAN_POINT('Ctrl Pts',(-16.7250429714639,-21.2215475515407,
3.93914436040935));
#214168=CARTESIAN_POINT('Ctrl Pts',(-19.5549199904986,-21.8696779809346,
4.06632016709078));
#214169=CARTESIAN_POINT('Ctrl Pts',(-21.6316538702915,-19.8410199543343,
4.19349597377222));
#214170=CARTESIAN_POINT('Ctrl Pts',(-21.0499701727744,-16.9967412984365,
4.32067178045365));
#214171=CARTESIAN_POINT('Ctrl Pts',(-18.3435275870569,-15.9462911441802,
4.44784758713509));
#214172=CARTESIAN_POINT('Ctrl Pts',(-15.9953192047637,-17.6533923098082,
4.57502339381652));
#214173=CARTESIAN_POINT('Ctrl Pts',(-16.159680470399,-20.5518854305035,
4.70219920049796));
#214174=CARTESIAN_POINT('Ctrl Pts',(-18.6858201241535,-21.9825829688008,
4.82937500717939));
#214175=CARTESIAN_POINT('Ctrl Pts',(-21.2561618236167,-20.632908732416,
4.95655081386082));
#214176=CARTESIAN_POINT('Ctrl Pts',(-21.5125765929291,-17.7411050630016,
5.08372662054225));
#214177=CARTESIAN_POINT('Ctrl Pts',(-19.219819796142,-15.9602223416674,
5.21090242722368));
#214178=CARTESIAN_POINT('Ctrl Pts',(-16.4813534897718,-16.9241099311898,
5.33807823390512));
#214179=CARTESIAN_POINT('Ctrl Pts',(-15.8095505415254,-19.748460793793,
5.46525404058656));
#214180=CARTESIAN_POINT('Ctrl Pts',(-17.8207484596252,-21.8421083120231,
5.59242984726799));
#214181=CARTESIAN_POINT('Ctrl Pts',(-20.6697979832357,-21.2842608343242,
5.71960565394943));
#214182=CARTESIAN_POINT('Ctrl Pts',(-21.7428730064005,-18.5867087975656,
5.84678146063087));
#214183=CARTESIAN_POINT('Ctrl Pts',(-20.0554937979133,-16.2242887665116,
5.9739572673123));
#214184=CARTESIAN_POINT('Ctrl Pts',(-17.1557260509959,-16.3643744913304,
6.10113307399374));
#214185=CARTESIAN_POINT('Ctrl Pts',(-15.7039266935608,-18.8784460142016,
6.22830888067516));
#214186=CARTESIAN_POINT('Ctrl Pts',(-17.0320315272241,-21.4599987537674,
6.3554846873566));
#214187=CARTESIAN_POINT('Ctrl Pts',(-19.9215867985823,-21.7406183007101,
6.48266049403803));
#214188=CARTESIAN_POINT('Ctrl Pts',(-21.7216048921908,-19.4628536379228,
6.60983630071947));
#214189=CARTESIAN_POINT('Ctrl Pts',(-20.7806809288866,-16.7164124694941,
6.73701210740091));
#214190=CARTESIAN_POINT('Ctrl Pts',(-17.9620542446739,-16.0209841040936,
6.86418791408233));
#214191=CARTESIAN_POINT('Ctrl Pts',(-15.8516398786157,-18.0145809038241,
6.99136372076378));
#214192=CARTESIAN_POINT('Ctrl Pts',(-16.3856120244824,-20.868201541505,
7.11853952744521));
#214193=CARTESIAN_POINT('Ctrl Pts',(-19.0740843804904,-21.9638261977359,
7.24571533412664));
#214194=CARTESIAN_POINT('Ctrl Pts',(-21.4505504254156,-20.2962872525602,
7.37289114080807));
#214195=CARTESIAN_POINT('Ctrl Pts',(-21.3347500631569,-17.3954481890373,
7.50006694748951));
#214196=CARTESIAN_POINT('Ctrl Pts',(-18.8329229387055,-15.9226488015715,
7.62724275417095));
#214197=CARTESIAN_POINT('Ctrl Pts',(-16.2403401578418,-17.2290911159235,
7.75441856085238));
#214198=CARTESIAN_POINT('Ctrl Pts',(-15.9355355081732,-20.1161953956302,
7.8815943675338));
#214199=CARTESIAN_POINT('Ctrl Pts',(-18.1981483374604,-21.9352226579616,
8.00877017421523));
#214200=CARTESIAN_POINT('Ctrl Pts',(-20.9523718084226,-21.0173282912935,
8.13594598089668));
#214201=CARTESIAN_POINT('Ctrl Pts',(-21.6713768328398,-18.2046234060944,
8.26312178757812));
#214202=CARTESIAN_POINT('Ctrl Pts',(-19.6955209272938,-16.0775901583807,
8.39029759425955));
#214203=CARTESIAN_POINT('Ctrl Pts',(-16.837529249675,-16.5876495343575,
8.51747340094099));
#214204=CARTESIAN_POINT('Ctrl Pts',(-15.7194317772296,-19.2668537144213,
8.64464920762241));
#214205=CARTESIAN_POINT('Ctrl Pts',(-17.3670135439705,-21.657199153529,
8.77182501430386));
#214206=CARTESIAN_POINT('Ctrl Pts',(-20.2687205393704,-21.5656922728693,
8.89900082098528));
#214207=CARTESIAN_POINT('Ctrl Pts',(-21.7624166953973,-19.07628495589,9.02617662766673));
#214208=CARTESIAN_POINT('Ctrl Pts',(-20.4777284981358,-16.4728539058758,
9.15335243434816));
#214209=CARTESIAN_POINT('Ctrl Pts',(-17.5932776318311,-16.1438855240604,
9.28052824102959));
#214210=CARTESIAN_POINT('Ctrl Pts',(-15.7553687371063,-18.3911878826788,
9.40770404771103));
#214211=CARTESIAN_POINT('Ctrl Pts',(-16.6501691513803,-21.1530005510137,
9.53487985439246));
#214212=CARTESIAN_POINT('Ctrl Pts',(-19.4567550321338,-21.8955318232944,
9.6620556610739));
#214213=CARTESIAN_POINT('Ctrl Pts',(-21.6002580301411,-19.9375553438918,
9.78923146775533));
#214214=CARTESIAN_POINT('Ctrl Pts',(-21.1141471855306,-17.0753930069318,
9.91640727443676));
#214215=CARTESIAN_POINT('Ctrl Pts',(-18.4443990267908,-15.9349011107459,
10.0435830811182));
#214216=CARTESIAN_POINT('Ctrl Pts',(-16.0403417863069,-17.5624101831744,
10.1707588877996));
#214217=CARTESIAN_POINT('Ctrl Pts',(-16.1075487696024,-20.4647816648694,
10.297934694481));
#214218=CARTESIAN_POINT('Ctrl Pts',(-18.5843617408396,-21.9792698628662,
10.4251105011625));
#214219=CARTESIAN_POINT('Ctrl Pts',(-21.1984585272586,-20.7164258552413,
10.5522863078439));
#214220=CARTESIAN_POINT('Ctrl Pts',(-21.5515675764649,-17.8348306380519,
10.6794621145253));
#214221=CARTESIAN_POINT('Ctrl Pts',(-19.319733252231,-15.9781689710992,
10.8066379212068));
#214222=CARTESIAN_POINT('Ctrl Pts',(-16.5505250237807,-16.849812696393,
10.9338137278882));
#214223=CARTESIAN_POINT('Ctrl Pts',(-15.7845195642707,-19.6500827962871,
11.0609895345697));
#214224=CARTESIAN_POINT('Ctrl Pts',(-17.7244793391404,-21.8099052584926,
11.1881653412511));
#214225=CARTESIAN_POINT('Ctrl Pts',(-20.5906116624301,-21.3477770276364,
11.3153411479325));
#214226=CARTESIAN_POINT('Ctrl Pts',(-21.753418019756,-18.6876720726163,
11.442516954614));
#214227=CARTESIAN_POINT('Ctrl Pts',(-20.1460957501734,-16.2700715849292,
11.5696927612954));
#214228=CARTESIAN_POINT('Ctrl Pts',(-17.2432632743535,-16.3129739588191,
11.6968685679768));
#214229=CARTESIAN_POINT('Ctrl Pts',(-15.7080892187581,-18.7770189290635,
11.8240443746583));
#214230=CARTESIAN_POINT('Ctrl Pts',(-16.9490004957481,-21.4015981713421,
11.9512201813397));
#214231=CARTESIAN_POINT('Ctrl Pts',(-19.8275380283252,-21.7788231306235,
12.0783959880211));
#214232=CARTESIAN_POINT('Ctrl Pts',(-21.7028222925386,-19.5626133199888,
12.2055717947026));
#214233=CARTESIAN_POINT('Ctrl Pts',(-20.8543963692405,-16.7862036872011,
12.332747601384));
#214234=CARTESIAN_POINT('Ctrl Pts',(-18.0606383838055,-15.996777746927,
12.4599234080654));
#214235=CARTESIAN_POINT('Ctrl Pts',(-15.8846478876935,-17.9185848020682,
12.5870992147468));
#214236=CARTESIAN_POINT('Ctrl Pts',(-16.3227611038855,-20.7884861603309,
12.7142750214283));
#214237=CARTESIAN_POINT('Ctrl Pts',(-18.9730363488984,-21.9735254516762,
12.8414508281097));
#214238=CARTESIAN_POINT('Ctrl Pts',(-21.404010580066,-20.3865026781285,
12.9686266347912));
#214239=CARTESIAN_POINT('Ctrl Pts',(-21.3854158235693,-17.4834127326752,
13.0958024414726));
#214240=CARTESIAN_POINT('Ctrl Pts',(-18.9343116143732,-15.9276604541869,
13.222978248154));
#214241=CARTESIAN_POINT('Ctrl Pts',(-16.2994339317307,-17.1465519972999,
13.3501540548355));
#214242=CARTESIAN_POINT('Ctrl Pts',(-15.8981195105134,-20.0218300241493,
13.4773298615169));
#214243=CARTESIAN_POINT('Ctrl Pts',(-18.0985494238061,-21.9156054049817,
13.6045056681983));
#214244=CARTESIAN_POINT('Ctrl Pts',(-20.8819658002459,-21.0904567688396,
13.7316814748798));
#214245=CARTESIAN_POINT('Ctrl Pts',(-21.694756872753,-18.3034067748831,
13.8588572815612));
#214246=CARTESIAN_POINT('Ctrl Pts',(-19.7912372798057,-16.1114008087357,
13.9860330882426));
#214247=CARTESIAN_POINT('Ctrl Pts',(-16.9177681021827,-16.5254682931038,
14.1132088949241));
#214248=CARTESIAN_POINT('Ctrl Pts',(-15.7105789627421,-19.1657280110059,
14.2403847016055));
#214249=CARTESIAN_POINT('Ctrl Pts',(-17.2771909703125,-21.6099055442666,
14.367560508287));
#214250=CARTESIAN_POINT('Ctrl Pts',(-20.1803348428554,-21.6156197088857,
14.4947363149684));
#214251=CARTESIAN_POINT('Ctrl Pts',(-21.7565562667429,-19.1776281134862,
14.6219121216498));
#214252=CARTESIAN_POINT('Ctrl Pts',(-20.5597699168931,-16.5326367280233,
14.7490879283312));
#214253=CARTESIAN_POINT('Ctrl Pts',(-17.6879529883551,-16.107260981979,
14.8762637350127));
#214254=CARTESIAN_POINT('Ctrl Pts',(-15.7758192680016,-18.2917567205529,
15.0034395416941));
#214255=CARTESIAN_POINT('Ctrl Pts',(-16.5776327638535,-21.0819846886999,
15.1306153483755));
#214256=CARTESIAN_POINT('Ctrl Pts',(-19.3577793596249,-21.9180839067241,
15.257791155057));
#214257=CARTESIAN_POINT('Ctrl Pts',(-21.5656471090539,-20.0329852362584,
15.3849669617384));
#214258=CARTESIAN_POINT('Ctrl Pts',(-21.1756543877665,-17.1561497050361,
15.5121427684199));
#214259=CARTESIAN_POINT('Ctrl Pts',(-18.545595311866,-15.9268953564031,
15.6393185751013));
#214260=CARTESIAN_POINT('Ctrl Pts',(-16.0883858436145,-17.4729867591009,
15.7664943817827));
#214261=CARTESIAN_POINT('Ctrl Pts',(-16.0583631585132,-20.3759810124089,
15.8936701884641));
#214262=CARTESIAN_POINT('Ctrl Pts',(-18.4830712067246,-21.9725610690611,
16.0208459951456));
#214263=CARTESIAN_POINT('Ctrl Pts',(-21.1379908483687,-20.7979638220132,
16.148021801827));
#214264=CARTESIAN_POINT('Ctrl Pts',(-21.5873980951341,-17.9298093417044,
16.2751976085084));
#214265=CARTESIAN_POINT('Ctrl Pts',(-19.418989691473,-15.9994513460744,
16.4023734151899));
#214266=CARTESIAN_POINT('Ctrl Pts',(-16.6221457611405,-16.7778734845843,
16.5295492218713));
#214267=CARTESIAN_POINT('Ctrl Pts',(-15.7627970185048,-19.550921759478,
16.6567250285528));
#214268=CARTESIAN_POINT('Ctrl Pts',(-17.6293425977359,-21.7744964933273,
16.7839008352342));
#214269=CARTESIAN_POINT('Ctrl Pts',(-20.5093427807734,-21.4086058784384,
16.9110766419156));
#214270=CARTESIAN_POINT('Ctrl Pts',(-21.7605761526514,-18.7889318442388,
17.0382524485971));
#214271=CARTESIAN_POINT('Ctrl Pts',(-20.2351137549734,-16.3188627217991,
17.1654282552785));
#214272=CARTESIAN_POINT('Ctrl Pts',(-17.3324726567343,-16.2645336211774,
17.2926040619599));
#214273=CARTESIAN_POINT('Ctrl Pts',(-15.7156459073444,-18.6757881201507,
17.4197798686414));
#214274=CARTESIAN_POINT('Ctrl Pts',(-16.8679716977821,-21.3404498752418,
17.5469556753228));
#214275=CARTESIAN_POINT('Ctrl Pts',(-19.7322626367279,-21.813857113719,
17.6741314820042));
#214276=CARTESIAN_POINT('Ctrl Pts',(-21.6807095656397,-19.6616880772395,
17.8013072886857));
#214277=CARTESIAN_POINT('Ctrl Pts',(-20.925733361505,-16.8584242781114,
17.9284830953671));
#214278=CARTESIAN_POINT('Ctrl Pts',(-18.1599778324925,-15.9758862618349,
18.0556589020486));
#214279=CARTESIAN_POINT('Ctrl Pts',(-15.9208520143557,-17.8237478819072,
18.18283470873));
#214280=CARTESIAN_POINT('Ctrl Pts',(-16.2626148693509,-20.7067107930414,
18.3100105154114));
#214281=CARTESIAN_POINT('Ctrl Pts',(-18.871720190335,-21.9798354613185,
18.4371863220928));
#214282=CARTESIAN_POINT('Ctrl Pts',(-21.3544757844137,-20.4751090222602,
18.5643621287743));
#214283=CARTESIAN_POINT('Ctrl Pts',(-21.4331074916559,-17.573024590546,
18.6915379354557));
#214284=CARTESIAN_POINT('Ctrl Pts',(-19.0354756002437,-15.9360645072522,
18.8187137421372));
#214285=CARTESIAN_POINT('Ctrl Pts',(-16.3612585583812,-17.0660380501958,
18.9458895488186));
#214286=CARTESIAN_POINT('Ctrl Pts',(-15.8638845181663,-19.926264622792,
19.0730653555));
#214287=CARTESIAN_POINT('Ctrl Pts',(-17.9996632971129,-21.8926638800028,
19.2002411621814));
#214288=CARTESIAN_POINT('Ctrl Pts',(-20.8091504151054,-21.1611865332722,
19.3274169688629));
#214289=CARTESIAN_POINT('Ctrl Pts',(-21.7148158405835,-18.4029176833963,
19.4545927755443));
#214290=CARTESIAN_POINT('Ctrl Pts',(-19.8857677137514,-16.1483977337339,
19.5817685822257));
#214291=CARTESIAN_POINT('Ctrl Pts',(-17.0000442519466,-16.4660089396223,
19.7089443889072));
#214292=CARTESIAN_POINT('Ctrl Pts',(-15.7051174603682,-19.0643624769379,
19.8361201955886));
#214293=CARTESIAN_POINT('Ctrl Pts',(-17.1890026117629,-21.5596307402518,
19.9632960022701));
#214294=CARTESIAN_POINT('Ctrl Pts',(-20.0903265756109,-21.6625590217998,
20.0904718089515));
#214295=CARTESIAN_POINT('Ctrl Pts',(-21.7473058561185,-19.2787188421125,
20.2176476156329));
#214296=CARTESIAN_POINT('Ctrl Pts',(-20.6397625633182,-16.5951320814986,
20.3448234223144));
#214297=CARTESIAN_POINT('Ctrl Pts',(-17.7838032497984,-16.0738298258407,
20.4719992289958));
#214298=CARTESIAN_POINT('Ctrl Pts',(-15.7995849948555,-18.1930614463123,
20.5991750356772));
#214299=CARTESIAN_POINT('Ctrl Pts',(-16.5075209429087,-21.0085886920376,
20.7263508423587));
#214300=CARTESIAN_POINT('Ctrl Pts',(-19.2580928765906,-21.9372914608301,
20.8535266490401));
#214301=CARTESIAN_POINT('Ctrl Pts',(-21.5278813506218,-20.1272362554868,
20.9807024557215));
#214302=CARTESIAN_POINT('Ctrl Pts',(-21.2343815144973,-17.2388559379038,
21.107878262403));
#214303=CARTESIAN_POINT('Ctrl Pts',(-18.647082453596,-15.9224078539418,
21.2350540690844));
#214304=CARTESIAN_POINT('Ctrl Pts',(-16.1392442526231,-17.3849814787741,
21.3622298757658));
#214305=CARTESIAN_POINT('Ctrl Pts',(-16.0124741552623,-20.2860474906393,
21.4894056824473));
#214306=CARTESIAN_POINT('Ctrl Pts',(-18.3814921015747,-21.9615662752975,
21.6165814891287));
#214307=CARTESIAN_POINT('Ctrl Pts',(-21.0759341658266,-20.8791897513666,
21.7437572958101));
#214308=CARTESIAN_POINT('Ctrl Pts',(-21.6178065999207,-18.0222756693125,
21.8709331024916));
#214309=CARTESIAN_POINT('Ctrl Pts',(-20.2210099178527,-16.6964452859245,
21.9557169736125));
#214310=CARTESIAN_POINT('Ctrl Pts',(-19.3965839472885,-16.475840953354,
21.998108909173));
#214311=CARTESIAN_POINT('Ctrl Pts',(-17.1140743056112,-17.5890877707427,
1.73472347597681E-18));
#214312=CARTESIAN_POINT('Ctrl Pts',(-17.0606037558837,-17.6406831599911,
2.50957526619234E-15));
#214313=CARTESIAN_POINT('Ctrl Pts',(-17.0102648206888,-17.6951284552545,
2.0073975135774E-14));
#214314=CARTESIAN_POINT('Ctrl Pts',(-16.9630512610728,-17.7520566525928,
1.3759826611448E-14));
#214315=CARTESIAN_POINT('Ctrl Pts',(-16.9139640310005,-17.811244045856,
7.39579948662126E-15));
#214316=CARTESIAN_POINT('Ctrl Pts',(-16.8682546395764,-17.873115719352,
-2.41757959083345E-14));
#214317=CARTESIAN_POINT('Ctrl Pts',(-16.8259443403958,-17.937308752054,
-1.47035161823794E-14));
#214318=CARTESIAN_POINT('Ctrl Pts',(-16.7856210013394,-17.9984871760508,
-5.6760700422245E-15));
#214319=CARTESIAN_POINT('Ctrl Pts',(-16.7483849217229,-18.061774974692,
4.48760828751193E-15));
#214320=CARTESIAN_POINT('Ctrl Pts',(-16.7142833600929,-18.1268912399334,
-5.97438765126412E-15));
#214321=CARTESIAN_POINT('Ctrl Pts',(-16.6917479443229,-18.1699221757752,
-1.29058387990152E-14));
#214322=CARTESIAN_POINT('Ctrl Pts',(-16.670581955631,-18.2137522504246,
-3.54114788609107E-14));
#214323=CARTESIAN_POINT('Ctrl Pts',(-16.6508067523184,-18.2583061596181,
-7.7715611723761E-15));
#214324=CARTESIAN_POINT('Ctrl Pts',(-16.6447946121616,-18.271851625744,
8.59586006653776E-16));
#214325=CARTESIAN_POINT('Ctrl Pts',(-16.6389106011744,-18.2854654139231,
1.30990802670221E-14));
#214326=CARTESIAN_POINT('Ctrl Pts',(-16.6331633226596,-18.2991259028343,
9.76302372279747E-15));
#214327=CARTESIAN_POINT('Ctrl Pts',(-16.6020274374077,-18.3731316107767,
-9.37108370488806E-15));
#214328=CARTESIAN_POINT('Ctrl Pts',(-16.5748437493431,-18.4486320984917,
-9.72962485609361E-16));
#214329=CARTESIAN_POINT('Ctrl Pts',(-16.5516340690814,-18.5252437971799,
1.88737914186277E-15));
#214330=CARTESIAN_POINT('Ctrl Pts',(-16.5281113691115,-18.602888727317,
4.78629705696217E-15));
#214331=CARTESIAN_POINT('Ctrl Pts',(-16.5086701130808,-18.6816758757728,
8.82622860769151E-15));
#214332=CARTESIAN_POINT('Ctrl Pts',(-16.4933735667248,-18.7612412026621,
7.36910532594948E-15));
#214333=CARTESIAN_POINT('Ctrl Pts',(-16.4780905784557,-18.8407360068606,
5.91327356475586E-15));
#214334=CARTESIAN_POINT('Ctrl Pts',(-16.4669445521086,-18.9210085588168,
-3.76344494961826E-15));
#214335=CARTESIAN_POINT('Ctrl Pts',(-16.4600452985084,-19.001717210151,
-8.72912853111529E-15));
#214336=CARTESIAN_POINT('Ctrl Pts',(-16.458249908906,-19.0227199854994,
-1.00213460937811E-14));
#214337=CARTESIAN_POINT('Ctrl Pts',(-16.4567423723362,-19.0437523637043,
-5.36502461302182E-15));
#214338=CARTESIAN_POINT('Ctrl Pts',(-16.4555251966164,-19.0648084381479,
2.56739074444567E-15));
#214339=CARTESIAN_POINT('Ctrl Pts',(-16.4546316923203,-19.0802652803004,
8.42156714837826E-15));
#214340=CARTESIAN_POINT('Ctrl Pts',(-16.4538946607534,-19.0957348924738,
2.92099871876547E-16));
#214341=CARTESIAN_POINT('Ctrl Pts',(-16.4533151797917,-19.1112149436894,
8.85402862138562E-15));
#214342=CARTESIAN_POINT('Ctrl Pts',(-16.4528674697077,-19.1231749138822,
1.55531854101286E-14));
#214343=CARTESIAN_POINT('Ctrl Pts',(-16.4525139746189,-19.1351378160613,
2.00079667589343E-14));
#214344=CARTESIAN_POINT('Ctrl Pts',(-16.4522551154433,-19.1470940326229,
1.58345558887163E-14));
#214345=CARTESIAN_POINT('Ctrl Pts',(-16.450448336251,-19.23054575209,-1.44011488464872E-14));
#214346=CARTESIAN_POINT('Ctrl Pts',(-16.4532433905666,-19.3137912323742,
-1.21694340773906E-14));
#214347=CARTESIAN_POINT('Ctrl Pts',(-16.4606965224471,-19.3964498394684,
-8.71525074330748E-15));
#214348=CARTESIAN_POINT('Ctrl Pts',(-16.4681353636814,-19.4789499568243,
-5.18520424887126E-15));
#214349=CARTESIAN_POINT('Ctrl Pts',(-16.4802140623254,-19.560866453353,
-1.0737231714089E-14));
#214350=CARTESIAN_POINT('Ctrl Pts',(-16.4970379007565,-19.6418365052423,
5.52335954751015E-15));
#214351=CARTESIAN_POINT('Ctrl Pts',(-16.5134756240274,-19.7209482556099,
2.1146494257637E-14));
#214352=CARTESIAN_POINT('Ctrl Pts',(-16.5344429618587,-19.7991574576156,
2.06622882565801E-14));
#214353=CARTESIAN_POINT('Ctrl Pts',(-16.5596742522225,-19.8762376297952,
9.2148511043888E-15));
#214354=CARTESIAN_POINT('Ctrl Pts',(-16.5700716763688,-19.9080011754509,
4.59487668223206E-15));
#214355=CARTESIAN_POINT('Ctrl Pts',(-16.5811937949009,-19.9395729260017,
-5.73054096894381E-15));
#214356=CARTESIAN_POINT('Ctrl Pts',(-16.593024502045,-19.9709365575929,
9.24260668000443E-15));
#214357=CARTESIAN_POINT('Ctrl Pts',(-16.599575769931,-19.9883042051838,
1.75753077980789E-14));
#214358=CARTESIAN_POINT('Ctrl Pts',(-16.6063465654584,-20.005613174688,
7.16385352924337E-15));
#214359=CARTESIAN_POINT('Ctrl Pts',(-16.6133217610784,-20.0228306160632,
1.08524300657109E-14));
#214360=CARTESIAN_POINT('Ctrl Pts',(-16.6442809363235,-20.0992496606094,
2.7032515933421E-14));
#214361=CARTESIAN_POINT('Ctrl Pts',(-16.6792960167752,-20.1739619594251,
1.93406742481452E-14));
#214362=CARTESIAN_POINT('Ctrl Pts',(-16.7180389842821,-20.246743899253,
5.35682609381638E-15));
#214363=CARTESIAN_POINT('Ctrl Pts',(-16.7588459173261,-20.3234031728317,
-9.3719877284186E-15));
#214364=CARTESIAN_POINT('Ctrl Pts',(-16.803788552284,-20.3979217843379,
-7.52420306717188E-15));
#214365=CARTESIAN_POINT('Ctrl Pts',(-16.8525440995263,-20.4700328123178,
7.57727214306669E-15));
#214366=CARTESIAN_POINT('Ctrl Pts',(-16.9012996467686,-20.5421438402977,
2.26787473533053E-14));
#214367=CARTESIAN_POINT('Ctrl Pts',(-16.9538687049381,-20.6118481705157,
1.06480511332545E-14));
#214368=CARTESIAN_POINT('Ctrl Pts',(-17.009981736112,-20.6788601850433,
-4.9960036108132E-15));
#214369=CARTESIAN_POINT('Ctrl Pts',(-17.0318954596463,-20.7050302694089,
-1.09832900983411E-14));
#214370=CARTESIAN_POINT('Ctrl Pts',(-17.0543502078806,-20.7307894693846,
3.40249426276482E-15));
#214371=CARTESIAN_POINT('Ctrl Pts',(-17.0773318266369,-20.7561195433156,
1.83186799063151E-14));
#214372=CARTESIAN_POINT('Ctrl Pts',(-17.0864635878594,-20.7661844647356,
2.42676587261844E-14));
#214373=CARTESIAN_POINT('Ctrl Pts',(-17.0956793012105,-20.776182428681,
2.64107502889692E-15));
#214374=CARTESIAN_POINT('Ctrl Pts',(-17.1049757714685,-20.7861097474567,
2.08166817117217E-15));
#214375=CARTESIAN_POINT('Ctrl Pts',(-17.1654853800672,-20.8507254733048,
-1.15724079903374E-15));
#214376=CARTESIAN_POINT('Ctrl Pts',(-17.2292147782235,-20.9121401114294,
1.62919071033182E-14));
#214377=CARTESIAN_POINT('Ctrl Pts',(-17.2958558788046,-20.9700792980957,
1.88737914186277E-15));
#214378=CARTESIAN_POINT('Ctrl Pts',(-17.3510487696017,-21.0180651682969,
-1.00426089860209E-14));
#214379=CARTESIAN_POINT('Ctrl Pts',(-17.4082400170084,-21.063667078019,
2.71337193772128E-14));
#214380=CARTESIAN_POINT('Ctrl Pts',(-17.4672777570143,-21.1067151950334,
5.63438184997267E-15));
#214381=CARTESIAN_POINT('Ctrl Pts',(-17.4867746670186,-21.1209316142798,
-1.5378003559757E-15));
#214382=CARTESIAN_POINT('Ctrl Pts',(-17.5064731111025,-21.1348693857667,
3.24666800846887E-14));
#214383=CARTESIAN_POINT('Ctrl Pts',(-17.5263680478785,-21.1485219846966,
2.39808173319034E-14));
#214384=CARTESIAN_POINT('Ctrl Pts',(-17.5422931318004,-21.1594503322534,
1.70518113475176E-14));
#214385=CARTESIAN_POINT('Ctrl Pts',(-17.5583454808324,-21.1701967133747,
2.25387075678082E-14));
#214386=CARTESIAN_POINT('Ctrl Pts',(-17.574506564613,-21.1807476004758,
2.41195952099815E-14));
#214387=CARTESIAN_POINT('Ctrl Pts',(-17.6490343637846,-21.2294036439462,
3.11874514914716E-14));
#214388=CARTESIAN_POINT('Ctrl Pts',(-17.7259442979181,-21.2739559986071,
3.27197442341185E-14));
#214389=CARTESIAN_POINT('Ctrl Pts',(-17.804955500985,-21.3141140597646,
1.57929225252929E-14));
#214390=CARTESIAN_POINT('Ctrl Pts',(-17.8827967354047,-21.3536774752179,
-1.3531531152433E-15));
#214391=CARTESIAN_POINT('Ctrl Pts',(-17.9626781499771,-21.3889764950412,
4.75096733707754E-15));
#214392=CARTESIAN_POINT('Ctrl Pts',(-18.0443636118602,-21.4196958725292,
-4.38538094726937E-15));
#214393=CARTESIAN_POINT('Ctrl Pts',(-18.0530583776972,-21.4229657052236,
-5.14211066895245E-15));
#214394=CARTESIAN_POINT('Ctrl Pts',(-18.0617736083461,-21.4261836096314,
-1.19767995287112E-14));
#214395=CARTESIAN_POINT('Ctrl Pts',(-18.0705088883292,-21.4293497159892,
1.11022302462516E-16));
#214396=CARTESIAN_POINT('Ctrl Pts',(-19.3965839546295,-21.4281590740807,
0.00189110722368242));
#214397=CARTESIAN_POINT('Ctrl Pts',(-20.2210099343281,-21.207554739066,
0.0442830427841606));
#214398=CARTESIAN_POINT('Ctrl Pts',(-21.6178066866466,-19.8817246731204,
0.129066913905116));
#214399=CARTESIAN_POINT('Ctrl Pts',(-21.0759341432978,-17.0248100445211,
0.256242720586551));
#214400=CARTESIAN_POINT('Ctrl Pts',(-18.381492106794,-15.9424338299618,
0.383418527267985));
#214401=CARTESIAN_POINT('Ctrl Pts',(-16.0124741472572,-17.6179524340247,
0.51059433394942));
#214402=CARTESIAN_POINT('Ctrl Pts',(-16.1392442377966,-20.5190185688902,
0.637770140630853));
#214403=CARTESIAN_POINT('Ctrl Pts',(-18.6470824574045,-21.9815921336574,
0.764945947312289));
#214404=CARTESIAN_POINT('Ctrl Pts',(-21.2343815212355,-20.6651440828081,
0.892121753993721));
#214405=CARTESIAN_POINT('Ctrl Pts',(-21.5278813636115,-17.7767637319101,
1.01929756067515));
#214406=CARTESIAN_POINT('Ctrl Pts',(-19.2580928773362,-15.966708532015,
1.14647336735659));
#214407=CARTESIAN_POINT('Ctrl Pts',(-16.5075209349949,-16.8954112973593,
1.27364917403802));
#214408=CARTESIAN_POINT('Ctrl Pts',(-15.7995849828837,-19.7109385580857,
1.40082498071946));
#214409=CARTESIAN_POINT('Ctrl Pts',(-17.7838032463622,-21.8301701846349,
1.52800078740089));
#214410=CARTESIAN_POINT('Ctrl Pts',(-20.6397625706149,-21.308867928169,
1.65517659408233));
#214411=CARTESIAN_POINT('Ctrl Pts',(-21.7473058680116,-18.6252811563658,
1.78235240076376));
#214412=CARTESIAN_POINT('Ctrl Pts',(-20.0903265808676,-16.2414409677205,
1.9095282074452));
#214413=CARTESIAN_POINT('Ctrl Pts',(-17.1890026057441,-16.3443692494651,
2.03670401412663));
#214414=CARTESIAN_POINT('Ctrl Pts',(-15.7051174484919,-18.839637522662,
2.16387982080806));
#214415=CARTESIAN_POINT('Ctrl Pts',(-17.000044245167,-21.4379910700896,
2.2910556274895));
#214416=CARTESIAN_POINT('Ctrl Pts',(-19.8857677182557,-21.7556022772552,
2.41823143417093));
#214417=CARTESIAN_POINT('Ctrl Pts',(-21.7148158522574,-19.5010823187472,
2.54540724085237));
#214418=CARTESIAN_POINT('Ctrl Pts',(-20.8091504232289,-16.7428134580815,
2.6725830475338));
#214419=CARTESIAN_POINT('Ctrl Pts',(-17.9996632942386,-16.0113361084815,
2.79975885421524));
#214420=CARTESIAN_POINT('Ctrl Pts',(-15.8638845069282,-17.9777353733943,
2.92693466089667));
#214421=CARTESIAN_POINT('Ctrl Pts',(-16.3612585490912,-20.837961957188,
3.0541104675781));
#214422=CARTESIAN_POINT('Ctrl Pts',(-19.035475601424,-21.9679355045566,
3.18128627425954));
#214423=CARTESIAN_POINT('Ctrl Pts',(-21.433107502224,-20.3309754148531,
3.30846208094097));
#214424=CARTESIAN_POINT('Ctrl Pts',(-21.354475794674,-17.4288909717763,
3.43563788762241));
#214425=CARTESIAN_POINT('Ctrl Pts',(-18.8717201908742,-15.9241645268262,
3.56281369430384));
#214426=CARTESIAN_POINT('Ctrl Pts',(-16.2626148596744,-17.1972892000883,
3.68998950098528));
#214427=CARTESIAN_POINT('Ctrl Pts',(-15.920852003341,-20.0802521225103,
3.8171653076667));
#214428=CARTESIAN_POINT('Ctrl Pts',(-18.1599778302449,-21.9281137498178,
3.94434111434815));
#214429=CARTESIAN_POINT('Ctrl Pts',(-20.9257333700864,-21.0455757300857,
4.07151692102957));
#214430=CARTESIAN_POINT('Ctrl Pts',(-21.6807095771773,-18.2423119199819,
4.19869272771102));
#214431=CARTESIAN_POINT('Ctrl Pts',(-19.7322626406367,-16.0901428750757,
4.32586853439245));
#214432=CARTESIAN_POINT('Ctrl Pts',(-16.867971690476,-16.5635501154064,
4.45304434107388));
#214433=CARTESIAN_POINT('Ctrl Pts',(-15.7156458955263,-19.2282118809307,
4.58022014775532));
#214434=CARTESIAN_POINT('Ctrl Pts',(-17.3324726512467,-21.639466389345,
4.70739595443675));
#214435=CARTESIAN_POINT('Ctrl Pts',(-20.2351137608509,-21.5851372885107,
4.83457176111819));
#214436=CARTESIAN_POINT('Ctrl Pts',(-21.7605761645016,-19.1150681563998,
4.96174756779962));
#214437=CARTESIAN_POINT('Ctrl Pts',(-20.5093427877246,-16.4953941119431,
5.08892337448106));
#214438=CARTESIAN_POINT('Ctrl Pts',(-17.6293425934107,-16.1295034956214,
5.21609918116249));
#214439=CARTESIAN_POINT('Ctrl Pts',(-15.7627970068714,-18.353078238177,
5.34327498784392));
#214440=CARTESIAN_POINT('Ctrl Pts',(-16.6221457528718,-21.1261265239282,
5.47045079452535));
#214441=CARTESIAN_POINT('Ctrl Pts',(-19.418989694155,-21.904548665486,5.5976266012068));
#214442=CARTESIAN_POINT('Ctrl Pts',(-21.5873981063063,-19.974190662298,
5.72480240788822));
#214443=CARTESIAN_POINT('Ctrl Pts',(-21.1379908577814,-17.1060361707592,
5.85197821456966));
#214444=CARTESIAN_POINT('Ctrl Pts',(-18.4830712057421,-15.9314389191122,
5.97915402125109));
#214445=CARTESIAN_POINT('Ctrl Pts',(-16.0583631480371,-17.5280189820156,
6.10632982793253));
#214446=CARTESIAN_POINT('Ctrl Pts',(-16.0883858332559,-20.43101324669,6.23350563461397));
#214447=CARTESIAN_POINT('Ctrl Pts',(-18.5455953111282,-21.9771046554414,
6.3606814412954));
#214448=CARTESIAN_POINT('Ctrl Pts',(-21.1756543973266,-20.7478503019954,
6.48785724797683));
#214449=CARTESIAN_POINT('Ctrl Pts',(-21.5656471201409,-17.8710147595092,
6.61503305465826));
#214450=CARTESIAN_POINT('Ctrl Pts',(-19.3577793620672,-15.9859160816625,
6.74220886133971));
#214451=CARTESIAN_POINT('Ctrl Pts',(-16.5776327554104,-16.8220153029603,
6.86938466802113));
#214452=CARTESIAN_POINT('Ctrl Pts',(-15.7758192564191,-19.6122432820323,
6.99656047470258));
#214453=CARTESIAN_POINT('Ctrl Pts',(-17.6879529842593,-21.7967390291592,
7.123736281384));
#214454=CARTESIAN_POINT('Ctrl Pts',(-20.5597699240417,-21.3713632814495,
7.25091208806544));
#214455=CARTESIAN_POINT('Ctrl Pts',(-21.7565562785773,-18.7263718856303,
7.37808789474687));
#214456=CARTESIAN_POINT('Ctrl Pts',(-20.1803348485183,-16.2883802806852,
7.50526370142831));
#214457=CARTESIAN_POINT('Ctrl Pts',(-17.2771909646086,-16.2940944453266,
7.63243950810973));
#214458=CARTESIAN_POINT('Ctrl Pts',(-15.7105789509042,-18.7382719881573,
7.75961531479118));
#214459=CARTESIAN_POINT('Ctrl Pts',(-16.9177680950714,-21.3785317163971,
7.8867911214726));
#214460=CARTESIAN_POINT('Ctrl Pts',(-19.7912372839452,-21.7925992023863,
8.01396692815404));
#214461=CARTESIAN_POINT('Ctrl Pts',(-21.6947568843456,-19.6005932276563,
8.14114273483548));
#214462=CARTESIAN_POINT('Ctrl Pts',(-20.8819658086561,-16.8135432227874,
8.26831854151691));
#214463=CARTESIAN_POINT('Ctrl Pts',(-18.098549421318,-15.9883945834145,
8.39549434819835));
#214464=CARTESIAN_POINT('Ctrl Pts',(-15.8981194994098,-17.8821699716618,
8.52267015487978));
#214465=CARTESIAN_POINT('Ctrl Pts',(-16.2994339221984,-20.7574480097692,
8.64984596156122));
#214466=CARTESIAN_POINT('Ctrl Pts',(-18.9343116151575,-21.9763395576547,
8.77702176824265));
#214467=CARTESIAN_POINT('Ctrl Pts',(-21.3854158339506,-20.4205872730748,
8.90419757492408));
#214468=CARTESIAN_POINT('Ctrl Pts',(-21.4040105905201,-17.5174973162549,
9.03137338160553));
#214469=CARTESIAN_POINT('Ctrl Pts',(-18.9730363498343,-15.9304745364933,
9.15854918828694));
#214470=CARTESIAN_POINT('Ctrl Pts',(-16.3227610944446,-17.1155138324785,
9.28572499496839));
#214471=CARTESIAN_POINT('Ctrl Pts',(-15.884647876537,-19.985415201978,9.41290080164982));
#214472=CARTESIAN_POINT('Ctrl Pts',(-18.060638381169,-21.9072222646439,
9.54007660833126));
#214473=CARTESIAN_POINT('Ctrl Pts',(-20.8543963775427,-21.1177963212788,
9.66725241501268));
#214474=CARTESIAN_POINT('Ctrl Pts',(-21.7028223041627,-18.3413866776205,
9.79442822169412));
#214475=CARTESIAN_POINT('Ctrl Pts',(-19.8275380326068,-16.1251768583083,
9.92160402837557));
#214476=CARTESIAN_POINT('Ctrl Pts',(-16.949000488759,-16.5024018190668,
10.048779835057));
#214477=CARTESIAN_POINT('Ctrl Pts',(-15.7080892069104,-19.1269810716216,
10.1759556417385));
#214478=CARTESIAN_POINT('Ctrl Pts',(-17.2432632685167,-21.5910260515137,
10.3031314484199));
#214479=CARTESIAN_POINT('Ctrl Pts',(-20.1460957557023,-21.6339284255716,
10.4303072551013));
#214480=CARTESIAN_POINT('Ctrl Pts',(-21.7534180315782,-19.2163279284187,
10.5574830617828));
#214481=CARTESIAN_POINT('Ctrl Pts',(-20.5906116696995,-16.5562229629832,
10.6846588684642));
#214482=CARTESIAN_POINT('Ctrl Pts',(-17.7244793351877,-16.0940947303175,
10.8118346751456));
#214483=CARTESIAN_POINT('Ctrl Pts',(-15.7845195527222,-18.2539172009796,
10.9390104818271));
#214484=CARTESIAN_POINT('Ctrl Pts',(-16.5505250152316,-21.0541873118379,
11.0661862885085));
#214485=CARTESIAN_POINT('Ctrl Pts',(-19.3197332545243,-21.9258310405445,
11.1933620951899));
#214486=CARTESIAN_POINT('Ctrl Pts',(-21.5515675874969,-20.0691693663223,
11.3205379018714));
#214487=CARTESIAN_POINT('Ctrl Pts',(-21.1984585369079,-17.1875741378502,
11.4477137085528));
#214488=CARTESIAN_POINT('Ctrl Pts',(-18.5843617402537,-15.9247301252809,
11.5748895152342));
#214489=CARTESIAN_POINT('Ctrl Pts',(-16.1075487593188,-17.4392183292074,
11.7020653219157));
#214490=CARTESIAN_POINT('Ctrl Pts',(-16.04034177576,-20.3415898222665,11.8292411285971));
#214491=CARTESIAN_POINT('Ctrl Pts',(-18.4443990256569,-21.9690989010672,
11.9564169352785));
#214492=CARTESIAN_POINT('Ctrl Pts',(-21.1141471948498,-20.828607000416,
12.08359274196));
#214493=CARTESIAN_POINT('Ctrl Pts',(-21.6002580413636,-17.9664446522494,
12.2107685486414));
#214494=CARTESIAN_POINT('Ctrl Pts',(-19.4567550349637,-16.0084681651805,
12.3379443553228));
#214495=CARTESIAN_POINT('Ctrl Pts',(-16.6501691432213,-16.7509994403685,
12.4651201620043));
#214496=CARTESIAN_POINT('Ctrl Pts',(-15.7553687254437,-19.512812119517,
12.5922959686857));
#214497=CARTESIAN_POINT('Ctrl Pts',(-17.5932776273647,-21.7601144869345,
12.7194717753671));
#214498=CARTESIAN_POINT('Ctrl Pts',(-20.4777285049632,-21.431146103831,
12.8466475820486));
#214499=CARTESIAN_POINT('Ctrl Pts',(-21.7624167072548,-18.8277150436234,
12.97382338873));
#214500=CARTESIAN_POINT('Ctrl Pts',(-20.2687205453794,-16.3383077168971,
13.1009991954114));
#214501=CARTESIAN_POINT('Ctrl Pts',(-17.3670135386182,-16.2468008358791,
13.2281750020929));
#214502=CARTESIAN_POINT('Ctrl Pts',(-15.7194317654263,-18.6371462843459,
13.3553508087743));
#214503=CARTESIAN_POINT('Ctrl Pts',(-16.8375292422496,-21.3163504748999,
13.4825266154557));
#214504=CARTESIAN_POINT('Ctrl Pts',(-19.6955209310585,-21.8264098528738,
13.6097024221372));
#214505=CARTESIAN_POINT('Ctrl Pts',(-21.6713768443407,-19.699376596832,
13.7368782288186));
#214506=CARTESIAN_POINT('Ctrl Pts',(-20.9523718171085,-16.8866717006199,
13.8640540355001));
#214507=CARTESIAN_POINT('Ctrl Pts',(-18.1981483353624,-15.9687773303578,
13.9912298421815));
#214508=CARTESIAN_POINT('Ctrl Pts',(-15.9355354972161,-17.7878045998115,
14.1184056488629));
#214509=CARTESIAN_POINT('Ctrl Pts',(-16.240340148078,-20.6749088908223,
14.2455814555443));
#214510=CARTESIAN_POINT('Ctrl Pts',(-18.8329229390928,-21.9813512102896,
14.3727572622258));
#214511=CARTESIAN_POINT('Ctrl Pts',(-21.3347500733399,-20.5085518170573,
14.4999330689072));
#214512=CARTESIAN_POINT('Ctrl Pts',(-21.450550436052,-17.6077127421763,
14.6271088755887));
#214513=CARTESIAN_POINT('Ctrl Pts',(-19.0740843818219,-15.9401737904716,
14.7542846822701));
#214514=CARTESIAN_POINT('Ctrl Pts',(-16.3856120152874,-17.0357984509923,
14.8814604889515));
#214515=CARTESIAN_POINT('Ctrl Pts',(-15.85163986733,-19.8894190998463,15.008636295633));
#214516=CARTESIAN_POINT('Ctrl Pts',(-17.9620542416513,-21.8830159073825,
15.1358121023144));
#214517=CARTESIAN_POINT('Ctrl Pts',(-20.7806809369003,-21.1875875392591,
15.2629879089958));
#214518=CARTESIAN_POINT('Ctrl Pts',(-21.7216049038886,-18.441146360077,
15.3901637156773));
#214519=CARTESIAN_POINT('Ctrl Pts',(-19.9215868032322,-16.1633816883713,
15.5173395223587));
#214520=CARTESIAN_POINT('Ctrl Pts',(-17.0320315205603,-16.4440012364127,
15.6445153290401));
#214521=CARTESIAN_POINT('Ctrl Pts',(-15.7039266816969,-19.0255539860864,
15.7716911357216));
#214522=CARTESIAN_POINT('Ctrl Pts',(-17.1557260448163,-21.5396255188012,
15.898866942403));
#214523=CARTESIAN_POINT('Ctrl Pts',(-20.0554938030875,-21.6797112441684,
16.0260427490844));
#214524=CARTESIAN_POINT('Ctrl Pts',(-21.7428730181815,-19.3172912038646,
16.1532185557659));
#214525=CARTESIAN_POINT('Ctrl Pts',(-20.6697979908152,-16.6197391565441,
16.2803943624473));
#214526=CARTESIAN_POINT('Ctrl Pts',(-17.8207484560495,-16.0618916766609,
16.4075701691287));
#214527=CARTESIAN_POINT('Ctrl Pts',(-15.8095505300749,-18.1555392030885,
16.5347459758102));
#214528=CARTESIAN_POINT('Ctrl Pts',(-16.4813534809519,-20.9798900767501,
16.6619217824916));
#214529=CARTESIAN_POINT('Ctrl Pts',(-19.2198197980441,-21.9437776700467,
16.789097589173));
#214530=CARTESIAN_POINT('Ctrl Pts',(-21.5125766038083,-20.1628949417396,
16.9162733958545));
#214531=CARTESIAN_POINT('Ctrl Pts',(-21.2561618334919,-17.2710912610025,
17.0434492025359));
#214532=CARTESIAN_POINT('Ctrl Pts',(-18.6858201239648,-15.9214170193332,
17.1706250092173));
#214533=CARTESIAN_POINT('Ctrl Pts',(-16.1596804603196,-17.3521145632324,
17.2978008158988));
#214534=CARTESIAN_POINT('Ctrl Pts',(-15.9953191940406,-20.2506076952764,
17.4249766225802));
#214535=CARTESIAN_POINT('Ctrl Pts',(-18.3435275855282,-21.9577088675884,
17.5521524292616));
#214536=CARTESIAN_POINT('Ctrl Pts',(-21.0499701818423,-20.9072587092191,
17.6793282359431));
#214537=CARTESIAN_POINT('Ctrl Pts',(-21.631653881637,-18.0629800421848,
17.8065040426245));
#214538=CARTESIAN_POINT('Ctrl Pts',(-19.5549199937129,-16.0343220076414,
17.933679849306));
#214539=CARTESIAN_POINT('Ctrl Pts',(-16.725042963598,-16.6824524395731,
18.0608556559873));
#214540=CARTESIAN_POINT('Ctrl Pts',(-15.7382593244464,-19.4127518941776,
18.1880314626688));
#214541=CARTESIAN_POINT('Ctrl Pts',(-17.4998818184781,-21.7203400833824,
18.3152072693502));
#214542=CARTESIAN_POINT('Ctrl Pts',(-20.3937311460449,-21.4881480686078,
18.4423830760317));
#214543=CARTESIAN_POINT('Ctrl Pts',(-21.7648801616449,-18.9291976120636,
18.5695588827131));
#214544=CARTESIAN_POINT('Ctrl Pts',(-20.3553847465806,-16.3911669310282,
18.6967346893946));
#214545=CARTESIAN_POINT('Ctrl Pts',(-17.4583694610031,-16.2025416478318,
18.823910496076));
#214546=CARTESIAN_POINT('Ctrl Pts',(-15.7316660204183,-18.5363737515732,
18.9510863027574));
#214547=CARTESIAN_POINT('Ctrl Pts',(-16.7594176601915,-21.2515171426226,
19.0782621094388));
#214548=CARTESIAN_POINT('Ctrl Pts',(-19.5987260404249,-21.8569962774213,
19.2054379161203));
#214549=CARTESIAN_POINT('Ctrl Pts',(-21.6447019493503,-19.7973216359904,
19.3326137228017));
#214550=CARTESIAN_POINT('Ctrl Pts',(-21.0202894786101,-16.9621168526002,
19.4597895294832));
#214551=CARTESIAN_POINT('Ctrl Pts',(-18.2983483137461,-15.9525063653534,
19.5869653361646));
#214552=CARTESIAN_POINT('Ctrl Pts',(-15.9760905326363,-17.6947450904228,
19.714141142846));
#214553=CARTESIAN_POINT('Ctrl Pts',(-16.184043510336,-20.5904372147467,
19.8413169495275));
#214554=CARTESIAN_POINT('Ctrl Pts',(-18.7314233036429,-21.9829647838468,
19.9684927562089));
#214555=CARTESIAN_POINT('Ctrl Pts',(-21.2811670472796,-20.5947704862204,
20.0956685628903));
#214556=CARTESIAN_POINT('Ctrl Pts',(-21.49404313672,-17.6994358448221,20.2228443695718));
#214557=CARTESIAN_POINT('Ctrl Pts',(-19.1747509237061,-15.9532518137242,
20.3500201762532));
#214558=CARTESIAN_POINT('Ctrl Pts',(-16.4510971561478,-16.9582316928714,
20.4771959829346));
#214559=CARTESIAN_POINT('Ctrl Pts',(-15.8218649356901,-19.7923729967134,
20.6043717896161));
#214560=CARTESIAN_POINT('Ctrl Pts',(-17.8643361189216,-21.8555189367891,
20.7315475962975));
#214561=CARTESIAN_POINT('Ctrl Pts',(-20.704669493102,-21.2548766742021,
20.8587234029789));
#214562=CARTESIAN_POINT('Ctrl Pts',(-21.7370367735022,-18.5414683255483,
20.9858992096604));
#214563=CARTESIAN_POINT('Ctrl Pts',(-20.0143025609789,-16.2047352065647,
21.1130750163418));
#214564=CARTESIAN_POINT('Ctrl Pts',(-17.1169733783673,-16.3883740006192,
21.2402508230232));
#214565=CARTESIAN_POINT('Ctrl Pts',(-15.7031596587772,-18.9241212228848,
21.3674266297047));
#214566=CARTESIAN_POINT('Ctrl Pts',(-17.0699655881192,-21.4851744179203,
21.4946024363861));
#214567=CARTESIAN_POINT('Ctrl Pts',(-19.963397156019,-21.7227196345909,
21.6217782430676));
#214568=CARTESIAN_POINT('Ctrl Pts',(-21.7289768951727,-19.4172948235399,
21.748954049749));
#214569=CARTESIAN_POINT('Ctrl Pts',(-20.7467658607354,-16.6869340105708,
21.8761298564304));
#214570=CARTESIAN_POINT('Ctrl Pts',(-17.9181415113151,-16.0308544058051,
22.0033056631118));
#214571=CARTESIAN_POINT('Ctrl Pts',(-15.8372814923396,-18.0626244799711,
22.1305001261329));
#214572=CARTESIAN_POINT('Ctrl Pts',(-16.2233207480177,-19.9500078885456,
22.2153026535935));
#214573=CARTESIAN_POINT('Ctrl Pts',(-16.7733104792501,-20.6030838137515,
22.2577132454937));
#214574=CARTESIAN_POINT('Ctrl Pts',(-19.3578031896578,-21.2832305070458,
-0.084727284346428));
#214575=CARTESIAN_POINT('Ctrl Pts',(-20.1339758575579,-21.0755380525683,
-0.0423353487859499));
#214576=CARTESIAN_POINT('Ctrl Pts',(-21.4490186733577,-19.8273082723234,
0.0424485223350063));
#214577=CARTESIAN_POINT('Ctrl Pts',(-20.9388617059771,-17.1376076759719,
0.169624329016441));
#214578=CARTESIAN_POINT('Ctrl Pts',(-18.4021242480669,-16.1185824938283,
0.296800135697875));
#214579=CARTESIAN_POINT('Ctrl Pts',(-16.1717639304198,-17.6960336866052,
0.42397594237931));
#214580=CARTESIAN_POINT('Ctrl Pts',(-16.2911142199628,-20.4273016198123,
0.551151749060743));
#214581=CARTESIAN_POINT('Ctrl Pts',(-18.6521697052435,-21.8042713584183,
0.678327555742179));
#214582=CARTESIAN_POINT('Ctrl Pts',(-21.0880352243816,-20.5648744678046,
0.805503362423611));
#214583=CARTESIAN_POINT('Ctrl Pts',(-21.3643566423075,-17.8455498248734,
0.932679169105048));
#214584=CARTESIAN_POINT('Ctrl Pts',(-19.2274179378702,-16.1414364076047,
1.05985497578648));
#214585=CARTESIAN_POINT('Ctrl Pts',(-16.6378358343089,-17.0157825839918,
1.18703078246792));
#214586=CARTESIAN_POINT('Ctrl Pts',(-15.9713350808349,-19.6665181980038,
1.31420658914935));
#214587=CARTESIAN_POINT('Ctrl Pts',(-17.8394178695693,-21.6617120734788,
1.44138239583079));
#214588=CARTESIAN_POINT('Ctrl Pts',(-20.5282190751429,-21.1709214225929,
1.56855820251222));
#214589=CARTESIAN_POINT('Ctrl Pts',(-21.5709383211686,-18.6444038752278,
1.69573400919365));
#214590=CARTESIAN_POINT('Ctrl Pts',(-20.0109413467548,-16.4000888674147,
1.82290981587509));
#214591=CARTESIAN_POINT('Ctrl Pts',(-17.2794306645736,-16.4969927993764,
1.95008562255652));
#214592=CARTESIAN_POINT('Ctrl Pts',(-15.882396692181,-18.8462140520133,
2.07726142923796));
#214593=CARTESIAN_POINT('Ctrl Pts',(-17.1015319587312,-21.2924870403926,
2.20443723591939));
#214594=CARTESIAN_POINT('Ctrl Pts',(-19.8183552298129,-21.5915085948938,
2.33161304260083));
#214595=CARTESIAN_POINT('Ctrl Pts',(-21.5403499326061,-19.4689447576054,
2.45878884928226));
#214596=CARTESIAN_POINT('Ctrl Pts',(-20.6876927267632,-16.8721162331674,
2.5859646559637));
#214597=CARTESIAN_POINT('Ctrl Pts',(-18.0426437180737,-16.1834519504684,
2.71314046264513));
#214598=CARTESIAN_POINT('Ctrl Pts',(-16.0318711803166,-18.0347586792573,
2.84031626932657));
#214599=CARTESIAN_POINT('Ctrl Pts',(-16.5001341253916,-20.7275773834348,
2.967492076008));
#214600=CARTESIAN_POINT('Ctrl Pts',(-19.0178303590937,-21.7914140461736,
3.09466788268943));
#214601=CARTESIAN_POINT('Ctrl Pts',(-21.2751298558503,-20.2502645538495,
3.22184368937087));
#214602=CARTESIAN_POINT('Ctrl Pts',(-21.201100429639,-17.5180379135899,
3.3490194960523));
#214603=CARTESIAN_POINT('Ctrl Pts',(-18.8636594850319,-16.1013824854533,
3.47619530273374));
#214604=CARTESIAN_POINT('Ctrl Pts',(-16.40726401034,-17.2999916978614,3.60337110941517));
#214605=CARTESIAN_POINT('Ctrl Pts',(-16.0855043927131,-20.0142159921659,
3.73054691609661));
#214606=CARTESIAN_POINT('Ctrl Pts',(-18.1935751105569,-21.7539230422786,
3.85772272277804));
#214607=CARTESIAN_POINT('Ctrl Pts',(-20.7974521219332,-20.9230396080263,
3.98489852945948));
#214608=CARTESIAN_POINT('Ctrl Pts',(-21.5082398837079,-18.2838496699412,
4.11207433614091));
#214609=CARTESIAN_POINT('Ctrl Pts',(-19.6738347409324,-16.2576461895902,
4.23925014282234));
#214610=CARTESIAN_POINT('Ctrl Pts',(-16.9771895560713,-16.703345099837,
4.36642594950377));
#214611=CARTESIAN_POINT('Ctrl Pts',(-15.8923089135627,-19.2120453137177,
4.49360175618521));
#214612=CARTESIAN_POINT('Ctrl Pts',(-17.4145034676192,-21.482170092496,
4.62077756286664));
#214613=CARTESIAN_POINT('Ctrl Pts',(-20.1472541929444,-21.4310208514753,
4.74795336954808));
#214614=CARTESIAN_POINT('Ctrl Pts',(-21.5834319126906,-19.1055238446132,
4.87512917622951));
#214615=CARTESIAN_POINT('Ctrl Pts',(-20.4054327082334,-16.6391782390827,
5.00230498291095));
#214616=CARTESIAN_POINT('Ctrl Pts',(-17.6939977347856,-16.2947030492859,
5.12948078959238));
#214617=CARTESIAN_POINT('Ctrl Pts',(-15.9367002898516,-18.3881328813199,
5.25665659627382));
#214618=CARTESIAN_POINT('Ctrl Pts',(-16.7457517089779,-20.9988757972025,
5.38383240295525));
#214619=CARTESIAN_POINT('Ctrl Pts',(-19.3788975305108,-21.7317372125915,
5.51100820963669));
#214620=CARTESIAN_POINT('Ctrl Pts',(-21.4203898946547,-19.914362265377,
5.63818401631812));
#214621=CARTESIAN_POINT('Ctrl Pts',(-20.9972862666143,-17.2140796706178,
5.76535982299955));
#214622=CARTESIAN_POINT('Ctrl Pts',(-18.4977579643435,-16.1082311105657,
5.89253562968099));
#214623=CARTESIAN_POINT('Ctrl Pts',(-16.2149670669532,-17.6113640023665,
6.01971143636243));
#214624=CARTESIAN_POINT('Ctrl Pts',(-16.2432325368166,-20.3444472127417,
6.14688724304385));
#214625=CARTESIAN_POINT('Ctrl Pts',(-18.5566225596869,-21.8000465304473,
6.2740630497253));
#214626=CARTESIAN_POINT('Ctrl Pts',(-21.0327453747589,-20.6427399261711,
6.40123885640672));
#214627=CARTESIAN_POINT('Ctrl Pts',(-21.3999119847184,-17.9342843787876,
6.52841466308816));
#214628=CARTESIAN_POINT('Ctrl Pts',(-19.3212698138575,-16.1595197473112,
6.6555904697696));
#214629=CARTESIAN_POINT('Ctrl Pts',(-16.7038440388577,-16.9466824268052,
6.78276627645102));
#214630=CARTESIAN_POINT('Ctrl Pts',(-15.9489603525162,-19.57359951566,6.90994208313247));
#214631=CARTESIAN_POINT('Ctrl Pts',(-17.7491776836857,-21.6302376297137,
7.03711788981389));
#214632=CARTESIAN_POINT('Ctrl Pts',(-20.452908365107,-21.2297589486797,
7.16429369649533));
#214633=CARTESIAN_POINT('Ctrl Pts',(-21.5796473090278,-18.7395778058964,
7.29146950317678));
#214634=CARTESIAN_POINT('Ctrl Pts',(-20.0956814677067,-16.4442808417949,
7.41864530985819));
#214635=CARTESIAN_POINT('Ctrl Pts',(-17.3624573952481,-16.4496605587419,
7.54582111653964));
#214636=CARTESIAN_POINT('Ctrl Pts',(-15.8875385351148,-18.7507814003416,
7.67299692322106));
#214637=CARTESIAN_POINT('Ctrl Pts',(-17.0240713976901,-21.236507818093,
7.80017272990251));
#214638=CARTESIAN_POINT('Ctrl Pts',(-19.7293576227465,-21.6263401052905,
7.92734853658393));
#214639=CARTESIAN_POINT('Ctrl Pts',(-21.5214650077943,-19.5626313341509,
8.05452434326538));
#214640=CARTESIAN_POINT('Ctrl Pts',(-20.756246257781,-16.9387062139828,
8.1817001499468));
#214641=CARTESIAN_POINT('Ctrl Pts',(-18.1357420810118,-16.1618531833802,
8.30887595662825));
#214642=CARTESIAN_POINT('Ctrl Pts',(-16.06410241284,-17.9447866809843,8.43605176330966));
#214643=CARTESIAN_POINT('Ctrl Pts',(-16.4419280683544,-20.6517758840763,
8.56322756999113));
#214644=CARTESIAN_POINT('Ctrl Pts',(-18.9225874591253,-21.7993262135178,
8.69040337667253));
#214645=CARTESIAN_POINT('Ctrl Pts',(-21.2302295612066,-20.3346314670524,
8.81757918335399));
#214646=CARTESIAN_POINT('Ctrl Pts',(-21.2477359743606,-17.6014581653534,
8.94475499003541));
#214647=CARTESIAN_POINT('Ctrl Pts',(-18.9590456510891,-16.1073231728629,
9.07193079671685));
#214648=CARTESIAN_POINT('Ctrl Pts',(-16.4638899108517,-17.2230026087143,
9.19910660339829));
#214649=CARTESIAN_POINT('Ctrl Pts',(-16.0514192784853,-19.9249298373897,
9.32628241007971));
#214650=CARTESIAN_POINT('Ctrl Pts',(-18.1000499583713,-21.7342543270959,
9.45345821676116));
#214651=CARTESIAN_POINT('Ctrl Pts',(-20.7302904540745,-20.9910331578707,
9.58063402344258));
#214652=CARTESIAN_POINT('Ctrl Pts',(-21.5290583619236,-18.3771256229697,
9.70780983012403));
#214653=CARTESIAN_POINT('Ctrl Pts',(-19.7635337035947,-16.2906296482662,
9.83498563680544));
#214654=CARTESIAN_POINT('Ctrl Pts',(-17.0534757722859,-16.6457757880052,
9.9621614434869));
#214655=CARTESIAN_POINT('Ctrl Pts',(-15.8851945148077,-19.1167395018316,
10.0893372501683));
#214656=CARTESIAN_POINT('Ctrl Pts',(-17.3305154731838,-21.4365649476141,
10.2165130568498));
#214657=CARTESIAN_POINT('Ctrl Pts',(-20.0634463748397,-21.4769562634529,
10.3436888635312));
#214658=CARTESIAN_POINT('Ctrl Pts',(-21.5766927423282,-19.2008569240337,
10.4708646702126));
#214659=CARTESIAN_POINT('Ctrl Pts',(-20.4819449561405,-16.6964468026162,
10.598040476894));
#214660=CARTESIAN_POINT('Ctrl Pts',(-17.7835661623932,-16.2613667443784,
10.7252162835755));
#214661=CARTESIAN_POINT('Ctrl Pts',(-15.9571514240733,-18.2947756986395,
10.8523920902569));
#214662=CARTESIAN_POINT('Ctrl Pts',(-16.678322903506,-20.9311471574582,
10.9795678969384));
#214663=CARTESIAN_POINT('Ctrl Pts',(-19.2854505292619,-21.7517739390354,
11.1067437036198));
#214664=CARTESIAN_POINT('Ctrl Pts',(-21.3866565212999,-20.0037819051163,
11.2339195103012));
#214665=CARTESIAN_POINT('Ctrl Pts',(-21.0542147974772,-17.2908452542003,
11.3610953169827));
#214666=CARTESIAN_POINT('Ctrl Pts',(-18.5931200057406,-16.1019149796642,
11.4882711236641));
#214667=CARTESIAN_POINT('Ctrl Pts',(-16.2612738647384,-17.5277608150597,
11.6154469303455));
#214668=CARTESIAN_POINT('Ctrl Pts',(-16.198000478146,-20.2602577043845,
11.742622737027));
#214669=CARTESIAN_POINT('Ctrl Pts',(-18.4613492509727,-21.7925093495675,
11.8697985437084));
#214670=CARTESIAN_POINT('Ctrl Pts',(-20.9748381634178,-20.7187699684155,
11.9969743503898));
#214671=CARTESIAN_POINT('Ctrl Pts',(-21.4324971430291,-18.0241287993538,
12.1241501570713));
#214672=CARTESIAN_POINT('Ctrl Pts',(-19.4144524815328,-16.1807518667032,
12.2513259637527));
#214673=CARTESIAN_POINT('Ctrl Pts',(-16.7721349018743,-16.879823093295,
12.3785017704341));
#214674=CARTESIAN_POINT('Ctrl Pts',(-15.9297067826652,-19.4799880179848,
12.5056775771156));
#214675=CARTESIAN_POINT('Ctrl Pts',(-17.6600436362941,-21.5957567068059,
12.632853383797));
#214676=CARTESIAN_POINT('Ctrl Pts',(-20.3756687963737,-21.2860427071796,
12.7600291904784));
#214677=CARTESIAN_POINT('Ctrl Pts',(-21.5851647292373,-18.8349893907445,
12.8872049971599));
#214678=CARTESIAN_POINT('Ctrl Pts',(-20.1788939862666,-16.4912860458039,
13.0143808038413));
#214679=CARTESIAN_POINT('Ctrl Pts',(-17.4470226911311,-16.4051350247055,
13.1415566105228));
#214680=CARTESIAN_POINT('Ctrl Pts',(-15.8958731980624,-18.6555745421719,
13.2687324172041));
#214681=CARTESIAN_POINT('Ctrl Pts',(-16.9485288917557,-21.1779660189567,
13.3959082238856));
#214682=CARTESIAN_POINT('Ctrl Pts',(-19.6392435084281,-21.6581718323812,
13.523084030567));
#214683=CARTESIAN_POINT('Ctrl Pts',(-21.4994533918664,-19.6556329535628,
13.6502598372485));
#214684=CARTESIAN_POINT('Ctrl Pts',(-20.8225314316626,-17.0075545122368,
13.7774356439299));
#214685=CARTESIAN_POINT('Ctrl Pts',(-18.2295115117883,-16.1433841200358,
13.9046114506113));
#214686=CARTESIAN_POINT('Ctrl Pts',(-16.0993284677614,-17.8559444753405,
14.0317872572928));
#214687=CARTESIAN_POINT('Ctrl Pts',(-16.3862930284057,-20.5740677456421,
14.1589630639742));
#214688=CARTESIAN_POINT('Ctrl Pts',(-18.8271330203595,-21.8040445361958,
14.2861388706557));
#214689=CARTESIAN_POINT('Ctrl Pts',(-21.1825292466206,-20.4174474826375,
14.4133146773371));
#214690=CARTESIAN_POINT('Ctrl Pts',(-21.2915518619716,-17.686393319688,
14.5404904840185));
#214691=CARTESIAN_POINT('Ctrl Pts',(-19.0541793835346,-16.1164547335152,
14.6676662907));
#214692=CARTESIAN_POINT('Ctrl Pts',(-16.5230621932784,-17.1479529355545,
14.7948420973814));
#214693=CARTESIAN_POINT('Ctrl Pts',(-16.0203432144126,-19.8345523474337,
14.9220179040628));
#214694=CARTESIAN_POINT('Ctrl Pts',(-18.0072359077879,-21.7114647579188,
15.0491937107442));
#214695=CARTESIAN_POINT('Ctrl Pts',(-20.6608895477009,-21.0567395247122,
15.1763695174257));
#214696=CARTESIAN_POINT('Ctrl Pts',(-21.5467416238517,-18.4710464124499,
15.3035453241071));
#214697=CARTESIAN_POINT('Ctrl Pts',(-19.8520778385523,-16.3265983654185,
15.4307211307886));
#214698=CARTESIAN_POINT('Ctrl Pts',(-17.1316470321183,-16.5907933673128,
15.55789693747));
#214699=CARTESIAN_POINT('Ctrl Pts',(-15.8812756204742,-19.0212489016859,
15.6850727441514));
#214700=CARTESIAN_POINT('Ctrl Pts',(-17.2481017670014,-21.3881728668337,
15.8122485508329));
#214701=CARTESIAN_POINT('Ctrl Pts',(-19.9781473170593,-21.5200594326025,
15.9394243575143));
#214702=CARTESIAN_POINT('Ctrl Pts',(-21.5667649242067,-19.295910860703,
16.0666001641957));
#214703=CARTESIAN_POINT('Ctrl Pts',(-20.5564965346144,-16.7562454196237,
16.1937759708772));
#214704=CARTESIAN_POINT('Ctrl Pts',(-17.8742006914056,-16.2310485221405,
16.3209517775586));
#214705=CARTESIAN_POINT('Ctrl Pts',(-15.9807173486685,-18.2021557242983,
16.44812758424));
#214706=CARTESIAN_POINT('Ctrl Pts',(-16.6131999505341,-20.8611985088279,
16.5753033909215));
#214707=CARTESIAN_POINT('Ctrl Pts',(-19.1913849660881,-21.7686701597314,
16.7024791976029));
#214708=CARTESIAN_POINT('Ctrl Pts',(-21.349947663769,-20.0920217613478,
16.8296550042843));
#214709=CARTESIAN_POINT('Ctrl Pts',(-21.1085407439649,-17.369474154658,
16.9568308109658));
#214710=CARTESIAN_POINT('Ctrl Pts',(-18.688640072193,-16.0987957884381,
17.0840066176472));
#214711=CARTESIAN_POINT('Ctrl Pts',(-16.3103543188293,-17.4457551965009,
17.2111824243287));
#214712=CARTESIAN_POINT('Ctrl Pts',(-16.1556130495236,-20.174600723678,
17.3383582310101));
#214713=CARTESIAN_POINT('Ctrl Pts',(-18.3663817745373,-21.7817859700398,
17.4655340376915));
#214714=CARTESIAN_POINT('Ctrl Pts',(-20.9144174044528,-20.7928182252147,
17.5927098443729));
#214715=CARTESIAN_POINT('Ctrl Pts',(-21.4620553977494,-18.1150140128212,
17.7198856510544));
#214716=CARTESIAN_POINT('Ctrl Pts',(-19.506871885825,-16.2050924944522,
17.8470614577358));
#214717=CARTESIAN_POINT('Ctrl Pts',(-16.8426263884951,-16.8152881201209,
17.9742372644172));
#214718=CARTESIAN_POINT('Ctrl Pts',(-15.9135987878357,-19.3857842762726,
18.1014130710987));
#214719=CARTESIAN_POINT('Ctrl Pts',(-17.5721142454945,-21.5583102826521,
18.2285888777801));
#214720=CARTESIAN_POINT('Ctrl Pts',(-20.2965877681507,-21.339708370521,
18.3557646844615));
#214721=CARTESIAN_POINT('Ctrl Pts',(-21.5874839986603,-18.9305322264037,
18.482940491143));
#214722=CARTESIAN_POINT('Ctrl Pts',(-20.2604857675958,-16.5410514319824,
18.6101162978244));
#214723=CARTESIAN_POINT('Ctrl Pts',(-17.5330315891426,-16.3634663086393,
18.7372921045058));
#214724=CARTESIAN_POINT('Ctrl Pts',(-15.907391387167,-18.560700184086,18.8644679111873));
#214725=CARTESIAN_POINT('Ctrl Pts',(-16.8749891483064,-21.1169273548174,
18.9916437178687));
#214726=CARTESIAN_POINT('Ctrl Pts',(-19.5481139827311,-21.6869680461436,
19.1188195245502));
#214727=CARTESIAN_POINT('Ctrl Pts',(-21.4743397674531,-19.7478453100669,
19.2459953312316));
#214728=CARTESIAN_POINT('Ctrl Pts',(-20.8864739005117,-17.0785838906586,
19.373171137913));
#214729=CARTESIAN_POINT('Ctrl Pts',(-18.323846826857,-16.1280654878871,
19.5003469445945));
#214730=CARTESIAN_POINT('Ctrl Pts',(-16.1375098337227,-17.7683317005682,
19.6275227512759));
#214731=CARTESIAN_POINT('Ctrl Pts',(-16.3332914095993,-20.4945401618491,
19.7546985579573));
#214732=CARTESIAN_POINT('Ctrl Pts',(-18.7315741166155,-21.8055636679596,
19.8818743646388));
#214733=CARTESIAN_POINT('Ctrl Pts',(-21.1320824129259,-20.4986198087347,
20.0090501713202));
#214734=CARTESIAN_POINT('Ctrl Pts',(-21.3324989528482,-17.7727479070516,
20.1362259780016));
#214735=CARTESIAN_POINT('Ctrl Pts',(-19.1489539543349,-16.1287673054729,
20.2634017846831));
#214736=CARTESIAN_POINT('Ctrl Pts',(-16.5847145159137,-17.0749261277227,
20.3905775913645));
#214737=CARTESIAN_POINT('Ctrl Pts',(-15.9923109972134,-19.7431863126012,
20.5177533980459));
#214738=CARTESIAN_POINT('Ctrl Pts',(-17.9152371863878,-21.6855771736479,
20.6449292047274));
#214739=CARTESIAN_POINT('Ctrl Pts',(-20.5893270222873,-21.1200902544022,
20.7721050114088));
#214740=CARTESIAN_POINT('Ctrl Pts',(-21.5612702725159,-18.5654965747524,
20.8992808180902));
#214741=CARTESIAN_POINT('Ctrl Pts',(-19.9393669813241,-16.3655314792863,
21.0264566247717));
#214742=CARTESIAN_POINT('Ctrl Pts',(-17.2116172781004,-16.5384219706357,
21.1536324314531));
#214743=CARTESIAN_POINT('Ctrl Pts',(-15.8805534910891,-18.9257529561851,
21.2808082381345));
#214744=CARTESIAN_POINT('Ctrl Pts',(-17.1673608343839,-21.3369087663789,
21.407984044816));
#214745=CARTESIAN_POINT('Ctrl Pts',(-19.8914410486737,-21.560550559712,
21.5351598514974));
#214746=CARTESIAN_POINT('Ctrl Pts',(-21.5536821355334,-19.3900613098573,
21.6623356581788));
#214747=CARTESIAN_POINT('Ctrl Pts',(-20.6289595069245,-16.8195073866206,
21.7895114648603));
#214748=CARTESIAN_POINT('Ctrl Pts',(-17.965893371406,-16.2018278499181,
21.9166872715417));
#214749=CARTESIAN_POINT('Ctrl Pts',(-16.006825229175,-18.1146792615168,
22.0438817345628));
#214750=CARTESIAN_POINT('Ctrl Pts',(-16.3702697667955,-19.8915948993761,
22.1286842620234));
#214751=CARTESIAN_POINT('Ctrl Pts',(-16.8880688264084,-20.506446560642,
22.1710948539236));
#214752=CARTESIAN_POINT('Ctrl Pts',(-19.3190224246859,-21.138301940011,
-0.171345675916538));
#214753=CARTESIAN_POINT('Ctrl Pts',(-20.0469417807877,-20.9435213660705,
-0.12895374035606));
#214754=CARTESIAN_POINT('Ctrl Pts',(-21.2802306600689,-19.7728918715264,
-0.0441698692351041));
#214755=CARTESIAN_POINT('Ctrl Pts',(-20.8017892686562,-17.2504053074226,
0.0830059374463301));
#214756=CARTESIAN_POINT('Ctrl Pts',(-18.42275638934,-16.2947311576948,0.210181744127764));
#214757=CARTESIAN_POINT('Ctrl Pts',(-16.3310537135823,-17.7741149391859,
0.337357550809199));
#214758=CARTESIAN_POINT('Ctrl Pts',(-16.4429842021291,-20.3355846707344,
0.464533357490633));
#214759=CARTESIAN_POINT('Ctrl Pts',(-18.6572569530825,-21.6269505831793,
0.591709164172068));
#214760=CARTESIAN_POINT('Ctrl Pts',(-20.9416889275276,-20.4646048528009,
0.718884970853502));
#214761=CARTESIAN_POINT('Ctrl Pts',(-21.2008319210033,-17.9143359178367,
0.846060777534936));
#214762=CARTESIAN_POINT('Ctrl Pts',(-19.1967429984043,-16.3161642831945,
0.973236584216371));
#214763=CARTESIAN_POINT('Ctrl Pts',(-16.7681507336229,-17.1361538706243,
1.1004123908978));
#214764=CARTESIAN_POINT('Ctrl Pts',(-16.1430851787862,-19.6220978379218,
1.22758819757924));
#214765=CARTESIAN_POINT('Ctrl Pts',(-17.8950324927765,-21.4932539623228,
1.35476400426067));
#214766=CARTESIAN_POINT('Ctrl Pts',(-20.4166755796707,-21.0329749170169,
1.48193981094211));
#214767=CARTESIAN_POINT('Ctrl Pts',(-21.3945707743255,-18.6635265940897,
1.60911561762354));
#214768=CARTESIAN_POINT('Ctrl Pts',(-19.9315561126419,-16.558736767109,
1.73629142430498));
#214769=CARTESIAN_POINT('Ctrl Pts',(-17.369858723403,-16.6496163492876,
1.86346723098641));
#214770=CARTESIAN_POINT('Ctrl Pts',(-16.0596759358701,-18.8527905813645,
1.99064303766784));
#214771=CARTESIAN_POINT('Ctrl Pts',(-17.2030196722955,-21.1469830106956,
2.11781884434928));
#214772=CARTESIAN_POINT('Ctrl Pts',(-19.7509427413702,-21.4274149125326,
2.24499465103071));
#214773=CARTESIAN_POINT('Ctrl Pts',(-21.3658840129548,-19.4368071964635,
2.37217045771215));
#214774=CARTESIAN_POINT('Ctrl Pts',(-20.5662350302976,-17.0014190082534,
2.49934626439358));
#214775=CARTESIAN_POINT('Ctrl Pts',(-18.0856241419088,-16.3555677924553,
2.62652207107501));
#214776=CARTESIAN_POINT('Ctrl Pts',(-16.1998578537051,-18.0917819851203,
2.75369787775646));
#214777=CARTESIAN_POINT('Ctrl Pts',(-16.639009701692,-20.6171928096815,
2.88087368443788));
#214778=CARTESIAN_POINT('Ctrl Pts',(-19.0001851167635,-21.6148925877907,
3.00804949111932));
#214779=CARTESIAN_POINT('Ctrl Pts',(-21.1171522094764,-20.169553692846,
3.13522529780075));
#214780=CARTESIAN_POINT('Ctrl Pts',(-21.0477250646041,-17.6071848554035,
3.26240110448218));
#214781=CARTESIAN_POINT('Ctrl Pts',(-18.8555987791894,-16.2786004440803,
3.38957691116362));
#214782=CARTESIAN_POINT('Ctrl Pts',(-16.5519131610055,-17.4026941956347,
3.51675271784505));
#214783=CARTESIAN_POINT('Ctrl Pts',(-16.2501567820852,-19.9481798618215,
3.64392852452649));
#214784=CARTESIAN_POINT('Ctrl Pts',(-18.2271723908689,-21.5797323347394,
3.77110433120793));
#214785=CARTESIAN_POINT('Ctrl Pts',(-20.6691708737799,-20.8005034859668,
3.89828013788936));
#214786=CARTESIAN_POINT('Ctrl Pts',(-21.3357701902385,-18.3253874199006,
4.02545594457079));
#214787=CARTESIAN_POINT('Ctrl Pts',(-19.6154068412282,-16.4251495041048,
4.15263175125223));
#214788=CARTESIAN_POINT('Ctrl Pts',(-17.0864074216668,-16.8431400842676,
4.27980755793366));
#214789=CARTESIAN_POINT('Ctrl Pts',(-16.068971931599,-19.1958787465047,
4.4069833646151));
#214790=CARTESIAN_POINT('Ctrl Pts',(-17.4965342839917,-21.3248737956469,
4.53415917129653));
#214791=CARTESIAN_POINT('Ctrl Pts',(-20.0593946250379,-21.2769044144401,
4.66133497797797));
#214792=CARTESIAN_POINT('Ctrl Pts',(-21.4062876608796,-19.0959795328267,
4.7885107846594));
#214793=CARTESIAN_POINT('Ctrl Pts',(-20.3015226287422,-16.7829623662223,
4.91568659134084));
#214794=CARTESIAN_POINT('Ctrl Pts',(-17.7586528761605,-16.4599026029505,
5.04286239802226));
#214795=CARTESIAN_POINT('Ctrl Pts',(-16.1106035728318,-18.4231875244628,
5.17003820470371));
#214796=CARTESIAN_POINT('Ctrl Pts',(-16.8693576650841,-20.8716250704767,
5.29721401138513));
#214797=CARTESIAN_POINT('Ctrl Pts',(-19.3388053668663,-21.5589257596971,
5.42438981806658));
#214798=CARTESIAN_POINT('Ctrl Pts',(-21.2533816830032,-19.8545338684562,
5.551565624748));
#214799=CARTESIAN_POINT('Ctrl Pts',(-20.8565816754472,-17.3221231704762,
5.67874143142944));
#214800=CARTESIAN_POINT('Ctrl Pts',(-18.5124447229449,-16.2850233020193,
5.80591723811088));
#214801=CARTESIAN_POINT('Ctrl Pts',(-16.3715709858693,-17.6947090227174,
5.93309304479231));
#214802=CARTESIAN_POINT('Ctrl Pts',(-16.3980792403773,-20.2578811787933,
6.06026885147374));
#214803=CARTESIAN_POINT('Ctrl Pts',(-18.5676498082457,-21.6229884054533,
6.18744465815518));
#214804=CARTESIAN_POINT('Ctrl Pts',(-20.8898363521913,-20.5376295503469,
6.31462046483661));
#214805=CARTESIAN_POINT('Ctrl Pts',(-21.234176849296,-17.9975539980662,
6.44179627151804));
#214806=CARTESIAN_POINT('Ctrl Pts',(-19.2847602656477,-16.33312341296,6.56897207819949));
#214807=CARTESIAN_POINT('Ctrl Pts',(-16.830055322305,-17.0713495506502,
6.6961478848809));
#214808=CARTESIAN_POINT('Ctrl Pts',(-16.1221014486134,-19.5349557492877,
6.82332369156236));
#214809=CARTESIAN_POINT('Ctrl Pts',(-17.810402383112,-21.4637362302682,
6.95049949824377));
#214810=CARTESIAN_POINT('Ctrl Pts',(-20.3460468061722,-21.0881546159098,
7.07767530492523));
#214811=CARTESIAN_POINT('Ctrl Pts',(-21.4027383394782,-18.7527837261624,
7.20485111160664));
#214812=CARTESIAN_POINT('Ctrl Pts',(-20.0110280868951,-16.6001814029045,
7.3320269182881));
#214813=CARTESIAN_POINT('Ctrl Pts',(-17.4477238258878,-16.6052266721572,
7.45920272496951));
#214814=CARTESIAN_POINT('Ctrl Pts',(-16.0644981193252,-18.7632908125259,
7.58637853165096));
#214815=CARTESIAN_POINT('Ctrl Pts',(-17.130374700309,-21.0944839197888,
7.71355433833239));
#214816=CARTESIAN_POINT('Ctrl Pts',(-19.6674779615479,-21.4600810081947,
7.84073014501382));
#214817=CARTESIAN_POINT('Ctrl Pts',(-21.3481731312431,-19.5246694406454,
7.96790595169526));
#214818=CARTESIAN_POINT('Ctrl Pts',(-20.630526706906,-17.0638692051782,
8.09508175837669));
#214819=CARTESIAN_POINT('Ctrl Pts',(-18.1729347407055,-16.3353117833461,
8.22225756505813));
#214820=CARTESIAN_POINT('Ctrl Pts',(-16.2300853262702,-18.0074033903068,
8.34943337173957));
#214821=CARTESIAN_POINT('Ctrl Pts',(-16.5844222145103,-20.5461037583834,
8.47660917842099));
#214822=CARTESIAN_POINT('Ctrl Pts',(-18.910863303093,-21.622312869381,8.60378498510243));
#214823=CARTESIAN_POINT('Ctrl Pts',(-21.0750432884624,-20.2486756610299,
8.73096079178387));
#214824=CARTESIAN_POINT('Ctrl Pts',(-21.091461358201,-17.685419014452,8.8581365984653));
#214825=CARTESIAN_POINT('Ctrl Pts',(-18.9450549523438,-16.2841718092325,
8.98531240514673));
#214826=CARTESIAN_POINT('Ctrl Pts',(-16.6050187272589,-17.3304913849503,
9.11248821182817));
#214827=CARTESIAN_POINT('Ctrl Pts',(-16.2181906804335,-19.8644444728012,
9.2396640185096));
#214828=CARTESIAN_POINT('Ctrl Pts',(-18.1394615355737,-21.561286389548,
9.36683982519104));
#214829=CARTESIAN_POINT('Ctrl Pts',(-20.6061845306062,-20.8642699944625,
9.49401563187247));
#214830=CARTESIAN_POINT('Ctrl Pts',(-21.3552944196844,-18.4128645683191,
9.62119143855391));
#214831=CARTESIAN_POINT('Ctrl Pts',(-19.6995293745825,-16.4560824382241,
9.74836724523534));
#214832=CARTESIAN_POINT('Ctrl Pts',(-17.1579510558127,-16.7891497569436,
9.87554305191677));
#214833=CARTESIAN_POINT('Ctrl Pts',(-16.062299822705,-19.1064979320416,
10.0027188585982));
#214834=CARTESIAN_POINT('Ctrl Pts',(-17.417767677851,-21.2821038437145,
10.1298946652796));
#214835=CARTESIAN_POINT('Ctrl Pts',(-19.9807969939772,-21.3199841013343,
10.257070471961));
#214836=CARTESIAN_POINT('Ctrl Pts',(-21.3999674530782,-19.1853859196488,
10.3842462786425));
#214837=CARTESIAN_POINT('Ctrl Pts',(-20.3732782425814,-16.8366706422493,
10.5114220853239));
#214838=CARTESIAN_POINT('Ctrl Pts',(-17.8426529895985,-16.4286387584391,
10.6385978920053));
#214839=CARTESIAN_POINT('Ctrl Pts',(-16.1297832954242,-18.3356341962992,
10.7657736986868));
#214840=CARTESIAN_POINT('Ctrl Pts',(-16.8061207917803,-20.8081070030786,
10.8929495053682));
#214841=CARTESIAN_POINT('Ctrl Pts',(-19.2511678039994,-21.5777168375263,
11.0201253120496));
#214842=CARTESIAN_POINT('Ctrl Pts',(-21.221745455103,-19.9383944439102,
11.1473011187311));
#214843=CARTESIAN_POINT('Ctrl Pts',(-20.9099710580464,-17.3941163705504,
11.2744769254125));
#214844=CARTESIAN_POINT('Ctrl Pts',(-18.6018782712276,-16.2790998340474,
11.401652732094));
#214845=CARTESIAN_POINT('Ctrl Pts',(-16.414998970158,-17.6163033009118,
11.5288285387754));
#214846=CARTESIAN_POINT('Ctrl Pts',(-16.3556591805319,-20.1789255865028,
11.6560043454568));
#214847=CARTESIAN_POINT('Ctrl Pts',(-18.4782994762885,-21.6159197980676,
11.7831801521383));
#214848=CARTESIAN_POINT('Ctrl Pts',(-20.8355291319859,-20.6089329364152,
11.9103559588197));
#214849=CARTESIAN_POINT('Ctrl Pts',(-21.2647362446946,-18.0818129464581,
12.0375317655011));
#214850=CARTESIAN_POINT('Ctrl Pts',(-19.372149928102,-16.3530355682261,
12.1647075721826));
#214851=CARTESIAN_POINT('Ctrl Pts',(-16.8941006605274,-17.0086467462216,
12.291883378864));
#214852=CARTESIAN_POINT('Ctrl Pts',(-16.1040448398867,-19.4471639164527,
12.4190591855454));
#214853=CARTESIAN_POINT('Ctrl Pts',(-17.7268096452235,-21.4313989266772,
12.5462349922269));
#214854=CARTESIAN_POINT('Ctrl Pts',(-20.2736090877839,-21.1409393105282,
12.6734107989083));
#214855=CARTESIAN_POINT('Ctrl Pts',(-21.4079127512197,-18.8422637378655,
12.8005866055897));
#214856=CARTESIAN_POINT('Ctrl Pts',(-20.0890674271536,-16.6442643747106,
12.9277624122712));
#214857=CARTESIAN_POINT('Ctrl Pts',(-17.5270318436439,-16.563469213532,
13.0549382189526));
#214858=CARTESIAN_POINT('Ctrl Pts',(-16.0723146306984,-18.6740027999979,
13.182114025634));
#214859=CARTESIAN_POINT('Ctrl Pts',(-17.0595285412618,-21.0395815630135,
13.3092898323155));
#214860=CARTESIAN_POINT('Ctrl Pts',(-19.5829660857976,-21.4899338118888,
13.4364656389969));
#214861=CARTESIAN_POINT('Ctrl Pts',(-21.3275299393921,-19.6118893102937,
13.5636414456783));
#214862=CARTESIAN_POINT('Ctrl Pts',(-20.6926910462166,-17.1284373238537,
13.6908172523598));
#214863=CARTESIAN_POINT('Ctrl Pts',(-18.2608746882143,-16.3179909097138,
13.8179930590412));
#214864=CARTESIAN_POINT('Ctrl Pts',(-16.2631214383067,-17.9240843508695,
13.9451688657226));
#214865=CARTESIAN_POINT('Ctrl Pts',(-16.5322459087333,-20.4732266004621,
14.0723446724041));
#214866=CARTESIAN_POINT('Ctrl Pts',(-18.8213431016262,-21.6267378621019,
14.1995204790855));
#214867=CARTESIAN_POINT('Ctrl Pts',(-21.0303084199013,-20.3263431482177,
14.326696285767));
#214868=CARTESIAN_POINT('Ctrl Pts',(-21.1325532878912,-17.7650738971998,
14.4538720924484));
#214869=CARTESIAN_POINT('Ctrl Pts',(-19.0342743852475,-16.2927356765588,
14.5810478991298));
#214870=CARTESIAN_POINT('Ctrl Pts',(-16.6605123712694,-17.2601074201168,
14.7082237058113));
#214871=CARTESIAN_POINT('Ctrl Pts',(-16.1890465614952,-19.779685595021,
14.8353995124927));
#214872=CARTESIAN_POINT('Ctrl Pts',(-18.0524175739244,-21.5399136084552,
14.9625753191741));
#214873=CARTESIAN_POINT('Ctrl Pts',(-20.5410981585017,-20.9258915101652,
15.0897511258555));
#214874=CARTESIAN_POINT('Ctrl Pts',(-21.3718783438148,-18.5009464648227,
15.216926932537));
#214875=CARTESIAN_POINT('Ctrl Pts',(-19.7825688738725,-16.4898150424656,
15.3441027392184));
#214876=CARTESIAN_POINT('Ctrl Pts',(-17.2312625436763,-16.7375854982129,
15.4712785458999));
#214877=CARTESIAN_POINT('Ctrl Pts',(-16.0586245592516,-19.0169438172852,
15.5984543525813));
#214878=CARTESIAN_POINT('Ctrl Pts',(-17.3404774891864,-21.2367202148663,
15.7256301592627));
#214879=CARTESIAN_POINT('Ctrl Pts',(-19.9008008310311,-21.3604076210367,
15.8528059659442));
#214880=CARTESIAN_POINT('Ctrl Pts',(-21.3906568302317,-19.2745305175414,
15.9799817726256));
#214881=CARTESIAN_POINT('Ctrl Pts',(-20.4431950784138,-16.8927516827034,
16.107157579307));
#214882=CARTESIAN_POINT('Ctrl Pts',(-17.9276529267619,-16.40020536762,16.2343333859885));
#214883=CARTESIAN_POINT('Ctrl Pts',(-16.1518841672621,-18.2487722455082,
16.3615091926699));
#214884=CARTESIAN_POINT('Ctrl Pts',(-16.7450464201164,-20.7425069409056,
16.4886849993513));
#214885=CARTESIAN_POINT('Ctrl Pts',(-19.1629501341323,-21.5935626494162,
16.6158608060327));
#214886=CARTESIAN_POINT('Ctrl Pts',(-21.1873187237296,-20.0211485809561,
16.7430366127142));
#214887=CARTESIAN_POINT('Ctrl Pts',(-20.9609196544379,-17.4678570483134,
16.8702124193956));
#214888=CARTESIAN_POINT('Ctrl Pts',(-18.6914600204213,-16.276174557543,
16.9973882260771));
#214889=CARTESIAN_POINT('Ctrl Pts',(-16.4610281773391,-17.5393958297695,
17.1245640327585));
#214890=CARTESIAN_POINT('Ctrl Pts',(-16.3159069050066,-20.0985937520796,
17.2517398394399));
#214891=CARTESIAN_POINT('Ctrl Pts',(-18.3892359635466,-21.6058630724912,
17.3789156461214));
#214892=CARTESIAN_POINT('Ctrl Pts',(-20.7788646270633,-20.6783777412105,
17.5060914528028));
#214893=CARTESIAN_POINT('Ctrl Pts',(-21.2924569138618,-18.1670479834574,
17.6332672594842));
#214894=CARTESIAN_POINT('Ctrl Pts',(-19.458823777937,-16.375862981263,17.7604430661657));
#214895=CARTESIAN_POINT('Ctrl Pts',(-16.9602098133921,-16.9481238006687,
17.8876188728471));
#214896=CARTESIAN_POINT('Ctrl Pts',(-16.0889382512251,-19.3588166583677,
18.0147946795285));
#214897=CARTESIAN_POINT('Ctrl Pts',(-17.6443466725109,-21.3962804819219,
18.14197048621));
#214898=CARTESIAN_POINT('Ctrl Pts',(-20.1994443902567,-21.1912686724342,
18.2691462928914));
#214899=CARTESIAN_POINT('Ctrl Pts',(-21.4100878356756,-18.9318668407438,
18.3963220995729));
#214900=CARTESIAN_POINT('Ctrl Pts',(-20.1655867886111,-16.6909359329365,
18.5234979062543));
#214901=CARTESIAN_POINT('Ctrl Pts',(-17.607693717282,-16.5243909694468,
18.6506737129357));
#214902=CARTESIAN_POINT('Ctrl Pts',(-16.0831167539157,-18.5850266165988,
18.7778495196171));
#214903=CARTESIAN_POINT('Ctrl Pts',(-16.9905606364213,-20.9823375670122,
18.9050253262986));
#214904=CARTESIAN_POINT('Ctrl Pts',(-19.4975019250372,-21.5169398148659,
19.03220113298));
#214905=CARTESIAN_POINT('Ctrl Pts',(-21.3039775855559,-19.6983689841434,
19.1593769396615));
#214906=CARTESIAN_POINT('Ctrl Pts',(-20.7526583224132,-17.1950509287168,
19.2865527463429));
#214907=CARTESIAN_POINT('Ctrl Pts',(-18.3493453399679,-16.3036246104209,
19.4137285530243));
#214908=CARTESIAN_POINT('Ctrl Pts',(-16.2989291348091,-17.8419183107137,
19.5409043597057));
#214909=CARTESIAN_POINT('Ctrl Pts',(-16.4825393088626,-20.3986431089516,
19.6680801663872));
#214910=CARTESIAN_POINT('Ctrl Pts',(-18.7317249295881,-21.6281625520724,
19.7952559730686));
#214911=CARTESIAN_POINT('Ctrl Pts',(-20.9829977785724,-20.402469131249,
19.9224317797501));
#214912=CARTESIAN_POINT('Ctrl Pts',(-21.1709547689763,-17.8460599692811,
20.0496075864315));
#214913=CARTESIAN_POINT('Ctrl Pts',(-19.1231569849638,-16.3042827972216,
20.1767833931129));
#214914=CARTESIAN_POINT('Ctrl Pts',(-16.7183318756798,-17.191620562574,
20.3039591997943));
#214915=CARTESIAN_POINT('Ctrl Pts',(-16.1627570587368,-19.6939996284889,
20.4311350064758));
#214916=CARTESIAN_POINT('Ctrl Pts',(-17.9661382538539,-21.5156354105067,
20.5583108131572));
#214917=CARTESIAN_POINT('Ctrl Pts',(-20.4739845514727,-20.9853038346024,
20.6854866198387));
#214918=CARTESIAN_POINT('Ctrl Pts',(-21.3855037715295,-18.5895248239564,
20.8126624265201));
#214919=CARTESIAN_POINT('Ctrl Pts',(-19.8644314016694,-16.5263277520078,
20.9398382332015));
#214920=CARTESIAN_POINT('Ctrl Pts',(-17.3062611778333,-16.6884699406521,
21.067014039883));
#214921=CARTESIAN_POINT('Ctrl Pts',(-16.0579473234008,-18.9273846894854,
21.1941898465644));
#214922=CARTESIAN_POINT('Ctrl Pts',(-17.2647560806485,-21.1886431148375,
21.3213656532458));
#214923=CARTESIAN_POINT('Ctrl Pts',(-19.8194849413283,-21.3983814848332,
21.4485414599273));
#214924=CARTESIAN_POINT('Ctrl Pts',(-21.3783873758939,-19.3628277961746,
21.5757172666087));
#214925=CARTESIAN_POINT('Ctrl Pts',(-20.5111531531137,-16.9520807626706,
21.7028930732902));
#214926=CARTESIAN_POINT('Ctrl Pts',(-18.0136452314969,-16.3728012940309,
21.8300688799716));
#214927=CARTESIAN_POINT('Ctrl Pts',(-16.1763689660104,-18.1667340430625,
21.9572633429927));
#214928=CARTESIAN_POINT('Ctrl Pts',(-16.5172187855734,-19.8331819102065,
22.0420658704533));
#214929=CARTESIAN_POINT('Ctrl Pts',(-17.0028271735668,-20.4098093075325,
22.0844764623534));
#214930=CARTESIAN_POINT('Ctrl Pts',(-19.2802416597141,-20.9933733729761,
-0.257964067486649));
#214931=CARTESIAN_POINT('Ctrl Pts',(-19.9599077040175,-20.8115046795727,
-0.215572131926171));
#214932=CARTESIAN_POINT('Ctrl Pts',(-21.1114426467799,-19.7184754707294,
-0.130788260805215));
#214933=CARTESIAN_POINT('Ctrl Pts',(-20.6647168313355,-17.3632029388733,
-0.00361245412378029));
#214934=CARTESIAN_POINT('Ctrl Pts',(-18.4433885306129,-16.4708798215613,
0.123563352557654));
#214935=CARTESIAN_POINT('Ctrl Pts',(-16.4903434967449,-17.8521961917666,
0.250739159239088));
#214936=CARTESIAN_POINT('Ctrl Pts',(-16.5948541842955,-20.2438677216565,
0.377914965920522));
#214937=CARTESIAN_POINT('Ctrl Pts',(-18.6623442009214,-21.4496298079404,
0.505090772601956));
#214938=CARTESIAN_POINT('Ctrl Pts',(-20.7953426306735,-20.3643352377974,
0.632266579283392));
#214939=CARTESIAN_POINT('Ctrl Pts',(-21.0373071996992,-17.9831220108,0.759442385964825));
#214940=CARTESIAN_POINT('Ctrl Pts',(-19.1660680589383,-16.4908921587843,
0.886618192646261));
#214941=CARTESIAN_POINT('Ctrl Pts',(-16.8984656329369,-17.2565251572569,
1.0137939993277));
#214942=CARTESIAN_POINT('Ctrl Pts',(-16.3148352767375,-19.5776774778398,
1.14096980600913));
#214943=CARTESIAN_POINT('Ctrl Pts',(-17.9506471159836,-21.3247958511667,
1.26814561269057));
#214944=CARTESIAN_POINT('Ctrl Pts',(-20.3051320841986,-20.8950284114407,
1.395321419372));
#214945=CARTESIAN_POINT('Ctrl Pts',(-21.2182032274825,-18.6826493129518,
1.52249722605343));
#214946=CARTESIAN_POINT('Ctrl Pts',(-19.8521708785292,-16.7173846668031,
1.64967303273487));
#214947=CARTESIAN_POINT('Ctrl Pts',(-17.4602867822325,-16.8022398991988,
1.7768488394163));
#214948=CARTESIAN_POINT('Ctrl Pts',(-16.2369551795592,-18.8593671107158,
1.90402464609774));
#214949=CARTESIAN_POINT('Ctrl Pts',(-17.3045073858597,-21.0014789809986,
2.03120045277917));
#214950=CARTESIAN_POINT('Ctrl Pts',(-19.6835302529274,-21.2633212301712,
2.15837625946061));
#214951=CARTESIAN_POINT('Ctrl Pts',(-21.1914180933035,-19.4046696353217,
2.28555206614204));
#214952=CARTESIAN_POINT('Ctrl Pts',(-20.4447773338319,-17.1307217833394,
2.41272787282348));
#214953=CARTESIAN_POINT('Ctrl Pts',(-18.1286045657439,-16.5276836344422,
2.53990367950491));
#214954=CARTESIAN_POINT('Ctrl Pts',(-16.3678445270935,-18.1488052909833,
2.66707948618633));
#214955=CARTESIAN_POINT('Ctrl Pts',(-16.7778852779924,-20.5068082359283,
2.79425529286778));
#214956=CARTESIAN_POINT('Ctrl Pts',(-18.9825398744333,-21.4383711294077,
2.92143109954921));
#214957=CARTESIAN_POINT('Ctrl Pts',(-20.9591745631026,-20.0888428318423,
3.04860690623065));
#214958=CARTESIAN_POINT('Ctrl Pts',(-20.8943496995691,-17.6963317972172,
3.17578271291207));
#214959=CARTESIAN_POINT('Ctrl Pts',(-18.847538073347,-16.4558184027074,
3.30295851959352));
#214960=CARTESIAN_POINT('Ctrl Pts',(-16.6965623116711,-17.5053966934078,
3.43013432627495));
#214961=CARTESIAN_POINT('Ctrl Pts',(-16.4148091714573,-19.8821437314771,
3.55731013295638));
#214962=CARTESIAN_POINT('Ctrl Pts',(-18.2607696711808,-21.4055416272001,
3.68448593963782));
#214963=CARTESIAN_POINT('Ctrl Pts',(-20.5408896256266,-20.6779673639072,
3.81166174631925));
#214964=CARTESIAN_POINT('Ctrl Pts',(-21.163300496769,-18.3669251698599,
3.93883755300069));
#214965=CARTESIAN_POINT('Ctrl Pts',(-19.5569789415241,-16.5926528186193,
4.06601335968212));
#214966=CARTESIAN_POINT('Ctrl Pts',(-17.1956252872621,-16.9829350686982,
4.19318916636356));
#214967=CARTESIAN_POINT('Ctrl Pts',(-16.2456349496354,-19.1797121792916,
4.32036497304499));
#214968=CARTESIAN_POINT('Ctrl Pts',(-17.5785651003642,-21.1675774987978,
4.44754077972642));
#214969=CARTESIAN_POINT('Ctrl Pts',(-19.9715350571314,-21.1227879774049,
4.57471658640786));
#214970=CARTESIAN_POINT('Ctrl Pts',(-21.2291434090686,-19.0864352210401,
4.70189239308929));
#214971=CARTESIAN_POINT('Ctrl Pts',(-20.197612549251,-16.9267464933619,
4.82906819977073));
#214972=CARTESIAN_POINT('Ctrl Pts',(-17.8233080175354,-16.6251021566151,
4.95624400645216));
#214973=CARTESIAN_POINT('Ctrl Pts',(-16.284506855812,-18.4582421676058,
5.0834198131336));
#214974=CARTESIAN_POINT('Ctrl Pts',(-16.9929636211903,-20.7443743437509,
5.21059561981502));
#214975=CARTESIAN_POINT('Ctrl Pts',(-19.298713203222,-21.3861143068026,
5.33777142649647));
#214976=CARTESIAN_POINT('Ctrl Pts',(-21.0863734713516,-19.7947054715354,
5.4649472331779));
#214977=CARTESIAN_POINT('Ctrl Pts',(-20.7158770842802,-17.4301666703347,
5.59212303985933));
#214978=CARTESIAN_POINT('Ctrl Pts',(-18.5271314815462,-16.4618154934729,
5.71929884654077));
#214979=CARTESIAN_POINT('Ctrl Pts',(-16.5281749047854,-17.7780540430683,
5.8464746532222));
#214980=CARTESIAN_POINT('Ctrl Pts',(-16.552925943938,-20.171315144845,5.97365045990364));
#214981=CARTESIAN_POINT('Ctrl Pts',(-18.5786770568045,-21.4459302804593,
6.10082626658507));
#214982=CARTESIAN_POINT('Ctrl Pts',(-20.7469273296236,-20.4325191745226,
6.22800207326651));
#214983=CARTESIAN_POINT('Ctrl Pts',(-21.0684417138734,-18.0608236173447,
6.35517787994794));
#214984=CARTESIAN_POINT('Ctrl Pts',(-19.2482507174378,-16.5067270786087,
6.48235368662938));
#214985=CARTESIAN_POINT('Ctrl Pts',(-16.9562666057522,-17.1960166744951,
6.6095294933108));
#214986=CARTESIAN_POINT('Ctrl Pts',(-16.2952425447106,-19.4963119829154,
6.73670529999224));
#214987=CARTESIAN_POINT('Ctrl Pts',(-17.8716270825383,-21.2972348308226,
6.86388110667369));
#214988=CARTESIAN_POINT('Ctrl Pts',(-20.2391852472374,-20.94655028314,6.9910569133551));
#214989=CARTESIAN_POINT('Ctrl Pts',(-21.2258293699287,-18.7659896464285,
7.11823272003656));
#214990=CARTESIAN_POINT('Ctrl Pts',(-19.9263747060834,-16.7560819640143,
7.24540852671797));
#214991=CARTESIAN_POINT('Ctrl Pts',(-17.5329902565274,-16.7607927855726,
7.37258433339943));
#214992=CARTESIAN_POINT('Ctrl Pts',(-16.2414577035358,-18.7758002247102,
7.49976014008084));
#214993=CARTESIAN_POINT('Ctrl Pts',(-17.2366780029277,-20.9524600214847,
7.62693594676229));
#214994=CARTESIAN_POINT('Ctrl Pts',(-19.6055983003493,-21.293821911099,
7.75411175344372));
#214995=CARTESIAN_POINT('Ctrl Pts',(-21.1748812546918,-19.48670754714,7.88128756012516));
#214996=CARTESIAN_POINT('Ctrl Pts',(-20.5048071560311,-17.1890321963735,
8.00846336680658));
#214997=CARTESIAN_POINT('Ctrl Pts',(-18.2101274003992,-16.5087703833118,
8.13563917348801));
#214998=CARTESIAN_POINT('Ctrl Pts',(-16.3960682397005,-18.0700200996293,
8.26281498016946));
#214999=CARTESIAN_POINT('Ctrl Pts',(-16.7269163606663,-20.4404316326905,
8.38999078685089));
#215000=CARTESIAN_POINT('Ctrl Pts',(-18.8991391470608,-21.4452995252443,
8.51716659353233));
#215001=CARTESIAN_POINT('Ctrl Pts',(-20.9198570157183,-20.1627198550076,
8.64434240021374));
#215002=CARTESIAN_POINT('Ctrl Pts',(-20.9351867420414,-17.7693798635505,
8.77151820689519));
#215003=CARTESIAN_POINT('Ctrl Pts',(-18.9310642535986,-16.4610204456021,
8.89869401357662));
#215004=CARTESIAN_POINT('Ctrl Pts',(-16.7461475436661,-17.4379801611861,
9.02586982025806));
#215005=CARTESIAN_POINT('Ctrl Pts',(-16.3849620823817,-19.8039591082128,
9.15304562693949));
#215006=CARTESIAN_POINT('Ctrl Pts',(-18.1788731127761,-21.3883184520001,
9.28022143362092));
#215007=CARTESIAN_POINT('Ctrl Pts',(-20.4820786071378,-20.7375068310543,
9.40739724030236));
#215008=CARTESIAN_POINT('Ctrl Pts',(-21.1815304774453,-18.4486035136685,
9.53457304698381));
#215009=CARTESIAN_POINT('Ctrl Pts',(-19.6355250455705,-16.6215352281822,
9.66174885366522));
#215010=CARTESIAN_POINT('Ctrl Pts',(-17.2624263393396,-16.932523725882,
9.78892466034668));
#215011=CARTESIAN_POINT('Ctrl Pts',(-16.2394051306023,-19.0962563622516,
9.91610046702808));
#215012=CARTESIAN_POINT('Ctrl Pts',(-17.5050198825181,-21.1276427398149,
10.0432762737096));
#215013=CARTESIAN_POINT('Ctrl Pts',(-19.8981476131147,-21.1630119392157,
10.170452080391));
#215014=CARTESIAN_POINT('Ctrl Pts',(-21.2232421638282,-19.1699149152638,
10.2976278870724));
#215015=CARTESIAN_POINT('Ctrl Pts',(-20.2646115290223,-16.9768944818824,
10.4248036937539));
#215016=CARTESIAN_POINT('Ctrl Pts',(-17.901739816804,-16.5959107725,10.5519795004353));
#215017=CARTESIAN_POINT('Ctrl Pts',(-16.3024151667752,-18.3764926939591,
10.6791553071167));
#215018=CARTESIAN_POINT('Ctrl Pts',(-16.9339186800547,-20.6850668486988,
10.8063311137982));
#215019=CARTESIAN_POINT('Ctrl Pts',(-19.2168850787369,-21.4036597360172,
10.9335069204796));
#215020=CARTESIAN_POINT('Ctrl Pts',(-21.0568343889061,-19.8730069827043,
11.0606827271611));
#215021=CARTESIAN_POINT('Ctrl Pts',(-20.7657273186155,-17.4973874869004,
11.1878585338425));
#215022=CARTESIAN_POINT('Ctrl Pts',(-18.6106365367144,-16.4562846884308,
11.3150343405239));
#215023=CARTESIAN_POINT('Ctrl Pts',(-16.5687240755777,-17.7048457867641,
11.4422101472054));
#215024=CARTESIAN_POINT('Ctrl Pts',(-16.5133178829179,-20.0975934686209,
11.5693859538868));
#215025=CARTESIAN_POINT('Ctrl Pts',(-18.4952497016042,-21.4393302465677,
11.6965617605682));
#215026=CARTESIAN_POINT('Ctrl Pts',(-20.6962201005539,-20.4990959044147,
11.8237375672497));
#215027=CARTESIAN_POINT('Ctrl Pts',(-21.09697534636,-18.1394970935624,11.9509133739311));
#215028=CARTESIAN_POINT('Ctrl Pts',(-19.3298473746713,-16.5253192697488,
12.0780891806125));
#215029=CARTESIAN_POINT('Ctrl Pts',(-17.0160664191804,-17.1374703991481,
12.205264987294));
#215030=CARTESIAN_POINT('Ctrl Pts',(-16.2783828971083,-19.4143398149205,
12.3324407939754));
#215031=CARTESIAN_POINT('Ctrl Pts',(-17.7935756541529,-21.2670411465485,
12.4596166006568));
#215032=CARTESIAN_POINT('Ctrl Pts',(-20.1715493791944,-20.9958359138768,
12.5867924073383));
#215033=CARTESIAN_POINT('Ctrl Pts',(-21.2306607732021,-18.8495380849864,
12.7139682140197));
#215034=CARTESIAN_POINT('Ctrl Pts',(-19.9992408680408,-16.7972427036174,
12.8411440207011));
#215035=CARTESIAN_POINT('Ctrl Pts',(-17.6070409961567,-16.7218034023586,
12.9683198273826));
#215036=CARTESIAN_POINT('Ctrl Pts',(-16.2487560633345,-18.6924310578239,
13.095495634064));
#215037=CARTESIAN_POINT('Ctrl Pts',(-17.1705281907678,-20.9011971070702,
13.2226714407454));
#215038=CARTESIAN_POINT('Ctrl Pts',(-19.526688663167,-21.3216957913963,
13.3498472474269));
#215039=CARTESIAN_POINT('Ctrl Pts',(-21.1556064869176,-19.5681456670245,
13.4770230541083));
#215040=CARTESIAN_POINT('Ctrl Pts',(-20.5628506607707,-17.2493201354707,
13.6041988607897));
#215041=CARTESIAN_POINT('Ctrl Pts',(-18.2922378646403,-16.4925976993917,
13.7313746674712));
#215042=CARTESIAN_POINT('Ctrl Pts',(-16.426914408852,-17.9922242263985,
13.8585504741526));
#215043=CARTESIAN_POINT('Ctrl Pts',(-16.6781987890609,-20.3723854552819,
13.985726280834));
#215044=CARTESIAN_POINT('Ctrl Pts',(-18.8155531828929,-21.449431188008,
14.1129020875155));
#215045=CARTESIAN_POINT('Ctrl Pts',(-20.878087593182,-20.2352388137978,
14.2400778941968));
#215046=CARTESIAN_POINT('Ctrl Pts',(-20.973554713811,-17.8437544747116,
14.3672537008784));
#215047=CARTESIAN_POINT('Ctrl Pts',(-19.0143693869603,-16.4690166196025,
14.4944295075598));
#215048=CARTESIAN_POINT('Ctrl Pts',(-16.7979625492603,-17.372261904679,
14.6216053142412));
#215049=CARTESIAN_POINT('Ctrl Pts',(-16.3577499085777,-19.7248188426085,
14.7487811209226));
#215050=CARTESIAN_POINT('Ctrl Pts',(-18.097599240061,-21.3683624589916,
14.8759569276041));
#215051=CARTESIAN_POINT('Ctrl Pts',(-20.4213067693024,-20.7950434956184,
15.0031327342855));
#215052=CARTESIAN_POINT('Ctrl Pts',(-21.1970150637779,-18.5308465171956,
15.130308540967));
#215053=CARTESIAN_POINT('Ctrl Pts',(-19.7130599091926,-16.6530317195128,
15.2574843476484));
#215054=CARTESIAN_POINT('Ctrl Pts',(-17.3308780552345,-16.884377629113,
15.3846601543298));
#215055=CARTESIAN_POINT('Ctrl Pts',(-16.2359734980291,-19.0126387328847,
15.5118359610112));
#215056=CARTESIAN_POINT('Ctrl Pts',(-17.4328532113714,-21.0852675628988,
15.6390117676927));
#215057=CARTESIAN_POINT('Ctrl Pts',(-19.823454345003,-21.2007558094709,
15.7661875743741));
#215058=CARTESIAN_POINT('Ctrl Pts',(-21.2145487362569,-19.2531501743798,
15.8933633810556));
#215059=CARTESIAN_POINT('Ctrl Pts',(-20.3298936222131,-17.0292579457831,
16.020539187737));
#215060=CARTESIAN_POINT('Ctrl Pts',(-17.9811051621181,-16.5693622130996,
16.1477149944184));
#215061=CARTESIAN_POINT('Ctrl Pts',(-16.3230509858558,-18.295388766718,
16.2748908010999));
#215062=CARTESIAN_POINT('Ctrl Pts',(-16.8768928896987,-20.6238153729833,
16.4020666077813));
#215063=CARTESIAN_POINT('Ctrl Pts',(-19.1345153021762,-21.418455139101,
16.5292424144627));
#215064=CARTESIAN_POINT('Ctrl Pts',(-21.0246897836904,-19.9502754005642,
16.6564182211442));
#215065=CARTESIAN_POINT('Ctrl Pts',(-20.8132985649108,-17.5662399419689,
16.7835940278256));
#215066=CARTESIAN_POINT('Ctrl Pts',(-18.6942799686495,-16.4535533266478,
16.910769834507));
#215067=CARTESIAN_POINT('Ctrl Pts',(-16.6117020358488,-17.6330364630381,
17.0379456411885));
#215068=CARTESIAN_POINT('Ctrl Pts',(-16.4762007604896,-20.0225867804811,
17.1651214478699));
#215069=CARTESIAN_POINT('Ctrl Pts',(-18.4120901525558,-21.4299401749425,
17.2922972545513));
#215070=CARTESIAN_POINT('Ctrl Pts',(-20.6433118496738,-20.563937257206,
17.4194730612328));
#215071=CARTESIAN_POINT('Ctrl Pts',(-21.1228584299742,-18.2190819540937,
17.5466488679142));
#215072=CARTESIAN_POINT('Ctrl Pts',(-19.4107756700491,-16.5466334680738,
17.6738246745956));
#215073=CARTESIAN_POINT('Ctrl Pts',(-17.0777932382892,-17.0809594812165,
17.8010004812771));
#215074=CARTESIAN_POINT('Ctrl Pts',(-16.2642777146144,-19.3318490404626,
17.9281762879585));
#215075=CARTESIAN_POINT('Ctrl Pts',(-17.7165790995274,-21.2342506811916,
18.05535209464));
#215076=CARTESIAN_POINT('Ctrl Pts',(-20.1023010123624,-21.0428289743473,
18.1825279013214));
#215077=CARTESIAN_POINT('Ctrl Pts',(-21.2326916726909,-18.9332014550839,
18.3097037080028));
#215078=CARTESIAN_POINT('Ctrl Pts',(-20.0706878096263,-16.8408204338905,
18.4368795146842));
#215079=CARTESIAN_POINT('Ctrl Pts',(-17.6823558454215,-16.6853156302542,
18.5640553213657));
#215080=CARTESIAN_POINT('Ctrl Pts',(-16.2588421206643,-18.6093530491115,
18.6912311280471));
#215081=CARTESIAN_POINT('Ctrl Pts',(-17.1061321245363,-20.8477477792071,
18.8184069347286));
#215082=CARTESIAN_POINT('Ctrl Pts',(-19.4468898673433,-21.3469115835881,
18.94558274141));
#215083=CARTESIAN_POINT('Ctrl Pts',(-21.1336154036588,-19.6488926582199,
19.0727585480914));
#215084=CARTESIAN_POINT('Ctrl Pts',(-20.6188427443147,-17.3115179667752,
19.1999343547728));
#215085=CARTESIAN_POINT('Ctrl Pts',(-18.3748438530787,-16.4791837329545,
19.3271101614543));
#215086=CARTESIAN_POINT('Ctrl Pts',(-16.4603484358955,-17.9155049208591,
19.4542859681357));
#215087=CARTESIAN_POINT('Ctrl Pts',(-16.6317872081259,-20.302746056054,
19.5814617748171));
#215088=CARTESIAN_POINT('Ctrl Pts',(-18.7318757425608,-21.4507614361853,
19.7086375814986));
#215089=CARTESIAN_POINT('Ctrl Pts',(-20.8339131442188,-20.3063184537634,
19.83581338818));
#215090=CARTESIAN_POINT('Ctrl Pts',(-21.0094105851045,-17.9193720315106,
19.9629891948615));
#215091=CARTESIAN_POINT('Ctrl Pts',(-19.0973600155928,-16.4797982889704,
20.0901650015429));
#215092=CARTESIAN_POINT('Ctrl Pts',(-16.8519492354458,-17.3083149974252,
20.2173408082243));
#215093=CARTESIAN_POINT('Ctrl Pts',(-16.3332031202602,-19.6448129443766,
20.3445166149058));
#215094=CARTESIAN_POINT('Ctrl Pts',(-18.01703932132,-21.3456936473654,20.4716924215872));
#215095=CARTESIAN_POINT('Ctrl Pts',(-20.358642080658,-20.8505174148026,
20.5988682282686));
#215096=CARTESIAN_POINT('Ctrl Pts',(-21.2097372705433,-18.6135530731602,
20.72604403495));
#215097=CARTESIAN_POINT('Ctrl Pts',(-19.7894958220145,-16.6871240247294,
20.8532198416315));
#215098=CARTESIAN_POINT('Ctrl Pts',(-17.4009050775665,-16.8385179106685,
20.9803956483129));
#215099=CARTESIAN_POINT('Ctrl Pts',(-16.2353411557127,-18.9290164227857,
21.1075714549944));
#215100=CARTESIAN_POINT('Ctrl Pts',(-17.3621513269132,-21.0403774632962,
21.2347472616758));
#215101=CARTESIAN_POINT('Ctrl Pts',(-19.7475288339831,-21.2362124099542,
21.3619230683572));
#215102=CARTESIAN_POINT('Ctrl Pts',(-21.2030926162545,-19.335594282492,
21.4890988750387));
#215103=CARTESIAN_POINT('Ctrl Pts',(-20.3933467993028,-17.0846541387204,
21.6162746817201));
#215104=CARTESIAN_POINT('Ctrl Pts',(-18.0613970915878,-16.5437747381437,
21.7434504884015));
#215105=CARTESIAN_POINT('Ctrl Pts',(-16.3459127028459,-18.2187888246082,
21.8706449514226));
#215106=CARTESIAN_POINT('Ctrl Pts',(-16.6641678043512,-19.7747689210369,
21.9554474788832));
#215107=CARTESIAN_POINT('Ctrl Pts',(-17.117585520725,-20.3131720544228,
21.9978580707833));
#215108=CARTESIAN_POINT('Ctrl Pts',(-19.3957372685685,-21.4249949024184,
-1.39254927034038E-15));
#215109=CARTESIAN_POINT('Ctrl Pts',(-19.4773891020297,-21.3954306668132,
2.38531586308131E-15));
#215110=CARTESIAN_POINT('Ctrl Pts',(-19.5571492231821,-21.3614659991419,
1.6186890260879E-14));
#215111=CARTESIAN_POINT('Ctrl Pts',(-19.6348156046203,-21.3234187284543,
1.5709655798446E-14));
#215112=CARTESIAN_POINT('Ctrl Pts',(-19.7143272588109,-21.2844674940362,
1.5221082739651E-14));
#215113=CARTESIAN_POINT('Ctrl Pts',(-19.791645221544,-21.2412367046751,
5.31486745776737E-15));
#215114=CARTESIAN_POINT('Ctrl Pts',(-19.8665232792529,-21.1940209467401,
3.51454976232901E-15));
#215115=CARTESIAN_POINT('Ctrl Pts',(-19.9365886939553,-21.1498398907482,
1.82994402085299E-15));
#215116=CARTESIAN_POINT('Ctrl Pts',(-20.0045179028409,-21.1021686855581,
2.13733777873822E-15));
#215117=CARTESIAN_POINT('Ctrl Pts',(-20.0700783470716,-21.0512211850772,
-1.82284742855643E-14));
#215118=CARTESIAN_POINT('Ctrl Pts',(-20.0997467345518,-21.0281656642803,
-2.7297595720857E-14));
#215119=CARTESIAN_POINT('Ctrl Pts',(-20.128929580841,-21.0044388940273,
8.44227451794598E-16));
#215120=CARTESIAN_POINT('Ctrl Pts',(-20.1576029444589,-20.9800594108908,
2.3037127760972E-15));
#215121=CARTESIAN_POINT('Ctrl Pts',(-20.1753081557669,-20.9650055823179,
2.84180167051755E-15));
#215122=CARTESIAN_POINT('Ctrl Pts',(-20.1928190804462,-20.9497028729833,
-1.45985713076056E-14));
#215123=CARTESIAN_POINT('Ctrl Pts',(-20.2101297684373,-20.9341555341053,
-1.7874590696465E-14));
#215124=CARTESIAN_POINT('Ctrl Pts',(-20.2222918053998,-20.923232380144,
-1.99659078843905E-14));
#215125=CARTESIAN_POINT('Ctrl Pts',(-20.2343567785502,-20.9121866751007,
-2.1053807985098E-14));
#215126=CARTESIAN_POINT('Ctrl Pts',(-20.2463057260566,-20.9010359825867,
-1.90333859784175E-14));
#215127=CARTESIAN_POINT('Ctrl Pts',(-20.3097375112913,-20.8418417872492,
-8.05854395286965E-15));
#215128=CARTESIAN_POINT('Ctrl Pts',(-20.3700069578684,-20.7796002467127,
-1.58672311013317E-14));
#215129=CARTESIAN_POINT('Ctrl Pts',(-20.4268835059678,-20.7145895545046,
-1.55431223447522E-15));
#215130=CARTESIAN_POINT('Ctrl Pts',(-20.4830376461208,-20.6504045847113,
1.25768134914526E-14));
#215131=CARTESIAN_POINT('Ctrl Pts',(-20.5358849804778,-20.583519523084,
-3.34795984228788E-14));
#215132=CARTESIAN_POINT('Ctrl Pts',(-20.5851611052647,-20.5141759583156,
-1.8471335572201E-14));
#215133=CARTESIAN_POINT('Ctrl Pts',(-20.6305983443516,-20.4502346450498,
-4.63230033198983E-15));
#215134=CARTESIAN_POINT('Ctrl Pts',(-20.6729990002168,-20.3842022514996,
-1.1961046526289E-14));
#215135=CARTESIAN_POINT('Ctrl Pts',(-20.7121180817081,-20.3162569684087,
-1.55292445569444E-14));
#215136=CARTESIAN_POINT('Ctrl Pts',(-20.7284901400346,-20.2878206121505,
-1.7251812553125E-14));
#215137=CARTESIAN_POINT('Ctrl Pts',(-20.7442869378835,-20.2590491139325,
-1.72679665432114E-15));
#215138=CARTESIAN_POINT('Ctrl Pts',(-20.7594884026036,-20.2299553026624,
8.32667268468867E-16));
#215139=CARTESIAN_POINT('Ctrl Pts',(-20.7693451022676,-20.2110907415789,
2.84488477332053E-15));
#215140=CARTESIAN_POINT('Ctrl Pts',(-20.7789514808442,-20.1920906691223,
-5.33029635918034E-15));
#215141=CARTESIAN_POINT('Ctrl Pts',(-20.7883017662921,-20.1729585792041,
-1.32671651442706E-14));
#215142=CARTESIAN_POINT('Ctrl Pts',(-20.7942277139279,-20.1608331993265,
-1.8152373887588E-14));
#215143=CARTESIAN_POINT('Ctrl Pts',(-20.8000469683619,-20.1486625665028,
1.84527092251997E-14));
#215144=CARTESIAN_POINT('Ctrl Pts',(-20.8057568610096,-20.1364512427194,
1.4585554986013E-14));
#215145=CARTESIAN_POINT('Ctrl Pts',(-20.8408823973353,-20.0613308641761,
-8.46139807618924E-15));
#215146=CARTESIAN_POINT('Ctrl Pts',(-20.8718944952827,-19.9846287385395,
1.40630333927033E-15));
#215147=CARTESIAN_POINT('Ctrl Pts',(-20.8985463569486,-19.9065734343537,
-7.97972798949331E-15));
#215148=CARTESIAN_POINT('Ctrl Pts',(-20.9251982186144,-19.8285181301678,
-1.7094606859296E-14));
#215149=CARTESIAN_POINT('Ctrl Pts',(-20.9474903161071,-19.7491089176507,
-2.28260845907407E-14));
#215150=CARTESIAN_POINT('Ctrl Pts',(-20.9651215428786,-19.6685651028304,
-1.17128529097954E-14));
#215151=CARTESIAN_POINT('Ctrl Pts',(-20.9829460124324,-19.5871385070737,
-3.41913440983829E-16));
#215152=CARTESIAN_POINT('Ctrl Pts',(-20.9960061448808,-19.5045510760419,
-8.44412583292002E-15));
#215153=CARTESIAN_POINT('Ctrl Pts',(-21.0043775994437,-19.4211942605515,
-5.21804821573824E-15));
#215154=CARTESIAN_POINT('Ctrl Pts',(-21.0078360662703,-19.3867573799617,
-3.86087694338245E-15));
#215155=CARTESIAN_POINT('Ctrl Pts',(-21.0104937056419,-19.3521893421996,
6.81493208789715E-15));
#215156=CARTESIAN_POINT('Ctrl Pts',(-21.0123534306943,-19.3175186761032,
9.90874049477952E-15));
#215157=CARTESIAN_POINT('Ctrl Pts',(-21.0130853886539,-19.3038728578793,
1.11360150531808E-14));
#215158=CARTESIAN_POINT('Ctrl Pts',(-21.0136937288726,-19.2902091507495,
9.61300125740955E-15));
#215159=CARTESIAN_POINT('Ctrl Pts',(-21.0141781582269,-19.2765469516024,
8.43769498715119E-15));
#215160=CARTESIAN_POINT('Ctrl Pts',(-21.0170629175674,-19.1951890482203,
-2.3977240746094E-16));
#215161=CARTESIAN_POINT('Ctrl Pts',(-21.0155663596031,-19.1137544906502,
3.90840785478979E-15));
#215162=CARTESIAN_POINT('Ctrl Pts',(-21.0098211098971,-19.032600466024,
6.68909372336657E-15));
#215163=CARTESIAN_POINT('Ctrl Pts',(-21.0040551996082,-18.9511546021311,
9.47977926020773E-15));
#215164=CARTESIAN_POINT('Ctrl Pts',(-20.9940096109013,-18.8699902747437,
4.03215545607249E-16));
#215165=CARTESIAN_POINT('Ctrl Pts',(-20.9797677234132,-18.7894801122668,
9.35362898246694E-15));
#215166=CARTESIAN_POINT('Ctrl Pts',(-20.9656475490767,-18.709658000838,
1.82275509410235E-14));
#215167=CARTESIAN_POINT('Ctrl Pts',(-20.9474020559152,-18.6304779977789,
-4.3520267587977E-15));
#215168=CARTESIAN_POINT('Ctrl Pts',(-20.9250689772833,-18.5523290403031,
-3.21964677141295E-15));
#215169=CARTESIAN_POINT('Ctrl Pts',(-20.9157717581042,-18.5197957743688,
-2.81628118295938E-15));
#215170=CARTESIAN_POINT('Ctrl Pts',(-20.9057656579654,-18.487441581366,
8.12354228918885E-15));
#215171=CARTESIAN_POINT('Ctrl Pts',(-20.895051417118,-18.4552964308102,
-9.57567358739198E-15));
#215172=CARTESIAN_POINT('Ctrl Pts',(-20.8895107429844,-18.4386731528066,
-1.88289619471796E-14));
#215173=CARTESIAN_POINT('Ctrl Pts',(-20.8837798116562,-18.4221037461655,
-4.83972879403747E-15));
#215174=CARTESIAN_POINT('Ctrl Pts',(-20.8778666087312,-18.4056137222238,
-3.13638004456607E-15));
#215175=CARTESIAN_POINT('Ctrl Pts',(-20.8511334397242,-18.3310634991803,
4.89831143352979E-15));
#215176=CARTESIAN_POINT('Ctrl Pts',(-20.820647395102,-18.2580374311815,
-9.744766559422E-15));
#215177=CARTESIAN_POINT('Ctrl Pts',(-20.7864673279414,-18.1868947789178,
-2.66453525910038E-15));
#215178=CARTESIAN_POINT('Ctrl Pts',(-20.7601551114488,-18.132128330993,
2.78590981802746E-15));
#215179=CARTESIAN_POINT('Ctrl Pts',(-20.7316528702852,-18.0784783891692,
2.11663013799853E-15));
#215180=CARTESIAN_POINT('Ctrl Pts',(-20.7009722503935,-18.0261235328628,
1.55986334959834E-14));
#215181=CARTESIAN_POINT('Ctrl Pts',(-20.6917379810896,-18.0103657403473,
1.97460531307573E-14));
#215182=CARTESIAN_POINT('Ctrl Pts',(-20.6823062897647,-17.9947253717853,
1.79594778764635E-14));
#215183=CARTESIAN_POINT('Ctrl Pts',(-20.6726772825947,-17.9792075775192,
1.94289029309402E-14));
#215184=CARTESIAN_POINT('Ctrl Pts',(-20.6644523726372,-17.9659525805787,
2.06523250739444E-14));
#215185=CARTESIAN_POINT('Ctrl Pts',(-20.6560857633015,-17.9527907829532,
9.64787106585675E-16));
#215186=CARTESIAN_POINT('Ctrl Pts',(-20.6475820647203,-17.939731697129,
8.60422844084496E-16));
#215187=CARTESIAN_POINT('Ctrl Pts',(-20.6064305493276,-17.8765355282888,
2.51002288245022E-16));
#215188=CARTESIAN_POINT('Ctrl Pts',(-20.5620419163801,-17.8156943120763,
1.53373012318955E-14));
#215189=CARTESIAN_POINT('Ctrl Pts',(-20.5144495416444,-17.7575477797155,
1.39610545346613E-14));
#215190=CARTESIAN_POINT('Ctrl Pts',(-20.4703172832204,-17.7036286843383,
1.22109826709272E-14));
#215191=CARTESIAN_POINT('Ctrl Pts',(-20.4234296462928,-17.6520265735113,
-9.73370719758813E-15));
#215192=CARTESIAN_POINT('Ctrl Pts',(-20.3737906735959,-17.6030455128839,
-2.54796184151473E-14));
#215193=CARTESIAN_POINT('Ctrl Pts',(-20.368202112649,-17.5975310224002,
-2.7237392166664E-14));
#215194=CARTESIAN_POINT('Ctrl Pts',(-20.3625786573857,-17.5920497923538,
-1.59933772775865E-15));
#215195=CARTESIAN_POINT('Ctrl Pts',(-20.3569206763285,-17.5866019717796,
2.66453525910038E-15));
#215196=CARTESIAN_POINT('Origin',(23.734,9.62950000000001,14.8));
#215197=CARTESIAN_POINT('',(23.734,10.6295,14.8));
#215198=CARTESIAN_POINT('',(23.734,9.62950000000001,14.8));
#215199=CARTESIAN_POINT('',(23.734,14.42025,14.8));
#215200=CARTESIAN_POINT('',(23.534,9.62950000000001,14.8));
#215201=CARTESIAN_POINT('',(23.734,9.62950000000001,14.8));
#215202=CARTESIAN_POINT('',(23.534,10.6295,14.8));
#215203=CARTESIAN_POINT('',(23.534,10.6295,14.8));
#215204=CARTESIAN_POINT('',(23.734,10.6295,14.8));
#215205=CARTESIAN_POINT('Origin',(23.734,9.62950000000001,17.2));
#215206=CARTESIAN_POINT('',(23.734,9.62950000000001,17.2));
#215207=CARTESIAN_POINT('',(23.734,9.62950000000001,8.6));
#215208=CARTESIAN_POINT('',(23.534,9.62950000000001,17.2));
#215209=CARTESIAN_POINT('',(23.734,9.62950000000001,17.2));
#215210=CARTESIAN_POINT('',(23.534,9.62950000000001,14.8));
#215211=CARTESIAN_POINT('Origin',(23.734,9.12950000000001,17.2));
#215212=CARTESIAN_POINT('',(23.734,9.12950000000001,17.2));
#215213=CARTESIAN_POINT('',(23.734,14.17025,17.2));
#215214=CARTESIAN_POINT('',(23.534,9.12950000000001,17.2));
#215215=CARTESIAN_POINT('',(23.734,9.12950000000001,17.2));
#215216=CARTESIAN_POINT('',(23.534,9.62950000000001,17.2));
#215217=CARTESIAN_POINT('Origin',(23.734,10.1295,19.2));
#215218=CARTESIAN_POINT('',(23.734,10.1295,19.2));
#215219=CARTESIAN_POINT('',(23.734,7.19765,13.3363));
#215220=CARTESIAN_POINT('',(23.534,10.1295,19.2));
#215221=CARTESIAN_POINT('',(23.734,10.1295,19.2));
#215222=CARTESIAN_POINT('',(23.534,9.12950000000001,17.2));
#215223=CARTESIAN_POINT('Origin',(23.734,11.1295,17.2));
#215224=CARTESIAN_POINT('',(23.734,11.1295,17.2));
#215225=CARTESIAN_POINT('',(23.734,15.37765,8.7037));
#215226=CARTESIAN_POINT('',(23.534,11.1295,17.2));
#215227=CARTESIAN_POINT('',(23.734,11.1295,17.2));
#215228=CARTESIAN_POINT('',(23.534,11.1295,17.2));
#215229=CARTESIAN_POINT('Origin',(23.734,10.6295,17.2));
#215230=CARTESIAN_POINT('',(23.734,10.6295,17.2));
#215231=CARTESIAN_POINT('',(23.734,14.92025,17.2));
#215232=CARTESIAN_POINT('',(23.534,10.6295,17.2));
#215233=CARTESIAN_POINT('',(23.734,10.6295,17.2));
#215234=CARTESIAN_POINT('',(23.534,10.6295,17.2));
#215235=CARTESIAN_POINT('Origin',(23.734,10.6295,14.8));
#215236=CARTESIAN_POINT('',(23.734,10.6295,7.4));
#215237=CARTESIAN_POINT('',(23.534,10.6295,14.8));
#215238=CARTESIAN_POINT('Origin',(23.734,10.1295,17.));
#215239=CARTESIAN_POINT('',(23.734,10.1295,20.));
#215240=CARTESIAN_POINT('Origin',(23.734,10.1295,17.));
#215241=CARTESIAN_POINT('',(23.534,10.1295,20.));
#215242=CARTESIAN_POINT('',(23.734,10.1295,20.));
#215243=CARTESIAN_POINT('Origin',(23.534,10.1295,17.));
#215244=CARTESIAN_POINT('Origin',(23.534,10.1295,17.));
#215245=CARTESIAN_POINT('Origin',(23.734,-9.8705,7.));
#215246=CARTESIAN_POINT('',(23.734,-5.8705,11.4721359549996));
#215247=CARTESIAN_POINT('',(23.734,-3.8705,7.));
#215248=CARTESIAN_POINT('Origin',(23.734,-9.8705,7.));
#215249=CARTESIAN_POINT('',(23.534,-3.87049999999999,7.));
#215250=CARTESIAN_POINT('',(23.734,-3.8705,7.));
#215251=CARTESIAN_POINT('',(23.534,-5.8705,11.4721359549996));
#215252=CARTESIAN_POINT('Origin',(23.534,-9.8705,7.));
#215253=CARTESIAN_POINT('',(23.734,-5.8705,11.4721359549996));
#215254=CARTESIAN_POINT('Origin',(23.734,4.1295,7.));
#215255=CARTESIAN_POINT('',(23.734,4.1295,7.));
#215256=CARTESIAN_POINT('',(23.734,11.67025,7.));
#215257=CARTESIAN_POINT('',(23.534,4.1295,7.));
#215258=CARTESIAN_POINT('',(23.734,4.1295,7.));
#215259=CARTESIAN_POINT('',(23.534,4.1295,7.));
#215260=CARTESIAN_POINT('Origin',(23.734,10.1295,7.));
#215261=CARTESIAN_POINT('',(23.734,6.1295,11.4721359549996));
#215262=CARTESIAN_POINT('Origin',(23.734,10.1295,7.));
#215263=CARTESIAN_POINT('',(23.534,6.1295,11.4721359549996));
#215264=CARTESIAN_POINT('',(23.734,6.1295,11.4721359549996));
#215265=CARTESIAN_POINT('Origin',(23.534,10.1295,7.));
#215266=CARTESIAN_POINT('Origin',(23.734,6.1295,22.));
#215267=CARTESIAN_POINT('',(23.734,6.1295,11.));
#215268=CARTESIAN_POINT('',(23.534,6.1295,22.));
#215269=CARTESIAN_POINT('Origin',(23.734,-5.8705,11.4721359549996));
#215270=CARTESIAN_POINT('',(23.734,-5.8705,5.73606797749979));
#215271=CARTESIAN_POINT('',(23.534,-5.8705,22.));
#215272=CARTESIAN_POINT('Origin',(23.534,0.129500000000005,11.5));
#215273=CARTESIAN_POINT('',(23.534,0.129500000000002,21.));
#215274=CARTESIAN_POINT('Origin',(23.534,0.129500000000004,17.));
#215275=CARTESIAN_POINT('',(23.534,-9.8705,12.));
#215276=CARTESIAN_POINT('Origin',(23.534,-9.8705,7.));
#215277=CARTESIAN_POINT('Origin',(23.734,-9.37049999999999,16.8));
#215278=CARTESIAN_POINT('',(23.734,-9.37049999999999,19.2));
#215279=CARTESIAN_POINT('',(23.734,-9.37049999999999,16.8));
#215280=CARTESIAN_POINT('',(23.734,-9.37049999999999,8.4));
#215281=CARTESIAN_POINT('',(23.534,-9.37049999999999,16.8));
#215282=CARTESIAN_POINT('',(23.734,-9.37049999999999,16.8));
#215283=CARTESIAN_POINT('',(23.534,-9.37049999999999,19.2));
#215284=CARTESIAN_POINT('',(23.534,-9.37049999999999,19.2));
#215285=CARTESIAN_POINT('',(23.734,-9.37049999999999,19.2));
#215286=CARTESIAN_POINT('Origin',(23.734,-8.87049999999999,16.8));
#215287=CARTESIAN_POINT('',(23.734,-8.87049999999999,16.8));
#215288=CARTESIAN_POINT('',(23.734,5.17025,16.8));
#215289=CARTESIAN_POINT('',(23.534,-8.87049999999999,16.8));
#215290=CARTESIAN_POINT('',(23.734,-8.87049999999999,16.8));
#215291=CARTESIAN_POINT('',(23.534,-9.37049999999999,16.8));
#215292=CARTESIAN_POINT('Origin',(23.734,-9.8705,14.8));
#215293=CARTESIAN_POINT('',(23.734,-9.8705,14.8));
#215294=CARTESIAN_POINT('',(23.734,-9.92234999999999,14.6963));
#215295=CARTESIAN_POINT('',(23.534,-9.8705,14.8));
#215296=CARTESIAN_POINT('',(23.734,-9.8705,14.8));
#215297=CARTESIAN_POINT('',(23.534,-8.87049999999999,16.8));
#215298=CARTESIAN_POINT('Origin',(23.734,-10.8705,16.8));
#215299=CARTESIAN_POINT('',(23.734,-10.8705,16.8));
#215300=CARTESIAN_POINT('',(23.734,-4.50234999999999,4.0637));
#215301=CARTESIAN_POINT('',(23.534,-10.8705,16.8));
#215302=CARTESIAN_POINT('',(23.734,-10.8705,16.8));
#215303=CARTESIAN_POINT('',(23.534,-10.8705,16.8));
#215304=CARTESIAN_POINT('Origin',(23.734,-10.3705,16.8));
#215305=CARTESIAN_POINT('',(23.734,-10.3705,16.8));
#215306=CARTESIAN_POINT('',(23.734,4.42025,16.8));
#215307=CARTESIAN_POINT('',(23.534,-10.3705,16.8));
#215308=CARTESIAN_POINT('',(23.734,-10.3705,16.8));
#215309=CARTESIAN_POINT('',(23.534,-10.3705,16.8));
#215310=CARTESIAN_POINT('Origin',(23.734,-10.3705,19.2));
#215311=CARTESIAN_POINT('',(23.734,-10.3705,19.2));
#215312=CARTESIAN_POINT('',(23.734,-10.3705,9.6));
#215313=CARTESIAN_POINT('',(23.534,-10.3705,19.2));
#215314=CARTESIAN_POINT('',(23.734,-10.3705,19.2));
#215315=CARTESIAN_POINT('',(23.534,-10.3705,19.2));
#215316=CARTESIAN_POINT('Origin',(23.734,-9.37049999999999,19.2));
#215317=CARTESIAN_POINT('',(23.734,4.92025,19.2));
#215318=CARTESIAN_POINT('',(23.534,-9.37049999999999,19.2));
#215319=CARTESIAN_POINT('Origin',(23.734,-9.8705,17.));
#215320=CARTESIAN_POINT('',(23.734,-9.8705,20.));
#215321=CARTESIAN_POINT('Origin',(23.734,-9.8705,17.));
#215322=CARTESIAN_POINT('',(23.534,-9.8705,20.));
#215323=CARTESIAN_POINT('',(23.734,-9.8705,20.));
#215324=CARTESIAN_POINT('Origin',(23.534,-9.8705,17.));
#215325=CARTESIAN_POINT('Origin',(23.534,-9.8705,17.));
#215326=CARTESIAN_POINT('Origin',(23.734,19.211,0.));
#215327=CARTESIAN_POINT('Origin',(23.734,19.211,0.));
#215328=CARTESIAN_POINT('Origin',(23.734,0.129500000000004,17.));
#215329=CARTESIAN_POINT('',(17.734,0.129500000000003,21.));
#215330=CARTESIAN_POINT('',(23.734,0.129500000000005,21.));
#215331=CARTESIAN_POINT('Origin',(17.734,0.129500000000004,17.));
#215332=CARTESIAN_POINT('Origin',(17.734,0.129500000000004,17.));
#215333=CARTESIAN_POINT('Origin',(17.734,10.1295,7.));
#215334=CARTESIAN_POINT('Origin',(23.734,-9.8705,7.));
#215335=CARTESIAN_POINT('',(17.734,-9.8705,12.));
#215336=CARTESIAN_POINT('',(23.734,-9.8705,12.));
#215337=CARTESIAN_POINT('Origin',(17.734,-9.8705,7.));
#215338=CARTESIAN_POINT('Origin',(17.734,-9.8705,7.));
#215339=CARTESIAN_POINT('Origin',(-23.734,-9.8705,7.));
#215340=CARTESIAN_POINT('',(-23.734,-3.8705,7.));
#215341=CARTESIAN_POINT('',(-23.734,-5.8705,11.4721359549996));
#215342=CARTESIAN_POINT('Origin',(-23.734,-9.8705,7.));
#215343=CARTESIAN_POINT('',(-23.534,-5.8705,11.4721359549996));
#215344=CARTESIAN_POINT('',(-23.734,-5.8705,11.4721359549996));
#215345=CARTESIAN_POINT('',(-23.534,-3.87049999999999,7.));
#215346=CARTESIAN_POINT('Origin',(-23.534,-9.8705,7.));
#215347=CARTESIAN_POINT('',(-23.734,-3.8705,7.));
#215348=CARTESIAN_POINT('Origin',(-23.734,4.1295,7.));
#215349=CARTESIAN_POINT('',(-23.734,4.1295,7.));
#215350=CARTESIAN_POINT('',(-23.734,-7.41125,7.));
#215351=CARTESIAN_POINT('',(-23.534,4.1295,7.));
#215352=CARTESIAN_POINT('',(-23.534,4.1295,7.));
#215353=CARTESIAN_POINT('',(-23.734,4.1295,7.));
#215354=CARTESIAN_POINT('Origin',(-23.734,10.1295,7.));
#215355=CARTESIAN_POINT('',(-23.734,6.1295,11.4721359549996));
#215356=CARTESIAN_POINT('Origin',(-23.734,10.1295,7.));
#215357=CARTESIAN_POINT('',(-23.534,6.1295,11.4721359549996));
#215358=CARTESIAN_POINT('Origin',(-23.534,10.1295,7.));
#215359=CARTESIAN_POINT('',(-23.734,6.1295,11.4721359549996));
#215360=CARTESIAN_POINT('Origin',(-23.734,6.1295,22.));
#215361=CARTESIAN_POINT('',(-23.734,6.1295,11.));
#215362=CARTESIAN_POINT('',(-23.534,6.1295,22.));
#215363=CARTESIAN_POINT('Origin',(-23.734,-5.8705,11.4721359549996));
#215364=CARTESIAN_POINT('',(-23.734,-5.8705,5.73606797749979));
#215365=CARTESIAN_POINT('',(-23.534,-5.8705,22.));
#215366=CARTESIAN_POINT('Origin',(-23.534,0.129500000000005,11.5));
#215367=CARTESIAN_POINT('',(-23.534,0.129500000000002,21.));
#215368=CARTESIAN_POINT('Origin',(-23.534,0.129500000000004,17.));
#215369=CARTESIAN_POINT('',(-23.534,-9.8705,12.));
#215370=CARTESIAN_POINT('Origin',(-23.534,-9.8705,7.));
#215371=CARTESIAN_POINT('Origin',(-23.734,-9.37049999999999,16.8));
#215372=CARTESIAN_POINT('',(-23.734,-9.37049999999999,16.8));
#215373=CARTESIAN_POINT('',(-23.734,-9.37049999999999,19.2));
#215374=CARTESIAN_POINT('',(-23.734,-9.3705,8.4));
#215375=CARTESIAN_POINT('',(-23.534,-9.37049999999999,19.2));
#215376=CARTESIAN_POINT('',(-23.734,-9.37049999999999,19.2));
#215377=CARTESIAN_POINT('',(-23.534,-9.37049999999999,16.8));
#215378=CARTESIAN_POINT('',(-23.534,-9.37049999999999,19.2));
#215379=CARTESIAN_POINT('',(-23.734,-9.37049999999999,16.8));
#215380=CARTESIAN_POINT('Origin',(-23.734,-8.87049999999999,16.8));
#215381=CARTESIAN_POINT('',(-23.734,-8.87049999999999,16.8));
#215382=CARTESIAN_POINT('',(-23.734,-13.91125,16.8));
#215383=CARTESIAN_POINT('',(-23.534,-8.87049999999999,16.8));
#215384=CARTESIAN_POINT('',(-23.534,-9.37049999999999,16.8));
#215385=CARTESIAN_POINT('',(-23.734,-8.87049999999999,16.8));
#215386=CARTESIAN_POINT('Origin',(-23.734,-9.8705,14.8));
#215387=CARTESIAN_POINT('',(-23.734,-9.8705,14.8));
#215388=CARTESIAN_POINT('',(-23.734,-13.73865,7.0637));
#215389=CARTESIAN_POINT('',(-23.534,-9.8705,14.8));
#215390=CARTESIAN_POINT('',(-23.534,-8.87049999999999,16.8));
#215391=CARTESIAN_POINT('',(-23.734,-9.8705,14.8));
#215392=CARTESIAN_POINT('Origin',(-23.734,-10.8705,16.8));
#215393=CARTESIAN_POINT('',(-23.734,-10.8705,16.8));
#215394=CARTESIAN_POINT('',(-23.734,-8.31864999999999,11.6963));
#215395=CARTESIAN_POINT('',(-23.534,-10.8705,16.8));
#215396=CARTESIAN_POINT('',(-23.534,-10.8705,16.8));
#215397=CARTESIAN_POINT('',(-23.734,-10.8705,16.8));
#215398=CARTESIAN_POINT('Origin',(-23.734,-10.3705,16.8));
#215399=CARTESIAN_POINT('',(-23.734,-10.3705,16.8));
#215400=CARTESIAN_POINT('',(-23.734,-14.66125,16.8));
#215401=CARTESIAN_POINT('',(-23.534,-10.3705,16.8));
#215402=CARTESIAN_POINT('',(-23.534,-10.3705,16.8));
#215403=CARTESIAN_POINT('',(-23.734,-10.3705,16.8));
#215404=CARTESIAN_POINT('Origin',(-23.734,-10.3705,19.2));
#215405=CARTESIAN_POINT('',(-23.734,-10.3705,19.2));
#215406=CARTESIAN_POINT('',(-23.734,-10.3705,9.6));
#215407=CARTESIAN_POINT('',(-23.534,-10.3705,19.2));
#215408=CARTESIAN_POINT('',(-23.534,-10.3705,19.2));
#215409=CARTESIAN_POINT('',(-23.734,-10.3705,19.2));
#215410=CARTESIAN_POINT('Origin',(-23.734,-9.37049999999999,19.2));
#215411=CARTESIAN_POINT('',(-23.734,-14.16125,19.2));
#215412=CARTESIAN_POINT('',(-23.534,-9.37049999999999,19.2));
#215413=CARTESIAN_POINT('Origin',(-23.734,-9.8705,17.));
#215414=CARTESIAN_POINT('',(-23.534,-9.8705,20.));
#215415=CARTESIAN_POINT('Origin',(-23.534,-9.8705,17.));
#215416=CARTESIAN_POINT('',(-23.734,-9.8705,20.));
#215417=CARTESIAN_POINT('',(-23.734,-9.8705,20.));
#215418=CARTESIAN_POINT('Origin',(-23.734,-9.8705,17.));
#215419=CARTESIAN_POINT('Origin',(-23.534,-9.8705,17.));
#215420=CARTESIAN_POINT('Origin',(-23.734,9.62950000000001,14.8));
#215421=CARTESIAN_POINT('',(-23.734,9.62950000000001,14.8));
#215422=CARTESIAN_POINT('',(-23.734,10.6295,14.8));
#215423=CARTESIAN_POINT('',(-23.734,-4.66124999999999,14.8));
#215424=CARTESIAN_POINT('',(-23.534,10.6295,14.8));
#215425=CARTESIAN_POINT('',(-23.734,10.6295,14.8));
#215426=CARTESIAN_POINT('',(-23.534,9.62950000000001,14.8));
#215427=CARTESIAN_POINT('',(-23.534,10.6295,14.8));
#215428=CARTESIAN_POINT('',(-23.734,9.62950000000001,14.8));
#215429=CARTESIAN_POINT('Origin',(-23.734,9.62950000000001,17.2));
#215430=CARTESIAN_POINT('',(-23.734,9.62950000000001,17.2));
#215431=CARTESIAN_POINT('',(-23.734,9.62950000000001,8.6));
#215432=CARTESIAN_POINT('',(-23.534,9.62950000000001,17.2));
#215433=CARTESIAN_POINT('',(-23.534,9.62950000000001,14.8));
#215434=CARTESIAN_POINT('',(-23.734,9.62950000000001,17.2));
#215435=CARTESIAN_POINT('Origin',(-23.734,9.12950000000001,17.2));
#215436=CARTESIAN_POINT('',(-23.734,9.12950000000001,17.2));
#215437=CARTESIAN_POINT('',(-23.734,-4.91124999999999,17.2));
#215438=CARTESIAN_POINT('',(-23.534,9.12950000000001,17.2));
#215439=CARTESIAN_POINT('',(-23.534,9.62950000000001,17.2));
#215440=CARTESIAN_POINT('',(-23.734,9.12950000000001,17.2));
#215441=CARTESIAN_POINT('Origin',(-23.734,10.1295,19.2));
#215442=CARTESIAN_POINT('',(-23.734,10.1295,19.2));
#215443=CARTESIAN_POINT('',(-23.734,3.38135000000002,5.7037));
#215444=CARTESIAN_POINT('',(-23.534,10.1295,19.2));
#215445=CARTESIAN_POINT('',(-23.534,9.12950000000001,17.2));
#215446=CARTESIAN_POINT('',(-23.734,10.1295,19.2));
#215447=CARTESIAN_POINT('Origin',(-23.734,11.1295,17.2));
#215448=CARTESIAN_POINT('',(-23.734,11.1295,17.2));
#215449=CARTESIAN_POINT('',(-23.734,11.56135,16.3363));
#215450=CARTESIAN_POINT('',(-23.534,11.1295,17.2));
#215451=CARTESIAN_POINT('',(-23.534,11.1295,17.2));
#215452=CARTESIAN_POINT('',(-23.734,11.1295,17.2));
#215453=CARTESIAN_POINT('Origin',(-23.734,10.6295,17.2));
#215454=CARTESIAN_POINT('',(-23.734,10.6295,17.2));
#215455=CARTESIAN_POINT('',(-23.734,-4.16125,17.2));
#215456=CARTESIAN_POINT('',(-23.534,10.6295,17.2));
#215457=CARTESIAN_POINT('',(-23.534,10.6295,17.2));
#215458=CARTESIAN_POINT('',(-23.734,10.6295,17.2));
#215459=CARTESIAN_POINT('Origin',(-23.734,10.6295,14.8));
#215460=CARTESIAN_POINT('',(-23.734,10.6295,7.4));
#215461=CARTESIAN_POINT('',(-23.534,10.6295,14.8));
#215462=CARTESIAN_POINT('Origin',(-23.734,10.1295,17.));
#215463=CARTESIAN_POINT('',(-23.534,10.1295,20.));
#215464=CARTESIAN_POINT('Origin',(-23.534,10.1295,17.));
#215465=CARTESIAN_POINT('',(-23.734,10.1295,20.));
#215466=CARTESIAN_POINT('',(-23.734,10.1295,20.));
#215467=CARTESIAN_POINT('Origin',(-23.734,10.1295,17.));
#215468=CARTESIAN_POINT('Origin',(-23.534,10.1295,17.));
#215469=CARTESIAN_POINT('Origin',(-23.734,-18.952,0.));
#215470=CARTESIAN_POINT('Origin',(-23.734,-18.952,0.));
#215471=CARTESIAN_POINT('Origin',(-23.734,-18.952,0.));
#215472=CARTESIAN_POINT('',(-23.734,19.211,0.));
#215473=CARTESIAN_POINT('',(-23.734,19.211,0.));
#215474=CARTESIAN_POINT('',(-23.734,-18.952,0.));
#215475=CARTESIAN_POINT('',(-23.734,19.211,0.));
#215476=CARTESIAN_POINT('',(-23.734,-18.952,0.));
#215477=CARTESIAN_POINT('Origin',(-17.734,10.1295,7.));
#215478=CARTESIAN_POINT('Origin',(-23.734,-9.8705,7.));
#215479=CARTESIAN_POINT('',(-17.734,-9.8705,12.));
#215480=CARTESIAN_POINT('Origin',(-17.734,-9.8705,7.));
#215481=CARTESIAN_POINT('',(-23.734,-9.8705,12.));
#215482=CARTESIAN_POINT('Origin',(-17.734,-9.8705,7.));
#215483=CARTESIAN_POINT('Origin',(-23.734,0.129500000000004,17.));
#215484=CARTESIAN_POINT('',(-17.734,0.129500000000003,21.));
#215485=CARTESIAN_POINT('Origin',(-17.734,0.129500000000004,17.));
#215486=CARTESIAN_POINT('',(-23.734,0.129500000000005,21.));
#215487=CARTESIAN_POINT('Origin',(-17.734,0.129500000000004,17.));
#215488=CARTESIAN_POINT('Origin',(-18.734,0.12950000000008,22.));
#215489=CARTESIAN_POINT('',(-21.234,0.12950000000008,21.5));
#215490=CARTESIAN_POINT('Origin',(-18.734,0.12950000000008,21.5));
#215491=CARTESIAN_POINT('',(-21.234,0.12950000000008,22.));
#215492=CARTESIAN_POINT('Origin',(0.,0.12950000000008,21.5));
#215493=CARTESIAN_POINT('Origin',(18.734,0.12950000000008,22.));
#215494=CARTESIAN_POINT('',(16.234,0.12950000000008,21.5));
#215495=CARTESIAN_POINT('Origin',(18.734,0.12950000000008,21.5));
#215496=CARTESIAN_POINT('',(16.234,0.12950000000008,22.));
#215497=CARTESIAN_POINT('Origin',(0.,0.12950000000008,21.5));
#215498=CARTESIAN_POINT('Origin',(-7.0995,19.4175,0.));
#215499=CARTESIAN_POINT('',(-7.0995,19.4175,0.));
#215500=CARTESIAN_POINT('',(-7.0995,16.8045,0.));
#215501=CARTESIAN_POINT('',(-7.0995,19.4175,0.));
#215502=CARTESIAN_POINT('Origin',(-10.7505,17.8045,0.));
#215503=CARTESIAN_POINT('Origin',(-10.7505,17.8045,0.));
#215504=CARTESIAN_POINT('Origin',(-9.06658668237251,24.2952266006623,0.));
#215505=CARTESIAN_POINT('',(-9.06658668237251,24.4862266006622,0.));
#215506=CARTESIAN_POINT('Origin',(-9.06658668237251,24.2952266006623,0.));
#215507=CARTESIAN_POINT('',(-9.06658668237251,24.4862266006622,0.));
#215508=CARTESIAN_POINT('Origin',(-7.30158668237251,24.4862266006622,0.));
#215509=CARTESIAN_POINT('',(-7.30158668237251,24.4862266006622,0.));
#215510=CARTESIAN_POINT('',(-9.06658668237251,24.4862266006622,0.));
#215511=CARTESIAN_POINT('',(-7.30158668237251,24.4862266006622,0.));
#215512=CARTESIAN_POINT('Origin',(-7.30158668237251,24.6772266006623,0.));
#215513=CARTESIAN_POINT('',(-7.11058668237251,24.6772266006623,0.));
#215514=CARTESIAN_POINT('Origin',(-7.30158668237251,24.6772266006623,0.));
#215515=CARTESIAN_POINT('',(-7.11058668237251,24.6772266006623,0.));
#215516=CARTESIAN_POINT('Origin',(-7.11058668237251,25.8032266006623,0.));
#215517=CARTESIAN_POINT('',(-7.11058668237251,25.8032266006623,0.));
#215518=CARTESIAN_POINT('',(-7.11058668237251,24.6772266006623,0.));
#215519=CARTESIAN_POINT('',(-7.11058668237251,25.8032266006623,0.));
#215520=CARTESIAN_POINT('Origin',(-7.36458668237251,25.8032266006623,0.));
#215521=CARTESIAN_POINT('',(-7.36458668237251,26.0572266006623,0.));
#215522=CARTESIAN_POINT('Origin',(-7.36458668237251,25.8032266006623,0.));
#215523=CARTESIAN_POINT('',(-7.36458668237251,26.0572266006623,0.));
#215524=CARTESIAN_POINT('Origin',(-18.734,24.211,0.));
#215525=CARTESIAN_POINT('',(-18.734,24.211,0.));
#215526=CARTESIAN_POINT('',(-7.36458668237251,26.0572266006622,0.));
#215527=CARTESIAN_POINT('',(-18.734,24.211,0.));
#215528=CARTESIAN_POINT('Origin',(-18.734,19.211,0.));
#215529=CARTESIAN_POINT('Origin',(-18.734,19.211,0.));
#215530=CARTESIAN_POINT('Origin',(-18.734,-18.952,0.));
#215531=CARTESIAN_POINT('',(-18.734,-23.952,0.));
#215532=CARTESIAN_POINT('Origin',(-18.734,-18.952,0.));
#215533=CARTESIAN_POINT('',(-18.734,-23.952,0.));
#215534=CARTESIAN_POINT('Origin',(18.734,-23.952,0.));
#215535=CARTESIAN_POINT('',(18.734,-23.952,0.));
#215536=CARTESIAN_POINT('',(-18.734,-23.952,0.));
#215537=CARTESIAN_POINT('',(18.734,-23.952,0.));
#215538=CARTESIAN_POINT('Origin',(18.734,-18.952,0.));
#215539=CARTESIAN_POINT('',(23.734,-18.952,0.));
#215540=CARTESIAN_POINT('Origin',(18.734,-18.952,0.));
#215541=CARTESIAN_POINT('',(23.734,-18.952,0.));
#215542=CARTESIAN_POINT('Origin',(23.734,19.211,0.));
#215543=CARTESIAN_POINT('',(23.734,19.211,0.));
#215544=CARTESIAN_POINT('',(23.734,19.211,0.));
#215545=CARTESIAN_POINT('',(23.734,19.211,0.));
#215546=CARTESIAN_POINT('Origin',(18.734,19.211,0.));
#215547=CARTESIAN_POINT('',(18.734,24.211,0.));
#215548=CARTESIAN_POINT('Origin',(18.734,19.211,0.));
#215549=CARTESIAN_POINT('',(18.734,24.211,0.));
#215550=CARTESIAN_POINT('Origin',(7.36458668237251,26.0572266006622,0.));
#215551=CARTESIAN_POINT('',(7.36458668237251,26.0572266006622,0.));
#215552=CARTESIAN_POINT('',(7.36458668237251,26.0572266006622,0.));
#215553=CARTESIAN_POINT('',(7.36458668237251,26.0572266006622,0.));
#215554=CARTESIAN_POINT('Origin',(7.36458668237251,25.8032266006622,0.));
#215555=CARTESIAN_POINT('',(7.11058668237251,25.8032266006622,0.));
#215556=CARTESIAN_POINT('Origin',(7.36458668237251,25.8032266006622,0.));
#215557=CARTESIAN_POINT('',(7.11058668237251,25.8032266006622,0.));
#215558=CARTESIAN_POINT('Origin',(7.11058668237251,24.6772266006623,0.));
#215559=CARTESIAN_POINT('',(7.11058668237251,24.6772266006623,0.));
#215560=CARTESIAN_POINT('',(7.11058668237251,24.6772266006623,0.));
#215561=CARTESIAN_POINT('',(7.11058668237251,24.6772266006623,0.));
#215562=CARTESIAN_POINT('Origin',(7.30158668237251,24.6772266006623,0.));
#215563=CARTESIAN_POINT('',(7.30158668237251,24.4862266006622,0.));
#215564=CARTESIAN_POINT('Origin',(7.30158668237251,24.6772266006623,0.));
#215565=CARTESIAN_POINT('',(7.30158668237251,24.4862266006622,0.));
#215566=CARTESIAN_POINT('Origin',(9.06658668237251,24.4862266006622,0.));
#215567=CARTESIAN_POINT('',(9.06658668237251,24.4862266006622,0.));
#215568=CARTESIAN_POINT('',(9.06658668237251,24.4862266006622,0.));
#215569=CARTESIAN_POINT('',(9.06658668237251,24.4862266006622,0.));
#215570=CARTESIAN_POINT('Origin',(9.06658668237251,24.2952266006623,0.));
#215571=CARTESIAN_POINT('',(9.25758668237251,24.2952266006623,0.));
#215572=CARTESIAN_POINT('Origin',(9.06658668237251,24.2952266006623,0.));
#215573=CARTESIAN_POINT('',(9.25758668237251,24.2952266006623,0.));
#215574=CARTESIAN_POINT('Origin',(9.25758668237251,21.5062266006623,0.));
#215575=CARTESIAN_POINT('',(9.25758668237251,21.5062266006623,0.));
#215576=CARTESIAN_POINT('',(9.25758668237251,21.5062266006623,0.));
#215577=CARTESIAN_POINT('',(9.25758668237251,21.5062266006623,0.));
#215578=CARTESIAN_POINT('Origin',(10.7505,17.8045,0.));
#215579=CARTESIAN_POINT('Origin',(10.7505,17.8045,0.));
#215580=CARTESIAN_POINT('Origin',(0.,1.05261330033112,0.));
#215581=CARTESIAN_POINT('',(0.,0.,0.));
#215582=CARTESIAN_POINT('',(0.,0.,0.));
#215583=CARTESIAN_POINT('',(0.,0.,0.));
#215584=CARTESIAN_POINT('',(0.,0.,0.));
#215585=CARTESIAN_POINT('',(0.,2.1,0.));
#215586=CARTESIAN_POINT('',(0.,0.,0.));
#215587=CARTESIAN_POINT('',(0.,0.,400.));
#215588=UNCERTAINTY_MEASURE_WITH_UNIT(LENGTH_MEASURE(0.01),#215610,
'DISTANCE_ACCURACY_VALUE',
'Maximum model space distance between geometric entities at asserted c
onnectivities');
#215589=UNCERTAINTY_MEASURE_WITH_UNIT(LENGTH_MEASURE(0.01),#215610,
'DISTANCE_ACCURACY_VALUE',
'Maximum model space distance between geometric entities at asserted c
onnectivities');
#215590=UNCERTAINTY_MEASURE_WITH_UNIT(LENGTH_MEASURE(0.01),#215610,
'DISTANCE_ACCURACY_VALUE',
'Maximum model space distance between geometric entities at asserted c
onnectivities');
#215591=UNCERTAINTY_MEASURE_WITH_UNIT(LENGTH_MEASURE(0.01),#215610,
'DISTANCE_ACCURACY_VALUE',
'Maximum model space distance between geometric entities at asserted c
onnectivities');
#215592=UNCERTAINTY_MEASURE_WITH_UNIT(LENGTH_MEASURE(0.01),#215610,
'DISTANCE_ACCURACY_VALUE',
'Maximum model space distance between geometric entities at asserted c
onnectivities');
#215593=UNCERTAINTY_MEASURE_WITH_UNIT(LENGTH_MEASURE(0.01),#215610,
'DISTANCE_ACCURACY_VALUE',
'Maximum model space distance between geometric entities at asserted c
onnectivities');
#215594=UNCERTAINTY_MEASURE_WITH_UNIT(LENGTH_MEASURE(0.01),#215610,
'DISTANCE_ACCURACY_VALUE',
'Maximum model space distance between geometric entities at asserted c
onnectivities');
#215595=UNCERTAINTY_MEASURE_WITH_UNIT(LENGTH_MEASURE(0.01),#215610,
'DISTANCE_ACCURACY_VALUE',
'Maximum model space distance between geometric entities at asserted c
onnectivities');
#215596=UNCERTAINTY_MEASURE_WITH_UNIT(LENGTH_MEASURE(0.01),#215610,
'DISTANCE_ACCURACY_VALUE',
'Maximum model space distance between geometric entities at asserted c
onnectivities');
#215597=UNCERTAINTY_MEASURE_WITH_UNIT(LENGTH_MEASURE(0.01),#215610,
'DISTANCE_ACCURACY_VALUE',
'Maximum model space distance between geometric entities at asserted c
onnectivities');
#215598=UNCERTAINTY_MEASURE_WITH_UNIT(LENGTH_MEASURE(0.01),#215610,
'DISTANCE_ACCURACY_VALUE',
'Maximum model space distance between geometric entities at asserted c
onnectivities');
#215599=(
GEOMETRIC_REPRESENTATION_CONTEXT(3)
GLOBAL_UNCERTAINTY_ASSIGNED_CONTEXT((#215588))
GLOBAL_UNIT_ASSIGNED_CONTEXT((#215610,#215612,#215613))
REPRESENTATION_CONTEXT('','3D')
);
#215600=(
GEOMETRIC_REPRESENTATION_CONTEXT(3)
GLOBAL_UNCERTAINTY_ASSIGNED_CONTEXT((#215589))
GLOBAL_UNIT_ASSIGNED_CONTEXT((#215610,#215612,#215613))
REPRESENTATION_CONTEXT('','3D')
);
#215601=(
GEOMETRIC_REPRESENTATION_CONTEXT(3)
GLOBAL_UNCERTAINTY_ASSIGNED_CONTEXT((#215590))
GLOBAL_UNIT_ASSIGNED_CONTEXT((#215610,#215612,#215613))
REPRESENTATION_CONTEXT('','3D')
);
#215602=(
GEOMETRIC_REPRESENTATION_CONTEXT(3)
GLOBAL_UNCERTAINTY_ASSIGNED_CONTEXT((#215591))
GLOBAL_UNIT_ASSIGNED_CONTEXT((#215610,#215612,#215613))
REPRESENTATION_CONTEXT('','3D')
);
#215603=(
GEOMETRIC_REPRESENTATION_CONTEXT(3)
GLOBAL_UNCERTAINTY_ASSIGNED_CONTEXT((#215592))
GLOBAL_UNIT_ASSIGNED_CONTEXT((#215610,#215612,#215613))
REPRESENTATION_CONTEXT('','3D')
);
#215604=(
GEOMETRIC_REPRESENTATION_CONTEXT(3)
GLOBAL_UNCERTAINTY_ASSIGNED_CONTEXT((#215593))
GLOBAL_UNIT_ASSIGNED_CONTEXT((#215610,#215612,#215613))
REPRESENTATION_CONTEXT('','3D')
);
#215605=(
GEOMETRIC_REPRESENTATION_CONTEXT(3)
GLOBAL_UNCERTAINTY_ASSIGNED_CONTEXT((#215594))
GLOBAL_UNIT_ASSIGNED_CONTEXT((#215610,#215612,#215613))
REPRESENTATION_CONTEXT('','3D')
);
#215606=(
GEOMETRIC_REPRESENTATION_CONTEXT(3)
GLOBAL_UNCERTAINTY_ASSIGNED_CONTEXT((#215595))
GLOBAL_UNIT_ASSIGNED_CONTEXT((#215610,#215612,#215613))
REPRESENTATION_CONTEXT('','3D')
);
#215607=(
GEOMETRIC_REPRESENTATION_CONTEXT(3)
GLOBAL_UNCERTAINTY_ASSIGNED_CONTEXT((#215596))
GLOBAL_UNIT_ASSIGNED_CONTEXT((#215610,#215612,#215613))
REPRESENTATION_CONTEXT('','3D')
);
#215608=(
GEOMETRIC_REPRESENTATION_CONTEXT(3)
GLOBAL_UNCERTAINTY_ASSIGNED_CONTEXT((#215597))
GLOBAL_UNIT_ASSIGNED_CONTEXT((#215610,#215612,#215613))
REPRESENTATION_CONTEXT('','3D')
);
#215609=(
GEOMETRIC_REPRESENTATION_CONTEXT(3)
GLOBAL_UNCERTAINTY_ASSIGNED_CONTEXT((#215598))
GLOBAL_UNIT_ASSIGNED_CONTEXT((#215610,#215612,#215613))
REPRESENTATION_CONTEXT('','3D')
);
#215610=(
LENGTH_UNIT()
NAMED_UNIT(*)
SI_UNIT(.MILLI.,.METRE.)
);
#215611=(
LENGTH_UNIT()
NAMED_UNIT(*)
SI_UNIT($,.METRE.)
);
#215612=(
NAMED_UNIT(*)
PLANE_ANGLE_UNIT()
SI_UNIT($,.RADIAN.)
);
#215613=(
NAMED_UNIT(*)
SI_UNIT($,.STERADIAN.)
SOLID_ANGLE_UNIT()
);
#215614=SHAPE_DEFINITION_REPRESENTATION(#215624,#215643);
#215615=SHAPE_DEFINITION_REPRESENTATION(#215625,#215644);
#215616=SHAPE_DEFINITION_REPRESENTATION(#215626,#215645);
#215617=SHAPE_DEFINITION_REPRESENTATION(#215627,#215646);
#215618=SHAPE_DEFINITION_REPRESENTATION(#215628,#215647);
#215619=SHAPE_DEFINITION_REPRESENTATION(#215629,#215648);
#215620=SHAPE_DEFINITION_REPRESENTATION(#215630,#215649);
#215621=SHAPE_DEFINITION_REPRESENTATION(#215633,#215650);
#215622=SHAPE_DEFINITION_REPRESENTATION(#215634,#215651);
#215623=SHAPE_DEFINITION_REPRESENTATION(#215635,#215652);
#215624=PRODUCT_DEFINITION_SHAPE('',$,#215654);
#215625=PRODUCT_DEFINITION_SHAPE('',$,#215655);
#215626=PRODUCT_DEFINITION_SHAPE('',$,#215656);
#215627=PRODUCT_DEFINITION_SHAPE('',$,#215657);
#215628=PRODUCT_DEFINITION_SHAPE('',$,#215658);
#215629=PRODUCT_DEFINITION_SHAPE('',$,#215659);
#215630=PRODUCT_DEFINITION_SHAPE('',$,#215660);
#215631=PRODUCT_DEFINITION_SHAPE($,$,#38);
#215632=PRODUCT_DEFINITION_SHAPE($,$,#39);
#215633=PRODUCT_DEFINITION_SHAPE('',$,#215661);
#215634=PRODUCT_DEFINITION_SHAPE('',$,#215662);
#215635=PRODUCT_DEFINITION_SHAPE('',$,#215663);
#215636=PRODUCT_DEFINITION_SHAPE($,$,#40);
#215637=PRODUCT_DEFINITION_SHAPE($,$,#41);
#215638=PRODUCT_DEFINITION_SHAPE($,$,#42);
#215639=PRODUCT_DEFINITION_SHAPE($,$,#43);
#215640=PRODUCT_DEFINITION_SHAPE($,$,#44);
#215641=PRODUCT_DEFINITION_SHAPE($,$,#45);
#215642=PRODUCT_DEFINITION_SHAPE($,$,#46);
#215643=SHAPE_REPRESENTATION('',(#28178,#30157,#30158,#30159,#30160,#30161,
#30162,#30163),#215599);
#215644=SHAPE_REPRESENTATION('',(#28179),#215600);
#215645=SHAPE_REPRESENTATION('',(#28227),#215601);
#215646=SHAPE_REPRESENTATION('',(#28272),#215602);
#215647=SHAPE_REPRESENTATION('',(#28709,#29431,#29432),#215603);
#215648=SHAPE_REPRESENTATION('',(#28710),#215604);
#215649=SHAPE_REPRESENTATION('',(#28931),#215605);
#215650=SHAPE_REPRESENTATION('',(#29433),#215606);
#215651=SHAPE_REPRESENTATION('',(#29550),#215607);
#215652=SHAPE_REPRESENTATION('',(#29720),#215608);
#215653=PRODUCT_DEFINITION_CONTEXT('part definition',#215685,'design');
#215654=PRODUCT_DEFINITION('2026-10-04-08-16-24-833','MAS-604',#215664,
#215653);
#215655=PRODUCT_DEFINITION('2026-10-04-09-58-43-959','TopStrip',#215665,
#215653);
#215656=PRODUCT_DEFINITION('2026-10-04-10-37-11-877','TopStripTop',#215666,
#215653);
#215657=PRODUCT_DEFINITION('2026-10-04-13-44-26-617','End_Cap',#215667,
#215653);
#215658=PRODUCT_DEFINITION('2026-10-04-15-17-49-077','Carriage',#215668,
#215653);
#215659=PRODUCT_DEFINITION('2026-10-04-16-01-39-984','CarregeSupport',#215669,
#215653);
#215660=PRODUCT_DEFINITION('2026-10-04-16-01-39-984_1',
'CarregeSupport(Mirror)',#215670,#215653);
#215661=PRODUCT_DEFINITION('2026-10-04-16-15-13-894','Carriage_Base',#215671,
#215653);
#215662=PRODUCT_DEFINITION('2026-10-04-08-25-38-216','Barrel',#215672,#215653);
#215663=PRODUCT_DEFINITION('2026-10-04-13-44-26-617_1',
'End_Cap(Mirror)',#215673,#215653);
#215664=PRODUCT_DEFINITION_FORMATION('',$,#215687);
#215665=PRODUCT_DEFINITION_FORMATION('',$,#215688);
#215666=PRODUCT_DEFINITION_FORMATION('',$,#215689);
#215667=PRODUCT_DEFINITION_FORMATION('',$,#215690);
#215668=PRODUCT_DEFINITION_FORMATION('',$,#215691);
#215669=PRODUCT_DEFINITION_FORMATION('',$,#215692);
#215670=PRODUCT_DEFINITION_FORMATION('',$,#215693);
#215671=PRODUCT_DEFINITION_FORMATION('',$,#215694);
#215672=PRODUCT_DEFINITION_FORMATION('',$,#215695);
#215673=PRODUCT_DEFINITION_FORMATION('',$,#215696);
#215674=PRODUCT_RELATED_PRODUCT_CATEGORY('MAS-604','MAS-604',(#215687));
#215675=PRODUCT_RELATED_PRODUCT_CATEGORY('TopStrip','TopStrip',(#215688));
#215676=PRODUCT_RELATED_PRODUCT_CATEGORY('TopStripTop','TopStripTop',(#215689));
#215677=PRODUCT_RELATED_PRODUCT_CATEGORY('End_Cap','End_Cap',(#215690));
#215678=PRODUCT_RELATED_PRODUCT_CATEGORY('Carriage','Carriage',(#215691));
#215679=PRODUCT_RELATED_PRODUCT_CATEGORY('CarregeSupport',
'CarregeSupport',(#215692));
#215680=PRODUCT_RELATED_PRODUCT_CATEGORY('CarregeSupport(Mirror)',
'CarregeSupport(Mirror)',(#215693));
#215681=PRODUCT_RELATED_PRODUCT_CATEGORY('Carriage_Base',
'Carriage_Base',(#215694));
#215682=PRODUCT_RELATED_PRODUCT_CATEGORY('Barrel','Barrel',(#215695));
#215683=PRODUCT_RELATED_PRODUCT_CATEGORY('End_Cap(Mirror)',
'End_Cap(Mirror)',(#215696));
#215684=APPLICATION_PROTOCOL_DEFINITION('international standard',
'automotive_design',2009,#215685);
#215685=APPLICATION_CONTEXT(
'Core Data for Automotive Mechanical Design Process');
#215686=PRODUCT_CONTEXT('part definition',#215685,'mechanical');
#215687=PRODUCT('2026-10-04-08-16-24-833','MAS-604',$,(#215686));
#215688=PRODUCT('2026-10-04-09-58-43-959','TopStrip',$,(#215686));
#215689=PRODUCT('2026-10-04-10-37-11-877','TopStripTop',$,(#215686));
#215690=PRODUCT('2026-10-04-13-44-26-617','End_Cap',$,(#215686));
#215691=PRODUCT('2026-10-04-15-17-49-077','Carriage',$,(#215686));
#215692=PRODUCT('2026-10-04-16-01-39-984','CarregeSupport',$,(#215686));
#215693=PRODUCT('2026-10-04-16-01-39-984_1','CarregeSupport(Mirror)',$,
(#215686));
#215694=PRODUCT('2026-10-04-16-15-13-894','Carriage_Base',$,(#215686));
#215695=PRODUCT('2026-10-04-08-25-38-216','Barrel',$,(#215686));
#215696=PRODUCT('2026-10-04-13-44-26-617_1','End_Cap(Mirror)',$,(#215686));
#215697=PRESENTATION_STYLE_ASSIGNMENT((#215699));
#215698=PRESENTATION_STYLE_ASSIGNMENT((#215700));
#215699=SURFACE_STYLE_USAGE(.BOTH.,#215701);
#215700=SURFACE_STYLE_USAGE(.BOTH.,#215702);
#215701=SURFACE_SIDE_STYLE('',(#215703));
#215702=SURFACE_SIDE_STYLE('',(#215704));
#215703=SURFACE_STYLE_FILL_AREA(#215705);
#215704=SURFACE_STYLE_FILL_AREA(#215706);
#215705=FILL_AREA_STYLE('Steel - Satin',(#215707));
#215706=FILL_AREA_STYLE('Opaque(245,245,246)',(#215708));
#215707=FILL_AREA_STYLE_COLOUR('Steel - Satin',#215709);
#215708=FILL_AREA_STYLE_COLOUR('Opaque(245,245,246)',#215710);
#215709=COLOUR_RGB('Steel - Satin', 0.66274510, 0.83137255, 0.94901961);
#215710=COLOUR_RGB('Opaque(245,245,246)', 0.66274510, 0.83137255, 0.94901961);
ENDSEC;
END-ISO-10303-21;
